#69506=CARTESIAN_POINT('Origin',(0.,133.2,13.3));
#69507=CARTESIAN_POINT('',(-7.31008487907097,133.2,10.5567976631721));
#69508=CARTESIAN_POINT('Origin',(-6.70494843988083,133.2,11.1214301896566));
#69509=CARTESIAN_POINT('',(-7.06568821984138,144.,10.7848359934202));
#69510=CARTESIAN_POINT('',(-7.06568821984138,138.6,10.7848359934202));
#69511=CARTESIAN_POINT('',(-7.31008487907097,144.,10.5567976631721));
#69512=CARTESIAN_POINT('Origin',(-7.06159463349151,144.,11.005548816766));
#69513=CARTESIAN_POINT('Origin',(0.,144.,13.3));
#69514=CARTESIAN_POINT('Origin',(-7.75872111940616,133.2,12.4255020918945));
#69515=CARTESIAN_POINT('',(-7.43743486603367,144.,12.3332722133368));
#69516=CARTESIAN_POINT('',(-7.43743486603367,133.2,12.3332722133368));
#69517=CARTESIAN_POINT('',(-7.43743486603367,138.6,12.3332722133368));
#69518=CARTESIAN_POINT('',(-6.96320280119572,144.,12.1971370214664));
#69519=CARTESIAN_POINT('',(-6.96320280119572,144.,12.1971370214664));
#69520=CARTESIAN_POINT('',(-6.96320280119572,133.2,12.1971370214664));
#69521=CARTESIAN_POINT('',(-6.96320280119572,133.2,12.1971370214664));
#69522=CARTESIAN_POINT('',(-6.96320280119572,133.2,12.1971370214664));
#69523=CARTESIAN_POINT('Origin',(-7.3335859289189,133.2,12.1384740970763));
#69524=CARTESIAN_POINT('',(-7.37215620887551,133.2,11.9211189928285));
#69525=CARTESIAN_POINT('Origin',(0.,133.2,13.3));
#69526=CARTESIAN_POINT('',(-7.64921699387799,133.2,11.7341202534779));
#69527=CARTESIAN_POINT('Origin',(-6.96320280119572,133.2,12.1971370214664));
#69528=CARTESIAN_POINT('',(-7.37215620887551,144.,11.9211189928285));
#69529=CARTESIAN_POINT('',(-7.37215620887551,138.6,11.9211189928285));
#69530=CARTESIAN_POINT('',(-7.64921699387799,144.,11.7341202534779));
#69531=CARTESIAN_POINT('Origin',(-7.3335859289189,144.,12.1384740970763));
#69532=CARTESIAN_POINT('Origin',(0.,144.,13.3));
#69533=CARTESIAN_POINT('Origin',(-7.8,133.2,13.65));
#69534=CARTESIAN_POINT('',(-7.4970972452634,144.,13.5086453811229));
#69535=CARTESIAN_POINT('',(-7.4970972452634,133.2,13.5086453811229));
#69536=CARTESIAN_POINT('',(-7.4970972452634,138.6,13.5086453811229));
#69537=CARTESIAN_POINT('',(-7.05,144.,13.3));
#69538=CARTESIAN_POINT('',(-7.05,144.,13.3));
#69539=CARTESIAN_POINT('',(-7.05,133.2,13.3));
#69540=CARTESIAN_POINT('',(-7.05,133.2,13.3));
#69541=CARTESIAN_POINT('',(-7.05,133.2,13.3));
#69542=CARTESIAN_POINT('Origin',(-7.425,133.2,13.3));
#69543=CARTESIAN_POINT('',(-7.5,133.2,13.3));
#69544=CARTESIAN_POINT('Origin',(0.,133.2,13.3));
#69545=CARTESIAN_POINT('',(-7.4970972452634,133.2,13.0913546188771));
#69546=CARTESIAN_POINT('',(-7.8,133.2,12.95));
#69547=CARTESIAN_POINT('Origin',(0.,133.2,13.3));
#69548=CARTESIAN_POINT('Origin',(-7.05,133.2,13.3));
#69549=CARTESIAN_POINT('',(-7.4970972452634,144.,13.0913546188771));
#69550=CARTESIAN_POINT('',(-7.4970972452634,138.6,13.0913546188771));
#69551=CARTESIAN_POINT('',(-7.8,144.,12.95));
#69552=CARTESIAN_POINT('Origin',(-7.425,144.,13.3));
#69553=CARTESIAN_POINT('',(-7.5,144.,13.3));
#69554=CARTESIAN_POINT('Origin',(0.,144.,13.3));
#69555=CARTESIAN_POINT('Origin',(0.,144.,13.3));
#69556=CARTESIAN_POINT('Origin',(-7.64921699387799,133.2,14.8658797465221));
#69557=CARTESIAN_POINT('',(-7.37215620887551,144.,14.6788810071715));
#69558=CARTESIAN_POINT('',(-7.37215620887551,133.2,14.6788810071715));
#69559=CARTESIAN_POINT('',(-7.37215620887551,138.6,14.6788810071715));
#69560=CARTESIAN_POINT('',(-6.96320280119572,144.,14.4028629785336));
#69561=CARTESIAN_POINT('',(-6.96320280119572,144.,14.4028629785336));
#69562=CARTESIAN_POINT('',(-6.96320280119572,133.2,14.4028629785336));
#69563=CARTESIAN_POINT('',(-6.96320280119572,133.2,14.4028629785336));
#69564=CARTESIAN_POINT('',(-6.96320280119572,133.2,14.4028629785336));
#69565=CARTESIAN_POINT('Origin',(-7.3335859289189,133.2,14.4615259029237));
#69566=CARTESIAN_POINT('',(-7.43743486603367,133.2,14.2667277866632));
#69567=CARTESIAN_POINT('Origin',(0.,133.2,13.3));
#69568=CARTESIAN_POINT('',(-7.75872111940616,133.2,14.1744979081055));
#69569=CARTESIAN_POINT('Origin',(-6.96320280119572,133.2,14.4028629785336));
#69570=CARTESIAN_POINT('',(-7.43743486603367,144.,14.2667277866632));
#69571=CARTESIAN_POINT('',(-7.43743486603367,138.6,14.2667277866632));
#69572=CARTESIAN_POINT('',(-7.75872111940616,144.,14.1744979081055));
#69573=CARTESIAN_POINT('Origin',(-7.3335859289189,144.,14.4615259029237));
#69574=CARTESIAN_POINT('Origin',(0.,144.,13.3));
#69575=CARTESIAN_POINT('Origin',(-7.31008487907097,133.2,16.0432023368279));
#69576=CARTESIAN_POINT('',(-7.06568821984138,144.,15.8151640065798));
#69577=CARTESIAN_POINT('',(-7.06568821984138,133.2,15.8151640065798));
#69578=CARTESIAN_POINT('',(-7.06568821984138,138.6,15.8151640065798));
#69579=CARTESIAN_POINT('',(-6.70494843988083,144.,15.4785698103434));
#69580=CARTESIAN_POINT('',(-6.70494843988083,144.,15.4785698103434));
#69581=CARTESIAN_POINT('',(-6.70494843988083,133.2,15.4785698103434));
#69582=CARTESIAN_POINT('',(-6.70494843988083,133.2,15.4785698103434));
#69583=CARTESIAN_POINT('',(-6.70494843988083,133.2,15.4785698103434));
#69584=CARTESIAN_POINT('Origin',(-7.06159463349151,133.2,15.594451183234));
#69585=CARTESIAN_POINT('',(-7.19463815697102,133.2,15.4182969079562));
#69586=CARTESIAN_POINT('Origin',(0.,133.2,13.3));
#69587=CARTESIAN_POINT('',(-7.52639677513343,133.2,15.3774627754213));
#69588=CARTESIAN_POINT('Origin',(-6.70494843988083,133.2,15.4785698103434));
#69589=CARTESIAN_POINT('',(-7.19463815697102,144.,15.4182969079562));
#69590=CARTESIAN_POINT('',(-7.19463815697102,138.6,15.4182969079562));
#69591=CARTESIAN_POINT('',(-7.52639677513343,144.,15.3774627754213));
#69592=CARTESIAN_POINT('Origin',(-7.06159463349151,144.,15.594451183234));
#69593=CARTESIAN_POINT('Origin',(0.,144.,13.3));
#69594=CARTESIAN_POINT('Origin',(-6.79095421376043,133.2,17.1529781814344));
#69595=CARTESIAN_POINT('',(-6.58523953715999,144.,16.8895153207954));
#69596=CARTESIAN_POINT('',(-6.58523953715999,133.2,16.8895153207954));
#69597=CARTESIAN_POINT('',(-6.58523953715999,138.6,16.8895153207954));
#69598=CARTESIAN_POINT('',(-6.28159599552799,144.,16.5006330231638));
#69599=CARTESIAN_POINT('',(-6.28159599552799,144.,16.5006330231638));
#69600=CARTESIAN_POINT('',(-6.28159599552799,133.2,16.5006330231638));
#69601=CARTESIAN_POINT('',(-6.28159599552799,133.2,16.5006330231638));
#69602=CARTESIAN_POINT('',(-6.28159599552799,133.2,16.5006330231638));
#69603=CARTESIAN_POINT('Origin',(-6.61572344209863,133.2,16.6708794605661));
#69604=CARTESIAN_POINT('',(-6.77468557884867,133.2,16.5177065291508));
#69605=CARTESIAN_POINT('Origin',(0.,133.2,13.3));
#69606=CARTESIAN_POINT('',(-7.10874756357811,133.2,16.5292736145025));
#69607=CARTESIAN_POINT('Origin',(-6.28159599552799,133.2,16.5006330231638));
#69608=CARTESIAN_POINT('',(-6.77468557884867,144.,16.5177065291508));
#69609=CARTESIAN_POINT('',(-6.77468557884867,138.6,16.5177065291508));
#69610=CARTESIAN_POINT('',(-7.10874756357811,144.,16.5292736145025));
#69611=CARTESIAN_POINT('Origin',(-6.61572344209863,144.,16.6708794605661));
#69612=CARTESIAN_POINT('Origin',(0.,144.,13.3));
#69613=CARTESIAN_POINT('Origin',(-6.10460771782222,133.2,18.1678809159125));
#69614=CARTESIAN_POINT('',(-5.9426404019167,144.,17.8754808548946));
#69615=CARTESIAN_POINT('',(-5.9426404019167,133.2,17.8754808548946));
#69616=CARTESIAN_POINT('',(-5.9426404019167,138.6,17.8754808548946));
#69617=CARTESIAN_POINT('',(-5.70356981034338,144.,17.4438860286619));
#69618=CARTESIAN_POINT('',(-5.70356981034338,144.,17.4438860286619));
#69619=CARTESIAN_POINT('',(-5.70356981034338,133.2,17.4438860286619));
#69620=CARTESIAN_POINT('',(-5.70356981034338,133.2,17.4438860286619));
#69621=CARTESIAN_POINT('',(-5.70356981034338,133.2,17.4438860286619));
#69622=CARTESIAN_POINT('Origin',(-6.00695118323398,133.2,17.6643054982716));
#69623=CARTESIAN_POINT('',(-6.18791775788269,133.2,17.5378855366421));
#69624=CARTESIAN_POINT('Origin',(0.,133.2,13.3));
#69625=CARTESIAN_POINT('',(-6.51605739442696,133.2,17.6015690198501));
#69626=CARTESIAN_POINT('Origin',(-5.70356981034338,133.2,17.4438860286619));
#69627=CARTESIAN_POINT('',(-6.18791775788269,144.,17.5378855366421));
#69628=CARTESIAN_POINT('',(-6.18791775788269,138.6,17.5378855366421));
#69629=CARTESIAN_POINT('',(-6.51605739442696,144.,17.6015690198501));
#69630=CARTESIAN_POINT('Origin',(-6.00695118323398,144.,17.6643054982716));
#69631=CARTESIAN_POINT('Origin',(0.,144.,13.3));
#69632=CARTESIAN_POINT('Origin',(-5.26794551983978,133.2,19.0629202666704));
#69633=CARTESIAN_POINT('',(-5.15371373748547,144.,18.748782865196));
#69634=CARTESIAN_POINT('',(-5.15371373748547,133.2,18.748782865196));
#69635=CARTESIAN_POINT('',(-5.15371373748547,138.6,18.748782865196));
#69636=CARTESIAN_POINT('',(-4.98510280736516,144.,18.2851028073652));
#69637=CARTESIAN_POINT('',(-4.98510280736516,144.,18.2851028073652));
#69638=CARTESIAN_POINT('',(-4.98510280736516,133.2,18.2851028073652));
#69639=CARTESIAN_POINT('',(-4.98510280736516,133.2,18.2851028073652));
#69640=CARTESIAN_POINT('',(-4.98510280736516,133.2,18.2851028073652));
#69641=CARTESIAN_POINT('Origin',(-5.25026785031011,133.2,18.5502678503101));
#69642=CARTESIAN_POINT('',(-5.44878286519601,133.2,18.4537137374855));
#69643=CARTESIAN_POINT('Origin',(0.,133.2,13.3));
#69644=CARTESIAN_POINT('',(-5.76292026667036,133.2,18.5679455198398));
#69645=CARTESIAN_POINT('Origin',(-4.98510280736516,133.2,18.2851028073652));
#69646=CARTESIAN_POINT('',(-5.44878286519601,144.,18.4537137374855));
#69647=CARTESIAN_POINT('',(-5.448782865196,138.6,18.4537137374855));
#69648=CARTESIAN_POINT('',(-5.76292026667036,144.,18.5679455198398));
#69649=CARTESIAN_POINT('Origin',(-5.25026785031011,144.,18.5502678503101));
#69650=CARTESIAN_POINT('Origin',(0.,144.,13.3));
#69651=CARTESIAN_POINT('Origin',(-4.30156901985006,133.2,19.816057394427));
#69652=CARTESIAN_POINT('',(-4.23788553664207,144.,19.4879177578827));
#69653=CARTESIAN_POINT('',(-4.23788553664207,133.2,19.4879177578827));
#69654=CARTESIAN_POINT('',(-4.23788553664207,138.6,19.4879177578827));
#69655=CARTESIAN_POINT('',(-4.14388602866194,144.,19.0035698103434));
#69656=CARTESIAN_POINT('',(-4.14388602866194,144.,19.0035698103434));
#69657=CARTESIAN_POINT('',(-4.14388602866194,133.2,19.0035698103434));
#69658=CARTESIAN_POINT('',(-4.14388602866194,133.2,19.0035698103434));
#69659=CARTESIAN_POINT('',(-4.14388602866194,133.2,19.0035698103434));
#69660=CARTESIAN_POINT('Origin',(-4.36430549827161,133.2,19.306951183234));
#69661=CARTESIAN_POINT('',(-4.57548085489463,133.2,19.2426404019167));
#69662=CARTESIAN_POINT('Origin',(0.,133.2,13.3));
#69663=CARTESIAN_POINT('',(-4.86788091591252,133.2,19.4046077178222));
#69664=CARTESIAN_POINT('Origin',(-4.14388602866194,133.2,19.0035698103434));
#69665=CARTESIAN_POINT('',(-4.57548085489463,144.,19.2426404019167));
#69666=CARTESIAN_POINT('',(-4.57548085489463,138.6,19.2426404019167));
#69667=CARTESIAN_POINT('',(-4.86788091591252,144.,19.4046077178222));
#69668=CARTESIAN_POINT('Origin',(-4.36430549827161,144.,19.306951183234));
#69669=CARTESIAN_POINT('Origin',(0.,144.,13.3));
#69670=CARTESIAN_POINT('Origin',(-3.22927361450253,133.2,20.4087475635781));
#69671=CARTESIAN_POINT('',(-3.21770652915082,144.,20.0746855788487));
#69672=CARTESIAN_POINT('',(-3.21770652915082,133.2,20.0746855788487));
#69673=CARTESIAN_POINT('',(-3.21770652915082,138.6,20.0746855788487));
#69674=CARTESIAN_POINT('',(-3.2006330231638,144.,19.581595995528));
#69675=CARTESIAN_POINT('',(-3.2006330231638,144.,19.581595995528));
#69676=CARTESIAN_POINT('',(-3.2006330231638,133.2,19.581595995528));
#69677=CARTESIAN_POINT('',(-3.2006330231638,133.2,19.581595995528));
#69678=CARTESIAN_POINT('',(-3.2006330231638,133.2,19.581595995528));
#69679=CARTESIAN_POINT('Origin',(-3.37087946056613,133.2,19.9157234420986));
#69680=CARTESIAN_POINT('',(-3.5895153207954,133.2,19.88523953716));
#69681=CARTESIAN_POINT('Origin',(0.,133.2,13.3));
#69682=CARTESIAN_POINT('',(-3.85297818143439,133.2,20.0909542137604));
#69683=CARTESIAN_POINT('Origin',(-3.2006330231638,133.2,19.581595995528));
#69684=CARTESIAN_POINT('',(-3.5895153207954,144.,19.88523953716));
#69685=CARTESIAN_POINT('',(-3.5895153207954,138.6,19.88523953716));
#69686=CARTESIAN_POINT('',(-3.85297818143439,144.,20.0909542137604));
#69687=CARTESIAN_POINT('Origin',(-3.37087946056613,144.,19.9157234420986));
#69688=CARTESIAN_POINT('Origin',(0.,144.,13.3));
#69689=CARTESIAN_POINT('Origin',(-2.07746277542129,133.2,20.8263967751334));
#69690=CARTESIAN_POINT('',(-2.11829690795615,144.,20.494638156971));
#69691=CARTESIAN_POINT('',(-2.11829690795615,133.2,20.494638156971));
#69692=CARTESIAN_POINT('',(-2.11829690795616,138.6,20.494638156971));
#69693=CARTESIAN_POINT('',(-2.17856981034338,144.,20.0049484398808));
#69694=CARTESIAN_POINT('',(-2.17856981034338,144.,20.0049484398808));
#69695=CARTESIAN_POINT('',(-2.17856981034338,133.2,20.0049484398808));
#69696=CARTESIAN_POINT('',(-2.17856981034338,133.2,20.0049484398808));
#69697=CARTESIAN_POINT('',(-2.17856981034338,133.2,20.0049484398808));
#69698=CARTESIAN_POINT('Origin',(-2.29445118323398,133.2,20.3615946334915));
#69699=CARTESIAN_POINT('',(-2.51516400657983,133.2,20.3656882198414));
#69700=CARTESIAN_POINT('Origin',(0.,133.2,13.3));
#69701=CARTESIAN_POINT('',(-2.74320233682789,133.2,20.610084879071));
#69702=CARTESIAN_POINT('Origin',(-2.17856981034338,133.2,20.0049484398808));
#69703=CARTESIAN_POINT('',(-2.51516400657983,144.,20.3656882198414));
#69704=CARTESIAN_POINT('',(-2.51516400657983,138.6,20.3656882198414));
#69705=CARTESIAN_POINT('',(-2.74320233682789,144.,20.610084879071));
#69706=CARTESIAN_POINT('Origin',(-2.29445118323398,144.,20.3615946334915));
#69707=CARTESIAN_POINT('Origin',(0.,144.,13.3));
#69708=CARTESIAN_POINT('Origin',(-0.874497908105503,133.2,21.0587211194062));
#69709=CARTESIAN_POINT('',(-0.966727786663231,144.,20.7374348660337));
#69710=CARTESIAN_POINT('',(-0.966727786663231,133.2,20.7374348660337));
#69711=CARTESIAN_POINT('',(-0.966727786663232,138.6,20.7374348660337));
#69712=CARTESIAN_POINT('',(-1.10286297853363,144.,20.2632028011957));
#69713=CARTESIAN_POINT('',(-1.10286297853363,144.,20.2632028011957));
#69714=CARTESIAN_POINT('',(-1.10286297853363,133.2,20.2632028011957));
#69715=CARTESIAN_POINT('',(-1.10286297853363,133.2,20.2632028011957));
#69716=CARTESIAN_POINT('',(-1.10286297853363,133.2,20.2632028011957));
#69717=CARTESIAN_POINT('Origin',(-1.16152590292371,133.2,20.6335859289189));
#69718=CARTESIAN_POINT('',(-1.37888100717151,133.2,20.6721562088755));
#69719=CARTESIAN_POINT('Origin',(0.,133.2,13.3));
#69720=CARTESIAN_POINT('',(-1.5658797465221,133.2,20.949216993878));
#69721=CARTESIAN_POINT('Origin',(-1.10286297853363,133.2,20.2632028011957));
#69722=CARTESIAN_POINT('',(-1.37888100717151,144.,20.6721562088755));
#69723=CARTESIAN_POINT('',(-1.37888100717151,138.6,20.6721562088755));
#69724=CARTESIAN_POINT('',(-1.5658797465221,144.,20.949216993878));
#69725=CARTESIAN_POINT('Origin',(-1.16152590292371,144.,20.6335859289189));
#69726=CARTESIAN_POINT('Origin',(0.,144.,13.3));
#69727=CARTESIAN_POINT('Origin',(0.349999999999999,133.2,21.1));
#69728=CARTESIAN_POINT('',(0.208645381122919,144.,20.7970972452634));
#69729=CARTESIAN_POINT('',(0.208645381122919,133.2,20.7970972452634));
#69730=CARTESIAN_POINT('',(0.208645381122919,138.6,20.7970972452634));
#69731=CARTESIAN_POINT('',(0.,144.,20.35));
#69732=CARTESIAN_POINT('',(0.,144.,20.35));
#69733=CARTESIAN_POINT('',(0.,133.2,20.35));
#69734=CARTESIAN_POINT('',(0.,133.2,20.35));
#69735=CARTESIAN_POINT('',(0.,133.2,20.35));
#69736=CARTESIAN_POINT('Origin',(0.,133.2,20.725));
#69737=CARTESIAN_POINT('',(-0.208645381122919,133.2,20.7970972452634));
#69738=CARTESIAN_POINT('Origin',(0.,133.2,13.3));
#69739=CARTESIAN_POINT('',(-0.349999999999999,133.2,21.1));
#69740=CARTESIAN_POINT('Origin',(0.,133.2,20.35));
#69741=CARTESIAN_POINT('',(-0.208645381122919,144.,20.7970972452634));
#69742=CARTESIAN_POINT('',(-0.208645381122919,138.6,20.7970972452634));
#69743=CARTESIAN_POINT('',(-0.349999999999999,144.,21.1));
#69744=CARTESIAN_POINT('Origin',(0.,144.,20.725));
#69745=CARTESIAN_POINT('Origin',(0.,144.,13.3));
#69746=CARTESIAN_POINT('Origin',(1.5658797465221,133.2,20.949216993878));
#69747=CARTESIAN_POINT('',(1.37888100717151,144.,20.6721562088755));
#69748=CARTESIAN_POINT('',(1.37888100717151,133.2,20.6721562088755));
#69749=CARTESIAN_POINT('',(1.37888100717151,138.6,20.6721562088755));
#69750=CARTESIAN_POINT('',(1.10286297853363,144.,20.2632028011957));
#69751=CARTESIAN_POINT('',(1.10286297853363,144.,20.2632028011957));
#69752=CARTESIAN_POINT('',(1.10286297853363,133.2,20.2632028011957));
#69753=CARTESIAN_POINT('',(1.10286297853363,133.2,20.2632028011957));
#69754=CARTESIAN_POINT('',(1.10286297853363,133.2,20.2632028011957));
#69755=CARTESIAN_POINT('Origin',(1.16152590292371,133.2,20.6335859289189));
#69756=CARTESIAN_POINT('',(0.966727786663231,133.2,20.7374348660337));
#69757=CARTESIAN_POINT('Origin',(0.,133.2,13.3));
#69758=CARTESIAN_POINT('',(0.874497908105503,133.2,21.0587211194062));
#69759=CARTESIAN_POINT('Origin',(1.10286297853363,133.2,20.2632028011957));
#69760=CARTESIAN_POINT('',(0.966727786663231,144.,20.7374348660337));
#69761=CARTESIAN_POINT('',(0.966727786663232,138.6,20.7374348660337));
#69762=CARTESIAN_POINT('',(0.874497908105503,144.,21.0587211194062));
#69763=CARTESIAN_POINT('Origin',(1.16152590292371,144.,20.6335859289189));
#69764=CARTESIAN_POINT('Origin',(0.,144.,13.3));
#69765=CARTESIAN_POINT('Origin',(2.74320233682789,133.2,20.610084879071));
#69766=CARTESIAN_POINT('',(2.51516400657983,144.,20.3656882198414));
#69767=CARTESIAN_POINT('',(2.51516400657983,133.2,20.3656882198414));
#69768=CARTESIAN_POINT('',(2.51516400657983,138.6,20.3656882198414));
#69769=CARTESIAN_POINT('',(2.17856981034338,144.,20.0049484398808));
#69770=CARTESIAN_POINT('',(2.17856981034338,144.,20.0049484398808));
#69771=CARTESIAN_POINT('',(2.17856981034338,133.2,20.0049484398808));
#69772=CARTESIAN_POINT('',(2.17856981034338,133.2,20.0049484398808));
#69773=CARTESIAN_POINT('',(2.17856981034338,133.2,20.0049484398808));
#69774=CARTESIAN_POINT('Origin',(2.29445118323399,133.2,20.3615946334915));
#69775=CARTESIAN_POINT('',(2.11829690795615,133.2,20.494638156971));
#69776=CARTESIAN_POINT('Origin',(0.,133.2,13.3));
#69777=CARTESIAN_POINT('',(2.07746277542129,133.2,20.8263967751334));
#69778=CARTESIAN_POINT('Origin',(2.17856981034338,133.2,20.0049484398808));
#69779=CARTESIAN_POINT('',(2.11829690795615,144.,20.494638156971));
#69780=CARTESIAN_POINT('',(2.11829690795616,138.6,20.494638156971));
#69781=CARTESIAN_POINT('',(2.07746277542129,144.,20.8263967751334));
#69782=CARTESIAN_POINT('Origin',(2.29445118323399,144.,20.3615946334915));
#69783=CARTESIAN_POINT('Origin',(0.,144.,13.3));
#69784=CARTESIAN_POINT('Origin',(3.85297818143439,133.2,20.0909542137604));
#69785=CARTESIAN_POINT('',(3.5895153207954,144.,19.88523953716));
#69786=CARTESIAN_POINT('',(3.5895153207954,133.2,19.88523953716));
#69787=CARTESIAN_POINT('',(3.5895153207954,138.6,19.88523953716));
#69788=CARTESIAN_POINT('',(3.20063302316381,144.,19.581595995528));
#69789=CARTESIAN_POINT('',(3.20063302316381,144.,19.581595995528));
#69790=CARTESIAN_POINT('',(3.20063302316381,133.2,19.581595995528));
#69791=CARTESIAN_POINT('',(3.20063302316381,133.2,19.581595995528));
#69792=CARTESIAN_POINT('',(3.20063302316381,133.2,19.581595995528));
#69793=CARTESIAN_POINT('Origin',(3.37087946056613,133.2,19.9157234420986));
#69794=CARTESIAN_POINT('',(3.21770652915082,133.2,20.0746855788487));
#69795=CARTESIAN_POINT('Origin',(0.,133.2,13.3));
#69796=CARTESIAN_POINT('',(3.22927361450254,133.2,20.4087475635781));
#69797=CARTESIAN_POINT('Origin',(3.20063302316381,133.2,19.581595995528));
#69798=CARTESIAN_POINT('',(3.21770652915082,144.,20.0746855788487));
#69799=CARTESIAN_POINT('',(3.21770652915082,138.6,20.0746855788487));
#69800=CARTESIAN_POINT('',(3.22927361450254,144.,20.4087475635781));
#69801=CARTESIAN_POINT('Origin',(3.37087946056613,144.,19.9157234420986));
#69802=CARTESIAN_POINT('Origin',(0.,144.,13.3));
#69803=CARTESIAN_POINT('Origin',(4.86788091591252,133.2,19.4046077178222));
#69804=CARTESIAN_POINT('',(4.57548085489463,144.,19.2426404019167));
#69805=CARTESIAN_POINT('',(4.57548085489463,133.2,19.2426404019167));
#69806=CARTESIAN_POINT('',(4.57548085489463,138.6,19.2426404019167));
#69807=CARTESIAN_POINT('',(4.14388602866194,144.,19.0035698103434));
#69808=CARTESIAN_POINT('',(4.14388602866194,144.,19.0035698103434));
#69809=CARTESIAN_POINT('',(4.14388602866194,133.2,19.0035698103434));
#69810=CARTESIAN_POINT('',(4.14388602866194,133.2,19.0035698103434));
#69811=CARTESIAN_POINT('',(4.14388602866194,133.2,19.0035698103434));
#69812=CARTESIAN_POINT('Origin',(4.36430549827161,133.2,19.306951183234));
#69813=CARTESIAN_POINT('',(4.23788553664207,133.2,19.4879177578827));
#69814=CARTESIAN_POINT('Origin',(0.,133.2,13.3));
#69815=CARTESIAN_POINT('',(4.30156901985006,133.2,19.816057394427));
#69816=CARTESIAN_POINT('Origin',(4.14388602866194,133.2,19.0035698103434));
#69817=CARTESIAN_POINT('',(4.23788553664207,144.,19.4879177578827));
#69818=CARTESIAN_POINT('',(4.23788553664207,138.6,19.4879177578827));
#69819=CARTESIAN_POINT('',(4.30156901985006,144.,19.816057394427));
#69820=CARTESIAN_POINT('Origin',(4.36430549827161,144.,19.306951183234));
#69821=CARTESIAN_POINT('Origin',(0.,144.,13.3));
#69822=CARTESIAN_POINT('Origin',(5.76292026667036,133.2,18.5679455198398));
#69823=CARTESIAN_POINT('',(5.44878286519601,144.,18.4537137374855));
#69824=CARTESIAN_POINT('',(5.44878286519601,133.2,18.4537137374855));
#69825=CARTESIAN_POINT('',(5.44878286519601,138.6,18.4537137374855));
#69826=CARTESIAN_POINT('',(4.98510280736516,144.,18.2851028073652));
#69827=CARTESIAN_POINT('',(4.98510280736516,144.,18.2851028073652));
#69828=CARTESIAN_POINT('',(4.98510280736516,133.2,18.2851028073652));
#69829=CARTESIAN_POINT('',(4.98510280736516,133.2,18.2851028073652));
#69830=CARTESIAN_POINT('',(4.98510280736516,133.2,18.2851028073652));
#69831=CARTESIAN_POINT('Origin',(5.25026785031011,133.2,18.5502678503101));
#69832=CARTESIAN_POINT('',(5.15371373748547,133.2,18.748782865196));
#69833=CARTESIAN_POINT('Origin',(0.,133.2,13.3));
#69834=CARTESIAN_POINT('',(5.26794551983978,133.2,19.0629202666704));
#69835=CARTESIAN_POINT('Origin',(4.98510280736516,133.2,18.2851028073652));
#69836=CARTESIAN_POINT('',(5.15371373748547,144.,18.748782865196));
#69837=CARTESIAN_POINT('',(5.15371373748547,138.6,18.748782865196));
#69838=CARTESIAN_POINT('',(5.26794551983978,144.,19.0629202666704));
#69839=CARTESIAN_POINT('Origin',(5.25026785031011,144.,18.5502678503101));
#69840=CARTESIAN_POINT('Origin',(0.,144.,13.3));
#69841=CARTESIAN_POINT('Origin',(6.51605739442696,133.2,17.6015690198501));
#69842=CARTESIAN_POINT('',(6.18791775788269,144.,17.5378855366421));
#69843=CARTESIAN_POINT('',(6.18791775788269,133.2,17.5378855366421));
#69844=CARTESIAN_POINT('',(6.18791775788269,138.6,17.5378855366421));
#69845=CARTESIAN_POINT('',(5.70356981034338,144.,17.4438860286619));
#69846=CARTESIAN_POINT('',(5.70356981034338,144.,17.4438860286619));
#69847=CARTESIAN_POINT('',(5.70356981034338,133.2,17.4438860286619));
#69848=CARTESIAN_POINT('',(5.70356981034338,133.2,17.4438860286619));
#69849=CARTESIAN_POINT('',(5.70356981034338,133.2,17.4438860286619));
#69850=CARTESIAN_POINT('Origin',(6.00695118323398,133.2,17.6643054982716));
#69851=CARTESIAN_POINT('',(5.9426404019167,133.2,17.8754808548946));
#69852=CARTESIAN_POINT('Origin',(0.,133.2,13.3));
#69853=CARTESIAN_POINT('',(6.10460771782223,133.2,18.1678809159125));
#69854=CARTESIAN_POINT('Origin',(5.70356981034338,133.2,17.4438860286619));
#69855=CARTESIAN_POINT('',(5.9426404019167,144.,17.8754808548946));
#69856=CARTESIAN_POINT('',(5.9426404019167,138.6,17.8754808548946));
#69857=CARTESIAN_POINT('',(6.10460771782223,144.,18.1678809159125));
#69858=CARTESIAN_POINT('Origin',(6.00695118323398,144.,17.6643054982716));
#69859=CARTESIAN_POINT('Origin',(0.,144.,13.3));
#69860=CARTESIAN_POINT('Origin',(7.10874756357811,133.2,16.5292736145025));
#69861=CARTESIAN_POINT('',(6.77468557884867,144.,16.5177065291508));
#69862=CARTESIAN_POINT('',(6.77468557884867,133.2,16.5177065291508));
#69863=CARTESIAN_POINT('',(6.77468557884867,138.6,16.5177065291508));
#69864=CARTESIAN_POINT('',(6.28159599552799,144.,16.5006330231638));
#69865=CARTESIAN_POINT('',(6.28159599552799,144.,16.5006330231638));
#69866=CARTESIAN_POINT('',(6.28159599552799,133.2,16.5006330231638));
#69867=CARTESIAN_POINT('',(6.28159599552799,133.2,16.5006330231638));
#69868=CARTESIAN_POINT('',(6.28159599552799,133.2,16.5006330231638));
#69869=CARTESIAN_POINT('Origin',(6.61572344209863,133.2,16.6708794605661));
#69870=CARTESIAN_POINT('',(6.58523953715999,133.2,16.8895153207954));
#69871=CARTESIAN_POINT('Origin',(0.,133.2,13.3));
#69872=CARTESIAN_POINT('',(6.79095421376043,133.2,17.1529781814344));
#69873=CARTESIAN_POINT('Origin',(6.28159599552799,133.2,16.5006330231638));
#69874=CARTESIAN_POINT('',(6.58523953715999,144.,16.8895153207954));
#69875=CARTESIAN_POINT('',(6.58523953715999,138.6,16.8895153207954));
#69876=CARTESIAN_POINT('',(6.79095421376043,144.,17.1529781814344));
#69877=CARTESIAN_POINT('Origin',(6.61572344209863,144.,16.6708794605661));
#69878=CARTESIAN_POINT('Origin',(0.,144.,13.3));
#69879=CARTESIAN_POINT('Origin',(7.52639677513343,133.2,15.3774627754213));
#69880=CARTESIAN_POINT('',(7.19463815697102,144.,15.4182969079562));
#69881=CARTESIAN_POINT('',(7.19463815697102,133.2,15.4182969079562));
#69882=CARTESIAN_POINT('',(7.19463815697102,138.6,15.4182969079562));
#69883=CARTESIAN_POINT('',(6.70494843988083,144.,15.4785698103434));
#69884=CARTESIAN_POINT('',(6.70494843988083,144.,15.4785698103434));
#69885=CARTESIAN_POINT('',(6.70494843988083,133.2,15.4785698103434));
#69886=CARTESIAN_POINT('',(6.70494843988083,133.2,15.4785698103434));
#69887=CARTESIAN_POINT('',(6.70494843988083,133.2,15.4785698103434));
#69888=CARTESIAN_POINT('Origin',(7.06159463349151,133.2,15.594451183234));
#69889=CARTESIAN_POINT('',(7.06568821984138,133.2,15.8151640065798));
#69890=CARTESIAN_POINT('Origin',(0.,133.2,13.3));
#69891=CARTESIAN_POINT('',(7.31008487907097,133.2,16.0432023368279));
#69892=CARTESIAN_POINT('Origin',(6.70494843988083,133.2,15.4785698103434));
#69893=CARTESIAN_POINT('',(7.06568821984138,144.,15.8151640065798));
#69894=CARTESIAN_POINT('',(7.06568821984138,138.6,15.8151640065798));
#69895=CARTESIAN_POINT('',(7.31008487907097,144.,16.0432023368279));
#69896=CARTESIAN_POINT('Origin',(7.06159463349151,144.,15.594451183234));
#69897=CARTESIAN_POINT('Origin',(0.,144.,13.3));
#69898=CARTESIAN_POINT('Origin',(7.75872111940616,133.2,14.1744979081055));
#69899=CARTESIAN_POINT('',(7.43743486603367,144.,14.2667277866632));
#69900=CARTESIAN_POINT('',(7.43743486603367,138.6,14.2667277866632));
#69901=CARTESIAN_POINT('',(6.96320280119572,144.,14.4028629785336));
#69902=CARTESIAN_POINT('',(6.96320280119572,144.,14.4028629785336));
#69903=CARTESIAN_POINT('',(6.96320280119572,133.2,14.4028629785336));
#69904=CARTESIAN_POINT('Origin',(7.3335859289189,133.2,14.4615259029237));
#69905=CARTESIAN_POINT('Origin',(0.,133.2,13.3));
#69906=CARTESIAN_POINT('Origin',(6.96320280119572,133.2,14.4028629785336));
#69907=CARTESIAN_POINT('',(7.37215620887551,144.,14.6788810071715));
#69908=CARTESIAN_POINT('',(7.64921699387799,144.,14.8658797465221));
#69909=CARTESIAN_POINT('',(7.37215620887551,138.6,14.6788810071715));
#69910=CARTESIAN_POINT('Origin',(7.3335859289189,144.,14.4615259029237));
#69911=CARTESIAN_POINT('Origin',(0.,144.,13.3));
#69912=CARTESIAN_POINT('Origin',(7.425,133.2,13.3));
#69913=CARTESIAN_POINT('Origin',(0.,133.2,13.3));
#69914=CARTESIAN_POINT('Origin',(7.425,144.,13.3));
#69915=CARTESIAN_POINT('Origin',(0.,144.,13.3));
#69916=CARTESIAN_POINT('Origin',(0.,144.95,13.3));
#69917=CARTESIAN_POINT('',(-2.01,144.7,13.3));
#69918=CARTESIAN_POINT('Origin',(0.,144.7,13.3));
#69919=CARTESIAN_POINT('',(-5.8,145.2,13.3));
#69920=CARTESIAN_POINT('',(-3.905,144.95,13.3));
#69921=CARTESIAN_POINT('Origin',(0.,145.2,13.3));
#69922=CARTESIAN_POINT('Origin',(6.9,145.2,13.3));
#69923=CARTESIAN_POINT('',(-6.9,145.2,13.3));
#69924=CARTESIAN_POINT('Origin',(0.,145.2,13.3));
#69925=CARTESIAN_POINT('Origin',(0.,144.9,13.3));
#69926=CARTESIAN_POINT('',(-7.5,144.6,13.3));
#69927=CARTESIAN_POINT('Origin',(0.,144.6,13.3));
#69928=CARTESIAN_POINT('',(-7.2,144.9,13.3));
#69929=CARTESIAN_POINT('Origin',(0.,138.6,13.3));
#69930=CARTESIAN_POINT('',(-7.5,132.6,13.3));
#69931=CARTESIAN_POINT('Origin',(0.,132.6,13.3));
#69932=CARTESIAN_POINT('',(-7.5,138.6,13.3));
#69933=CARTESIAN_POINT('',(-7.5,138.6,13.3));
#69934=CARTESIAN_POINT('Origin',(0.,132.4,13.3));
#69935=CARTESIAN_POINT('',(-7.1,132.2,13.3));
#69936=CARTESIAN_POINT('',(-7.3,132.4,13.3));
#69937=CARTESIAN_POINT('Origin',(0.,132.2,13.3));
#69938=CARTESIAN_POINT('Origin',(2.8,132.2,13.3));
#69939=CARTESIAN_POINT('',(-2.8,132.2,13.3));
#69940=CARTESIAN_POINT('Origin',(0.,132.2,13.3));
#69941=CARTESIAN_POINT('Origin',(0.,131.125,13.3));
#69942=CARTESIAN_POINT('',(-2.8,130.05,13.3));
#69943=CARTESIAN_POINT('Origin',(0.,130.05,13.3));
#69944=CARTESIAN_POINT('',(-2.8,131.125,13.3));
#69945=CARTESIAN_POINT('Origin',(2.01,130.05,13.3));
#69946=CARTESIAN_POINT('',(-2.01,130.05,13.3));
#69947=CARTESIAN_POINT('Origin',(0.,130.05,13.3));
#69948=CARTESIAN_POINT('Origin',(0.,137.625,13.3));
#69949=CARTESIAN_POINT('',(-2.01,137.625,13.3));
#69950=CARTESIAN_POINT('',(0.,0.,0.));
#69951=CARTESIAN_POINT('Ctrl Pts',(18.3,110.643929117918,2.64843108169734));
#69952=CARTESIAN_POINT('Ctrl Pts',(18.1272,110.643929117918,2.64843108169734));
#69953=CARTESIAN_POINT('Ctrl Pts',(18.3,110.643929117918,2.78376536481082));
#69954=CARTESIAN_POINT('Ctrl Pts',(18.1272,110.643929117918,2.78376536481082));
#69955=CARTESIAN_POINT('Ctrl Pts',(18.3,110.529331588745,2.86452936045825));
#69956=CARTESIAN_POINT('Ctrl Pts',(18.1272,110.529331588745,2.86452936045825));
#69957=CARTESIAN_POINT('',(18.3,110.643929117918,2.64843108169734));
#69958=CARTESIAN_POINT('',(18.3,110.529331588745,2.86452936045825));
#69959=CARTESIAN_POINT('Ctrl Pts',(18.3,110.643929117918,2.64843108169734));
#69960=CARTESIAN_POINT('Ctrl Pts',(18.3,110.643929117918,2.78376536481082));
#69961=CARTESIAN_POINT('Ctrl Pts',(18.3,110.529331588745,2.86452936045825));
#69962=CARTESIAN_POINT('',(18.18,110.643929117918,2.64843108169734));
#69963=CARTESIAN_POINT('',(18.3,110.643929117918,2.64843108169734));
#69964=CARTESIAN_POINT('',(18.18,110.529331588745,2.86452936045825));
#69965=CARTESIAN_POINT('Ctrl Pts',(18.18,110.643929117918,2.64843108169734));
#69966=CARTESIAN_POINT('Ctrl Pts',(18.18,110.643929117918,2.78376536481082));
#69967=CARTESIAN_POINT('Ctrl Pts',(18.18,110.529331588745,2.86452936045825));
#69968=CARTESIAN_POINT('',(18.3,110.529331588745,2.86452936045825));
#69969=CARTESIAN_POINT('Ctrl Pts',(18.3,110.514051938057,2.41869034282863));
#69970=CARTESIAN_POINT('Ctrl Pts',(18.1272,110.514051938057,2.41869034282863));
#69971=CARTESIAN_POINT('Ctrl Pts',(18.3,110.643929117918,2.51091407649219));
#69972=CARTESIAN_POINT('Ctrl Pts',(18.1272,110.643929117918,2.51091407649219));
#69973=CARTESIAN_POINT('Ctrl Pts',(18.3,110.643929117918,2.64843108169734));
#69974=CARTESIAN_POINT('Ctrl Pts',(18.1272,110.643929117918,2.64843108169734));
#69975=CARTESIAN_POINT('',(18.3,110.514051938057,2.41869034282863));
#69976=CARTESIAN_POINT('Ctrl Pts',(18.3,110.514051938057,2.41869034282863));
#69977=CARTESIAN_POINT('Ctrl Pts',(18.3,110.643929117918,2.51091407649219));
#69978=CARTESIAN_POINT('Ctrl Pts',(18.3,110.643929117918,2.64843108169734));
#69979=CARTESIAN_POINT('',(18.18,110.514051938057,2.41869034282863));
#69980=CARTESIAN_POINT('',(18.3,110.514051938057,2.41869034282863));
#69981=CARTESIAN_POINT('Ctrl Pts',(18.18,110.514051938057,2.41869034282863));
#69982=CARTESIAN_POINT('Ctrl Pts',(18.18,110.643929117918,2.51091407649219));
#69983=CARTESIAN_POINT('Ctrl Pts',(18.18,110.643929117918,2.64843108169734));
#69984=CARTESIAN_POINT('Ctrl Pts',(18.3,109.989085966349,2.32646660916507));
#69985=CARTESIAN_POINT('Ctrl Pts',(18.1272,109.989085966349,2.32646660916507));
#69986=CARTESIAN_POINT('Ctrl Pts',(18.3,110.384174609184,2.32646660916507));
#69987=CARTESIAN_POINT('Ctrl Pts',(18.1272,110.384174609184,2.32646660916507));
#69988=CARTESIAN_POINT('Ctrl Pts',(18.3,110.514051938057,2.41869034282863));
#69989=CARTESIAN_POINT('Ctrl Pts',(18.1272,110.514051938057,2.41869034282863));
#69990=CARTESIAN_POINT('',(18.3,109.989085966349,2.32646660916507));
#69991=CARTESIAN_POINT('Ctrl Pts',(18.3,109.989085966349,2.32646660916507));
#69992=CARTESIAN_POINT('Ctrl Pts',(18.3,110.384174609184,2.32646660916507));
#69993=CARTESIAN_POINT('Ctrl Pts',(18.3,110.514051938057,2.41869034282863));
#69994=CARTESIAN_POINT('',(18.18,109.989085966349,2.32646660916507));
#69995=CARTESIAN_POINT('',(18.3,109.989085966349,2.32646660916507));
#69996=CARTESIAN_POINT('Ctrl Pts',(18.18,109.989085966349,2.32646660916507));
#69997=CARTESIAN_POINT('Ctrl Pts',(18.18,110.384174609184,2.32646660916507));
#69998=CARTESIAN_POINT('Ctrl Pts',(18.18,110.514051938057,2.41869034282863));
#69999=CARTESIAN_POINT('Ctrl Pts',(18.3,109.465211504698,2.41869034282863));
#70000=CARTESIAN_POINT('Ctrl Pts',(18.1272,109.465211504698,2.41869034282863));
#70001=CARTESIAN_POINT('Ctrl Pts',(18.3,109.596180194616,2.32646660916507));
#70002=CARTESIAN_POINT('Ctrl Pts',(18.1272,109.596180194616,2.32646660916507));
#70003=CARTESIAN_POINT('Ctrl Pts',(18.3,109.989085966349,2.32646660916507));
#70004=CARTESIAN_POINT('Ctrl Pts',(18.1272,109.989085966349,2.32646660916507));
#70005=CARTESIAN_POINT('',(18.3,109.465211504698,2.41869034282863));
#70006=CARTESIAN_POINT('Ctrl Pts',(18.3,109.465211504698,2.41869034282863));
#70007=CARTESIAN_POINT('Ctrl Pts',(18.3,109.596180194616,2.32646660916507));
#70008=CARTESIAN_POINT('Ctrl Pts',(18.3,109.989085966349,2.32646660916507));
#70009=CARTESIAN_POINT('',(18.18,109.465211504698,2.41869034282863));
#70010=CARTESIAN_POINT('',(18.3,109.465211504698,2.41869034282863));
#70011=CARTESIAN_POINT('Ctrl Pts',(18.18,109.465211504698,2.41869034282863));
#70012=CARTESIAN_POINT('Ctrl Pts',(18.18,109.596180194616,2.32646660916507));
#70013=CARTESIAN_POINT('Ctrl Pts',(18.18,109.989085966349,2.32646660916507));
#70014=CARTESIAN_POINT('Ctrl Pts',(18.3,109.334242814779,2.64624821059406));
#70015=CARTESIAN_POINT('Ctrl Pts',(18.1272,109.334242814779,2.64624821059406));
#70016=CARTESIAN_POINT('Ctrl Pts',(18.3,109.334242814779,2.51091407649219));
#70017=CARTESIAN_POINT('Ctrl Pts',(18.1272,109.334242814779,2.51091407649219));
#70018=CARTESIAN_POINT('Ctrl Pts',(18.3,109.465211504698,2.41869034282863));
#70019=CARTESIAN_POINT('Ctrl Pts',(18.1272,109.465211504698,2.41869034282863));
#70020=CARTESIAN_POINT('',(18.3,109.334242814779,2.64624821059406));
#70021=CARTESIAN_POINT('Ctrl Pts',(18.3,109.334242814779,2.64624821059406));
#70022=CARTESIAN_POINT('Ctrl Pts',(18.3,109.334242814779,2.51091407649219));
#70023=CARTESIAN_POINT('Ctrl Pts',(18.3,109.465211504698,2.41869034282863));
#70024=CARTESIAN_POINT('',(18.18,109.334242814779,2.64624821059406));
#70025=CARTESIAN_POINT('',(18.3,109.334242814779,2.64624821059406));
#70026=CARTESIAN_POINT('Ctrl Pts',(18.18,109.334242814779,2.64624821059406));
#70027=CARTESIAN_POINT('Ctrl Pts',(18.18,109.334242814779,2.51091407649219));
#70028=CARTESIAN_POINT('Ctrl Pts',(18.18,109.465211504698,2.41869034282863));
#70029=CARTESIAN_POINT('Ctrl Pts',(18.3,109.464665824175,2.8738062273711));
#70030=CARTESIAN_POINT('Ctrl Pts',(18.1272,109.464665824175,2.8738062273711));
#70031=CARTESIAN_POINT('Ctrl Pts',(18.3,109.334242814779,2.78158249370754));
#70032=CARTESIAN_POINT('Ctrl Pts',(18.1272,109.334242814779,2.78158249370754));
#70033=CARTESIAN_POINT('Ctrl Pts',(18.3,109.334242814779,2.64624821059406));
#70034=CARTESIAN_POINT('Ctrl Pts',(18.1272,109.334242814779,2.64624821059406));
#70035=CARTESIAN_POINT('',(18.3,109.464665824175,2.8738062273711));
#70036=CARTESIAN_POINT('Ctrl Pts',(18.3,109.464665824175,2.8738062273711));
#70037=CARTESIAN_POINT('Ctrl Pts',(18.3,109.334242814779,2.78158249370754));
#70038=CARTESIAN_POINT('Ctrl Pts',(18.3,109.334242814779,2.64624821059406));
#70039=CARTESIAN_POINT('',(18.18,109.464665824175,2.8738062273711));
#70040=CARTESIAN_POINT('',(18.3,109.464665824175,2.8738062273711));
#70041=CARTESIAN_POINT('Ctrl Pts',(18.18,109.464665824175,2.8738062273711));
#70042=CARTESIAN_POINT('Ctrl Pts',(18.18,109.334242814779,2.78158249370754));
#70043=CARTESIAN_POINT('Ctrl Pts',(18.18,109.334242814779,2.64624821059406));
#70044=CARTESIAN_POINT('Ctrl Pts',(18.3,109.989085966349,2.96602996103466));
#70045=CARTESIAN_POINT('Ctrl Pts',(18.1272,109.989085966349,2.96602996103466));
#70046=CARTESIAN_POINT('Ctrl Pts',(18.3,109.59508883357,2.96602996103466));
#70047=CARTESIAN_POINT('Ctrl Pts',(18.1272,109.59508883357,2.96602996103466));
#70048=CARTESIAN_POINT('Ctrl Pts',(18.3,109.464665824175,2.8738062273711));
#70049=CARTESIAN_POINT('Ctrl Pts',(18.1272,109.464665824175,2.8738062273711));
#70050=CARTESIAN_POINT('',(18.3,109.989085966349,2.96602996103466));
#70051=CARTESIAN_POINT('Ctrl Pts',(18.3,109.989085966349,2.96602996103466));
#70052=CARTESIAN_POINT('Ctrl Pts',(18.3,109.59508883357,2.96602996103466));
#70053=CARTESIAN_POINT('Ctrl Pts',(18.3,109.464665824175,2.8738062273711));
#70054=CARTESIAN_POINT('',(18.18,109.989085966349,2.96602996103466));
#70055=CARTESIAN_POINT('',(18.3,109.989085966349,2.96602996103466));
#70056=CARTESIAN_POINT('Ctrl Pts',(18.18,109.989085966349,2.96602996103466));
#70057=CARTESIAN_POINT('Ctrl Pts',(18.18,109.59508883357,2.96602996103466));
#70058=CARTESIAN_POINT('Ctrl Pts',(18.18,109.464665824175,2.8738062273711));
#70059=CARTESIAN_POINT('Ctrl Pts',(18.3,110.529331588745,2.86452936045825));
#70060=CARTESIAN_POINT('Ctrl Pts',(18.1272,110.529331588745,2.86452936045825));
#70061=CARTESIAN_POINT('Ctrl Pts',(18.3,110.383083099127,2.96602996103466));
#70062=CARTESIAN_POINT('Ctrl Pts',(18.1272,110.383083099127,2.96602996103466));
#70063=CARTESIAN_POINT('Ctrl Pts',(18.3,109.989085966349,2.96602996103466));
#70064=CARTESIAN_POINT('Ctrl Pts',(18.1272,109.989085966349,2.96602996103466));
#70065=CARTESIAN_POINT('Ctrl Pts',(18.3,110.529331588745,2.86452936045825));
#70066=CARTESIAN_POINT('Ctrl Pts',(18.3,110.383083099127,2.96602996103466));
#70067=CARTESIAN_POINT('Ctrl Pts',(18.3,109.989085966349,2.96602996103466));
#70068=CARTESIAN_POINT('Ctrl Pts',(18.18,110.529331588745,2.86452936045825));
#70069=CARTESIAN_POINT('Ctrl Pts',(18.18,110.383083099127,2.96602996103466));
#70070=CARTESIAN_POINT('Ctrl Pts',(18.18,109.989085966349,2.96602996103466));
#70071=CARTESIAN_POINT('Ctrl Pts',(18.3,109.172714823484,2.64624821059406));
#70072=CARTESIAN_POINT('Ctrl Pts',(18.1272,109.172714823484,2.64624821059406));
#70073=CARTESIAN_POINT('Ctrl Pts',(18.3,109.172714823484,2.87762614004314));
#70074=CARTESIAN_POINT('Ctrl Pts',(18.1272,109.172714823484,2.87762614004314));
#70075=CARTESIAN_POINT('Ctrl Pts',(18.3,109.338608556986,3.00968619100749));
#70076=CARTESIAN_POINT('Ctrl Pts',(18.1272,109.338608556986,3.00968619100749));
#70077=CARTESIAN_POINT('',(18.3,109.172714823484,2.64624821059406));
#70078=CARTESIAN_POINT('',(18.3,109.338608556986,3.00968619100749));
#70079=CARTESIAN_POINT('Ctrl Pts',(18.3,109.172714823484,2.64624821059406));
#70080=CARTESIAN_POINT('Ctrl Pts',(18.3,109.172714823484,2.87762614004314));
#70081=CARTESIAN_POINT('Ctrl Pts',(18.3,109.338608556986,3.00968619100749));
#70082=CARTESIAN_POINT('',(18.18,109.172714823484,2.64624821059406));
#70083=CARTESIAN_POINT('',(18.3,109.172714823484,2.64624821059406));
#70084=CARTESIAN_POINT('',(18.18,109.338608556986,3.00968619100749));
#70085=CARTESIAN_POINT('Ctrl Pts',(18.18,109.172714823484,2.64624821059406));
#70086=CARTESIAN_POINT('Ctrl Pts',(18.18,109.172714823484,2.87762614004314));
#70087=CARTESIAN_POINT('Ctrl Pts',(18.18,109.338608556986,3.00968619100749));
#70088=CARTESIAN_POINT('',(18.3,109.338608556986,3.00968619100749));
#70089=CARTESIAN_POINT('Ctrl Pts',(18.3,109.267121428251,2.35538886897266));
#70090=CARTESIAN_POINT('Ctrl Pts',(18.1272,109.267121428251,2.35538886897266));
#70091=CARTESIAN_POINT('Ctrl Pts',(18.3,109.172714823484,2.47053207866847));
#70092=CARTESIAN_POINT('Ctrl Pts',(18.1272,109.172714823484,2.47053207866847));
#70093=CARTESIAN_POINT('Ctrl Pts',(18.3,109.172714823484,2.64624821059406));
#70094=CARTESIAN_POINT('Ctrl Pts',(18.1272,109.172714823484,2.64624821059406));
#70095=CARTESIAN_POINT('',(18.3,109.267121428251,2.35538886897266));
#70096=CARTESIAN_POINT('Ctrl Pts',(18.3,109.267121428251,2.35538886897266));
#70097=CARTESIAN_POINT('Ctrl Pts',(18.3,109.172714823484,2.47053207866847));
#70098=CARTESIAN_POINT('Ctrl Pts',(18.3,109.172714823484,2.64624821059406));
#70099=CARTESIAN_POINT('',(18.18,109.267121428251,2.35538886897266));
#70100=CARTESIAN_POINT('',(18.3,109.267121428251,2.35538886897266));
#70101=CARTESIAN_POINT('Ctrl Pts',(18.18,109.267121428251,2.35538886897266));
#70102=CARTESIAN_POINT('Ctrl Pts',(18.18,109.172714823484,2.47053207866847));
#70103=CARTESIAN_POINT('Ctrl Pts',(18.18,109.172714823484,2.64624821059406));
#70104=CARTESIAN_POINT('Ctrl Pts',(18.3,109.534515613317,2.18240113966167));
#70105=CARTESIAN_POINT('Ctrl Pts',(18.1272,109.534515613317,2.18240113966167));
#70106=CARTESIAN_POINT('Ctrl Pts',(18.3,109.361528033018,2.24024551026523));
#70107=CARTESIAN_POINT('Ctrl Pts',(18.1272,109.361528033018,2.24024551026523));
#70108=CARTESIAN_POINT('Ctrl Pts',(18.3,109.267121428251,2.35538886897266));
#70109=CARTESIAN_POINT('Ctrl Pts',(18.1272,109.267121428251,2.35538886897266));
#70110=CARTESIAN_POINT('',(18.3,109.534515613317,2.18240113966167));
#70111=CARTESIAN_POINT('Ctrl Pts',(18.3,109.534515613317,2.18240113966167));
#70112=CARTESIAN_POINT('Ctrl Pts',(18.3,109.361528033018,2.24024551026523));
#70113=CARTESIAN_POINT('Ctrl Pts',(18.3,109.267121428251,2.35538886897266));
#70114=CARTESIAN_POINT('',(18.18,109.534515613317,2.18240113966167));
#70115=CARTESIAN_POINT('',(18.3,109.534515613317,2.18240113966167));
#70116=CARTESIAN_POINT('Ctrl Pts',(18.18,109.534515613317,2.18240113966167));
#70117=CARTESIAN_POINT('Ctrl Pts',(18.18,109.361528033018,2.24024551026523));
#70118=CARTESIAN_POINT('Ctrl Pts',(18.18,109.267121428251,2.35538886897266));
#70119=CARTESIAN_POINT('Ctrl Pts',(18.3,109.989085966349,2.12455647103488));
#70120=CARTESIAN_POINT('Ctrl Pts',(18.1272,109.989085966349,2.12455647103488));
#70121=CARTESIAN_POINT('Ctrl Pts',(18.3,109.70750349164,2.12455647103488));
#70122=CARTESIAN_POINT('Ctrl Pts',(18.1272,109.70750349164,2.12455647103488));
#70123=CARTESIAN_POINT('Ctrl Pts',(18.3,109.534515613317,2.18240113966167));
#70124=CARTESIAN_POINT('Ctrl Pts',(18.1272,109.534515613317,2.18240113966167));
#70125=CARTESIAN_POINT('',(18.3,109.989085966349,2.12455647103488));
#70126=CARTESIAN_POINT('Ctrl Pts',(18.3,109.989085966349,2.12455647103488));
#70127=CARTESIAN_POINT('Ctrl Pts',(18.3,109.70750349164,2.12455647103488));
#70128=CARTESIAN_POINT('Ctrl Pts',(18.3,109.534515613317,2.18240113966167));
#70129=CARTESIAN_POINT('',(18.18,109.989085966349,2.12455647103488));
#70130=CARTESIAN_POINT('',(18.3,109.989085966349,2.12455647103488));
#70131=CARTESIAN_POINT('Ctrl Pts',(18.18,109.989085966349,2.12455647103488));
#70132=CARTESIAN_POINT('Ctrl Pts',(18.18,109.70750349164,2.12455647103488));
#70133=CARTESIAN_POINT('Ctrl Pts',(18.18,109.534515613317,2.18240113966167));
#70134=CARTESIAN_POINT('Ctrl Pts',(18.3,110.367257767916,2.16057302467525));
#70135=CARTESIAN_POINT('Ctrl Pts',(18.1272,110.367257767916,2.16057302467525));
#70136=CARTESIAN_POINT('Ctrl Pts',(18.3,110.227012211084,2.12455647103488));
#70137=CARTESIAN_POINT('Ctrl Pts',(18.1272,110.227012211084,2.12455647103488));
#70138=CARTESIAN_POINT('Ctrl Pts',(18.3,109.989085966349,2.12455647103488));
#70139=CARTESIAN_POINT('Ctrl Pts',(18.1272,109.989085966349,2.12455647103488));
#70140=CARTESIAN_POINT('',(18.3,110.367257767916,2.16057302467525));
#70141=CARTESIAN_POINT('Ctrl Pts',(18.3,110.367257767916,2.16057302467525));
#70142=CARTESIAN_POINT('Ctrl Pts',(18.3,110.227012211084,2.12455647103488));
#70143=CARTESIAN_POINT('Ctrl Pts',(18.3,109.989085966349,2.12455647103488));
#70144=CARTESIAN_POINT('',(18.18,110.367257767916,2.16057302467525));
#70145=CARTESIAN_POINT('',(18.3,110.367257767916,2.16057302467525));
#70146=CARTESIAN_POINT('Ctrl Pts',(18.18,110.367257767916,2.16057302467525));
#70147=CARTESIAN_POINT('Ctrl Pts',(18.18,110.227012211084,2.12455647103488));
#70148=CARTESIAN_POINT('Ctrl Pts',(18.18,109.989085966349,2.12455647103488));
#70149=CARTESIAN_POINT('Ctrl Pts',(18.3,110.605184161663,2.25989090315998));
#70150=CARTESIAN_POINT('Ctrl Pts',(18.1272,110.605184161663,2.25989090315998));
#70151=CARTESIAN_POINT('Ctrl Pts',(18.3,110.507503473759,2.19658928029239));
#70152=CARTESIAN_POINT('Ctrl Pts',(18.1272,110.507503473759,2.19658928029239));
#70153=CARTESIAN_POINT('Ctrl Pts',(18.3,110.367257767916,2.16057302467525));
#70154=CARTESIAN_POINT('Ctrl Pts',(18.1272,110.367257767916,2.16057302467525));
#70155=CARTESIAN_POINT('',(18.3,110.605184161663,2.25989090315998));
#70156=CARTESIAN_POINT('Ctrl Pts',(18.3,110.605184161663,2.25989090315998));
#70157=CARTESIAN_POINT('Ctrl Pts',(18.3,110.507503473759,2.19658928029239));
#70158=CARTESIAN_POINT('Ctrl Pts',(18.3,110.367257767916,2.16057302467525));
#70159=CARTESIAN_POINT('',(18.18,110.605184161663,2.25989090315998));
#70160=CARTESIAN_POINT('',(18.3,110.605184161663,2.25989090315998));
#70161=CARTESIAN_POINT('Ctrl Pts',(18.18,110.605184161663,2.25989090315998));
#70162=CARTESIAN_POINT('Ctrl Pts',(18.18,110.507503473759,2.19658928029239));
#70163=CARTESIAN_POINT('Ctrl Pts',(18.18,110.367257767916,2.16057302467525));
#70164=CARTESIAN_POINT('Ctrl Pts',(18.3,110.754706734419,2.420327533409));
#70165=CARTESIAN_POINT('Ctrl Pts',(18.1272,110.754706734419,2.420327533409));
#70166=CARTESIAN_POINT('Ctrl Pts',(18.3,110.702864998579,2.32319237701595));
#70167=CARTESIAN_POINT('Ctrl Pts',(18.1272,110.702864998579,2.32319237701595));
#70168=CARTESIAN_POINT('Ctrl Pts',(18.3,110.605184161663,2.25989090315998));
#70169=CARTESIAN_POINT('Ctrl Pts',(18.1272,110.605184161663,2.25989090315998));
#70170=CARTESIAN_POINT('',(18.3,110.754706734419,2.420327533409));
#70171=CARTESIAN_POINT('Ctrl Pts',(18.3,110.754706734419,2.420327533409));
#70172=CARTESIAN_POINT('Ctrl Pts',(18.3,110.702864998579,2.32319237701595));
#70173=CARTESIAN_POINT('Ctrl Pts',(18.3,110.605184161663,2.25989090315998));
#70174=CARTESIAN_POINT('',(18.18,110.754706734419,2.420327533409));
#70175=CARTESIAN_POINT('',(18.3,110.754706734419,2.420327533409));
#70176=CARTESIAN_POINT('Ctrl Pts',(18.18,110.754706734419,2.420327533409));
#70177=CARTESIAN_POINT('Ctrl Pts',(18.18,110.702864998579,2.32319237701595));
#70178=CARTESIAN_POINT('Ctrl Pts',(18.18,110.605184161663,2.25989090315998));
#70179=CARTESIAN_POINT('Ctrl Pts',(18.3,110.806548470259,2.64624821059406));
#70180=CARTESIAN_POINT('Ctrl Pts',(18.1272,110.806548470259,2.64624821059406));
#70181=CARTESIAN_POINT('Ctrl Pts',(18.3,110.806548470259,2.51746254079044));
#70182=CARTESIAN_POINT('Ctrl Pts',(18.1272,110.806548470259,2.51746254079044));
#70183=CARTESIAN_POINT('Ctrl Pts',(18.3,110.754706734419,2.420327533409));
#70184=CARTESIAN_POINT('Ctrl Pts',(18.1272,110.754706734419,2.420327533409));
#70185=CARTESIAN_POINT('',(18.3,110.806548470259,2.64624821059406));
#70186=CARTESIAN_POINT('Ctrl Pts',(18.3,110.806548470259,2.64624821059406));
#70187=CARTESIAN_POINT('Ctrl Pts',(18.3,110.806548470259,2.51746254079044));
#70188=CARTESIAN_POINT('Ctrl Pts',(18.3,110.754706734419,2.420327533409));
#70189=CARTESIAN_POINT('',(18.18,110.806548470259,2.64624821059406));
#70190=CARTESIAN_POINT('',(18.3,110.806548470259,2.64624821059406));
#70191=CARTESIAN_POINT('Ctrl Pts',(18.18,110.806548470259,2.64624821059406));
#70192=CARTESIAN_POINT('Ctrl Pts',(18.18,110.806548470259,2.51746254079044));
#70193=CARTESIAN_POINT('Ctrl Pts',(18.18,110.754706734419,2.420327533409));
#70194=CARTESIAN_POINT('Ctrl Pts',(18.3,110.712687695026,2.93601634018123));
#70195=CARTESIAN_POINT('Ctrl Pts',(18.1272,110.712687695026,2.93601634018123));
#70196=CARTESIAN_POINT('Ctrl Pts',(18.3,110.806548470259,2.82087313048542));
#70197=CARTESIAN_POINT('Ctrl Pts',(18.1272,110.806548470259,2.82087313048542));
#70198=CARTESIAN_POINT('Ctrl Pts',(18.3,110.806548470259,2.64624821059406));
#70199=CARTESIAN_POINT('Ctrl Pts',(18.1272,110.806548470259,2.64624821059406));
#70200=CARTESIAN_POINT('',(18.3,110.712687695026,2.93601634018123));
#70201=CARTESIAN_POINT('Ctrl Pts',(18.3,110.712687695026,2.93601634018123));
#70202=CARTESIAN_POINT('Ctrl Pts',(18.3,110.806548470259,2.82087313048542));
#70203=CARTESIAN_POINT('Ctrl Pts',(18.3,110.806548470259,2.64624821059406));
#70204=CARTESIAN_POINT('',(18.18,110.712687695026,2.93601634018123));
#70205=CARTESIAN_POINT('',(18.3,110.712687695026,2.93601634018123));
#70206=CARTESIAN_POINT('Ctrl Pts',(18.18,110.712687695026,2.93601634018123));
#70207=CARTESIAN_POINT('Ctrl Pts',(18.18,110.806548470259,2.82087313048542));
#70208=CARTESIAN_POINT('Ctrl Pts',(18.18,110.806548470259,2.64624821059406));
#70209=CARTESIAN_POINT('Ctrl Pts',(18.3,110.445839041471,3.10954975001514));
#70210=CARTESIAN_POINT('Ctrl Pts',(18.1272,110.445839041471,3.10954975001514));
#70211=CARTESIAN_POINT('Ctrl Pts',(18.3,110.618826770782,3.05115954987705));
#70212=CARTESIAN_POINT('Ctrl Pts',(18.1272,110.618826770782,3.05115954987705));
#70213=CARTESIAN_POINT('Ctrl Pts',(18.3,110.712687695026,2.93601634018123));
#70214=CARTESIAN_POINT('Ctrl Pts',(18.1272,110.712687695026,2.93601634018123));
#70215=CARTESIAN_POINT('',(18.3,110.445839041471,3.10954975001514));
#70216=CARTESIAN_POINT('Ctrl Pts',(18.3,110.445839041471,3.10954975001514));
#70217=CARTESIAN_POINT('Ctrl Pts',(18.3,110.618826770782,3.05115954987705));
#70218=CARTESIAN_POINT('Ctrl Pts',(18.3,110.712687695026,2.93601634018123));
#70219=CARTESIAN_POINT('',(18.18,110.445839041471,3.10954975001514));
#70220=CARTESIAN_POINT('',(18.3,110.445839041471,3.10954975001514));
#70221=CARTESIAN_POINT('Ctrl Pts',(18.18,110.445839041471,3.10954975001514));
#70222=CARTESIAN_POINT('Ctrl Pts',(18.18,110.618826770782,3.05115954987705));
#70223=CARTESIAN_POINT('Ctrl Pts',(18.18,110.712687695026,2.93601634018123));
#70224=CARTESIAN_POINT('Ctrl Pts',(18.3,109.989085966349,3.16793995015323));
#70225=CARTESIAN_POINT('Ctrl Pts',(18.1272,109.989085966349,3.16793995015323));
#70226=CARTESIAN_POINT('Ctrl Pts',(18.3,110.27285131216,3.16793995015323));
#70227=CARTESIAN_POINT('Ctrl Pts',(18.1272,110.27285131216,3.16793995015323));
#70228=CARTESIAN_POINT('Ctrl Pts',(18.3,110.445839041471,3.10954975001514));
#70229=CARTESIAN_POINT('Ctrl Pts',(18.1272,110.445839041471,3.10954975001514));
#70230=CARTESIAN_POINT('',(18.3,109.989085966349,3.16793995015323));
#70231=CARTESIAN_POINT('Ctrl Pts',(18.3,109.989085966349,3.16793995015323));
#70232=CARTESIAN_POINT('Ctrl Pts',(18.3,110.27285131216,3.16793995015323));
#70233=CARTESIAN_POINT('Ctrl Pts',(18.3,110.445839041471,3.10954975001514));
#70234=CARTESIAN_POINT('',(18.18,109.989085966349,3.16793995015323));
#70235=CARTESIAN_POINT('',(18.3,109.989085966349,3.16793995015323));
#70236=CARTESIAN_POINT('Ctrl Pts',(18.18,109.989085966349,3.16793995015323));
#70237=CARTESIAN_POINT('Ctrl Pts',(18.18,110.27285131216,3.16793995015323));
#70238=CARTESIAN_POINT('Ctrl Pts',(18.18,110.445839041471,3.10954975001514));
#70239=CARTESIAN_POINT('Ctrl Pts',(18.3,109.338608556986,3.00968619100749));
#70240=CARTESIAN_POINT('Ctrl Pts',(18.1272,109.338608556986,3.00968619100749));
#70241=CARTESIAN_POINT('Ctrl Pts',(18.3,109.538335675001,3.16793995015323));
#70242=CARTESIAN_POINT('Ctrl Pts',(18.1272,109.538335675001,3.16793995015323));
#70243=CARTESIAN_POINT('Ctrl Pts',(18.3,109.989085966349,3.16793995015323));
#70244=CARTESIAN_POINT('Ctrl Pts',(18.1272,109.989085966349,3.16793995015323));
#70245=CARTESIAN_POINT('Ctrl Pts',(18.3,109.338608556986,3.00968619100749));
#70246=CARTESIAN_POINT('Ctrl Pts',(18.3,109.538335675001,3.16793995015323));
#70247=CARTESIAN_POINT('Ctrl Pts',(18.3,109.989085966349,3.16793995015323));
#70248=CARTESIAN_POINT('Ctrl Pts',(18.18,109.338608556986,3.00968619100749));
#70249=CARTESIAN_POINT('Ctrl Pts',(18.18,109.538335675001,3.16793995015323));
#70250=CARTESIAN_POINT('Ctrl Pts',(18.18,109.989085966349,3.16793995015323));
#70251=CARTESIAN_POINT('Origin',(18.18,109.989631646872,3.29999987538904));
#70252=CARTESIAN_POINT('Origin',(18.3,110.484583848715,3.78130966834724));
#70253=CARTESIAN_POINT('',(18.3,110.484583848715,3.78130966834724));
#70254=CARTESIAN_POINT('',(18.3,109.76316499114,4.28226457946002));
#70255=CARTESIAN_POINT('',(18.3,96.4250103615061,13.5443097793353));
#70256=CARTESIAN_POINT('',(18.18,110.484583848715,3.78130966834724));
#70257=CARTESIAN_POINT('',(18.3,110.484583848715,3.78130966834724));
#70258=CARTESIAN_POINT('',(18.18,109.76316499114,4.28226457946002));
#70259=CARTESIAN_POINT('',(18.18,110.484583848715,3.78130966834724));
#70260=CARTESIAN_POINT('',(18.3,109.76316499114,4.28226457946002));
#70261=CARTESIAN_POINT('Origin',(18.3,109.76316499114,3.78130966834724));
#70262=CARTESIAN_POINT('',(18.3,109.76316499114,3.78130966834724));
#70263=CARTESIAN_POINT('',(18.3,89.8815824955702,3.78130966834724));
#70264=CARTESIAN_POINT('',(18.18,109.76316499114,3.78130966834724));
#70265=CARTESIAN_POINT('',(18.3,109.76316499114,3.78130966834724));
#70266=CARTESIAN_POINT('',(18.18,109.76316499114,3.78130966834724));
#70267=CARTESIAN_POINT('Origin',(18.3,109.76316499114,4.28226457946002));
#70268=CARTESIAN_POINT('',(18.3,109.76316499114,4.89113228973001));
#70269=CARTESIAN_POINT('',(18.18,109.76316499114,4.28226457946002));
#70270=CARTESIAN_POINT('Origin',(18.3,109.58308326602,3.58485670797527));
#70271=CARTESIAN_POINT('',(18.3,109.58308326602,3.58485670797527));
#70272=CARTESIAN_POINT('',(18.3,109.200000041723,3.58485670797527));
#70273=CARTESIAN_POINT('',(18.3,89.7915416330099,3.58485670797527));
#70274=CARTESIAN_POINT('',(18.18,109.58308326602,3.58485670797527));
#70275=CARTESIAN_POINT('',(18.3,109.58308326602,3.58485670797527));
#70276=CARTESIAN_POINT('',(18.18,109.200000041723,3.58485670797527));
#70277=CARTESIAN_POINT('',(18.18,109.58308326602,3.58485670797527));
#70278=CARTESIAN_POINT('',(18.3,109.200000041723,3.58485670797527));
#70279=CARTESIAN_POINT('Origin',(18.3,109.58308326602,3.36875842921436));
#70280=CARTESIAN_POINT('',(18.3,109.58308326602,3.36875842921436));
#70281=CARTESIAN_POINT('',(18.3,109.58308326602,4.43437921460718));
#70282=CARTESIAN_POINT('',(18.18,109.58308326602,3.36875842921436));
#70283=CARTESIAN_POINT('',(18.3,109.58308326602,3.36875842921436));
#70284=CARTESIAN_POINT('',(18.18,109.58308326602,3.36875842921436));
#70285=CARTESIAN_POINT('Origin',(18.3,109.76316499114,3.36875842921436));
#70286=CARTESIAN_POINT('',(18.3,109.76316499114,3.36875842921436));
#70287=CARTESIAN_POINT('',(18.3,89.8815824955702,3.36875842921436));
#70288=CARTESIAN_POINT('',(18.18,109.76316499114,3.36875842921436));
#70289=CARTESIAN_POINT('',(18.3,109.76316499114,3.36875842921436));
#70290=CARTESIAN_POINT('',(18.18,109.76316499114,3.36875842921436));
#70291=CARTESIAN_POINT('Origin',(18.3,109.76316499114,3.58485670797527));
#70292=CARTESIAN_POINT('',(18.3,109.76316499114,3.58485670797527));
#70293=CARTESIAN_POINT('',(18.3,109.76316499114,4.54242835398763));
#70294=CARTESIAN_POINT('',(18.18,109.76316499114,3.58485670797527));
#70295=CARTESIAN_POINT('',(18.3,109.76316499114,3.58485670797527));
#70296=CARTESIAN_POINT('',(18.18,109.76316499114,3.58485670797527));
#70297=CARTESIAN_POINT('Origin',(18.3,110.80000000596,3.58485670797527));
#70298=CARTESIAN_POINT('',(18.3,110.80000000596,3.58485670797527));
#70299=CARTESIAN_POINT('',(18.3,90.4000000029802,3.58485670797527));
#70300=CARTESIAN_POINT('',(18.18,110.80000000596,3.58485670797527));
#70301=CARTESIAN_POINT('',(18.3,110.80000000596,3.58485670797527));
#70302=CARTESIAN_POINT('',(18.18,110.80000000596,3.58485670797527));
#70303=CARTESIAN_POINT('Origin',(18.3,110.80000000596,3.74529326371849));
#70304=CARTESIAN_POINT('',(18.3,110.80000000596,3.74529326371849));
#70305=CARTESIAN_POINT('',(18.3,110.80000000596,4.62264663185924));
#70306=CARTESIAN_POINT('',(18.18,110.80000000596,3.74529326371849));
#70307=CARTESIAN_POINT('',(18.3,110.80000000596,3.74529326371849));
#70308=CARTESIAN_POINT('',(18.18,110.80000000596,3.74529326371849));
#70309=CARTESIAN_POINT('Origin',(18.3,109.76316499114,4.47544327974319));
#70310=CARTESIAN_POINT('',(18.3,109.76316499114,4.47544327974319));
#70311=CARTESIAN_POINT('',(18.3,96.2313997020141,14.0046533290512));
#70312=CARTESIAN_POINT('',(18.18,109.76316499114,4.47544327974319));
#70313=CARTESIAN_POINT('',(18.3,109.76316499114,4.47544327974319));
#70314=CARTESIAN_POINT('',(18.18,109.76316499114,4.47544327974319));
#70315=CARTESIAN_POINT('Origin',(18.3,109.58308326602,4.47544327974319));
#70316=CARTESIAN_POINT('',(18.3,109.58308326602,4.47544327974319));
#70317=CARTESIAN_POINT('',(18.3,89.7915416330099,4.47544327974319));
#70318=CARTESIAN_POINT('',(18.18,109.58308326602,4.47544327974319));
#70319=CARTESIAN_POINT('',(18.3,109.58308326602,4.47544327974319));
#70320=CARTESIAN_POINT('',(18.18,109.58308326602,4.47544327974319));
#70321=CARTESIAN_POINT('Origin',(18.3,109.58308326602,3.78130966834724));
#70322=CARTESIAN_POINT('',(18.3,109.58308326602,3.78130966834724));
#70323=CARTESIAN_POINT('',(18.3,109.58308326602,4.64065483417362));
#70324=CARTESIAN_POINT('',(18.18,109.58308326602,3.78130966834724));
#70325=CARTESIAN_POINT('',(18.3,109.58308326602,3.78130966834724));
#70326=CARTESIAN_POINT('',(18.18,109.58308326602,3.78130966834724));
#70327=CARTESIAN_POINT('Origin',(18.3,109.200000041723,3.78130966834724));
#70328=CARTESIAN_POINT('',(18.3,109.200000041723,3.78130966834724));
#70329=CARTESIAN_POINT('',(18.3,89.6000000208616,3.78130966834724));
#70330=CARTESIAN_POINT('',(18.18,109.200000041723,3.78130966834724));
#70331=CARTESIAN_POINT('',(18.3,109.200000041723,3.78130966834724));
#70332=CARTESIAN_POINT('',(18.18,109.200000041723,3.78130966834724));
#70333=CARTESIAN_POINT('Origin',(18.3,109.200000041723,3.58485670797527));
#70334=CARTESIAN_POINT('',(18.3,109.200000041723,4.54242835398763));
#70335=CARTESIAN_POINT('',(18.18,109.200000041723,3.58485670797527));
#70336=CARTESIAN_POINT('Origin',(18.18,109.989631646872,3.29999987538904));
#70337=CARTESIAN_POINT('Origin',(18.3,70.,5.5));
#70338=CARTESIAN_POINT('Origin',(18.3,70.,5.5));
#70339=CARTESIAN_POINT('Ctrl Pts',(18.3,100.643929117918,2.68117321692407));
#70340=CARTESIAN_POINT('Ctrl Pts',(18.1272,100.643929117918,2.68117321692407));
#70341=CARTESIAN_POINT('Ctrl Pts',(18.3,100.643929117918,2.81650750003755));
#70342=CARTESIAN_POINT('Ctrl Pts',(18.1272,100.643929117918,2.81650750003755));
#70343=CARTESIAN_POINT('Ctrl Pts',(18.3,100.529331588745,2.89727149568498));
#70344=CARTESIAN_POINT('Ctrl Pts',(18.1272,100.529331588745,2.89727149568498));
#70345=CARTESIAN_POINT('',(18.3,100.643929117918,2.68117321692407));
#70346=CARTESIAN_POINT('',(18.3,100.529331588745,2.89727149568498));
#70347=CARTESIAN_POINT('Ctrl Pts',(18.3,100.643929117918,2.68117321692407));
#70348=CARTESIAN_POINT('Ctrl Pts',(18.3,100.643929117918,2.81650750003755));
#70349=CARTESIAN_POINT('Ctrl Pts',(18.3,100.529331588745,2.89727149568498));
#70350=CARTESIAN_POINT('',(18.18,100.643929117918,2.68117321692407));
#70351=CARTESIAN_POINT('',(18.3,100.643929117918,2.68117321692407));
#70352=CARTESIAN_POINT('',(18.18,100.529331588745,2.89727149568498));
#70353=CARTESIAN_POINT('Ctrl Pts',(18.18,100.643929117918,2.68117321692407));
#70354=CARTESIAN_POINT('Ctrl Pts',(18.18,100.643929117918,2.81650750003755));
#70355=CARTESIAN_POINT('Ctrl Pts',(18.18,100.529331588745,2.89727149568498));
#70356=CARTESIAN_POINT('',(18.3,100.529331588745,2.89727149568498));
#70357=CARTESIAN_POINT('Ctrl Pts',(18.3,100.514051938057,2.45143247805536));
#70358=CARTESIAN_POINT('Ctrl Pts',(18.1272,100.514051938057,2.45143247805536));
#70359=CARTESIAN_POINT('Ctrl Pts',(18.3,100.643929117918,2.54365621171892));
#70360=CARTESIAN_POINT('Ctrl Pts',(18.1272,100.643929117918,2.54365621171892));
#70361=CARTESIAN_POINT('Ctrl Pts',(18.3,100.643929117918,2.68117321692407));
#70362=CARTESIAN_POINT('Ctrl Pts',(18.1272,100.643929117918,2.68117321692407));
#70363=CARTESIAN_POINT('',(18.3,100.514051938057,2.45143247805536));
#70364=CARTESIAN_POINT('Ctrl Pts',(18.3,100.514051938057,2.45143247805536));
#70365=CARTESIAN_POINT('Ctrl Pts',(18.3,100.643929117918,2.54365621171892));
#70366=CARTESIAN_POINT('Ctrl Pts',(18.3,100.643929117918,2.68117321692407));
#70367=CARTESIAN_POINT('',(18.18,100.514051938057,2.45143247805536));
#70368=CARTESIAN_POINT('',(18.3,100.514051938057,2.45143247805536));
#70369=CARTESIAN_POINT('Ctrl Pts',(18.18,100.514051938057,2.45143247805536));
#70370=CARTESIAN_POINT('Ctrl Pts',(18.18,100.643929117918,2.54365621171892));
#70371=CARTESIAN_POINT('Ctrl Pts',(18.18,100.643929117918,2.68117321692407));
#70372=CARTESIAN_POINT('Ctrl Pts',(18.3,99.9890859663486,2.3592087443918));
#70373=CARTESIAN_POINT('Ctrl Pts',(18.1272,99.9890859663486,2.3592087443918));
#70374=CARTESIAN_POINT('Ctrl Pts',(18.3,100.384174609184,2.3592087443918));
#70375=CARTESIAN_POINT('Ctrl Pts',(18.1272,100.384174609184,2.3592087443918));
#70376=CARTESIAN_POINT('Ctrl Pts',(18.3,100.514051938057,2.45143247805536));
#70377=CARTESIAN_POINT('Ctrl Pts',(18.1272,100.514051938057,2.45143247805536));
#70378=CARTESIAN_POINT('',(18.3,99.9890859663486,2.3592087443918));
#70379=CARTESIAN_POINT('Ctrl Pts',(18.3,99.9890859663486,2.3592087443918));
#70380=CARTESIAN_POINT('Ctrl Pts',(18.3,100.384174609184,2.3592087443918));
#70381=CARTESIAN_POINT('Ctrl Pts',(18.3,100.514051938057,2.45143247805536));
#70382=CARTESIAN_POINT('',(18.18,99.9890859663486,2.3592087443918));
#70383=CARTESIAN_POINT('',(18.3,99.9890859663486,2.3592087443918));
#70384=CARTESIAN_POINT('Ctrl Pts',(18.18,99.9890859663486,2.3592087443918));
#70385=CARTESIAN_POINT('Ctrl Pts',(18.18,100.384174609184,2.3592087443918));
#70386=CARTESIAN_POINT('Ctrl Pts',(18.18,100.514051938057,2.45143247805536));
#70387=CARTESIAN_POINT('Ctrl Pts',(18.3,99.4652115046978,2.45143247805536));
#70388=CARTESIAN_POINT('Ctrl Pts',(18.1272,99.4652115046978,2.45143247805536));
#70389=CARTESIAN_POINT('Ctrl Pts',(18.3,99.5961801946163,2.3592087443918));
#70390=CARTESIAN_POINT('Ctrl Pts',(18.1272,99.5961801946163,2.3592087443918));
#70391=CARTESIAN_POINT('Ctrl Pts',(18.3,99.9890859663486,2.3592087443918));
#70392=CARTESIAN_POINT('Ctrl Pts',(18.1272,99.9890859663486,2.3592087443918));
#70393=CARTESIAN_POINT('',(18.3,99.4652115046978,2.45143247805536));
#70394=CARTESIAN_POINT('Ctrl Pts',(18.3,99.4652115046978,2.45143247805536));
#70395=CARTESIAN_POINT('Ctrl Pts',(18.3,99.5961801946163,2.3592087443918));
#70396=CARTESIAN_POINT('Ctrl Pts',(18.3,99.9890859663486,2.3592087443918));
#70397=CARTESIAN_POINT('',(18.18,99.4652115046978,2.45143247805536));
#70398=CARTESIAN_POINT('',(18.3,99.4652115046978,2.45143247805536));
#70399=CARTESIAN_POINT('Ctrl Pts',(18.18,99.4652115046978,2.45143247805536));
#70400=CARTESIAN_POINT('Ctrl Pts',(18.18,99.5961801946163,2.3592087443918));
#70401=CARTESIAN_POINT('Ctrl Pts',(18.18,99.9890859663486,2.3592087443918));
#70402=CARTESIAN_POINT('Ctrl Pts',(18.3,99.3342428147793,2.67899034582078));
#70403=CARTESIAN_POINT('Ctrl Pts',(18.1272,99.3342428147793,2.67899034582078));
#70404=CARTESIAN_POINT('Ctrl Pts',(18.3,99.3342428147793,2.54365621171892));
#70405=CARTESIAN_POINT('Ctrl Pts',(18.1272,99.3342428147793,2.54365621171892));
#70406=CARTESIAN_POINT('Ctrl Pts',(18.3,99.4652115046978,2.45143247805536));
#70407=CARTESIAN_POINT('Ctrl Pts',(18.1272,99.4652115046978,2.45143247805536));
#70408=CARTESIAN_POINT('',(18.3,99.3342428147793,2.67899034582078));
#70409=CARTESIAN_POINT('Ctrl Pts',(18.3,99.3342428147793,2.67899034582078));
#70410=CARTESIAN_POINT('Ctrl Pts',(18.3,99.3342428147793,2.54365621171892));
#70411=CARTESIAN_POINT('Ctrl Pts',(18.3,99.4652115046978,2.45143247805536));
#70412=CARTESIAN_POINT('',(18.18,99.3342428147793,2.67899034582078));
#70413=CARTESIAN_POINT('',(18.3,99.3342428147793,2.67899034582078));
#70414=CARTESIAN_POINT('Ctrl Pts',(18.18,99.3342428147793,2.67899034582078));
#70415=CARTESIAN_POINT('Ctrl Pts',(18.18,99.3342428147793,2.54365621171892));
#70416=CARTESIAN_POINT('Ctrl Pts',(18.18,99.4652115046978,2.45143247805536));
#70417=CARTESIAN_POINT('Ctrl Pts',(18.3,99.4646658241749,2.90654836259782));
#70418=CARTESIAN_POINT('Ctrl Pts',(18.1272,99.4646658241749,2.90654836259782));
#70419=CARTESIAN_POINT('Ctrl Pts',(18.3,99.3342428147793,2.81432462893426));
#70420=CARTESIAN_POINT('Ctrl Pts',(18.1272,99.3342428147793,2.81432462893426));
#70421=CARTESIAN_POINT('Ctrl Pts',(18.3,99.3342428147793,2.67899034582078));
#70422=CARTESIAN_POINT('Ctrl Pts',(18.1272,99.3342428147793,2.67899034582078));
#70423=CARTESIAN_POINT('',(18.3,99.4646658241749,2.90654836259782));
#70424=CARTESIAN_POINT('Ctrl Pts',(18.3,99.4646658241749,2.90654836259782));
#70425=CARTESIAN_POINT('Ctrl Pts',(18.3,99.3342428147793,2.81432462893426));
#70426=CARTESIAN_POINT('Ctrl Pts',(18.3,99.3342428147793,2.67899034582078));
#70427=CARTESIAN_POINT('',(18.18,99.4646658241749,2.90654836259782));
#70428=CARTESIAN_POINT('',(18.3,99.4646658241749,2.90654836259782));
#70429=CARTESIAN_POINT('Ctrl Pts',(18.18,99.4646658241749,2.90654836259782));
#70430=CARTESIAN_POINT('Ctrl Pts',(18.18,99.3342428147793,2.81432462893426));
#70431=CARTESIAN_POINT('Ctrl Pts',(18.18,99.3342428147793,2.67899034582078));
#70432=CARTESIAN_POINT('Ctrl Pts',(18.3,99.9890859663486,2.99877209626138));
#70433=CARTESIAN_POINT('Ctrl Pts',(18.1272,99.9890859663486,2.99877209626138));
#70434=CARTESIAN_POINT('Ctrl Pts',(18.3,99.5950888335705,2.99877209626138));
#70435=CARTESIAN_POINT('Ctrl Pts',(18.1272,99.5950888335705,2.99877209626138));
#70436=CARTESIAN_POINT('Ctrl Pts',(18.3,99.4646658241749,2.90654836259782));
#70437=CARTESIAN_POINT('Ctrl Pts',(18.1272,99.4646658241749,2.90654836259782));
#70438=CARTESIAN_POINT('',(18.3,99.9890859663486,2.99877209626138));
#70439=CARTESIAN_POINT('Ctrl Pts',(18.3,99.9890859663486,2.99877209626138));
#70440=CARTESIAN_POINT('Ctrl Pts',(18.3,99.5950888335705,2.99877209626138));
#70441=CARTESIAN_POINT('Ctrl Pts',(18.3,99.4646658241749,2.90654836259782));
#70442=CARTESIAN_POINT('',(18.18,99.9890859663486,2.99877209626138));
#70443=CARTESIAN_POINT('',(18.3,99.9890859663486,2.99877209626138));
#70444=CARTESIAN_POINT('Ctrl Pts',(18.18,99.9890859663486,2.99877209626138));
#70445=CARTESIAN_POINT('Ctrl Pts',(18.18,99.5950888335705,2.99877209626138));
#70446=CARTESIAN_POINT('Ctrl Pts',(18.18,99.4646658241749,2.90654836259782));
#70447=CARTESIAN_POINT('Ctrl Pts',(18.3,100.529331588745,2.89727149568498));
#70448=CARTESIAN_POINT('Ctrl Pts',(18.1272,100.529331588745,2.89727149568498));
#70449=CARTESIAN_POINT('Ctrl Pts',(18.3,100.383083099127,2.99877209626138));
#70450=CARTESIAN_POINT('Ctrl Pts',(18.1272,100.383083099127,2.99877209626138));
#70451=CARTESIAN_POINT('Ctrl Pts',(18.3,99.9890859663486,2.99877209626138));
#70452=CARTESIAN_POINT('Ctrl Pts',(18.1272,99.9890859663486,2.99877209626138));
#70453=CARTESIAN_POINT('Ctrl Pts',(18.3,100.529331588745,2.89727149568498));
#70454=CARTESIAN_POINT('Ctrl Pts',(18.3,100.383083099127,2.99877209626138));
#70455=CARTESIAN_POINT('Ctrl Pts',(18.3,99.9890859663486,2.99877209626138));
#70456=CARTESIAN_POINT('Ctrl Pts',(18.18,100.529331588745,2.89727149568498));
#70457=CARTESIAN_POINT('Ctrl Pts',(18.18,100.383083099127,2.99877209626138));
#70458=CARTESIAN_POINT('Ctrl Pts',(18.18,99.9890859663486,2.99877209626138));
#70459=CARTESIAN_POINT('Ctrl Pts',(18.3,99.1727148234844,2.67899034582078));
#70460=CARTESIAN_POINT('Ctrl Pts',(18.1272,99.1727148234844,2.67899034582078));
#70461=CARTESIAN_POINT('Ctrl Pts',(18.3,99.1727148234844,2.91036827526987));
#70462=CARTESIAN_POINT('Ctrl Pts',(18.1272,99.1727148234844,2.91036827526987));
#70463=CARTESIAN_POINT('Ctrl Pts',(18.3,99.3386085569858,3.04242832623422));
#70464=CARTESIAN_POINT('Ctrl Pts',(18.1272,99.3386085569858,3.04242832623422));
#70465=CARTESIAN_POINT('',(18.3,99.1727148234844,2.67899034582078));
#70466=CARTESIAN_POINT('',(18.3,99.3386085569858,3.04242832623422));
#70467=CARTESIAN_POINT('Ctrl Pts',(18.3,99.1727148234844,2.67899034582078));
#70468=CARTESIAN_POINT('Ctrl Pts',(18.3,99.1727148234844,2.91036827526987));
#70469=CARTESIAN_POINT('Ctrl Pts',(18.3,99.3386085569858,3.04242832623422));
#70470=CARTESIAN_POINT('',(18.18,99.1727148234844,2.67899034582078));
#70471=CARTESIAN_POINT('',(18.3,99.1727148234844,2.67899034582078));
#70472=CARTESIAN_POINT('',(18.18,99.3386085569858,3.04242832623422));
#70473=CARTESIAN_POINT('Ctrl Pts',(18.18,99.1727148234844,2.67899034582078));
#70474=CARTESIAN_POINT('Ctrl Pts',(18.18,99.1727148234844,2.91036827526987));
#70475=CARTESIAN_POINT('Ctrl Pts',(18.18,99.3386085569858,3.04242832623422));
#70476=CARTESIAN_POINT('',(18.3,99.3386085569858,3.04242832623422));
#70477=CARTESIAN_POINT('Ctrl Pts',(18.3,99.2671214282513,2.38813100419939));
#70478=CARTESIAN_POINT('Ctrl Pts',(18.1272,99.2671214282513,2.38813100419939));
#70479=CARTESIAN_POINT('Ctrl Pts',(18.3,99.1727148234844,2.5032742138952));
#70480=CARTESIAN_POINT('Ctrl Pts',(18.1272,99.1727148234844,2.5032742138952));
#70481=CARTESIAN_POINT('Ctrl Pts',(18.3,99.1727148234844,2.67899034582078));
#70482=CARTESIAN_POINT('Ctrl Pts',(18.1272,99.1727148234844,2.67899034582078));
#70483=CARTESIAN_POINT('',(18.3,99.2671214282513,2.38813100419939));
#70484=CARTESIAN_POINT('Ctrl Pts',(18.3,99.2671214282513,2.38813100419939));
#70485=CARTESIAN_POINT('Ctrl Pts',(18.3,99.1727148234844,2.5032742138952));
#70486=CARTESIAN_POINT('Ctrl Pts',(18.3,99.1727148234844,2.67899034582078));
#70487=CARTESIAN_POINT('',(18.18,99.2671214282513,2.38813100419939));
#70488=CARTESIAN_POINT('',(18.3,99.2671214282513,2.38813100419939));
#70489=CARTESIAN_POINT('Ctrl Pts',(18.18,99.2671214282513,2.38813100419939));
#70490=CARTESIAN_POINT('Ctrl Pts',(18.18,99.1727148234844,2.5032742138952));
#70491=CARTESIAN_POINT('Ctrl Pts',(18.18,99.1727148234844,2.67899034582078));
#70492=CARTESIAN_POINT('Ctrl Pts',(18.3,99.5345156133175,2.2151432748884));
#70493=CARTESIAN_POINT('Ctrl Pts',(18.1272,99.5345156133175,2.2151432748884));
#70494=CARTESIAN_POINT('Ctrl Pts',(18.3,99.3615280330181,2.27298764549196));
#70495=CARTESIAN_POINT('Ctrl Pts',(18.1272,99.3615280330181,2.27298764549196));
#70496=CARTESIAN_POINT('Ctrl Pts',(18.3,99.2671214282513,2.38813100419939));
#70497=CARTESIAN_POINT('Ctrl Pts',(18.1272,99.2671214282513,2.38813100419939));
#70498=CARTESIAN_POINT('',(18.3,99.5345156133175,2.2151432748884));
#70499=CARTESIAN_POINT('Ctrl Pts',(18.3,99.5345156133175,2.2151432748884));
#70500=CARTESIAN_POINT('Ctrl Pts',(18.3,99.3615280330181,2.27298764549196));
#70501=CARTESIAN_POINT('Ctrl Pts',(18.3,99.2671214282513,2.38813100419939));
#70502=CARTESIAN_POINT('',(18.18,99.5345156133175,2.2151432748884));
#70503=CARTESIAN_POINT('',(18.3,99.5345156133175,2.2151432748884));
#70504=CARTESIAN_POINT('Ctrl Pts',(18.18,99.5345156133175,2.2151432748884));
#70505=CARTESIAN_POINT('Ctrl Pts',(18.18,99.3615280330181,2.27298764549196));
#70506=CARTESIAN_POINT('Ctrl Pts',(18.18,99.2671214282513,2.38813100419939));
#70507=CARTESIAN_POINT('Ctrl Pts',(18.3,99.9890859663486,2.15729875527322));
#70508=CARTESIAN_POINT('Ctrl Pts',(18.1272,99.9890859663486,2.15729875527322));
#70509=CARTESIAN_POINT('Ctrl Pts',(18.3,99.7075034916401,2.15729875527322));
#70510=CARTESIAN_POINT('Ctrl Pts',(18.1272,99.7075034916401,2.15729875527322));
#70511=CARTESIAN_POINT('Ctrl Pts',(18.3,99.5345156133175,2.2151432748884));
#70512=CARTESIAN_POINT('Ctrl Pts',(18.1272,99.5345156133175,2.2151432748884));
#70513=CARTESIAN_POINT('',(18.3,99.9890859663486,2.15729875527322));
#70514=CARTESIAN_POINT('Ctrl Pts',(18.3,99.9890859663486,2.15729875527322));
#70515=CARTESIAN_POINT('Ctrl Pts',(18.3,99.7075034916401,2.15729875527322));
#70516=CARTESIAN_POINT('Ctrl Pts',(18.3,99.5345156133175,2.2151432748884));
#70517=CARTESIAN_POINT('',(18.18,99.9890859663486,2.15729875527322));
#70518=CARTESIAN_POINT('',(18.3,99.9890859663486,2.15729875527322));
#70519=CARTESIAN_POINT('Ctrl Pts',(18.18,99.9890859663486,2.15729875527322));
#70520=CARTESIAN_POINT('Ctrl Pts',(18.18,99.7075034916401,2.15729875527322));
#70521=CARTESIAN_POINT('Ctrl Pts',(18.18,99.5345156133175,2.2151432748884));
#70522=CARTESIAN_POINT('Ctrl Pts',(18.3,100.367257767916,2.19331515990198));
#70523=CARTESIAN_POINT('Ctrl Pts',(18.1272,100.367257767916,2.19331515990198));
#70524=CARTESIAN_POINT('Ctrl Pts',(18.3,100.227012211084,2.15729875527322));
#70525=CARTESIAN_POINT('Ctrl Pts',(18.1272,100.227012211084,2.15729875527322));
#70526=CARTESIAN_POINT('Ctrl Pts',(18.3,99.9890859663486,2.15729875527322));
#70527=CARTESIAN_POINT('Ctrl Pts',(18.1272,99.9890859663486,2.15729875527322));
#70528=CARTESIAN_POINT('',(18.3,100.367257767916,2.19331515990198));
#70529=CARTESIAN_POINT('Ctrl Pts',(18.3,100.367257767916,2.19331515990198));
#70530=CARTESIAN_POINT('Ctrl Pts',(18.3,100.227012211084,2.15729875527322));
#70531=CARTESIAN_POINT('Ctrl Pts',(18.3,99.9890859663486,2.15729875527322));
#70532=CARTESIAN_POINT('',(18.18,100.367257767916,2.19331515990198));
#70533=CARTESIAN_POINT('',(18.3,100.367257767916,2.19331515990198));
#70534=CARTESIAN_POINT('Ctrl Pts',(18.18,100.367257767916,2.19331515990198));
#70535=CARTESIAN_POINT('Ctrl Pts',(18.18,100.227012211084,2.15729875527322));
#70536=CARTESIAN_POINT('Ctrl Pts',(18.18,99.9890859663486,2.15729875527322));
#70537=CARTESIAN_POINT('Ctrl Pts',(18.3,100.605184161663,2.2926330383867));
#70538=CARTESIAN_POINT('Ctrl Pts',(18.1272,100.605184161663,2.2926330383867));
#70539=CARTESIAN_POINT('Ctrl Pts',(18.3,100.507503473759,2.22933141551912));
#70540=CARTESIAN_POINT('Ctrl Pts',(18.1272,100.507503473759,2.22933141551912));
#70541=CARTESIAN_POINT('Ctrl Pts',(18.3,100.367257767916,2.19331515990198));
#70542=CARTESIAN_POINT('Ctrl Pts',(18.1272,100.367257767916,2.19331515990198));
#70543=CARTESIAN_POINT('',(18.3,100.605184161663,2.2926330383867));
#70544=CARTESIAN_POINT('Ctrl Pts',(18.3,100.605184161663,2.2926330383867));
#70545=CARTESIAN_POINT('Ctrl Pts',(18.3,100.507503473759,2.22933141551912));
#70546=CARTESIAN_POINT('Ctrl Pts',(18.3,100.367257767916,2.19331515990198));
#70547=CARTESIAN_POINT('',(18.18,100.605184161663,2.2926330383867));
#70548=CARTESIAN_POINT('',(18.3,100.605184161663,2.2926330383867));
#70549=CARTESIAN_POINT('Ctrl Pts',(18.18,100.605184161663,2.2926330383867));
#70550=CARTESIAN_POINT('Ctrl Pts',(18.18,100.507503473759,2.22933141551912));
#70551=CARTESIAN_POINT('Ctrl Pts',(18.18,100.367257767916,2.19331515990198));
#70552=CARTESIAN_POINT('Ctrl Pts',(18.3,100.754706734419,2.45306966863573));
#70553=CARTESIAN_POINT('Ctrl Pts',(18.1272,100.754706734419,2.45306966863573));
#70554=CARTESIAN_POINT('Ctrl Pts',(18.3,100.702864998579,2.35593451224267));
#70555=CARTESIAN_POINT('Ctrl Pts',(18.1272,100.702864998579,2.35593451224267));
#70556=CARTESIAN_POINT('Ctrl Pts',(18.3,100.605184161663,2.2926330383867));
#70557=CARTESIAN_POINT('Ctrl Pts',(18.1272,100.605184161663,2.2926330383867));
#70558=CARTESIAN_POINT('',(18.3,100.754706734419,2.45306966863573));
#70559=CARTESIAN_POINT('Ctrl Pts',(18.3,100.754706734419,2.45306966863573));
#70560=CARTESIAN_POINT('Ctrl Pts',(18.3,100.702864998579,2.35593451224267));
#70561=CARTESIAN_POINT('Ctrl Pts',(18.3,100.605184161663,2.2926330383867));
#70562=CARTESIAN_POINT('',(18.18,100.754706734419,2.45306966863573));
#70563=CARTESIAN_POINT('',(18.3,100.754706734419,2.45306966863573));
#70564=CARTESIAN_POINT('Ctrl Pts',(18.18,100.754706734419,2.45306966863573));
#70565=CARTESIAN_POINT('Ctrl Pts',(18.18,100.702864998579,2.35593451224267));
#70566=CARTESIAN_POINT('Ctrl Pts',(18.18,100.605184161663,2.2926330383867));
#70567=CARTESIAN_POINT('Ctrl Pts',(18.3,100.806548470259,2.67899034582078));
#70568=CARTESIAN_POINT('Ctrl Pts',(18.1272,100.806548470259,2.67899034582078));
#70569=CARTESIAN_POINT('Ctrl Pts',(18.3,100.806548470259,2.55020467601716));
#70570=CARTESIAN_POINT('Ctrl Pts',(18.1272,100.806548470259,2.55020467601716));
#70571=CARTESIAN_POINT('Ctrl Pts',(18.3,100.754706734419,2.45306966863573));
#70572=CARTESIAN_POINT('Ctrl Pts',(18.1272,100.754706734419,2.45306966863573));
#70573=CARTESIAN_POINT('',(18.3,100.806548470259,2.67899034582078));
#70574=CARTESIAN_POINT('Ctrl Pts',(18.3,100.806548470259,2.67899034582078));
#70575=CARTESIAN_POINT('Ctrl Pts',(18.3,100.806548470259,2.55020467601716));
#70576=CARTESIAN_POINT('Ctrl Pts',(18.3,100.754706734419,2.45306966863573));
#70577=CARTESIAN_POINT('',(18.18,100.806548470259,2.67899034582078));
#70578=CARTESIAN_POINT('',(18.3,100.806548470259,2.67899034582078));
#70579=CARTESIAN_POINT('Ctrl Pts',(18.18,100.806548470259,2.67899034582078));
#70580=CARTESIAN_POINT('Ctrl Pts',(18.18,100.806548470259,2.55020467601716));
#70581=CARTESIAN_POINT('Ctrl Pts',(18.18,100.754706734419,2.45306966863573));
#70582=CARTESIAN_POINT('Ctrl Pts',(18.3,100.712687695026,2.96875847540796));
#70583=CARTESIAN_POINT('Ctrl Pts',(18.1272,100.712687695026,2.96875847540796));
#70584=CARTESIAN_POINT('Ctrl Pts',(18.3,100.806548470259,2.85361526571214));
#70585=CARTESIAN_POINT('Ctrl Pts',(18.1272,100.806548470259,2.85361526571214));
#70586=CARTESIAN_POINT('Ctrl Pts',(18.3,100.806548470259,2.67899034582078));
#70587=CARTESIAN_POINT('Ctrl Pts',(18.1272,100.806548470259,2.67899034582078));
#70588=CARTESIAN_POINT('',(18.3,100.712687695026,2.96875847540796));
#70589=CARTESIAN_POINT('Ctrl Pts',(18.3,100.712687695026,2.96875847540796));
#70590=CARTESIAN_POINT('Ctrl Pts',(18.3,100.806548470259,2.85361526571214));
#70591=CARTESIAN_POINT('Ctrl Pts',(18.3,100.806548470259,2.67899034582078));
#70592=CARTESIAN_POINT('',(18.18,100.712687695026,2.96875847540796));
#70593=CARTESIAN_POINT('',(18.3,100.712687695026,2.96875847540796));
#70594=CARTESIAN_POINT('Ctrl Pts',(18.18,100.712687695026,2.96875847540796));
#70595=CARTESIAN_POINT('Ctrl Pts',(18.18,100.806548470259,2.85361526571214));
#70596=CARTESIAN_POINT('Ctrl Pts',(18.18,100.806548470259,2.67899034582078));
#70597=CARTESIAN_POINT('Ctrl Pts',(18.3,100.445839041471,3.14229188524187));
#70598=CARTESIAN_POINT('Ctrl Pts',(18.1272,100.445839041471,3.14229188524187));
#70599=CARTESIAN_POINT('Ctrl Pts',(18.3,100.618826770782,3.08390168510377));
#70600=CARTESIAN_POINT('Ctrl Pts',(18.1272,100.618826770782,3.08390168510377));
#70601=CARTESIAN_POINT('Ctrl Pts',(18.3,100.712687695026,2.96875847540796));
#70602=CARTESIAN_POINT('Ctrl Pts',(18.1272,100.712687695026,2.96875847540796));
#70603=CARTESIAN_POINT('',(18.3,100.445839041471,3.14229188524187));
#70604=CARTESIAN_POINT('Ctrl Pts',(18.3,100.445839041471,3.14229188524187));
#70605=CARTESIAN_POINT('Ctrl Pts',(18.3,100.618826770782,3.08390168510377));
#70606=CARTESIAN_POINT('Ctrl Pts',(18.3,100.712687695026,2.96875847540796));
#70607=CARTESIAN_POINT('',(18.18,100.445839041471,3.14229188524187));
#70608=CARTESIAN_POINT('',(18.3,100.445839041471,3.14229188524187));
#70609=CARTESIAN_POINT('Ctrl Pts',(18.18,100.445839041471,3.14229188524187));
#70610=CARTESIAN_POINT('Ctrl Pts',(18.18,100.618826770782,3.08390168510377));
#70611=CARTESIAN_POINT('Ctrl Pts',(18.18,100.712687695026,2.96875847540796));
#70612=CARTESIAN_POINT('Ctrl Pts',(18.3,99.9890859663486,3.20068208537996));
#70613=CARTESIAN_POINT('Ctrl Pts',(18.1272,99.9890859663486,3.20068208537996));
#70614=CARTESIAN_POINT('Ctrl Pts',(18.3,100.27285131216,3.20068208537996));
#70615=CARTESIAN_POINT('Ctrl Pts',(18.1272,100.27285131216,3.20068208537996));
#70616=CARTESIAN_POINT('Ctrl Pts',(18.3,100.445839041471,3.14229188524187));
#70617=CARTESIAN_POINT('Ctrl Pts',(18.1272,100.445839041471,3.14229188524187));
#70618=CARTESIAN_POINT('',(18.3,99.9890859663486,3.20068208537996));
#70619=CARTESIAN_POINT('Ctrl Pts',(18.3,99.9890859663486,3.20068208537996));
#70620=CARTESIAN_POINT('Ctrl Pts',(18.3,100.27285131216,3.20068208537996));
#70621=CARTESIAN_POINT('Ctrl Pts',(18.3,100.445839041471,3.14229188524187));
#70622=CARTESIAN_POINT('',(18.18,99.9890859663486,3.20068208537996));
#70623=CARTESIAN_POINT('',(18.3,99.9890859663486,3.20068208537996));
#70624=CARTESIAN_POINT('Ctrl Pts',(18.18,99.9890859663486,3.20068208537996));
#70625=CARTESIAN_POINT('Ctrl Pts',(18.18,100.27285131216,3.20068208537996));
#70626=CARTESIAN_POINT('Ctrl Pts',(18.18,100.445839041471,3.14229188524187));
#70627=CARTESIAN_POINT('Ctrl Pts',(18.3,99.3386085569858,3.04242832623422));
#70628=CARTESIAN_POINT('Ctrl Pts',(18.1272,99.3386085569858,3.04242832623422));
#70629=CARTESIAN_POINT('Ctrl Pts',(18.3,99.5383356750011,3.20068208537996));
#70630=CARTESIAN_POINT('Ctrl Pts',(18.1272,99.5383356750011,3.20068208537996));
#70631=CARTESIAN_POINT('Ctrl Pts',(18.3,99.9890859663486,3.20068208537996));
#70632=CARTESIAN_POINT('Ctrl Pts',(18.1272,99.9890859663486,3.20068208537996));
#70633=CARTESIAN_POINT('Ctrl Pts',(18.3,99.3386085569858,3.04242832623422));
#70634=CARTESIAN_POINT('Ctrl Pts',(18.3,99.5383356750011,3.20068208537996));
#70635=CARTESIAN_POINT('Ctrl Pts',(18.3,99.9890859663486,3.20068208537996));
#70636=CARTESIAN_POINT('Ctrl Pts',(18.18,99.3386085569858,3.04242832623422));
#70637=CARTESIAN_POINT('Ctrl Pts',(18.18,99.5383356750011,3.20068208537996));
#70638=CARTESIAN_POINT('Ctrl Pts',(18.18,99.9890859663486,3.20068208537996));
#70639=CARTESIAN_POINT('Origin',(18.18,99.9890859663486,3.29999992661178));
#70640=CARTESIAN_POINT('Ctrl Pts',(18.3,99.1716234624386,3.93410628698766));
#70641=CARTESIAN_POINT('Ctrl Pts',(18.1272,99.1716234624386,3.93410628698766));
#70642=CARTESIAN_POINT('Ctrl Pts',(18.3,99.1716234624386,4.14474749974906));
#70643=CARTESIAN_POINT('Ctrl Pts',(18.1272,99.1716234624386,4.14474749974906));
#70644=CARTESIAN_POINT('Ctrl Pts',(18.3,99.2971350491047,4.28390165828168));
#70645=CARTESIAN_POINT('Ctrl Pts',(18.1272,99.2971350491047,4.28390165828168));
#70646=CARTESIAN_POINT('',(18.3,99.1716234624386,3.93410628698766));
#70647=CARTESIAN_POINT('',(18.3,99.2971350491047,4.28390165828168));
#70648=CARTESIAN_POINT('Ctrl Pts',(18.3,99.1716234624386,3.93410628698766));
#70649=CARTESIAN_POINT('Ctrl Pts',(18.3,99.1716234624386,4.14474749974906));
#70650=CARTESIAN_POINT('Ctrl Pts',(18.3,99.2971350491047,4.28390165828168));
#70651=CARTESIAN_POINT('',(18.18,99.1716234624386,3.93410628698766));
#70652=CARTESIAN_POINT('',(18.3,99.1716234624386,3.93410628698766));
#70653=CARTESIAN_POINT('',(18.18,99.2971350491047,4.28390165828168));
#70654=CARTESIAN_POINT('Ctrl Pts',(18.18,99.1716234624386,3.93410628698766));
#70655=CARTESIAN_POINT('Ctrl Pts',(18.18,99.1716234624386,4.14474749974906));
#70656=CARTESIAN_POINT('Ctrl Pts',(18.18,99.2971350491047,4.28390165828168));
#70657=CARTESIAN_POINT('',(18.3,99.2971350491047,4.28390165828168));
#70658=CARTESIAN_POINT('Ctrl Pts',(18.3,99.3173261225223,3.54774890504777));
#70659=CARTESIAN_POINT('Ctrl Pts',(18.1272,99.3173261225223,3.54774890504777));
#70660=CARTESIAN_POINT('Ctrl Pts',(18.3,99.1716234624386,3.70054563544691));
#70661=CARTESIAN_POINT('Ctrl Pts',(18.1272,99.1716234624386,3.70054563544691));
#70662=CARTESIAN_POINT('Ctrl Pts',(18.3,99.1716234624386,3.93410628698766));
#70663=CARTESIAN_POINT('Ctrl Pts',(18.1272,99.1716234624386,3.93410628698766));
#70664=CARTESIAN_POINT('',(18.3,99.3173261225223,3.54774890504777));
#70665=CARTESIAN_POINT('Ctrl Pts',(18.3,99.3173261225223,3.54774890504777));
#70666=CARTESIAN_POINT('Ctrl Pts',(18.3,99.1716234624386,3.70054563544691));
#70667=CARTESIAN_POINT('Ctrl Pts',(18.3,99.1716234624386,3.93410628698766));
#70668=CARTESIAN_POINT('',(18.18,99.3173261225223,3.54774890504777));
#70669=CARTESIAN_POINT('',(18.3,99.3173261225223,3.54774890504777));
#70670=CARTESIAN_POINT('Ctrl Pts',(18.18,99.3173261225223,3.54774890504777));
#70671=CARTESIAN_POINT('Ctrl Pts',(18.18,99.1716234624386,3.70054563544691));
#70672=CARTESIAN_POINT('Ctrl Pts',(18.18,99.1716234624386,3.93410628698766));
#70673=CARTESIAN_POINT('Ctrl Pts',(18.3,99.6725784480572,3.39495224915445));
#70674=CARTESIAN_POINT('Ctrl Pts',(18.1272,99.6725784480572,3.39495224915445));
#70675=CARTESIAN_POINT('Ctrl Pts',(18.3,99.4630287826061,3.39495224915445));
#70676=CARTESIAN_POINT('Ctrl Pts',(18.1272,99.4630287826061,3.39495224915445));
#70677=CARTESIAN_POINT('Ctrl Pts',(18.3,99.3173261225223,3.54774890504777));
#70678=CARTESIAN_POINT('Ctrl Pts',(18.1272,99.3173261225223,3.54774890504777));
#70679=CARTESIAN_POINT('',(18.3,99.6725784480572,3.39495224915445));
#70680=CARTESIAN_POINT('Ctrl Pts',(18.3,99.6725784480572,3.39495224915445));
#70681=CARTESIAN_POINT('Ctrl Pts',(18.3,99.4630287826061,3.39495224915445));
#70682=CARTESIAN_POINT('Ctrl Pts',(18.3,99.3173261225223,3.54774890504777));
#70683=CARTESIAN_POINT('',(18.18,99.6725784480572,3.39495224915445));
#70684=CARTESIAN_POINT('',(18.3,99.6725784480572,3.39495224915445));
#70685=CARTESIAN_POINT('Ctrl Pts',(18.18,99.6725784480572,3.39495224915445));
#70686=CARTESIAN_POINT('Ctrl Pts',(18.18,99.4630287826061,3.39495224915445));
#70687=CARTESIAN_POINT('Ctrl Pts',(18.18,99.3173261225223,3.54774890504777));
#70688=CARTESIAN_POINT('Ctrl Pts',(18.3,99.9306957662105,3.47353329919279));
#70689=CARTESIAN_POINT('Ctrl Pts',(18.1272,99.9306957662105,3.47353329919279));
#70690=CARTESIAN_POINT('Ctrl Pts',(18.3,99.8275579750538,3.39495224915445));
#70691=CARTESIAN_POINT('Ctrl Pts',(18.1272,99.8275579750538,3.39495224915445));
#70692=CARTESIAN_POINT('Ctrl Pts',(18.3,99.6725784480572,3.39495224915445));
#70693=CARTESIAN_POINT('Ctrl Pts',(18.1272,99.6725784480572,3.39495224915445));
#70694=CARTESIAN_POINT('',(18.3,99.9306957662105,3.47353329919279));
#70695=CARTESIAN_POINT('Ctrl Pts',(18.3,99.9306957662105,3.47353329919279));
#70696=CARTESIAN_POINT('Ctrl Pts',(18.3,99.8275579750538,3.39495224915445));
#70697=CARTESIAN_POINT('Ctrl Pts',(18.3,99.6725784480572,3.39495224915445));
#70698=CARTESIAN_POINT('',(18.18,99.9306957662105,3.47353329919279));
#70699=CARTESIAN_POINT('',(18.3,99.9306957662105,3.47353329919279));
#70700=CARTESIAN_POINT('Ctrl Pts',(18.18,99.9306957662105,3.47353329919279));
#70701=CARTESIAN_POINT('Ctrl Pts',(18.18,99.8275579750538,3.39495224915445));
#70702=CARTESIAN_POINT('Ctrl Pts',(18.18,99.6725784480572,3.39495224915445));
#70703=CARTESIAN_POINT('Ctrl Pts',(18.3,100.066575729847,3.69399717114866));
#70704=CARTESIAN_POINT('Ctrl Pts',(18.1272,100.066575729847,3.69399717114866));
#70705=CARTESIAN_POINT('Ctrl Pts',(18.3,100.033833557367,3.55211449824274));
#70706=CARTESIAN_POINT('Ctrl Pts',(18.1272,100.033833557367,3.55211449824274));
#70707=CARTESIAN_POINT('Ctrl Pts',(18.3,99.9306957662105,3.47353329919279));
#70708=CARTESIAN_POINT('Ctrl Pts',(18.1272,99.9306957662105,3.47353329919279));
#70709=CARTESIAN_POINT('',(18.3,100.066575729847,3.69399717114866));
#70710=CARTESIAN_POINT('Ctrl Pts',(18.3,100.066575729847,3.69399717114866));
#70711=CARTESIAN_POINT('Ctrl Pts',(18.3,100.033833557367,3.55211449824274));
#70712=CARTESIAN_POINT('Ctrl Pts',(18.3,99.9306957662105,3.47353329919279));
#70713=CARTESIAN_POINT('',(18.18,100.066575729847,3.69399717114866));
#70714=CARTESIAN_POINT('',(18.3,100.066575729847,3.69399717114866));
#70715=CARTESIAN_POINT('Ctrl Pts',(18.18,100.066575729847,3.69399717114866));
#70716=CARTESIAN_POINT('Ctrl Pts',(18.18,100.033833557367,3.55211449824274));
#70717=CARTESIAN_POINT('Ctrl Pts',(18.18,99.9306957662105,3.47353329919279));
#70718=CARTESIAN_POINT('Ctrl Pts',(18.3,100.20191001296,3.52919502221048));
#70719=CARTESIAN_POINT('Ctrl Pts',(18.1272,100.20191001296,3.52919502221048));
#70720=CARTESIAN_POINT('Ctrl Pts',(18.3,100.116780275106,3.58485667072237));
#70721=CARTESIAN_POINT('Ctrl Pts',(18.1272,100.116780275106,3.58485667072237));
#70722=CARTESIAN_POINT('Ctrl Pts',(18.3,100.066575729847,3.69399717114866));
#70723=CARTESIAN_POINT('Ctrl Pts',(18.1272,100.066575729847,3.69399717114866));
#70724=CARTESIAN_POINT('',(18.3,100.20191001296,3.52919502221048));
#70725=CARTESIAN_POINT('Ctrl Pts',(18.3,100.20191001296,3.52919502221048));
#70726=CARTESIAN_POINT('Ctrl Pts',(18.3,100.116780275106,3.58485667072237));
#70727=CARTESIAN_POINT('Ctrl Pts',(18.3,100.066575729847,3.69399717114866));
#70728=CARTESIAN_POINT('',(18.18,100.20191001296,3.52919502221048));
#70729=CARTESIAN_POINT('',(18.3,100.20191001296,3.52919502221048));
#70730=CARTESIAN_POINT('Ctrl Pts',(18.18,100.20191001296,3.52919502221048));
#70731=CARTESIAN_POINT('Ctrl Pts',(18.18,100.116780275106,3.58485667072237));
#70732=CARTESIAN_POINT('Ctrl Pts',(18.18,100.066575729847,3.69399717114866));
#70733=CARTESIAN_POINT('Ctrl Pts',(18.3,100.390723073483,3.47353329919279));
#70734=CARTESIAN_POINT('Ctrl Pts',(18.1272,100.390723073483,3.47353329919279));
#70735=CARTESIAN_POINT('Ctrl Pts',(18.3,100.287039601803,3.47353329919279));
#70736=CARTESIAN_POINT('Ctrl Pts',(18.1272,100.287039601803,3.47353329919279));
#70737=CARTESIAN_POINT('Ctrl Pts',(18.3,100.20191001296,3.52919502221048));
#70738=CARTESIAN_POINT('Ctrl Pts',(18.1272,100.20191001296,3.52919502221048));
#70739=CARTESIAN_POINT('',(18.3,100.390723073483,3.47353329919279));
#70740=CARTESIAN_POINT('Ctrl Pts',(18.3,100.390723073483,3.47353329919279));
#70741=CARTESIAN_POINT('Ctrl Pts',(18.3,100.287039601803,3.47353329919279));
#70742=CARTESIAN_POINT('Ctrl Pts',(18.3,100.20191001296,3.52919502221048));
#70743=CARTESIAN_POINT('',(18.18,100.390723073483,3.47353329919279));
#70744=CARTESIAN_POINT('',(18.3,100.390723073483,3.47353329919279));
#70745=CARTESIAN_POINT('Ctrl Pts',(18.18,100.390723073483,3.47353329919279));
#70746=CARTESIAN_POINT('Ctrl Pts',(18.18,100.287039601803,3.47353329919279));
#70747=CARTESIAN_POINT('Ctrl Pts',(18.18,100.20191001296,3.52919502221048));
#70748=CARTESIAN_POINT('Ctrl Pts',(18.3,100.596998506784,3.53192349933088));
#70749=CARTESIAN_POINT('Ctrl Pts',(18.1272,100.596998506784,3.53192349933088));
#70750=CARTESIAN_POINT('Ctrl Pts',(18.3,100.499863499403,3.47353329919279));
#70751=CARTESIAN_POINT('Ctrl Pts',(18.1272,100.499863499403,3.47353329919279));
#70752=CARTESIAN_POINT('Ctrl Pts',(18.3,100.390723073483,3.47353329919279));
#70753=CARTESIAN_POINT('Ctrl Pts',(18.1272,100.390723073483,3.47353329919279));
#70754=CARTESIAN_POINT('',(18.3,100.596998506784,3.53192349933088));
#70755=CARTESIAN_POINT('Ctrl Pts',(18.3,100.596998506784,3.53192349933088));
#70756=CARTESIAN_POINT('Ctrl Pts',(18.3,100.499863499403,3.47353329919279));
#70757=CARTESIAN_POINT('Ctrl Pts',(18.3,100.390723073483,3.47353329919279));
#70758=CARTESIAN_POINT('',(18.18,100.596998506784,3.53192349933088));
#70759=CARTESIAN_POINT('',(18.3,100.596998506784,3.53192349933088));
#70760=CARTESIAN_POINT('Ctrl Pts',(18.18,100.596998506784,3.53192349933088));
#70761=CARTESIAN_POINT('Ctrl Pts',(18.18,100.499863499403,3.47353329919279));
#70762=CARTESIAN_POINT('Ctrl Pts',(18.18,100.390723073483,3.47353329919279));
#70763=CARTESIAN_POINT('Ctrl Pts',(18.3,100.750340992212,3.70054563544691));
#70764=CARTESIAN_POINT('Ctrl Pts',(18.1272,100.750340992212,3.70054563544691));
#70765=CARTESIAN_POINT('Ctrl Pts',(18.3,100.694133663177,3.59031369946897));
#70766=CARTESIAN_POINT('Ctrl Pts',(18.1272,100.694133663177,3.59031369946897));
#70767=CARTESIAN_POINT('Ctrl Pts',(18.3,100.596998506784,3.53192349933088));
#70768=CARTESIAN_POINT('Ctrl Pts',(18.1272,100.596998506784,3.53192349933088));
#70769=CARTESIAN_POINT('',(18.3,100.750340992212,3.70054563544691));
#70770=CARTESIAN_POINT('Ctrl Pts',(18.3,100.750340992212,3.70054563544691));
#70771=CARTESIAN_POINT('Ctrl Pts',(18.3,100.694133663177,3.59031369946897));
#70772=CARTESIAN_POINT('Ctrl Pts',(18.3,100.596998506784,3.53192349933088));
#70773=CARTESIAN_POINT('',(18.18,100.750340992212,3.70054563544691));
#70774=CARTESIAN_POINT('',(18.3,100.750340992212,3.70054563544691));
#70775=CARTESIAN_POINT('Ctrl Pts',(18.18,100.750340992212,3.70054563544691));
#70776=CARTESIAN_POINT('Ctrl Pts',(18.18,100.694133663177,3.59031369946897));
#70777=CARTESIAN_POINT('Ctrl Pts',(18.18,100.596998506784,3.53192349933088));
#70778=CARTESIAN_POINT('Ctrl Pts',(18.3,100.806548321247,3.94174618683755));
#70779=CARTESIAN_POINT('Ctrl Pts',(18.1272,100.806548321247,3.94174618683755));
#70780=CARTESIAN_POINT('Ctrl Pts',(18.3,100.806548321247,3.81077749691904));
#70781=CARTESIAN_POINT('Ctrl Pts',(18.1272,100.806548321247,3.81077749691904));
#70782=CARTESIAN_POINT('Ctrl Pts',(18.3,100.750340992212,3.70054563544691));
#70783=CARTESIAN_POINT('Ctrl Pts',(18.1272,100.750340992212,3.70054563544691));
#70784=CARTESIAN_POINT('',(18.3,100.806548321247,3.94174618683755));
#70785=CARTESIAN_POINT('Ctrl Pts',(18.3,100.806548321247,3.94174618683755));
#70786=CARTESIAN_POINT('Ctrl Pts',(18.3,100.806548321247,3.81077749691904));
#70787=CARTESIAN_POINT('Ctrl Pts',(18.3,100.750340992212,3.70054563544691));
#70788=CARTESIAN_POINT('',(18.18,100.806548321247,3.94174618683755));
#70789=CARTESIAN_POINT('',(18.3,100.806548321247,3.94174618683755));
#70790=CARTESIAN_POINT('Ctrl Pts',(18.18,100.806548321247,3.94174618683755));
#70791=CARTESIAN_POINT('Ctrl Pts',(18.18,100.806548321247,3.81077749691904));
#70792=CARTESIAN_POINT('Ctrl Pts',(18.18,100.750340992212,3.70054563544691));
#70793=CARTESIAN_POINT('Ctrl Pts',(18.3,100.69795357585,4.25934502892196));
#70794=CARTESIAN_POINT('Ctrl Pts',(18.1272,100.69795357585,4.25934502892196));
#70795=CARTESIAN_POINT('Ctrl Pts',(18.3,100.806548321247,4.13165064565837));
#70796=CARTESIAN_POINT('Ctrl Pts',(18.1272,100.806548321247,4.13165064565837));
#70797=CARTESIAN_POINT('Ctrl Pts',(18.3,100.806548321247,3.94174618683755));
#70798=CARTESIAN_POINT('Ctrl Pts',(18.1272,100.806548321247,3.94174618683755));
#70799=CARTESIAN_POINT('',(18.3,100.69795357585,4.25934502892196));
#70800=CARTESIAN_POINT('Ctrl Pts',(18.3,100.69795357585,4.25934502892196));
#70801=CARTESIAN_POINT('Ctrl Pts',(18.3,100.806548321247,4.13165064565837));
#70802=CARTESIAN_POINT('Ctrl Pts',(18.3,100.806548321247,3.94174618683755));
#70803=CARTESIAN_POINT('',(18.18,100.69795357585,4.25934502892196));
#70804=CARTESIAN_POINT('',(18.3,100.69795357585,4.25934502892196));
#70805=CARTESIAN_POINT('Ctrl Pts',(18.18,100.69795357585,4.25934502892196));
#70806=CARTESIAN_POINT('Ctrl Pts',(18.18,100.806548321247,4.13165064565837));
#70807=CARTESIAN_POINT('Ctrl Pts',(18.18,100.806548321247,3.94174618683755));
#70808=CARTESIAN_POINT('Ctrl Pts',(18.3,100.39181458354,4.4230558168143));
#70809=CARTESIAN_POINT('Ctrl Pts',(18.1272,100.39181458354,4.4230558168143));
#70810=CARTESIAN_POINT('Ctrl Pts',(18.3,100.58935868144,4.38703944943845));
#70811=CARTESIAN_POINT('Ctrl Pts',(18.1272,100.58935868144,4.38703944943845));
#70812=CARTESIAN_POINT('Ctrl Pts',(18.3,100.69795357585,4.25934502892196));
#70813=CARTESIAN_POINT('Ctrl Pts',(18.1272,100.69795357585,4.25934502892196));
#70814=CARTESIAN_POINT('',(18.3,100.39181458354,4.4230558168143));
#70815=CARTESIAN_POINT('Ctrl Pts',(18.3,100.39181458354,4.4230558168143));
#70816=CARTESIAN_POINT('Ctrl Pts',(18.3,100.58935868144,4.38703944943845));
#70817=CARTESIAN_POINT('Ctrl Pts',(18.3,100.69795357585,4.25934502892196));
#70818=CARTESIAN_POINT('',(18.18,100.39181458354,4.4230558168143));
#70819=CARTESIAN_POINT('',(18.3,100.39181458354,4.4230558168143));
#70820=CARTESIAN_POINT('Ctrl Pts',(18.18,100.39181458354,4.4230558168143));
#70821=CARTESIAN_POINT('Ctrl Pts',(18.18,100.58935868144,4.38703944943845));
#70822=CARTESIAN_POINT('Ctrl Pts',(18.18,100.69795357585,4.25934502892196));
#70823=CARTESIAN_POINT('Origin',(18.3,100.356889539957,4.22660289369523));
#70824=CARTESIAN_POINT('',(18.3,100.356889539957,4.22660289369523));
#70825=CARTESIAN_POINT('',(18.3,100.001593808947,2.22806895448985));
#70826=CARTESIAN_POINT('',(18.18,100.356889539957,4.22660289369523));
#70827=CARTESIAN_POINT('',(18.3,100.356889539957,4.22660289369523));
#70828=CARTESIAN_POINT('',(18.18,100.356889539957,4.22660289369523));
#70829=CARTESIAN_POINT('Ctrl Pts',(18.3,100.572987669706,4.12837641350925));
#70830=CARTESIAN_POINT('Ctrl Pts',(18.1272,100.572987669706,4.12837641350925));
#70831=CARTESIAN_POINT('Ctrl Pts',(18.3,100.500954860449,4.20477477870882));
#70832=CARTESIAN_POINT('Ctrl Pts',(18.1272,100.500954860449,4.20477477870882));
#70833=CARTESIAN_POINT('Ctrl Pts',(18.3,100.356889539957,4.22660289369523));
#70834=CARTESIAN_POINT('Ctrl Pts',(18.1272,100.356889539957,4.22660289369523));
#70835=CARTESIAN_POINT('',(18.3,100.572987669706,4.12837641350925));
#70836=CARTESIAN_POINT('Ctrl Pts',(18.3,100.572987669706,4.12837641350925));
#70837=CARTESIAN_POINT('Ctrl Pts',(18.3,100.500954860449,4.20477477870882));
#70838=CARTESIAN_POINT('Ctrl Pts',(18.3,100.356889539957,4.22660289369523));
#70839=CARTESIAN_POINT('',(18.18,100.572987669706,4.12837641350925));
#70840=CARTESIAN_POINT('',(18.3,100.572987669706,4.12837641350925));
#70841=CARTESIAN_POINT('Ctrl Pts',(18.18,100.572987669706,4.12837641350925));
#70842=CARTESIAN_POINT('Ctrl Pts',(18.18,100.500954860449,4.20477477870882));
#70843=CARTESIAN_POINT('Ctrl Pts',(18.18,100.356889539957,4.22660289369523));
#70844=CARTESIAN_POINT('Ctrl Pts',(18.3,100.645020329952,3.93738051913679));
#70845=CARTESIAN_POINT('Ctrl Pts',(18.1272,100.645020329952,3.93738051913679));
#70846=CARTESIAN_POINT('Ctrl Pts',(18.3,100.645020329952,4.05197804830968));
#70847=CARTESIAN_POINT('Ctrl Pts',(18.1272,100.645020329952,4.05197804830968));
#70848=CARTESIAN_POINT('Ctrl Pts',(18.3,100.572987669706,4.12837641350925));
#70849=CARTESIAN_POINT('Ctrl Pts',(18.1272,100.572987669706,4.12837641350925));
#70850=CARTESIAN_POINT('',(18.3,100.645020329952,3.93738051913679));
#70851=CARTESIAN_POINT('Ctrl Pts',(18.3,100.645020329952,3.93738051913679));
#70852=CARTESIAN_POINT('Ctrl Pts',(18.3,100.645020329952,4.05197804830968));
#70853=CARTESIAN_POINT('Ctrl Pts',(18.3,100.572987669706,4.12837641350925));
#70854=CARTESIAN_POINT('',(18.18,100.645020329952,3.93738051913679));
#70855=CARTESIAN_POINT('',(18.3,100.645020329952,3.93738051913679));
#70856=CARTESIAN_POINT('Ctrl Pts',(18.18,100.645020329952,3.93738051913679));
#70857=CARTESIAN_POINT('Ctrl Pts',(18.18,100.645020329952,4.05197804830968));
#70858=CARTESIAN_POINT('Ctrl Pts',(18.18,100.572987669706,4.12837641350925));
#70859=CARTESIAN_POINT('Ctrl Pts',(18.3,100.574079030752,3.74856745861471));
#70860=CARTESIAN_POINT('Ctrl Pts',(18.1272,100.574079030752,3.74856745861471));
#70861=CARTESIAN_POINT('Ctrl Pts',(18.3,100.645020329952,3.82169162891805));
#70862=CARTESIAN_POINT('Ctrl Pts',(18.1272,100.645020329952,3.82169162891805));
#70863=CARTESIAN_POINT('Ctrl Pts',(18.3,100.645020329952,3.93738051913679));
#70864=CARTESIAN_POINT('Ctrl Pts',(18.1272,100.645020329952,3.93738051913679));
#70865=CARTESIAN_POINT('',(18.3,100.574079030752,3.74856745861471));
#70866=CARTESIAN_POINT('Ctrl Pts',(18.3,100.574079030752,3.74856745861471));
#70867=CARTESIAN_POINT('Ctrl Pts',(18.3,100.645020329952,3.82169162891805));
#70868=CARTESIAN_POINT('Ctrl Pts',(18.3,100.645020329952,3.93738051913679));
#70869=CARTESIAN_POINT('',(18.18,100.574079030752,3.74856745861471));
#70870=CARTESIAN_POINT('',(18.3,100.574079030752,3.74856745861471));
#70871=CARTESIAN_POINT('Ctrl Pts',(18.18,100.574079030752,3.74856745861471));
#70872=CARTESIAN_POINT('Ctrl Pts',(18.18,100.645020329952,3.82169162891805));
#70873=CARTESIAN_POINT('Ctrl Pts',(18.18,100.645020329952,3.93738051913679));
#70874=CARTESIAN_POINT('Ctrl Pts',(18.3,100.395088666677,3.67544328831136));
#70875=CARTESIAN_POINT('Ctrl Pts',(18.1272,100.395088666677,3.67544328831136));
#70876=CARTESIAN_POINT('Ctrl Pts',(18.3,100.503137731552,3.67544328831136));
#70877=CARTESIAN_POINT('Ctrl Pts',(18.1272,100.503137731552,3.67544328831136));
#70878=CARTESIAN_POINT('Ctrl Pts',(18.3,100.574079030752,3.74856745861471));
#70879=CARTESIAN_POINT('Ctrl Pts',(18.1272,100.574079030752,3.74856745861471));
#70880=CARTESIAN_POINT('',(18.3,100.395088666677,3.67544328831136));
#70881=CARTESIAN_POINT('Ctrl Pts',(18.3,100.395088666677,3.67544328831136));
#70882=CARTESIAN_POINT('Ctrl Pts',(18.3,100.503137731552,3.67544328831136));
#70883=CARTESIAN_POINT('Ctrl Pts',(18.3,100.574079030752,3.74856745861471));
#70884=CARTESIAN_POINT('',(18.18,100.395088666677,3.67544328831136));
#70885=CARTESIAN_POINT('',(18.3,100.395088666677,3.67544328831136));
#70886=CARTESIAN_POINT('Ctrl Pts',(18.18,100.395088666677,3.67544328831136));
#70887=CARTESIAN_POINT('Ctrl Pts',(18.18,100.503137731552,3.67544328831136));
#70888=CARTESIAN_POINT('Ctrl Pts',(18.18,100.574079030752,3.74856745861471));
#70889=CARTESIAN_POINT('Ctrl Pts',(18.3,100.193178826571,3.77585252784193));
#70890=CARTESIAN_POINT('Ctrl Pts',(18.1272,100.193178826571,3.77585252784193));
#70891=CARTESIAN_POINT('Ctrl Pts',(18.3,100.258663022518,3.67544328831136));
#70892=CARTESIAN_POINT('Ctrl Pts',(18.1272,100.258663022518,3.67544328831136));
#70893=CARTESIAN_POINT('Ctrl Pts',(18.3,100.395088666677,3.67544328831136));
#70894=CARTESIAN_POINT('Ctrl Pts',(18.1272,100.395088666677,3.67544328831136));
#70895=CARTESIAN_POINT('',(18.3,100.193178826571,3.77585252784193));
#70896=CARTESIAN_POINT('Ctrl Pts',(18.3,100.193178826571,3.77585252784193));
#70897=CARTESIAN_POINT('Ctrl Pts',(18.3,100.258663022518,3.67544328831136));
#70898=CARTESIAN_POINT('Ctrl Pts',(18.3,100.395088666677,3.67544328831136));
#70899=CARTESIAN_POINT('',(18.18,100.193178826571,3.77585252784193));
#70900=CARTESIAN_POINT('',(18.3,100.193178826571,3.77585252784193));
#70901=CARTESIAN_POINT('Ctrl Pts',(18.18,100.193178826571,3.77585252784193));
#70902=CARTESIAN_POINT('Ctrl Pts',(18.18,100.258663022518,3.67544328831136));
#70903=CARTESIAN_POINT('Ctrl Pts',(18.18,100.395088666677,3.67544328831136));
#70904=CARTESIAN_POINT('Ctrl Pts',(18.3,100.127694481611,4.0017734285444));
#70905=CARTESIAN_POINT('Ctrl Pts',(18.1272,100.127694481611,4.0017734285444));
#70906=CARTESIAN_POINT('Ctrl Pts',(18.3,100.127694481611,3.87626184187829));
#70907=CARTESIAN_POINT('Ctrl Pts',(18.1272,100.127694481611,3.87626184187829));
#70908=CARTESIAN_POINT('Ctrl Pts',(18.3,100.193178826571,3.77585252784193));
#70909=CARTESIAN_POINT('Ctrl Pts',(18.1272,100.193178826571,3.77585252784193));
#70910=CARTESIAN_POINT('',(18.3,100.127694481611,4.0017734285444));
#70911=CARTESIAN_POINT('Ctrl Pts',(18.3,100.127694481611,4.0017734285444));
#70912=CARTESIAN_POINT('Ctrl Pts',(18.3,100.127694481611,3.87626184187829));
#70913=CARTESIAN_POINT('Ctrl Pts',(18.3,100.193178826571,3.77585252784193));
#70914=CARTESIAN_POINT('',(18.18,100.127694481611,4.0017734285444));
#70915=CARTESIAN_POINT('',(18.3,100.127694481611,4.0017734285444));
#70916=CARTESIAN_POINT('Ctrl Pts',(18.18,100.127694481611,4.0017734285444));
#70917=CARTESIAN_POINT('Ctrl Pts',(18.18,100.127694481611,3.87626184187829));
#70918=CARTESIAN_POINT('Ctrl Pts',(18.18,100.193178826571,3.77585252784193));
#70919=CARTESIAN_POINT('Ctrl Pts',(18.3,100.129877203703,4.03342416547239));
#70920=CARTESIAN_POINT('Ctrl Pts',(18.1272,100.129877203703,4.03342416547239));
#70921=CARTESIAN_POINT('Ctrl Pts',(18.3,100.127694481611,4.01377884708345));
#70922=CARTESIAN_POINT('Ctrl Pts',(18.1272,100.127694481611,4.01377884708345));
#70923=CARTESIAN_POINT('Ctrl Pts',(18.3,100.127694481611,4.0017734285444));
#70924=CARTESIAN_POINT('Ctrl Pts',(18.1272,100.127694481611,4.0017734285444));
#70925=CARTESIAN_POINT('',(18.3,100.129877203703,4.03342416547239));
#70926=CARTESIAN_POINT('Ctrl Pts',(18.3,100.129877203703,4.03342416547239));
#70927=CARTESIAN_POINT('Ctrl Pts',(18.3,100.127694481611,4.01377884708345));
#70928=CARTESIAN_POINT('Ctrl Pts',(18.3,100.127694481611,4.0017734285444));
#70929=CARTESIAN_POINT('',(18.18,100.129877203703,4.03342416547239));
#70930=CARTESIAN_POINT('',(18.3,100.129877203703,4.03342416547239));
#70931=CARTESIAN_POINT('Ctrl Pts',(18.18,100.129877203703,4.03342416547239));
#70932=CARTESIAN_POINT('Ctrl Pts',(18.18,100.127694481611,4.01377884708345));
#70933=CARTESIAN_POINT('Ctrl Pts',(18.18,100.127694481611,4.0017734285444));
#70934=CARTESIAN_POINT('Origin',(18.3,99.9574353039265,4.05525228045881));
#70935=CARTESIAN_POINT('',(18.3,99.9574353039265,4.05525228045881));
#70936=CARTESIAN_POINT('',(18.3,85.124940537059,5.93278553500053));
#70937=CARTESIAN_POINT('',(18.18,99.9574353039265,4.05525228045881));
#70938=CARTESIAN_POINT('',(18.3,99.9574353039265,4.05525228045881));
#70939=CARTESIAN_POINT('',(18.18,99.9574353039265,4.05525228045881));
#70940=CARTESIAN_POINT('Ctrl Pts',(18.3,99.9792634189129,3.91664383970201));
#70941=CARTESIAN_POINT('Ctrl Pts',(18.1272,99.9792634189129,3.91664383970201));
#70942=CARTESIAN_POINT('Ctrl Pts',(18.3,99.9792634189129,3.9723054882139));
#70943=CARTESIAN_POINT('Ctrl Pts',(18.1272,99.9792634189129,3.9723054882139));
#70944=CARTESIAN_POINT('Ctrl Pts',(18.3,99.9574353039265,4.05525228045881));
#70945=CARTESIAN_POINT('Ctrl Pts',(18.1272,99.9574353039265,4.05525228045881));
#70946=CARTESIAN_POINT('',(18.3,99.9792634189129,3.91664383970201));
#70947=CARTESIAN_POINT('Ctrl Pts',(18.3,99.9792634189129,3.91664383970201));
#70948=CARTESIAN_POINT('Ctrl Pts',(18.3,99.9792634189129,3.9723054882139));
#70949=CARTESIAN_POINT('Ctrl Pts',(18.3,99.9574353039265,4.05525228045881));
#70950=CARTESIAN_POINT('',(18.18,99.9792634189129,3.91664383970201));
#70951=CARTESIAN_POINT('',(18.3,99.9792634189129,3.91664383970201));
#70952=CARTESIAN_POINT('Ctrl Pts',(18.18,99.9792634189129,3.91664383970201));
#70953=CARTESIAN_POINT('Ctrl Pts',(18.18,99.9792634189129,3.9723054882139));
#70954=CARTESIAN_POINT('Ctrl Pts',(18.18,99.9574353039265,4.05525228045881));
#70955=CARTESIAN_POINT('Ctrl Pts',(18.3,99.8914052784443,3.69181437455118));
#70956=CARTESIAN_POINT('Ctrl Pts',(18.1272,99.8914052784443,3.69181437455118));
#70957=CARTESIAN_POINT('Ctrl Pts',(18.3,99.9792634189129,3.78021819554269));
#70958=CARTESIAN_POINT('Ctrl Pts',(18.1272,99.9792634189129,3.78021819554269));
#70959=CARTESIAN_POINT('Ctrl Pts',(18.3,99.9792634189129,3.91664383970201));
#70960=CARTESIAN_POINT('Ctrl Pts',(18.1272,99.9792634189129,3.91664383970201));
#70961=CARTESIAN_POINT('',(18.3,99.8914052784443,3.69181437455118));
#70962=CARTESIAN_POINT('Ctrl Pts',(18.3,99.8914052784443,3.69181437455118));
#70963=CARTESIAN_POINT('Ctrl Pts',(18.3,99.9792634189129,3.78021819554269));
#70964=CARTESIAN_POINT('Ctrl Pts',(18.3,99.9792634189129,3.91664383970201));
#70965=CARTESIAN_POINT('',(18.18,99.8914052784443,3.69181437455118));
#70966=CARTESIAN_POINT('',(18.3,99.8914052784443,3.69181437455118));
#70967=CARTESIAN_POINT('Ctrl Pts',(18.18,99.8914052784443,3.69181437455118));
#70968=CARTESIAN_POINT('Ctrl Pts',(18.18,99.9792634189129,3.78021819554269));
#70969=CARTESIAN_POINT('Ctrl Pts',(18.18,99.9792634189129,3.91664383970201));
#70970=CARTESIAN_POINT('Ctrl Pts',(18.3,99.6682130038738,3.60341055355966));
#70971=CARTESIAN_POINT('Ctrl Pts',(18.1272,99.6682130038738,3.60341055355966));
#70972=CARTESIAN_POINT('Ctrl Pts',(18.3,99.8035471379757,3.60341055355966));
#70973=CARTESIAN_POINT('Ctrl Pts',(18.1272,99.8035471379757,3.60341055355966));
#70974=CARTESIAN_POINT('Ctrl Pts',(18.3,99.8914052784443,3.69181437455118));
#70975=CARTESIAN_POINT('Ctrl Pts',(18.1272,99.8914052784443,3.69181437455118));
#70976=CARTESIAN_POINT('',(18.3,99.6682130038738,3.60341055355966));
#70977=CARTESIAN_POINT('Ctrl Pts',(18.3,99.6682130038738,3.60341055355966));
#70978=CARTESIAN_POINT('Ctrl Pts',(18.3,99.8035471379757,3.60341055355966));
#70979=CARTESIAN_POINT('Ctrl Pts',(18.3,99.8914052784443,3.69181437455118));
#70980=CARTESIAN_POINT('',(18.18,99.6682130038738,3.60341055355966));
#70981=CARTESIAN_POINT('',(18.3,99.6682130038738,3.60341055355966));
#70982=CARTESIAN_POINT('Ctrl Pts',(18.18,99.6682130038738,3.60341055355966));
#70983=CARTESIAN_POINT('Ctrl Pts',(18.18,99.8035471379757,3.60341055355966));
#70984=CARTESIAN_POINT('Ctrl Pts',(18.18,99.8914052784443,3.69181437455118));
#70985=CARTESIAN_POINT('Ctrl Pts',(18.3,99.4302864611149,3.69890851937234));
#70986=CARTESIAN_POINT('Ctrl Pts',(18.1272,99.4302864611149,3.69890851937234));
#70987=CARTESIAN_POINT('Ctrl Pts',(18.3,99.5263301074505,3.60341055355966));
#70988=CARTESIAN_POINT('Ctrl Pts',(18.1272,99.5263301074505,3.60341055355966));
#70989=CARTESIAN_POINT('Ctrl Pts',(18.3,99.6682130038738,3.60341055355966));
#70990=CARTESIAN_POINT('Ctrl Pts',(18.1272,99.6682130038738,3.60341055355966));
#70991=CARTESIAN_POINT('',(18.3,99.4302864611149,3.69890851937234));
#70992=CARTESIAN_POINT('Ctrl Pts',(18.3,99.4302864611149,3.69890851937234));
#70993=CARTESIAN_POINT('Ctrl Pts',(18.3,99.5263301074505,3.60341055355966));
#70994=CARTESIAN_POINT('Ctrl Pts',(18.3,99.6682130038738,3.60341055355966));
#70995=CARTESIAN_POINT('',(18.18,99.4302864611149,3.69890851937234));
#70996=CARTESIAN_POINT('',(18.3,99.4302864611149,3.69890851937234));
#70997=CARTESIAN_POINT('Ctrl Pts',(18.18,99.4302864611149,3.69890851937234));
#70998=CARTESIAN_POINT('Ctrl Pts',(18.18,99.5263301074505,3.60341055355966));
#70999=CARTESIAN_POINT('Ctrl Pts',(18.18,99.6682130038738,3.60341055355966));
#71000=CARTESIAN_POINT('Ctrl Pts',(18.3,99.3342428147793,3.93301485143602));
#71001=CARTESIAN_POINT('Ctrl Pts',(18.1272,99.3342428147793,3.93301485143602));
#71002=CARTESIAN_POINT('Ctrl Pts',(18.3,99.3342428147793,3.79440641067922));
#71003=CARTESIAN_POINT('Ctrl Pts',(18.1272,99.3342428147793,3.79440641067922));
#71004=CARTESIAN_POINT('Ctrl Pts',(18.3,99.4302864611149,3.69890851937234));
#71005=CARTESIAN_POINT('Ctrl Pts',(18.1272,99.4302864611149,3.69890851937234));
#71006=CARTESIAN_POINT('',(18.3,99.3342428147793,3.93301485143602));
#71007=CARTESIAN_POINT('Ctrl Pts',(18.3,99.3342428147793,3.93301485143602));
#71008=CARTESIAN_POINT('Ctrl Pts',(18.3,99.3342428147793,3.79440641067922));
#71009=CARTESIAN_POINT('Ctrl Pts',(18.3,99.4302864611149,3.69890851937234));
#71010=CARTESIAN_POINT('',(18.18,99.3342428147793,3.93301485143602));
#71011=CARTESIAN_POINT('',(18.3,99.3342428147793,3.93301485143602));
#71012=CARTESIAN_POINT('Ctrl Pts',(18.18,99.3342428147793,3.93301485143602));
#71013=CARTESIAN_POINT('Ctrl Pts',(18.18,99.3342428147793,3.79440641067922));
#71014=CARTESIAN_POINT('Ctrl Pts',(18.18,99.4302864611149,3.69890851937234));
#71015=CARTESIAN_POINT('Ctrl Pts',(18.3,99.4079126656055,4.13110492788255));
#71016=CARTESIAN_POINT('Ctrl Pts',(18.1272,99.4079126656055,4.13110492788255));
#71017=CARTESIAN_POINT('Ctrl Pts',(18.3,99.3342428147793,4.0497952517122));
#71018=CARTESIAN_POINT('Ctrl Pts',(18.1272,99.3342428147793,4.0497952517122));
#71019=CARTESIAN_POINT('Ctrl Pts',(18.3,99.3342428147793,3.93301485143602));
#71020=CARTESIAN_POINT('Ctrl Pts',(18.1272,99.3342428147793,3.93301485143602));
#71021=CARTESIAN_POINT('',(18.3,99.4079126656055,4.13110492788255));
#71022=CARTESIAN_POINT('Ctrl Pts',(18.3,99.4079126656055,4.13110492788255));
#71023=CARTESIAN_POINT('Ctrl Pts',(18.3,99.3342428147793,4.0497952517122));
#71024=CARTESIAN_POINT('Ctrl Pts',(18.3,99.3342428147793,3.93301485143602));
#71025=CARTESIAN_POINT('',(18.18,99.4079126656055,4.13110492788255));
#71026=CARTESIAN_POINT('',(18.3,99.4079126656055,4.13110492788255));
#71027=CARTESIAN_POINT('Ctrl Pts',(18.18,99.4079126656055,4.13110492788255));
#71028=CARTESIAN_POINT('Ctrl Pts',(18.18,99.3342428147793,4.0497952517122));
#71029=CARTESIAN_POINT('Ctrl Pts',(18.18,99.3342428147793,3.93301485143602));
#71030=CARTESIAN_POINT('Ctrl Pts',(18.3,99.6485676109791,4.24624817483127));
#71031=CARTESIAN_POINT('Ctrl Pts',(18.1272,99.6485676109791,4.24624817483127));
#71032=CARTESIAN_POINT('Ctrl Pts',(18.3,99.4815825164318,4.2124146413058));
#71033=CARTESIAN_POINT('Ctrl Pts',(18.1272,99.4815825164318,4.2124146413058));
#71034=CARTESIAN_POINT('Ctrl Pts',(18.3,99.4079126656055,4.13110492788255));
#71035=CARTESIAN_POINT('Ctrl Pts',(18.1272,99.4079126656055,4.13110492788255));
#71036=CARTESIAN_POINT('',(18.3,99.6485676109791,4.24624817483127));
#71037=CARTESIAN_POINT('Ctrl Pts',(18.3,99.6485676109791,4.24624817483127));
#71038=CARTESIAN_POINT('Ctrl Pts',(18.3,99.4815825164318,4.2124146413058));
#71039=CARTESIAN_POINT('Ctrl Pts',(18.3,99.4079126656055,4.13110492788255));
#71040=CARTESIAN_POINT('',(18.18,99.6485676109791,4.24624817483127));
#71041=CARTESIAN_POINT('',(18.3,99.6485676109791,4.24624817483127));
#71042=CARTESIAN_POINT('Ctrl Pts',(18.18,99.6485676109791,4.24624817483127));
#71043=CARTESIAN_POINT('Ctrl Pts',(18.18,99.4815825164318,4.2124146413058));
#71044=CARTESIAN_POINT('Ctrl Pts',(18.18,99.4079126656055,4.13110492788255));
#71045=CARTESIAN_POINT('Origin',(18.3,99.6223737537861,4.44270109795034));
#71046=CARTESIAN_POINT('',(18.3,99.6223737537861,4.44270109795034));
#71047=CARTESIAN_POINT('',(18.3,99.2944047342843,6.90245615040001));
#71048=CARTESIAN_POINT('',(18.18,99.6223737537861,4.44270109795034));
#71049=CARTESIAN_POINT('',(18.3,99.6223737537861,4.44270109795034));
#71050=CARTESIAN_POINT('',(18.18,99.6223737537861,4.44270109795034));
#71051=CARTESIAN_POINT('Ctrl Pts',(18.3,99.2971350491047,4.28390165828168));
#71052=CARTESIAN_POINT('Ctrl Pts',(18.1272,99.2971350491047,4.28390165828168));
#71053=CARTESIAN_POINT('Ctrl Pts',(18.3,99.4226466357708,4.4230558168143));
#71054=CARTESIAN_POINT('Ctrl Pts',(18.1272,99.4226466357708,4.4230558168143));
#71055=CARTESIAN_POINT('Ctrl Pts',(18.3,99.6223737537861,4.44270109795034));
#71056=CARTESIAN_POINT('Ctrl Pts',(18.1272,99.6223737537861,4.44270109795034));
#71057=CARTESIAN_POINT('Ctrl Pts',(18.3,99.2971350491047,4.28390165828168));
#71058=CARTESIAN_POINT('Ctrl Pts',(18.3,99.4226466357708,4.4230558168143));
#71059=CARTESIAN_POINT('Ctrl Pts',(18.3,99.6223737537861,4.44270109795034));
#71060=CARTESIAN_POINT('Ctrl Pts',(18.18,99.2971350491047,4.28390165828168));
#71061=CARTESIAN_POINT('Ctrl Pts',(18.18,99.4226466357708,4.4230558168143));
#71062=CARTESIAN_POINT('Ctrl Pts',(18.18,99.6223737537861,4.44270109795034));
#71063=CARTESIAN_POINT('Origin',(18.18,99.9890859663486,3.29999992661178));
#71064=CARTESIAN_POINT('Origin',(18.3,70.,5.5));
#71065=CARTESIAN_POINT('Ctrl Pts',(18.3,90.643929117918,2.66698497384787));
#71066=CARTESIAN_POINT('Ctrl Pts',(18.1272,90.643929117918,2.66698497384787));
#71067=CARTESIAN_POINT('Ctrl Pts',(18.3,90.643929117918,2.80231925696135));
#71068=CARTESIAN_POINT('Ctrl Pts',(18.1272,90.643929117918,2.80231925696135));
#71069=CARTESIAN_POINT('Ctrl Pts',(18.3,90.5293315887451,2.88308325260878));
#71070=CARTESIAN_POINT('Ctrl Pts',(18.1272,90.5293315887451,2.88308325260878));
#71071=CARTESIAN_POINT('',(18.3,90.643929117918,2.66698497384787));
#71072=CARTESIAN_POINT('',(18.3,90.5293315887451,2.88308325260878));
#71073=CARTESIAN_POINT('Ctrl Pts',(18.3,90.643929117918,2.66698497384787));
#71074=CARTESIAN_POINT('Ctrl Pts',(18.3,90.643929117918,2.80231925696135));
#71075=CARTESIAN_POINT('Ctrl Pts',(18.3,90.5293315887451,2.88308325260878));
#71076=CARTESIAN_POINT('',(18.18,90.643929117918,2.66698497384787));
#71077=CARTESIAN_POINT('',(18.3,90.643929117918,2.66698497384787));
#71078=CARTESIAN_POINT('',(18.18,90.5293315887451,2.88308325260878));
#71079=CARTESIAN_POINT('Ctrl Pts',(18.18,90.643929117918,2.66698497384787));
#71080=CARTESIAN_POINT('Ctrl Pts',(18.18,90.643929117918,2.80231925696135));
#71081=CARTESIAN_POINT('Ctrl Pts',(18.18,90.5293315887451,2.88308325260878));
#71082=CARTESIAN_POINT('',(18.3,90.5293315887451,2.88308325260878));
#71083=CARTESIAN_POINT('Ctrl Pts',(18.3,90.5140519380569,2.43724423497915));
#71084=CARTESIAN_POINT('Ctrl Pts',(18.1272,90.5140519380569,2.43724423497915));
#71085=CARTESIAN_POINT('Ctrl Pts',(18.3,90.643929117918,2.52946796864271));
#71086=CARTESIAN_POINT('Ctrl Pts',(18.1272,90.643929117918,2.52946796864271));
#71087=CARTESIAN_POINT('Ctrl Pts',(18.3,90.643929117918,2.66698497384787));
#71088=CARTESIAN_POINT('Ctrl Pts',(18.1272,90.643929117918,2.66698497384787));
#71089=CARTESIAN_POINT('',(18.3,90.5140519380569,2.43724423497915));
#71090=CARTESIAN_POINT('Ctrl Pts',(18.3,90.5140519380569,2.43724423497915));
#71091=CARTESIAN_POINT('Ctrl Pts',(18.3,90.643929117918,2.52946796864271));
#71092=CARTESIAN_POINT('Ctrl Pts',(18.3,90.643929117918,2.66698497384787));
#71093=CARTESIAN_POINT('',(18.18,90.5140519380569,2.43724423497915));
#71094=CARTESIAN_POINT('',(18.3,90.5140519380569,2.43724423497915));
#71095=CARTESIAN_POINT('Ctrl Pts',(18.18,90.5140519380569,2.43724423497915));
#71096=CARTESIAN_POINT('Ctrl Pts',(18.18,90.643929117918,2.52946796864271));
#71097=CARTESIAN_POINT('Ctrl Pts',(18.18,90.643929117918,2.66698497384787));
#71098=CARTESIAN_POINT('Ctrl Pts',(18.3,89.9890859663486,2.34502050131559));
#71099=CARTESIAN_POINT('Ctrl Pts',(18.1272,89.9890859663486,2.34502050131559));
#71100=CARTESIAN_POINT('Ctrl Pts',(18.3,90.3841746091843,2.34502050131559));
#71101=CARTESIAN_POINT('Ctrl Pts',(18.1272,90.3841746091843,2.34502050131559));
#71102=CARTESIAN_POINT('Ctrl Pts',(18.3,90.5140519380569,2.43724423497915));
#71103=CARTESIAN_POINT('Ctrl Pts',(18.1272,90.5140519380569,2.43724423497915));
#71104=CARTESIAN_POINT('',(18.3,89.9890859663486,2.34502050131559));
#71105=CARTESIAN_POINT('Ctrl Pts',(18.3,89.9890859663486,2.34502050131559));
#71106=CARTESIAN_POINT('Ctrl Pts',(18.3,90.3841746091843,2.34502050131559));
#71107=CARTESIAN_POINT('Ctrl Pts',(18.3,90.5140519380569,2.43724423497915));
#71108=CARTESIAN_POINT('',(18.18,89.9890859663486,2.34502050131559));
#71109=CARTESIAN_POINT('',(18.3,89.9890859663486,2.34502050131559));
#71110=CARTESIAN_POINT('Ctrl Pts',(18.18,89.9890859663486,2.34502050131559));
#71111=CARTESIAN_POINT('Ctrl Pts',(18.18,90.3841746091843,2.34502050131559));
#71112=CARTESIAN_POINT('Ctrl Pts',(18.18,90.5140519380569,2.43724423497915));
#71113=CARTESIAN_POINT('Ctrl Pts',(18.3,89.4652115046978,2.43724423497915));
#71114=CARTESIAN_POINT('Ctrl Pts',(18.1272,89.4652115046978,2.43724423497915));
#71115=CARTESIAN_POINT('Ctrl Pts',(18.3,89.5961801946163,2.34502050131559));
#71116=CARTESIAN_POINT('Ctrl Pts',(18.1272,89.5961801946163,2.34502050131559));
#71117=CARTESIAN_POINT('Ctrl Pts',(18.3,89.9890859663486,2.34502050131559));
#71118=CARTESIAN_POINT('Ctrl Pts',(18.1272,89.9890859663486,2.34502050131559));
#71119=CARTESIAN_POINT('',(18.3,89.4652115046978,2.43724423497915));
#71120=CARTESIAN_POINT('Ctrl Pts',(18.3,89.4652115046978,2.43724423497915));
#71121=CARTESIAN_POINT('Ctrl Pts',(18.3,89.5961801946163,2.34502050131559));
#71122=CARTESIAN_POINT('Ctrl Pts',(18.3,89.9890859663486,2.34502050131559));
#71123=CARTESIAN_POINT('',(18.18,89.4652115046978,2.43724423497915));
#71124=CARTESIAN_POINT('',(18.3,89.4652115046978,2.43724423497915));
#71125=CARTESIAN_POINT('Ctrl Pts',(18.18,89.4652115046978,2.43724423497915));
#71126=CARTESIAN_POINT('Ctrl Pts',(18.18,89.5961801946163,2.34502050131559));
#71127=CARTESIAN_POINT('Ctrl Pts',(18.18,89.9890859663486,2.34502050131559));
#71128=CARTESIAN_POINT('Ctrl Pts',(18.3,89.3342428147793,2.66480210274458));
#71129=CARTESIAN_POINT('Ctrl Pts',(18.1272,89.3342428147793,2.66480210274458));
#71130=CARTESIAN_POINT('Ctrl Pts',(18.3,89.3342428147793,2.52946796864271));
#71131=CARTESIAN_POINT('Ctrl Pts',(18.1272,89.3342428147793,2.52946796864271));
#71132=CARTESIAN_POINT('Ctrl Pts',(18.3,89.4652115046978,2.43724423497915));
#71133=CARTESIAN_POINT('Ctrl Pts',(18.1272,89.4652115046978,2.43724423497915));
#71134=CARTESIAN_POINT('',(18.3,89.3342428147793,2.66480210274458));
#71135=CARTESIAN_POINT('Ctrl Pts',(18.3,89.3342428147793,2.66480210274458));
#71136=CARTESIAN_POINT('Ctrl Pts',(18.3,89.3342428147793,2.52946796864271));
#71137=CARTESIAN_POINT('Ctrl Pts',(18.3,89.4652115046978,2.43724423497915));
#71138=CARTESIAN_POINT('',(18.18,89.3342428147793,2.66480210274458));
#71139=CARTESIAN_POINT('',(18.3,89.3342428147793,2.66480210274458));
#71140=CARTESIAN_POINT('Ctrl Pts',(18.18,89.3342428147793,2.66480210274458));
#71141=CARTESIAN_POINT('Ctrl Pts',(18.18,89.3342428147793,2.52946796864271));
#71142=CARTESIAN_POINT('Ctrl Pts',(18.18,89.4652115046978,2.43724423497915));
#71143=CARTESIAN_POINT('Ctrl Pts',(18.3,89.4646658241749,2.89236011952162));
#71144=CARTESIAN_POINT('Ctrl Pts',(18.1272,89.4646658241749,2.89236011952162));
#71145=CARTESIAN_POINT('Ctrl Pts',(18.3,89.3342428147793,2.80013638585806));
#71146=CARTESIAN_POINT('Ctrl Pts',(18.1272,89.3342428147793,2.80013638585806));
#71147=CARTESIAN_POINT('Ctrl Pts',(18.3,89.3342428147793,2.66480210274458));
#71148=CARTESIAN_POINT('Ctrl Pts',(18.1272,89.3342428147793,2.66480210274458));
#71149=CARTESIAN_POINT('',(18.3,89.4646658241749,2.89236011952162));
#71150=CARTESIAN_POINT('Ctrl Pts',(18.3,89.4646658241749,2.89236011952162));
#71151=CARTESIAN_POINT('Ctrl Pts',(18.3,89.3342428147793,2.80013638585806));
#71152=CARTESIAN_POINT('Ctrl Pts',(18.3,89.3342428147793,2.66480210274458));
#71153=CARTESIAN_POINT('',(18.18,89.4646658241749,2.89236011952162));
#71154=CARTESIAN_POINT('',(18.3,89.4646658241749,2.89236011952162));
#71155=CARTESIAN_POINT('Ctrl Pts',(18.18,89.4646658241749,2.89236011952162));
#71156=CARTESIAN_POINT('Ctrl Pts',(18.18,89.3342428147793,2.80013638585806));
#71157=CARTESIAN_POINT('Ctrl Pts',(18.18,89.3342428147793,2.66480210274458));
#71158=CARTESIAN_POINT('Ctrl Pts',(18.3,89.9890859663486,2.98458385318518));
#71159=CARTESIAN_POINT('Ctrl Pts',(18.1272,89.9890859663486,2.98458385318518));
#71160=CARTESIAN_POINT('Ctrl Pts',(18.3,89.5950888335705,2.98458385318518));
#71161=CARTESIAN_POINT('Ctrl Pts',(18.1272,89.5950888335705,2.98458385318518));
#71162=CARTESIAN_POINT('Ctrl Pts',(18.3,89.4646658241749,2.89236011952162));
#71163=CARTESIAN_POINT('Ctrl Pts',(18.1272,89.4646658241749,2.89236011952162));
#71164=CARTESIAN_POINT('',(18.3,89.9890859663486,2.98458385318518));
#71165=CARTESIAN_POINT('Ctrl Pts',(18.3,89.9890859663486,2.98458385318518));
#71166=CARTESIAN_POINT('Ctrl Pts',(18.3,89.5950888335705,2.98458385318518));
#71167=CARTESIAN_POINT('Ctrl Pts',(18.3,89.4646658241749,2.89236011952162));
#71168=CARTESIAN_POINT('',(18.18,89.9890859663486,2.98458385318518));
#71169=CARTESIAN_POINT('',(18.3,89.9890859663486,2.98458385318518));
#71170=CARTESIAN_POINT('Ctrl Pts',(18.18,89.9890859663486,2.98458385318518));
#71171=CARTESIAN_POINT('Ctrl Pts',(18.18,89.5950888335705,2.98458385318518));
#71172=CARTESIAN_POINT('Ctrl Pts',(18.18,89.4646658241749,2.89236011952162));
#71173=CARTESIAN_POINT('Ctrl Pts',(18.3,90.5293315887451,2.88308325260878));
#71174=CARTESIAN_POINT('Ctrl Pts',(18.1272,90.5293315887451,2.88308325260878));
#71175=CARTESIAN_POINT('Ctrl Pts',(18.3,90.3830830991268,2.98458385318518));
#71176=CARTESIAN_POINT('Ctrl Pts',(18.1272,90.3830830991268,2.98458385318518));
#71177=CARTESIAN_POINT('Ctrl Pts',(18.3,89.9890859663486,2.98458385318518));
#71178=CARTESIAN_POINT('Ctrl Pts',(18.1272,89.9890859663486,2.98458385318518));
#71179=CARTESIAN_POINT('Ctrl Pts',(18.3,90.5293315887451,2.88308325260878));
#71180=CARTESIAN_POINT('Ctrl Pts',(18.3,90.3830830991268,2.98458385318518));
#71181=CARTESIAN_POINT('Ctrl Pts',(18.3,89.9890859663486,2.98458385318518));
#71182=CARTESIAN_POINT('Ctrl Pts',(18.18,90.5293315887451,2.88308325260878));
#71183=CARTESIAN_POINT('Ctrl Pts',(18.18,90.3830830991268,2.98458385318518));
#71184=CARTESIAN_POINT('Ctrl Pts',(18.18,89.9890859663486,2.98458385318518));
#71185=CARTESIAN_POINT('Ctrl Pts',(18.3,89.1727148234844,2.66480210274458));
#71186=CARTESIAN_POINT('Ctrl Pts',(18.1272,89.1727148234844,2.66480210274458));
#71187=CARTESIAN_POINT('Ctrl Pts',(18.3,89.1727148234844,2.89618003219366));
#71188=CARTESIAN_POINT('Ctrl Pts',(18.1272,89.1727148234844,2.89618003219366));
#71189=CARTESIAN_POINT('Ctrl Pts',(18.3,89.3386085569858,3.02824008315802));
#71190=CARTESIAN_POINT('Ctrl Pts',(18.1272,89.3386085569858,3.02824008315802));
#71191=CARTESIAN_POINT('',(18.3,89.1727148234844,2.66480210274458));
#71192=CARTESIAN_POINT('',(18.3,89.3386085569858,3.02824008315802));
#71193=CARTESIAN_POINT('Ctrl Pts',(18.3,89.1727148234844,2.66480210274458));
#71194=CARTESIAN_POINT('Ctrl Pts',(18.3,89.1727148234844,2.89618003219366));
#71195=CARTESIAN_POINT('Ctrl Pts',(18.3,89.3386085569858,3.02824008315802));
#71196=CARTESIAN_POINT('',(18.18,89.1727148234844,2.66480210274458));
#71197=CARTESIAN_POINT('',(18.3,89.1727148234844,2.66480210274458));
#71198=CARTESIAN_POINT('',(18.18,89.3386085569858,3.02824008315802));
#71199=CARTESIAN_POINT('Ctrl Pts',(18.18,89.1727148234844,2.66480210274458));
#71200=CARTESIAN_POINT('Ctrl Pts',(18.18,89.1727148234844,2.89618003219366));
#71201=CARTESIAN_POINT('Ctrl Pts',(18.18,89.3386085569858,3.02824008315802));
#71202=CARTESIAN_POINT('',(18.3,89.3386085569858,3.02824008315802));
#71203=CARTESIAN_POINT('Ctrl Pts',(18.3,89.2671214282513,2.37394276112318));
#71204=CARTESIAN_POINT('Ctrl Pts',(18.1272,89.2671214282513,2.37394276112318));
#71205=CARTESIAN_POINT('Ctrl Pts',(18.3,89.1727148234844,2.489085970819));
#71206=CARTESIAN_POINT('Ctrl Pts',(18.1272,89.1727148234844,2.489085970819));
#71207=CARTESIAN_POINT('Ctrl Pts',(18.3,89.1727148234844,2.66480210274458));
#71208=CARTESIAN_POINT('Ctrl Pts',(18.1272,89.1727148234844,2.66480210274458));
#71209=CARTESIAN_POINT('',(18.3,89.2671214282513,2.37394276112318));
#71210=CARTESIAN_POINT('Ctrl Pts',(18.3,89.2671214282513,2.37394276112318));
#71211=CARTESIAN_POINT('Ctrl Pts',(18.3,89.1727148234844,2.489085970819));
#71212=CARTESIAN_POINT('Ctrl Pts',(18.3,89.1727148234844,2.66480210274458));
#71213=CARTESIAN_POINT('',(18.18,89.2671214282513,2.37394276112318));
#71214=CARTESIAN_POINT('',(18.3,89.2671214282513,2.37394276112318));
#71215=CARTESIAN_POINT('Ctrl Pts',(18.18,89.2671214282513,2.37394276112318));
#71216=CARTESIAN_POINT('Ctrl Pts',(18.18,89.1727148234844,2.489085970819));
#71217=CARTESIAN_POINT('Ctrl Pts',(18.18,89.1727148234844,2.66480210274458));
#71218=CARTESIAN_POINT('Ctrl Pts',(18.3,89.5345156133175,2.20095503181219));
#71219=CARTESIAN_POINT('Ctrl Pts',(18.1272,89.5345156133175,2.20095503181219));
#71220=CARTESIAN_POINT('Ctrl Pts',(18.3,89.3615280330181,2.25879940241575));
#71221=CARTESIAN_POINT('Ctrl Pts',(18.1272,89.3615280330181,2.25879940241575));
#71222=CARTESIAN_POINT('Ctrl Pts',(18.3,89.2671214282513,2.37394276112318));
#71223=CARTESIAN_POINT('Ctrl Pts',(18.1272,89.2671214282513,2.37394276112318));
#71224=CARTESIAN_POINT('',(18.3,89.5345156133175,2.20095503181219));
#71225=CARTESIAN_POINT('Ctrl Pts',(18.3,89.5345156133175,2.20095503181219));
#71226=CARTESIAN_POINT('Ctrl Pts',(18.3,89.3615280330181,2.25879940241575));
#71227=CARTESIAN_POINT('Ctrl Pts',(18.3,89.2671214282513,2.37394276112318));
#71228=CARTESIAN_POINT('',(18.18,89.5345156133175,2.20095503181219));
#71229=CARTESIAN_POINT('',(18.3,89.5345156133175,2.20095503181219));
#71230=CARTESIAN_POINT('Ctrl Pts',(18.18,89.5345156133175,2.20095503181219));
#71231=CARTESIAN_POINT('Ctrl Pts',(18.18,89.3615280330181,2.25879940241575));
#71232=CARTESIAN_POINT('Ctrl Pts',(18.18,89.2671214282513,2.37394276112318));
#71233=CARTESIAN_POINT('Ctrl Pts',(18.3,89.9890859663486,2.14311051219702));
#71234=CARTESIAN_POINT('Ctrl Pts',(18.1272,89.9890859663486,2.14311051219702));
#71235=CARTESIAN_POINT('Ctrl Pts',(18.3,89.7075034916401,2.14311051219702));
#71236=CARTESIAN_POINT('Ctrl Pts',(18.1272,89.7075034916401,2.14311051219702));
#71237=CARTESIAN_POINT('Ctrl Pts',(18.3,89.5345156133175,2.20095503181219));
#71238=CARTESIAN_POINT('Ctrl Pts',(18.1272,89.5345156133175,2.20095503181219));
#71239=CARTESIAN_POINT('',(18.3,89.9890859663486,2.14311051219702));
#71240=CARTESIAN_POINT('Ctrl Pts',(18.3,89.9890859663486,2.14311051219702));
#71241=CARTESIAN_POINT('Ctrl Pts',(18.3,89.7075034916401,2.14311051219702));
#71242=CARTESIAN_POINT('Ctrl Pts',(18.3,89.5345156133175,2.20095503181219));
#71243=CARTESIAN_POINT('',(18.18,89.9890859663486,2.14311051219702));
#71244=CARTESIAN_POINT('',(18.3,89.9890859663486,2.14311051219702));
#71245=CARTESIAN_POINT('Ctrl Pts',(18.18,89.9890859663486,2.14311051219702));
#71246=CARTESIAN_POINT('Ctrl Pts',(18.18,89.7075034916401,2.14311051219702));
#71247=CARTESIAN_POINT('Ctrl Pts',(18.18,89.5345156133175,2.20095503181219));
#71248=CARTESIAN_POINT('Ctrl Pts',(18.3,90.3672577679157,2.17912691682577));
#71249=CARTESIAN_POINT('Ctrl Pts',(18.1272,90.3672577679157,2.17912691682577));
#71250=CARTESIAN_POINT('Ctrl Pts',(18.3,90.2270122110844,2.14311051219702));
#71251=CARTESIAN_POINT('Ctrl Pts',(18.1272,90.2270122110844,2.14311051219702));
#71252=CARTESIAN_POINT('Ctrl Pts',(18.3,89.9890859663486,2.14311051219702));
#71253=CARTESIAN_POINT('Ctrl Pts',(18.1272,89.9890859663486,2.14311051219702));
#71254=CARTESIAN_POINT('',(18.3,90.3672577679157,2.17912691682577));
#71255=CARTESIAN_POINT('Ctrl Pts',(18.3,90.3672577679157,2.17912691682577));
#71256=CARTESIAN_POINT('Ctrl Pts',(18.3,90.2270122110844,2.14311051219702));
#71257=CARTESIAN_POINT('Ctrl Pts',(18.3,89.9890859663486,2.14311051219702));
#71258=CARTESIAN_POINT('',(18.18,90.3672577679157,2.17912691682577));
#71259=CARTESIAN_POINT('',(18.3,90.3672577679157,2.17912691682577));
#71260=CARTESIAN_POINT('Ctrl Pts',(18.18,90.3672577679157,2.17912691682577));
#71261=CARTESIAN_POINT('Ctrl Pts',(18.18,90.2270122110844,2.14311051219702));
#71262=CARTESIAN_POINT('Ctrl Pts',(18.18,89.9890859663486,2.14311051219702));
#71263=CARTESIAN_POINT('Ctrl Pts',(18.3,90.605184161663,2.2784447953105));
#71264=CARTESIAN_POINT('Ctrl Pts',(18.1272,90.605184161663,2.2784447953105));
#71265=CARTESIAN_POINT('Ctrl Pts',(18.3,90.5075034737587,2.21514317244291));
#71266=CARTESIAN_POINT('Ctrl Pts',(18.1272,90.5075034737587,2.21514317244291));
#71267=CARTESIAN_POINT('Ctrl Pts',(18.3,90.3672577679157,2.17912691682577));
#71268=CARTESIAN_POINT('Ctrl Pts',(18.1272,90.3672577679157,2.17912691682577));
#71269=CARTESIAN_POINT('',(18.3,90.605184161663,2.2784447953105));
#71270=CARTESIAN_POINT('Ctrl Pts',(18.3,90.605184161663,2.2784447953105));
#71271=CARTESIAN_POINT('Ctrl Pts',(18.3,90.5075034737587,2.21514317244291));
#71272=CARTESIAN_POINT('Ctrl Pts',(18.3,90.3672577679157,2.17912691682577));
#71273=CARTESIAN_POINT('',(18.18,90.605184161663,2.2784447953105));
#71274=CARTESIAN_POINT('',(18.3,90.605184161663,2.2784447953105));
#71275=CARTESIAN_POINT('Ctrl Pts',(18.18,90.605184161663,2.2784447953105));
#71276=CARTESIAN_POINT('Ctrl Pts',(18.18,90.5075034737587,2.21514317244291));
#71277=CARTESIAN_POINT('Ctrl Pts',(18.18,90.3672577679157,2.17912691682577));
#71278=CARTESIAN_POINT('Ctrl Pts',(18.3,90.7547067344189,2.43888142555952));
#71279=CARTESIAN_POINT('Ctrl Pts',(18.1272,90.7547067344189,2.43888142555952));
#71280=CARTESIAN_POINT('Ctrl Pts',(18.3,90.702864998579,2.34174626916647));
#71281=CARTESIAN_POINT('Ctrl Pts',(18.1272,90.702864998579,2.34174626916647));
#71282=CARTESIAN_POINT('Ctrl Pts',(18.3,90.605184161663,2.2784447953105));
#71283=CARTESIAN_POINT('Ctrl Pts',(18.1272,90.605184161663,2.2784447953105));
#71284=CARTESIAN_POINT('',(18.3,90.7547067344189,2.43888142555952));
#71285=CARTESIAN_POINT('Ctrl Pts',(18.3,90.7547067344189,2.43888142555952));
#71286=CARTESIAN_POINT('Ctrl Pts',(18.3,90.702864998579,2.34174626916647));
#71287=CARTESIAN_POINT('Ctrl Pts',(18.3,90.605184161663,2.2784447953105));
#71288=CARTESIAN_POINT('',(18.18,90.7547067344189,2.43888142555952));
#71289=CARTESIAN_POINT('',(18.3,90.7547067344189,2.43888142555952));
#71290=CARTESIAN_POINT('Ctrl Pts',(18.18,90.7547067344189,2.43888142555952));
#71291=CARTESIAN_POINT('Ctrl Pts',(18.18,90.702864998579,2.34174626916647));
#71292=CARTESIAN_POINT('Ctrl Pts',(18.18,90.605184161663,2.2784447953105));
#71293=CARTESIAN_POINT('Ctrl Pts',(18.3,90.8065484702587,2.66480210274458));
#71294=CARTESIAN_POINT('Ctrl Pts',(18.1272,90.8065484702587,2.66480210274458));
#71295=CARTESIAN_POINT('Ctrl Pts',(18.3,90.8065484702587,2.53601643294096));
#71296=CARTESIAN_POINT('Ctrl Pts',(18.1272,90.8065484702587,2.53601643294096));
#71297=CARTESIAN_POINT('Ctrl Pts',(18.3,90.7547067344189,2.43888142555952));
#71298=CARTESIAN_POINT('Ctrl Pts',(18.1272,90.7547067344189,2.43888142555952));
#71299=CARTESIAN_POINT('',(18.3,90.8065484702587,2.66480210274458));
#71300=CARTESIAN_POINT('Ctrl Pts',(18.3,90.8065484702587,2.66480210274458));
#71301=CARTESIAN_POINT('Ctrl Pts',(18.3,90.8065484702587,2.53601643294096));
#71302=CARTESIAN_POINT('Ctrl Pts',(18.3,90.7547067344189,2.43888142555952));
#71303=CARTESIAN_POINT('',(18.18,90.8065484702587,2.66480210274458));
#71304=CARTESIAN_POINT('',(18.3,90.8065484702587,2.66480210274458));
#71305=CARTESIAN_POINT('Ctrl Pts',(18.18,90.8065484702587,2.66480210274458));
#71306=CARTESIAN_POINT('Ctrl Pts',(18.18,90.8065484702587,2.53601643294096));
#71307=CARTESIAN_POINT('Ctrl Pts',(18.18,90.7547067344189,2.43888142555952));
#71308=CARTESIAN_POINT('Ctrl Pts',(18.3,90.7126876950264,2.95457023233175));
#71309=CARTESIAN_POINT('Ctrl Pts',(18.1272,90.7126876950264,2.95457023233175));
#71310=CARTESIAN_POINT('Ctrl Pts',(18.3,90.8065484702587,2.83942702263594));
#71311=CARTESIAN_POINT('Ctrl Pts',(18.1272,90.8065484702587,2.83942702263594));
#71312=CARTESIAN_POINT('Ctrl Pts',(18.3,90.8065484702587,2.66480210274458));
#71313=CARTESIAN_POINT('Ctrl Pts',(18.1272,90.8065484702587,2.66480210274458));
#71314=CARTESIAN_POINT('',(18.3,90.7126876950264,2.95457023233175));
#71315=CARTESIAN_POINT('Ctrl Pts',(18.3,90.7126876950264,2.95457023233175));
#71316=CARTESIAN_POINT('Ctrl Pts',(18.3,90.8065484702587,2.83942702263594));
#71317=CARTESIAN_POINT('Ctrl Pts',(18.3,90.8065484702587,2.66480210274458));
#71318=CARTESIAN_POINT('',(18.18,90.7126876950264,2.95457023233175));
#71319=CARTESIAN_POINT('',(18.3,90.7126876950264,2.95457023233175));
#71320=CARTESIAN_POINT('Ctrl Pts',(18.18,90.7126876950264,2.95457023233175));
#71321=CARTESIAN_POINT('Ctrl Pts',(18.18,90.8065484702587,2.83942702263594));
#71322=CARTESIAN_POINT('Ctrl Pts',(18.18,90.8065484702587,2.66480210274458));
#71323=CARTESIAN_POINT('Ctrl Pts',(18.3,90.4458390414715,3.12810364216566));
#71324=CARTESIAN_POINT('Ctrl Pts',(18.1272,90.4458390414715,3.12810364216566));
#71325=CARTESIAN_POINT('Ctrl Pts',(18.3,90.6188267707825,3.06971344202757));
#71326=CARTESIAN_POINT('Ctrl Pts',(18.1272,90.6188267707825,3.06971344202757));
#71327=CARTESIAN_POINT('Ctrl Pts',(18.3,90.7126876950264,2.95457023233175));
#71328=CARTESIAN_POINT('Ctrl Pts',(18.1272,90.7126876950264,2.95457023233175));
#71329=CARTESIAN_POINT('',(18.3,90.4458390414715,3.12810364216566));
#71330=CARTESIAN_POINT('Ctrl Pts',(18.3,90.4458390414715,3.12810364216566));
#71331=CARTESIAN_POINT('Ctrl Pts',(18.3,90.6188267707825,3.06971344202757));
#71332=CARTESIAN_POINT('Ctrl Pts',(18.3,90.7126876950264,2.95457023233175));
#71333=CARTESIAN_POINT('',(18.18,90.4458390414715,3.12810364216566));
#71334=CARTESIAN_POINT('',(18.3,90.4458390414715,3.12810364216566));
#71335=CARTESIAN_POINT('Ctrl Pts',(18.18,90.4458390414715,3.12810364216566));
#71336=CARTESIAN_POINT('Ctrl Pts',(18.18,90.6188267707825,3.06971344202757));
#71337=CARTESIAN_POINT('Ctrl Pts',(18.18,90.7126876950264,2.95457023233175));
#71338=CARTESIAN_POINT('Ctrl Pts',(18.3,89.9890859663486,3.18649384230375));
#71339=CARTESIAN_POINT('Ctrl Pts',(18.1272,89.9890859663486,3.18649384230375));
#71340=CARTESIAN_POINT('Ctrl Pts',(18.3,90.2728513121605,3.18649384230375));
#71341=CARTESIAN_POINT('Ctrl Pts',(18.1272,90.2728513121605,3.18649384230375));
#71342=CARTESIAN_POINT('Ctrl Pts',(18.3,90.4458390414715,3.12810364216566));
#71343=CARTESIAN_POINT('Ctrl Pts',(18.1272,90.4458390414715,3.12810364216566));
#71344=CARTESIAN_POINT('',(18.3,89.9890859663486,3.18649384230375));
#71345=CARTESIAN_POINT('Ctrl Pts',(18.3,89.9890859663486,3.18649384230375));
#71346=CARTESIAN_POINT('Ctrl Pts',(18.3,90.2728513121605,3.18649384230375));
#71347=CARTESIAN_POINT('Ctrl Pts',(18.3,90.4458390414715,3.12810364216566));
#71348=CARTESIAN_POINT('',(18.18,89.9890859663486,3.18649384230375));
#71349=CARTESIAN_POINT('',(18.3,89.9890859663486,3.18649384230375));
#71350=CARTESIAN_POINT('Ctrl Pts',(18.18,89.9890859663486,3.18649384230375));
#71351=CARTESIAN_POINT('Ctrl Pts',(18.18,90.2728513121605,3.18649384230375));
#71352=CARTESIAN_POINT('Ctrl Pts',(18.18,90.4458390414715,3.12810364216566));
#71353=CARTESIAN_POINT('Ctrl Pts',(18.3,89.3386085569858,3.02824008315802));
#71354=CARTESIAN_POINT('Ctrl Pts',(18.1272,89.3386085569858,3.02824008315802));
#71355=CARTESIAN_POINT('Ctrl Pts',(18.3,89.5383356750011,3.18649384230375));
#71356=CARTESIAN_POINT('Ctrl Pts',(18.1272,89.5383356750011,3.18649384230375));
#71357=CARTESIAN_POINT('Ctrl Pts',(18.3,89.9890859663486,3.18649384230375));
#71358=CARTESIAN_POINT('Ctrl Pts',(18.1272,89.9890859663486,3.18649384230375));
#71359=CARTESIAN_POINT('Ctrl Pts',(18.3,89.3386085569858,3.02824008315802));
#71360=CARTESIAN_POINT('Ctrl Pts',(18.3,89.5383356750011,3.18649384230375));
#71361=CARTESIAN_POINT('Ctrl Pts',(18.3,89.9890859663486,3.18649384230375));
#71362=CARTESIAN_POINT('Ctrl Pts',(18.18,89.3386085569858,3.02824008315802));
#71363=CARTESIAN_POINT('Ctrl Pts',(18.18,89.5383356750011,3.18649384230375));
#71364=CARTESIAN_POINT('Ctrl Pts',(18.18,89.9890859663486,3.18649384230375));
#71365=CARTESIAN_POINT('Origin',(18.18,89.9896316468716,3.29999995455146));
#71366=CARTESIAN_POINT('Ctrl Pts',(18.3,89.4952251255512,4.09890851974487));
#71367=CARTESIAN_POINT('Ctrl Pts',(18.1272,89.4952251255512,4.09890851974487));
#71368=CARTESIAN_POINT('Ctrl Pts',(18.3,89.4422920286655,4.14911313951015));
#71369=CARTESIAN_POINT('Ctrl Pts',(18.1272,89.4422920286655,4.14911313951015));
#71370=CARTESIAN_POINT('Ctrl Pts',(18.3,89.3888132512569,4.18185527473688));
#71371=CARTESIAN_POINT('Ctrl Pts',(18.1272,89.3888132512569,4.18185527473688));
#71372=CARTESIAN_POINT('',(18.3,89.4952251255512,4.09890851974487));
#71373=CARTESIAN_POINT('',(18.3,89.3888132512569,4.18185527473688));
#71374=CARTESIAN_POINT('Ctrl Pts',(18.3,89.4952251255512,4.09890851974487));
#71375=CARTESIAN_POINT('Ctrl Pts',(18.3,89.4422920286655,4.14911313951015));
#71376=CARTESIAN_POINT('Ctrl Pts',(18.3,89.3888132512569,4.18185527473688));
#71377=CARTESIAN_POINT('',(18.18,89.4952251255512,4.09890851974487));
#71378=CARTESIAN_POINT('',(18.3,89.4952251255512,4.09890851974487));
#71379=CARTESIAN_POINT('',(18.18,89.3888132512569,4.18185527473688));
#71380=CARTESIAN_POINT('Ctrl Pts',(18.18,89.4952251255512,4.09890851974487));
#71381=CARTESIAN_POINT('Ctrl Pts',(18.18,89.4422920286655,4.14911313951015));
#71382=CARTESIAN_POINT('Ctrl Pts',(18.18,89.3888132512569,4.18185527473688));
#71383=CARTESIAN_POINT('',(18.3,89.3888132512569,4.18185527473688));
#71384=CARTESIAN_POINT('Ctrl Pts',(18.3,89.6965892851353,3.87189629524946));
#71385=CARTESIAN_POINT('Ctrl Pts',(18.1272,89.6965892851353,3.87189629524946));
#71386=CARTESIAN_POINT('Ctrl Pts',(18.3,89.5481582224369,4.04870386272669));
#71387=CARTESIAN_POINT('Ctrl Pts',(18.1272,89.5481582224369,4.04870386272669));
#71388=CARTESIAN_POINT('Ctrl Pts',(18.3,89.4952251255512,4.09890851974487));
#71389=CARTESIAN_POINT('Ctrl Pts',(18.1272,89.4952251255512,4.09890851974487));
#71390=CARTESIAN_POINT('',(18.3,89.6965892851353,3.87189629524946));
#71391=CARTESIAN_POINT('Ctrl Pts',(18.3,89.6965892851353,3.87189629524946));
#71392=CARTESIAN_POINT('Ctrl Pts',(18.3,89.5481582224369,4.04870386272669));
#71393=CARTESIAN_POINT('Ctrl Pts',(18.3,89.4952251255512,4.09890851974487));
#71394=CARTESIAN_POINT('',(18.18,89.6965892851353,3.87189629524946));
#71395=CARTESIAN_POINT('',(18.3,89.6965892851353,3.87189629524946));
#71396=CARTESIAN_POINT('Ctrl Pts',(18.18,89.6965892851353,3.87189629524946));
#71397=CARTESIAN_POINT('Ctrl Pts',(18.18,89.5481582224369,4.04870386272669));
#71398=CARTESIAN_POINT('Ctrl Pts',(18.18,89.4952251255512,4.09890851974487));
#71399=CARTESIAN_POINT('Ctrl Pts',(18.3,89.978172057867,3.5690313860774));
#71400=CARTESIAN_POINT('Ctrl Pts',(18.1272,89.978172057867,3.5690313860774));
#71401=CARTESIAN_POINT('Ctrl Pts',(18.3,89.8755799472332,3.66016360968351));
#71402=CARTESIAN_POINT('Ctrl Pts',(18.1272,89.8755799472332,3.66016360968351));
#71403=CARTESIAN_POINT('Ctrl Pts',(18.3,89.6965892851353,3.87189629524946));
#71404=CARTESIAN_POINT('Ctrl Pts',(18.1272,89.6965892851353,3.87189629524946));
#71405=CARTESIAN_POINT('',(18.3,89.978172057867,3.5690313860774));
#71406=CARTESIAN_POINT('Ctrl Pts',(18.3,89.978172057867,3.5690313860774));
#71407=CARTESIAN_POINT('Ctrl Pts',(18.3,89.8755799472332,3.66016360968351));
#71408=CARTESIAN_POINT('Ctrl Pts',(18.3,89.6965892851353,3.87189629524946));
#71409=CARTESIAN_POINT('',(18.18,89.978172057867,3.5690313860774));
#71410=CARTESIAN_POINT('',(18.3,89.978172057867,3.5690313860774));
#71411=CARTESIAN_POINT('Ctrl Pts',(18.18,89.978172057867,3.5690313860774));
#71412=CARTESIAN_POINT('Ctrl Pts',(18.18,89.8755799472332,3.66016360968351));
#71413=CARTESIAN_POINT('Ctrl Pts',(18.18,89.6965892851353,3.87189629524946));
#71414=CARTESIAN_POINT('Ctrl Pts',(18.3,90.1735334336758,3.4386083766818));
#71415=CARTESIAN_POINT('Ctrl Pts',(18.1272,90.1735334336758,3.4386083766818));
#71416=CARTESIAN_POINT('Ctrl Pts',(18.3,90.0807640194893,3.47789901345968));
#71417=CARTESIAN_POINT('Ctrl Pts',(18.1272,90.0807640194893,3.47789901345968));
#71418=CARTESIAN_POINT('Ctrl Pts',(18.3,89.978172057867,3.5690313860774));
#71419=CARTESIAN_POINT('Ctrl Pts',(18.1272,89.978172057867,3.5690313860774));
#71420=CARTESIAN_POINT('',(18.3,90.1735334336758,3.4386083766818));
#71421=CARTESIAN_POINT('Ctrl Pts',(18.3,90.1735334336758,3.4386083766818));
#71422=CARTESIAN_POINT('Ctrl Pts',(18.3,90.0807640194893,3.47789901345968));
#71423=CARTESIAN_POINT('Ctrl Pts',(18.3,89.978172057867,3.5690313860774));
#71424=CARTESIAN_POINT('',(18.18,90.1735334336758,3.4386083766818));
#71425=CARTESIAN_POINT('',(18.3,90.1735334336758,3.4386083766818));
#71426=CARTESIAN_POINT('Ctrl Pts',(18.18,90.1735334336758,3.4386083766818));
#71427=CARTESIAN_POINT('Ctrl Pts',(18.18,90.0807640194893,3.47789901345968));
#71428=CARTESIAN_POINT('Ctrl Pts',(18.18,89.978172057867,3.5690313860774));
#71429=CARTESIAN_POINT('Ctrl Pts',(18.3,90.3623466432094,3.39931788891554));
#71430=CARTESIAN_POINT('Ctrl Pts',(18.1272,90.3623466432094,3.39931788891554));
#71431=CARTESIAN_POINT('Ctrl Pts',(18.3,90.2663029968738,3.39931788891554));
#71432=CARTESIAN_POINT('Ctrl Pts',(18.1272,90.2663029968738,3.39931788891554));
#71433=CARTESIAN_POINT('Ctrl Pts',(18.3,90.1735334336758,3.4386083766818));
#71434=CARTESIAN_POINT('Ctrl Pts',(18.1272,90.1735334336758,3.4386083766818));
#71435=CARTESIAN_POINT('',(18.3,90.3623466432094,3.39931788891554));
#71436=CARTESIAN_POINT('Ctrl Pts',(18.3,90.3623466432094,3.39931788891554));
#71437=CARTESIAN_POINT('Ctrl Pts',(18.3,90.2663029968738,3.39931788891554));
#71438=CARTESIAN_POINT('Ctrl Pts',(18.3,90.1735334336758,3.4386083766818));
#71439=CARTESIAN_POINT('',(18.18,90.3623466432094,3.39931788891554));
#71440=CARTESIAN_POINT('',(18.3,90.3623466432094,3.39931788891554));
#71441=CARTESIAN_POINT('Ctrl Pts',(18.18,90.3623466432094,3.39931788891554));
#71442=CARTESIAN_POINT('Ctrl Pts',(18.18,90.2663029968738,3.39931788891554));
#71443=CARTESIAN_POINT('Ctrl Pts',(18.18,90.1735334336758,3.4386083766818));
#71444=CARTESIAN_POINT('Ctrl Pts',(18.3,90.6788541615009,3.53356066197157));
#71445=CARTESIAN_POINT('Ctrl Pts',(18.1272,90.6788541615009,3.53356066197157));
#71446=CARTESIAN_POINT('Ctrl Pts',(18.3,90.5511597037315,3.39931788891554));
#71447=CARTESIAN_POINT('Ctrl Pts',(18.1272,90.5511597037315,3.39931788891554));
#71448=CARTESIAN_POINT('Ctrl Pts',(18.3,90.3623466432094,3.39931788891554));
#71449=CARTESIAN_POINT('Ctrl Pts',(18.1272,90.3623466432094,3.39931788891554));
#71450=CARTESIAN_POINT('',(18.3,90.6788541615009,3.53356066197157));
#71451=CARTESIAN_POINT('Ctrl Pts',(18.3,90.6788541615009,3.53356066197157));
#71452=CARTESIAN_POINT('Ctrl Pts',(18.3,90.5511597037315,3.39931788891554));
#71453=CARTESIAN_POINT('Ctrl Pts',(18.3,90.3623466432094,3.39931788891554));
#71454=CARTESIAN_POINT('',(18.18,90.6788541615009,3.53356066197157));
#71455=CARTESIAN_POINT('',(18.3,90.6788541615009,3.53356066197157));
#71456=CARTESIAN_POINT('Ctrl Pts',(18.18,90.6788541615009,3.53356066197157));
#71457=CARTESIAN_POINT('Ctrl Pts',(18.18,90.5511597037315,3.39931788891554));
#71458=CARTESIAN_POINT('Ctrl Pts',(18.18,90.3623466432094,3.39931788891554));
#71459=CARTESIAN_POINT('Ctrl Pts',(18.3,90.8065484702587,3.89809000343084));
#71460=CARTESIAN_POINT('Ctrl Pts',(18.1272,90.8065484702587,3.89809000343084));
#71461=CARTESIAN_POINT('Ctrl Pts',(18.3,90.8065484702587,3.6678034350276));
#71462=CARTESIAN_POINT('Ctrl Pts',(18.1272,90.8065484702587,3.6678034350276));
#71463=CARTESIAN_POINT('Ctrl Pts',(18.3,90.6788541615009,3.53356066197157));
#71464=CARTESIAN_POINT('Ctrl Pts',(18.1272,90.6788541615009,3.53356066197157));
#71465=CARTESIAN_POINT('',(18.3,90.8065484702587,3.89809000343084));
#71466=CARTESIAN_POINT('Ctrl Pts',(18.3,90.8065484702587,3.89809000343084));
#71467=CARTESIAN_POINT('Ctrl Pts',(18.3,90.8065484702587,3.6678034350276));
#71468=CARTESIAN_POINT('Ctrl Pts',(18.3,90.6788541615009,3.53356066197157));
#71469=CARTESIAN_POINT('',(18.18,90.8065484702587,3.89809000343084));
#71470=CARTESIAN_POINT('',(18.3,90.8065484702587,3.89809000343084));
#71471=CARTESIAN_POINT('Ctrl Pts',(18.18,90.8065484702587,3.89809000343084));
#71472=CARTESIAN_POINT('Ctrl Pts',(18.18,90.8065484702587,3.6678034350276));
#71473=CARTESIAN_POINT('Ctrl Pts',(18.18,90.6788541615009,3.53356066197157));
#71474=CARTESIAN_POINT('Ctrl Pts',(18.3,90.6881310284138,4.26152787208557));
#71475=CARTESIAN_POINT('Ctrl Pts',(18.1272,90.6881310284138,4.26152787208557));
#71476=CARTESIAN_POINT('Ctrl Pts',(18.3,90.8065484702587,4.12619362622499));
#71477=CARTESIAN_POINT('Ctrl Pts',(18.1272,90.8065484702587,4.12619362622499));
#71478=CARTESIAN_POINT('Ctrl Pts',(18.3,90.8065484702587,3.89809000343084));
#71479=CARTESIAN_POINT('Ctrl Pts',(18.1272,90.8065484702587,3.89809000343084));
#71480=CARTESIAN_POINT('',(18.3,90.6881310284138,4.26152787208557));
#71481=CARTESIAN_POINT('Ctrl Pts',(18.3,90.6881310284138,4.26152787208557));
#71482=CARTESIAN_POINT('Ctrl Pts',(18.3,90.8065484702587,4.12619362622499));
#71483=CARTESIAN_POINT('Ctrl Pts',(18.3,90.8065484702587,3.89809000343084));
#71484=CARTESIAN_POINT('',(18.18,90.6881310284138,4.26152787208557));
#71485=CARTESIAN_POINT('',(18.3,90.6881310284138,4.26152787208557));
#71486=CARTESIAN_POINT('Ctrl Pts',(18.18,90.6881310284138,4.26152787208557));
#71487=CARTESIAN_POINT('Ctrl Pts',(18.18,90.8065484702587,4.12619362622499));
#71488=CARTESIAN_POINT('Ctrl Pts',(18.18,90.8065484702587,3.89809000343084));
#71489=CARTESIAN_POINT('Ctrl Pts',(18.3,90.3437926113605,4.41759881600738));
#71490=CARTESIAN_POINT('Ctrl Pts',(18.1272,90.3437926113605,4.41759881600738));
#71491=CARTESIAN_POINT('Ctrl Pts',(18.3,90.5697135865688,4.39686211794615));
#71492=CARTESIAN_POINT('Ctrl Pts',(18.1272,90.5697135865688,4.39686211794615));
#71493=CARTESIAN_POINT('Ctrl Pts',(18.3,90.6881310284138,4.26152787208557));
#71494=CARTESIAN_POINT('Ctrl Pts',(18.1272,90.6881310284138,4.26152787208557));
#71495=CARTESIAN_POINT('',(18.3,90.3437926113605,4.41759881600738));
#71496=CARTESIAN_POINT('Ctrl Pts',(18.3,90.3437926113605,4.41759881600738));
#71497=CARTESIAN_POINT('Ctrl Pts',(18.3,90.5697135865688,4.39686211794615));
#71498=CARTESIAN_POINT('Ctrl Pts',(18.3,90.6881310284138,4.26152787208557));
#71499=CARTESIAN_POINT('',(18.18,90.3437926113605,4.41759881600738));
#71500=CARTESIAN_POINT('',(18.3,90.3437926113605,4.41759881600738));
#71501=CARTESIAN_POINT('Ctrl Pts',(18.18,90.3437926113605,4.41759881600738));
#71502=CARTESIAN_POINT('Ctrl Pts',(18.18,90.5697135865688,4.39686211794615));
#71503=CARTESIAN_POINT('Ctrl Pts',(18.18,90.6881310284138,4.26152787208557));
#71504=CARTESIAN_POINT('Origin',(18.3,90.3230560064316,4.21568888276815));
#71505=CARTESIAN_POINT('',(18.3,90.3230560064316,4.21568888276815));
#71506=CARTESIAN_POINT('',(18.3,90.2822558942559,3.8184228908779));
#71507=CARTESIAN_POINT('',(18.18,90.3230560064316,4.21568888276815));
#71508=CARTESIAN_POINT('',(18.3,90.3230560064316,4.21568888276815));
#71509=CARTESIAN_POINT('',(18.18,90.3230560064316,4.21568888276815));
#71510=CARTESIAN_POINT('Ctrl Pts',(18.3,90.5587995290756,4.12946785837412));
#71511=CARTESIAN_POINT('Ctrl Pts',(18.1272,90.5587995290756,4.12946785837412));
#71512=CARTESIAN_POINT('Ctrl Pts',(18.3,90.4736699402332,4.21459744721651));
#71513=CARTESIAN_POINT('Ctrl Pts',(18.1272,90.4736699402332,4.21459744721651));
#71514=CARTESIAN_POINT('Ctrl Pts',(18.3,90.3230560064316,4.21568888276815));
#71515=CARTESIAN_POINT('Ctrl Pts',(18.1272,90.3230560064316,4.21568888276815));
#71516=CARTESIAN_POINT('',(18.3,90.5587995290756,4.12946785837412));
#71517=CARTESIAN_POINT('Ctrl Pts',(18.3,90.5587995290756,4.12946785837412));
#71518=CARTESIAN_POINT('Ctrl Pts',(18.3,90.4736699402332,4.21459744721651));
#71519=CARTESIAN_POINT('Ctrl Pts',(18.3,90.3230560064316,4.21568888276815));
#71520=CARTESIAN_POINT('',(18.18,90.5587995290756,4.12946785837412));
#71521=CARTESIAN_POINT('',(18.3,90.5587995290756,4.12946785837412));
#71522=CARTESIAN_POINT('Ctrl Pts',(18.18,90.5587995290756,4.12946785837412));
#71523=CARTESIAN_POINT('Ctrl Pts',(18.18,90.4736699402332,4.21459744721651));
#71524=CARTESIAN_POINT('Ctrl Pts',(18.18,90.3230560064316,4.21568888276815));
#71525=CARTESIAN_POINT('Ctrl Pts',(18.3,90.643929117918,3.9024555966258));
#71526=CARTESIAN_POINT('Ctrl Pts',(18.1272,90.643929117918,3.9024555966258));
#71527=CARTESIAN_POINT('Ctrl Pts',(18.3,90.643929117918,4.04433826953173));
#71528=CARTESIAN_POINT('Ctrl Pts',(18.1272,90.643929117918,4.04433826953173));
#71529=CARTESIAN_POINT('Ctrl Pts',(18.3,90.5587995290756,4.12946785837412));
#71530=CARTESIAN_POINT('Ctrl Pts',(18.1272,90.5587995290756,4.12946785837412));
#71531=CARTESIAN_POINT('',(18.3,90.643929117918,3.9024555966258));
#71532=CARTESIAN_POINT('Ctrl Pts',(18.3,90.643929117918,3.9024555966258));
#71533=CARTESIAN_POINT('Ctrl Pts',(18.3,90.643929117918,4.04433826953173));
#71534=CARTESIAN_POINT('Ctrl Pts',(18.3,90.5587995290756,4.12946785837412));
#71535=CARTESIAN_POINT('',(18.18,90.643929117918,3.9024555966258));
#71536=CARTESIAN_POINT('',(18.3,90.643929117918,3.9024555966258));
#71537=CARTESIAN_POINT('Ctrl Pts',(18.18,90.643929117918,3.9024555966258));
#71538=CARTESIAN_POINT('Ctrl Pts',(18.18,90.643929117918,4.04433826953173));
#71539=CARTESIAN_POINT('Ctrl Pts',(18.18,90.5587995290756,4.12946785837412));
#71540=CARTESIAN_POINT('Ctrl Pts',(18.3,90.5637108027935,3.68472027629614));
#71541=CARTESIAN_POINT('Ctrl Pts',(18.1272,90.5637108027935,3.68472027629614));
#71542=CARTESIAN_POINT('Ctrl Pts',(18.3,90.643929117918,3.76821282356977));
#71543=CARTESIAN_POINT('Ctrl Pts',(18.1272,90.643929117918,3.76821282356977));
#71544=CARTESIAN_POINT('Ctrl Pts',(18.3,90.643929117918,3.9024555966258));
#71545=CARTESIAN_POINT('Ctrl Pts',(18.1272,90.643929117918,3.9024555966258));
#71546=CARTESIAN_POINT('',(18.3,90.5637108027935,3.68472027629614));
#71547=CARTESIAN_POINT('Ctrl Pts',(18.3,90.5637108027935,3.68472027629614));
#71548=CARTESIAN_POINT('Ctrl Pts',(18.3,90.643929117918,3.76821282356977));
#71549=CARTESIAN_POINT('Ctrl Pts',(18.3,90.643929117918,3.9024555966258));
#71550=CARTESIAN_POINT('',(18.18,90.5637108027935,3.68472027629614));
#71551=CARTESIAN_POINT('',(18.3,90.5637108027935,3.68472027629614));
#71552=CARTESIAN_POINT('Ctrl Pts',(18.18,90.5637108027935,3.68472027629614));
#71553=CARTESIAN_POINT('Ctrl Pts',(18.18,90.643929117918,3.76821282356977));
#71554=CARTESIAN_POINT('Ctrl Pts',(18.18,90.643929117918,3.9024555966258));
#71555=CARTESIAN_POINT('Ctrl Pts',(18.3,90.3667122364044,3.6012277290225));
#71556=CARTESIAN_POINT('Ctrl Pts',(18.1272,90.3667122364044,3.6012277290225));
#71557=CARTESIAN_POINT('Ctrl Pts',(18.3,90.4834926366806,3.6012277290225));
#71558=CARTESIAN_POINT('Ctrl Pts',(18.1272,90.4834926366806,3.6012277290225));
#71559=CARTESIAN_POINT('Ctrl Pts',(18.3,90.5637108027935,3.68472027629614));
#71560=CARTESIAN_POINT('Ctrl Pts',(18.1272,90.5637108027935,3.68472027629614));
#71561=CARTESIAN_POINT('',(18.3,90.3667122364044,3.6012277290225));
#71562=CARTESIAN_POINT('Ctrl Pts',(18.3,90.3667122364044,3.6012277290225));
#71563=CARTESIAN_POINT('Ctrl Pts',(18.3,90.4834926366806,3.6012277290225));
#71564=CARTESIAN_POINT('Ctrl Pts',(18.3,90.5637108027935,3.68472027629614));
#71565=CARTESIAN_POINT('',(18.18,90.3667122364044,3.6012277290225));
#71566=CARTESIAN_POINT('',(18.3,90.3667122364044,3.6012277290225));
#71567=CARTESIAN_POINT('Ctrl Pts',(18.18,90.3667122364044,3.6012277290225));
#71568=CARTESIAN_POINT('Ctrl Pts',(18.18,90.4834926366806,3.6012277290225));
#71569=CARTESIAN_POINT('Ctrl Pts',(18.18,90.5637108027935,3.68472027629614));
#71570=CARTESIAN_POINT('Ctrl Pts',(18.3,90.1304228842258,3.69290578216314));
#71571=CARTESIAN_POINT('Ctrl Pts',(18.1272,90.1304228842258,3.69290578216314));
#71572=CARTESIAN_POINT('Ctrl Pts',(18.3,90.255388790369,3.6012277290225));
#71573=CARTESIAN_POINT('Ctrl Pts',(18.1272,90.255388790369,3.6012277290225));
#71574=CARTESIAN_POINT('Ctrl Pts',(18.3,90.3667122364044,3.6012277290225));
#71575=CARTESIAN_POINT('Ctrl Pts',(18.1272,90.3667122364044,3.6012277290225));
#71576=CARTESIAN_POINT('',(18.3,90.1304228842258,3.69290578216314));
#71577=CARTESIAN_POINT('Ctrl Pts',(18.3,90.1304228842258,3.69290578216314));
#71578=CARTESIAN_POINT('Ctrl Pts',(18.3,90.255388790369,3.6012277290225));
#71579=CARTESIAN_POINT('Ctrl Pts',(18.3,90.3667122364044,3.6012277290225));
#71580=CARTESIAN_POINT('',(18.18,90.1304228842258,3.69290578216314));
#71581=CARTESIAN_POINT('',(18.3,90.1304228842258,3.69290578216314));
#71582=CARTESIAN_POINT('Ctrl Pts',(18.18,90.1304228842258,3.69290578216314));
#71583=CARTESIAN_POINT('Ctrl Pts',(18.18,90.255388790369,3.6012277290225));
#71584=CARTESIAN_POINT('Ctrl Pts',(18.18,90.3667122364044,3.6012277290225));
#71585=CARTESIAN_POINT('Ctrl Pts',(18.3,89.791541570425,4.04542966783047));
#71586=CARTESIAN_POINT('Ctrl Pts',(18.1272,89.791541570425,4.04542966783047));
#71587=CARTESIAN_POINT('Ctrl Pts',(18.3,90.0054569780826,3.78458383530378));
#71588=CARTESIAN_POINT('Ctrl Pts',(18.1272,90.0054569780826,3.78458383530378));
#71589=CARTESIAN_POINT('Ctrl Pts',(18.3,90.1304228842258,3.69290578216314));
#71590=CARTESIAN_POINT('Ctrl Pts',(18.1272,90.1304228842258,3.69290578216314));
#71591=CARTESIAN_POINT('',(18.3,89.791541570425,4.04542966783047));
#71592=CARTESIAN_POINT('Ctrl Pts',(18.3,89.791541570425,4.04542966783047));
#71593=CARTESIAN_POINT('Ctrl Pts',(18.3,90.0054569780826,3.78458383530378));
#71594=CARTESIAN_POINT('Ctrl Pts',(18.3,90.1304228842258,3.69290578216314));
#71595=CARTESIAN_POINT('',(18.18,89.791541570425,4.04542966783047));
#71596=CARTESIAN_POINT('',(18.3,89.791541570425,4.04542966783047));
#71597=CARTESIAN_POINT('Ctrl Pts',(18.18,89.791541570425,4.04542966783047));
#71598=CARTESIAN_POINT('Ctrl Pts',(18.18,90.0054569780826,3.78458383530378));
#71599=CARTESIAN_POINT('Ctrl Pts',(18.18,90.1304228842258,3.69290578216314));
#71600=CARTESIAN_POINT('Ctrl Pts',(18.3,89.5492495834827,4.30245558768511));
#71601=CARTESIAN_POINT('Ctrl Pts',(18.1272,89.5492495834827,4.30245558768511));
#71602=CARTESIAN_POINT('Ctrl Pts',(18.3,89.6540247142315,4.21350604891777));
#71603=CARTESIAN_POINT('Ctrl Pts',(18.1272,89.6540247142315,4.21350604891777));
#71604=CARTESIAN_POINT('Ctrl Pts',(18.3,89.791541570425,4.04542966783047));
#71605=CARTESIAN_POINT('Ctrl Pts',(18.1272,89.791541570425,4.04542966783047));
#71606=CARTESIAN_POINT('',(18.3,89.5492495834827,4.30245558768511));
#71607=CARTESIAN_POINT('Ctrl Pts',(18.3,89.5492495834827,4.30245558768511));
#71608=CARTESIAN_POINT('Ctrl Pts',(18.3,89.6540247142315,4.21350604891777));
#71609=CARTESIAN_POINT('Ctrl Pts',(18.3,89.791541570425,4.04542966783047));
#71610=CARTESIAN_POINT('',(18.18,89.5492495834827,4.30245558768511));
#71611=CARTESIAN_POINT('',(18.3,89.5492495834827,4.30245558768511));
#71612=CARTESIAN_POINT('Ctrl Pts',(18.18,89.5492495834827,4.30245558768511));
#71613=CARTESIAN_POINT('Ctrl Pts',(18.18,89.6540247142315,4.21350604891777));
#71614=CARTESIAN_POINT('Ctrl Pts',(18.18,89.791541570425,4.04542966783047));
#71615=CARTESIAN_POINT('Ctrl Pts',(18.3,89.3364258348942,4.43178708702326));
#71616=CARTESIAN_POINT('Ctrl Pts',(18.1272,89.3364258348942,4.43178708702326));
#71617=CARTESIAN_POINT('Ctrl Pts',(18.3,89.4444747507572,4.39140508919954));
#71618=CARTESIAN_POINT('Ctrl Pts',(18.1272,89.4444747507572,4.39140508919954));
#71619=CARTESIAN_POINT('Ctrl Pts',(18.3,89.5492495834827,4.30245558768511));
#71620=CARTESIAN_POINT('Ctrl Pts',(18.1272,89.5492495834827,4.30245558768511));
#71621=CARTESIAN_POINT('',(18.3,89.3364258348942,4.43178708702326));
#71622=CARTESIAN_POINT('Ctrl Pts',(18.3,89.3364258348942,4.43178708702326));
#71623=CARTESIAN_POINT('Ctrl Pts',(18.3,89.4444747507572,4.39140508919954));
#71624=CARTESIAN_POINT('Ctrl Pts',(18.3,89.5492495834827,4.30245558768511));
#71625=CARTESIAN_POINT('',(18.18,89.3364258348942,4.43178708702326));
#71626=CARTESIAN_POINT('',(18.3,89.3364258348942,4.43178708702326));
#71627=CARTESIAN_POINT('Ctrl Pts',(18.18,89.3364258348942,4.43178708702326));
#71628=CARTESIAN_POINT('Ctrl Pts',(18.18,89.4444747507572,4.39140508919954));
#71629=CARTESIAN_POINT('Ctrl Pts',(18.18,89.5492495834827,4.30245558768511));
#71630=CARTESIAN_POINT('Ctrl Pts',(18.3,89.2000000417232,4.45470658168197));
#71631=CARTESIAN_POINT('Ctrl Pts',(18.1272,89.2000000417232,4.45470658168197));
#71632=CARTESIAN_POINT('Ctrl Pts',(18.3,89.2709414899349,4.4568893969059));
#71633=CARTESIAN_POINT('Ctrl Pts',(18.1272,89.2709414899349,4.4568893969059));
#71634=CARTESIAN_POINT('Ctrl Pts',(18.3,89.3364258348942,4.43178708702326));
#71635=CARTESIAN_POINT('Ctrl Pts',(18.1272,89.3364258348942,4.43178708702326));
#71636=CARTESIAN_POINT('',(18.3,89.2000000417232,4.45470658168197));
#71637=CARTESIAN_POINT('Ctrl Pts',(18.3,89.2000000417232,4.45470658168197));
#71638=CARTESIAN_POINT('Ctrl Pts',(18.3,89.2709414899349,4.4568893969059));
#71639=CARTESIAN_POINT('Ctrl Pts',(18.3,89.3364258348942,4.43178708702326));
#71640=CARTESIAN_POINT('',(18.18,89.2000000417232,4.45470658168197));
#71641=CARTESIAN_POINT('',(18.3,89.2000000417232,4.45470658168197));
#71642=CARTESIAN_POINT('Ctrl Pts',(18.18,89.2000000417232,4.45470658168197));
#71643=CARTESIAN_POINT('Ctrl Pts',(18.18,89.2709414899349,4.4568893969059));
#71644=CARTESIAN_POINT('Ctrl Pts',(18.18,89.3364258348942,4.43178708702326));
#71645=CARTESIAN_POINT('Origin',(18.3,89.2000000417232,3.39713501781225));
#71646=CARTESIAN_POINT('',(18.3,89.2000000417232,3.39713501781225));
#71647=CARTESIAN_POINT('',(18.3,89.2000000417232,4.44856750890613));
#71648=CARTESIAN_POINT('',(18.18,89.2000000417232,3.39713501781225));
#71649=CARTESIAN_POINT('',(18.3,89.2000000417232,3.39713501781225));
#71650=CARTESIAN_POINT('',(18.18,89.2000000417232,3.39713501781225));
#71651=CARTESIAN_POINT('Origin',(18.3,89.3888132512569,3.39713501781225));
#71652=CARTESIAN_POINT('',(18.3,89.3888132512569,3.39713501781225));
#71653=CARTESIAN_POINT('',(18.3,79.6944066256285,3.39713501781225));
#71654=CARTESIAN_POINT('',(18.18,89.3888132512569,3.39713501781225));
#71655=CARTESIAN_POINT('',(18.3,89.3888132512569,3.39713501781225));
#71656=CARTESIAN_POINT('',(18.18,89.3888132512569,3.39713501781225));
#71657=CARTESIAN_POINT('Origin',(18.3,89.3888132512569,4.18185527473688));
#71658=CARTESIAN_POINT('',(18.3,89.3888132512569,4.84092763736844));
#71659=CARTESIAN_POINT('',(18.18,89.3888132512569,4.18185527473688));
#71660=CARTESIAN_POINT('Origin',(18.18,89.9896316468716,3.29999995455146));
#71661=CARTESIAN_POINT('Origin',(18.3,70.,5.5));
#71662=CARTESIAN_POINT('Ctrl Pts',(18.3,80.643929117918,2.7559345126152));
#71663=CARTESIAN_POINT('Ctrl Pts',(18.1272,80.643929117918,2.7559345126152));
#71664=CARTESIAN_POINT('Ctrl Pts',(18.3,80.643929117918,2.89126879572868));
#71665=CARTESIAN_POINT('Ctrl Pts',(18.1272,80.643929117918,2.89126879572868));
#71666=CARTESIAN_POINT('Ctrl Pts',(18.3,80.5293315887451,2.97203279137611));
#71667=CARTESIAN_POINT('Ctrl Pts',(18.1272,80.5293315887451,2.97203279137611));
#71668=CARTESIAN_POINT('',(18.3,80.643929117918,2.7559345126152));
#71669=CARTESIAN_POINT('',(18.3,80.5293315887451,2.97203279137611));
#71670=CARTESIAN_POINT('Ctrl Pts',(18.3,80.643929117918,2.7559345126152));
#71671=CARTESIAN_POINT('Ctrl Pts',(18.3,80.643929117918,2.89126879572868));
#71672=CARTESIAN_POINT('Ctrl Pts',(18.3,80.5293315887451,2.97203279137611));
#71673=CARTESIAN_POINT('',(18.18,80.643929117918,2.7559345126152));
#71674=CARTESIAN_POINT('',(18.3,80.643929117918,2.7559345126152));
#71675=CARTESIAN_POINT('',(18.18,80.5293315887451,2.97203279137611));
#71676=CARTESIAN_POINT('Ctrl Pts',(18.18,80.643929117918,2.7559345126152));
#71677=CARTESIAN_POINT('Ctrl Pts',(18.18,80.643929117918,2.89126879572868));
#71678=CARTESIAN_POINT('Ctrl Pts',(18.18,80.5293315887451,2.97203279137611));
#71679=CARTESIAN_POINT('',(18.3,80.5293315887451,2.97203279137611));
#71680=CARTESIAN_POINT('Ctrl Pts',(18.3,80.5140519380569,2.52619377374649));
#71681=CARTESIAN_POINT('Ctrl Pts',(18.1272,80.5140519380569,2.52619377374649));
#71682=CARTESIAN_POINT('Ctrl Pts',(18.3,80.643929117918,2.61841750741005));
#71683=CARTESIAN_POINT('Ctrl Pts',(18.1272,80.643929117918,2.61841750741005));
#71684=CARTESIAN_POINT('Ctrl Pts',(18.3,80.643929117918,2.7559345126152));
#71685=CARTESIAN_POINT('Ctrl Pts',(18.1272,80.643929117918,2.7559345126152));
#71686=CARTESIAN_POINT('',(18.3,80.5140519380569,2.52619377374649));
#71687=CARTESIAN_POINT('Ctrl Pts',(18.3,80.5140519380569,2.52619377374649));
#71688=CARTESIAN_POINT('Ctrl Pts',(18.3,80.643929117918,2.61841750741005));
#71689=CARTESIAN_POINT('Ctrl Pts',(18.3,80.643929117918,2.7559345126152));
#71690=CARTESIAN_POINT('',(18.18,80.5140519380569,2.52619377374649));
#71691=CARTESIAN_POINT('',(18.3,80.5140519380569,2.52619377374649));
#71692=CARTESIAN_POINT('Ctrl Pts',(18.18,80.5140519380569,2.52619377374649));
#71693=CARTESIAN_POINT('Ctrl Pts',(18.18,80.643929117918,2.61841750741005));
#71694=CARTESIAN_POINT('Ctrl Pts',(18.18,80.643929117918,2.7559345126152));
#71695=CARTESIAN_POINT('Ctrl Pts',(18.3,79.9890859663486,2.43397004008293));
#71696=CARTESIAN_POINT('Ctrl Pts',(18.1272,79.9890859663486,2.43397004008293));
#71697=CARTESIAN_POINT('Ctrl Pts',(18.3,80.3841746091843,2.43397004008293));
#71698=CARTESIAN_POINT('Ctrl Pts',(18.1272,80.3841746091843,2.43397004008293));
#71699=CARTESIAN_POINT('Ctrl Pts',(18.3,80.5140519380569,2.52619377374649));
#71700=CARTESIAN_POINT('Ctrl Pts',(18.1272,80.5140519380569,2.52619377374649));
#71701=CARTESIAN_POINT('',(18.3,79.9890859663486,2.43397004008293));
#71702=CARTESIAN_POINT('Ctrl Pts',(18.3,79.9890859663486,2.43397004008293));
#71703=CARTESIAN_POINT('Ctrl Pts',(18.3,80.3841746091843,2.43397004008293));
#71704=CARTESIAN_POINT('Ctrl Pts',(18.3,80.5140519380569,2.52619377374649));
#71705=CARTESIAN_POINT('',(18.18,79.9890859663486,2.43397004008293));
#71706=CARTESIAN_POINT('',(18.3,79.9890859663486,2.43397004008293));
#71707=CARTESIAN_POINT('Ctrl Pts',(18.18,79.9890859663486,2.43397004008293));
#71708=CARTESIAN_POINT('Ctrl Pts',(18.18,80.3841746091843,2.43397004008293));
#71709=CARTESIAN_POINT('Ctrl Pts',(18.18,80.5140519380569,2.52619377374649));
#71710=CARTESIAN_POINT('Ctrl Pts',(18.3,79.4652115046978,2.52619377374649));
#71711=CARTESIAN_POINT('Ctrl Pts',(18.1272,79.4652115046978,2.52619377374649));
#71712=CARTESIAN_POINT('Ctrl Pts',(18.3,79.5961801946163,2.43397004008293));
#71713=CARTESIAN_POINT('Ctrl Pts',(18.1272,79.5961801946163,2.43397004008293));
#71714=CARTESIAN_POINT('Ctrl Pts',(18.3,79.9890859663486,2.43397004008293));
#71715=CARTESIAN_POINT('Ctrl Pts',(18.1272,79.9890859663486,2.43397004008293));
#71716=CARTESIAN_POINT('',(18.3,79.4652115046978,2.52619377374649));
#71717=CARTESIAN_POINT('Ctrl Pts',(18.3,79.4652115046978,2.52619377374649));
#71718=CARTESIAN_POINT('Ctrl Pts',(18.3,79.5961801946163,2.43397004008293));
#71719=CARTESIAN_POINT('Ctrl Pts',(18.3,79.9890859663486,2.43397004008293));
#71720=CARTESIAN_POINT('',(18.18,79.4652115046978,2.52619377374649));
#71721=CARTESIAN_POINT('',(18.3,79.4652115046978,2.52619377374649));
#71722=CARTESIAN_POINT('Ctrl Pts',(18.18,79.4652115046978,2.52619377374649));
#71723=CARTESIAN_POINT('Ctrl Pts',(18.18,79.5961801946163,2.43397004008293));
#71724=CARTESIAN_POINT('Ctrl Pts',(18.18,79.9890859663486,2.43397004008293));
#71725=CARTESIAN_POINT('Ctrl Pts',(18.3,79.3342428147793,2.75375164151192));
#71726=CARTESIAN_POINT('Ctrl Pts',(18.1272,79.3342428147793,2.75375164151192));
#71727=CARTESIAN_POINT('Ctrl Pts',(18.3,79.3342428147793,2.61841750741005));
#71728=CARTESIAN_POINT('Ctrl Pts',(18.1272,79.3342428147793,2.61841750741005));
#71729=CARTESIAN_POINT('Ctrl Pts',(18.3,79.4652115046978,2.52619377374649));
#71730=CARTESIAN_POINT('Ctrl Pts',(18.1272,79.4652115046978,2.52619377374649));
#71731=CARTESIAN_POINT('',(18.3,79.3342428147793,2.75375164151192));
#71732=CARTESIAN_POINT('Ctrl Pts',(18.3,79.3342428147793,2.75375164151192));
#71733=CARTESIAN_POINT('Ctrl Pts',(18.3,79.3342428147793,2.61841750741005));
#71734=CARTESIAN_POINT('Ctrl Pts',(18.3,79.4652115046978,2.52619377374649));
#71735=CARTESIAN_POINT('',(18.18,79.3342428147793,2.75375164151192));
#71736=CARTESIAN_POINT('',(18.3,79.3342428147793,2.75375164151192));
#71737=CARTESIAN_POINT('Ctrl Pts',(18.18,79.3342428147793,2.75375164151192));
#71738=CARTESIAN_POINT('Ctrl Pts',(18.18,79.3342428147793,2.61841750741005));
#71739=CARTESIAN_POINT('Ctrl Pts',(18.18,79.4652115046978,2.52619377374649));
#71740=CARTESIAN_POINT('Ctrl Pts',(18.3,79.4646658241749,2.98130965828896));
#71741=CARTESIAN_POINT('Ctrl Pts',(18.1272,79.4646658241749,2.98130965828896));
#71742=CARTESIAN_POINT('Ctrl Pts',(18.3,79.3342428147793,2.8890859246254));
#71743=CARTESIAN_POINT('Ctrl Pts',(18.1272,79.3342428147793,2.8890859246254));
#71744=CARTESIAN_POINT('Ctrl Pts',(18.3,79.3342428147793,2.75375164151192));
#71745=CARTESIAN_POINT('Ctrl Pts',(18.1272,79.3342428147793,2.75375164151192));
#71746=CARTESIAN_POINT('',(18.3,79.4646658241749,2.98130965828896));
#71747=CARTESIAN_POINT('Ctrl Pts',(18.3,79.4646658241749,2.98130965828896));
#71748=CARTESIAN_POINT('Ctrl Pts',(18.3,79.3342428147793,2.8890859246254));
#71749=CARTESIAN_POINT('Ctrl Pts',(18.3,79.3342428147793,2.75375164151192));
#71750=CARTESIAN_POINT('',(18.18,79.4646658241749,2.98130965828896));
#71751=CARTESIAN_POINT('',(18.3,79.4646658241749,2.98130965828896));
#71752=CARTESIAN_POINT('Ctrl Pts',(18.18,79.4646658241749,2.98130965828896));
#71753=CARTESIAN_POINT('Ctrl Pts',(18.18,79.3342428147793,2.8890859246254));
#71754=CARTESIAN_POINT('Ctrl Pts',(18.18,79.3342428147793,2.75375164151192));
#71755=CARTESIAN_POINT('Ctrl Pts',(18.3,79.9890859663486,3.07353339195251));
#71756=CARTESIAN_POINT('Ctrl Pts',(18.1272,79.9890859663486,3.07353339195251));
#71757=CARTESIAN_POINT('Ctrl Pts',(18.3,79.5950888335705,3.07353339195251));
#71758=CARTESIAN_POINT('Ctrl Pts',(18.1272,79.5950888335705,3.07353339195251));
#71759=CARTESIAN_POINT('Ctrl Pts',(18.3,79.4646658241749,2.98130965828896));
#71760=CARTESIAN_POINT('Ctrl Pts',(18.1272,79.4646658241749,2.98130965828896));
#71761=CARTESIAN_POINT('',(18.3,79.9890859663486,3.07353339195251));
#71762=CARTESIAN_POINT('Ctrl Pts',(18.3,79.9890859663486,3.07353339195251));
#71763=CARTESIAN_POINT('Ctrl Pts',(18.3,79.5950888335705,3.07353339195251));
#71764=CARTESIAN_POINT('Ctrl Pts',(18.3,79.4646658241749,2.98130965828896));
#71765=CARTESIAN_POINT('',(18.18,79.9890859663486,3.07353339195251));
#71766=CARTESIAN_POINT('',(18.3,79.9890859663486,3.07353339195251));
#71767=CARTESIAN_POINT('Ctrl Pts',(18.18,79.9890859663486,3.07353339195251));
#71768=CARTESIAN_POINT('Ctrl Pts',(18.18,79.5950888335705,3.07353339195251));
#71769=CARTESIAN_POINT('Ctrl Pts',(18.18,79.4646658241749,2.98130965828896));
#71770=CARTESIAN_POINT('Ctrl Pts',(18.3,80.5293315887451,2.97203279137611));
#71771=CARTESIAN_POINT('Ctrl Pts',(18.1272,80.5293315887451,2.97203279137611));
#71772=CARTESIAN_POINT('Ctrl Pts',(18.3,80.3830830991268,3.07353339195251));
#71773=CARTESIAN_POINT('Ctrl Pts',(18.1272,80.3830830991268,3.07353339195251));
#71774=CARTESIAN_POINT('Ctrl Pts',(18.3,79.9890859663486,3.07353339195251));
#71775=CARTESIAN_POINT('Ctrl Pts',(18.1272,79.9890859663486,3.07353339195251));
#71776=CARTESIAN_POINT('Ctrl Pts',(18.3,80.5293315887451,2.97203279137611));
#71777=CARTESIAN_POINT('Ctrl Pts',(18.3,80.3830830991268,3.07353339195251));
#71778=CARTESIAN_POINT('Ctrl Pts',(18.3,79.9890859663486,3.07353339195251));
#71779=CARTESIAN_POINT('Ctrl Pts',(18.18,80.5293315887451,2.97203279137611));
#71780=CARTESIAN_POINT('Ctrl Pts',(18.18,80.3830830991268,3.07353339195251));
#71781=CARTESIAN_POINT('Ctrl Pts',(18.18,79.9890859663486,3.07353339195251));
#71782=CARTESIAN_POINT('Ctrl Pts',(18.3,79.1727148234844,2.75375164151192));
#71783=CARTESIAN_POINT('Ctrl Pts',(18.1272,79.1727148234844,2.75375164151192));
#71784=CARTESIAN_POINT('Ctrl Pts',(18.3,79.1727148234844,2.985129570961));
#71785=CARTESIAN_POINT('Ctrl Pts',(18.1272,79.1727148234844,2.985129570961));
#71786=CARTESIAN_POINT('Ctrl Pts',(18.3,79.3386085569858,3.11718962192535));
#71787=CARTESIAN_POINT('Ctrl Pts',(18.1272,79.3386085569858,3.11718962192535));
#71788=CARTESIAN_POINT('',(18.3,79.1727148234844,2.75375164151192));
#71789=CARTESIAN_POINT('',(18.3,79.3386085569858,3.11718962192535));
#71790=CARTESIAN_POINT('Ctrl Pts',(18.3,79.1727148234844,2.75375164151192));
#71791=CARTESIAN_POINT('Ctrl Pts',(18.3,79.1727148234844,2.985129570961));
#71792=CARTESIAN_POINT('Ctrl Pts',(18.3,79.3386085569858,3.11718962192535));
#71793=CARTESIAN_POINT('',(18.18,79.1727148234844,2.75375164151192));
#71794=CARTESIAN_POINT('',(18.3,79.1727148234844,2.75375164151192));
#71795=CARTESIAN_POINT('',(18.18,79.3386085569858,3.11718962192535));
#71796=CARTESIAN_POINT('Ctrl Pts',(18.18,79.1727148234844,2.75375164151192));
#71797=CARTESIAN_POINT('Ctrl Pts',(18.18,79.1727148234844,2.985129570961));
#71798=CARTESIAN_POINT('Ctrl Pts',(18.18,79.3386085569858,3.11718962192535));
#71799=CARTESIAN_POINT('',(18.3,79.3386085569858,3.11718962192535));
#71800=CARTESIAN_POINT('Ctrl Pts',(18.3,79.2671214282513,2.46289229989052));
#71801=CARTESIAN_POINT('Ctrl Pts',(18.1272,79.2671214282513,2.46289229989052));
#71802=CARTESIAN_POINT('Ctrl Pts',(18.3,79.1727148234844,2.57803550958633));
#71803=CARTESIAN_POINT('Ctrl Pts',(18.1272,79.1727148234844,2.57803550958633));
#71804=CARTESIAN_POINT('Ctrl Pts',(18.3,79.1727148234844,2.75375164151192));
#71805=CARTESIAN_POINT('Ctrl Pts',(18.1272,79.1727148234844,2.75375164151192));
#71806=CARTESIAN_POINT('',(18.3,79.2671214282513,2.46289229989052));
#71807=CARTESIAN_POINT('Ctrl Pts',(18.3,79.2671214282513,2.46289229989052));
#71808=CARTESIAN_POINT('Ctrl Pts',(18.3,79.1727148234844,2.57803550958633));
#71809=CARTESIAN_POINT('Ctrl Pts',(18.3,79.1727148234844,2.75375164151192));
#71810=CARTESIAN_POINT('',(18.18,79.2671214282513,2.46289229989052));
#71811=CARTESIAN_POINT('',(18.3,79.2671214282513,2.46289229989052));
#71812=CARTESIAN_POINT('Ctrl Pts',(18.18,79.2671214282513,2.46289229989052));
#71813=CARTESIAN_POINT('Ctrl Pts',(18.18,79.1727148234844,2.57803550958633));
#71814=CARTESIAN_POINT('Ctrl Pts',(18.18,79.1727148234844,2.75375164151192));
#71815=CARTESIAN_POINT('Ctrl Pts',(18.3,79.5345156133175,2.28990457057953));
#71816=CARTESIAN_POINT('Ctrl Pts',(18.1272,79.5345156133175,2.28990457057953));
#71817=CARTESIAN_POINT('Ctrl Pts',(18.3,79.3615280330181,2.34774894118309));
#71818=CARTESIAN_POINT('Ctrl Pts',(18.1272,79.3615280330181,2.34774894118309));
#71819=CARTESIAN_POINT('Ctrl Pts',(18.3,79.2671214282513,2.46289229989052));
#71820=CARTESIAN_POINT('Ctrl Pts',(18.1272,79.2671214282513,2.46289229989052));
#71821=CARTESIAN_POINT('',(18.3,79.5345156133175,2.28990457057953));
#71822=CARTESIAN_POINT('Ctrl Pts',(18.3,79.5345156133175,2.28990457057953));
#71823=CARTESIAN_POINT('Ctrl Pts',(18.3,79.3615280330181,2.34774894118309));
#71824=CARTESIAN_POINT('Ctrl Pts',(18.3,79.2671214282513,2.46289229989052));
#71825=CARTESIAN_POINT('',(18.18,79.5345156133175,2.28990457057953));
#71826=CARTESIAN_POINT('',(18.3,79.5345156133175,2.28990457057953));
#71827=CARTESIAN_POINT('Ctrl Pts',(18.18,79.5345156133175,2.28990457057953));
#71828=CARTESIAN_POINT('Ctrl Pts',(18.18,79.3615280330181,2.34774894118309));
#71829=CARTESIAN_POINT('Ctrl Pts',(18.18,79.2671214282513,2.46289229989052));
#71830=CARTESIAN_POINT('Ctrl Pts',(18.3,79.9890859663486,2.23206005096436));
#71831=CARTESIAN_POINT('Ctrl Pts',(18.1272,79.9890859663486,2.23206005096436));
#71832=CARTESIAN_POINT('Ctrl Pts',(18.3,79.7075034916401,2.23206005096436));
#71833=CARTESIAN_POINT('Ctrl Pts',(18.1272,79.7075034916401,2.23206005096436));
#71834=CARTESIAN_POINT('Ctrl Pts',(18.3,79.5345156133175,2.28990457057953));
#71835=CARTESIAN_POINT('Ctrl Pts',(18.1272,79.5345156133175,2.28990457057953));
#71836=CARTESIAN_POINT('',(18.3,79.9890859663486,2.23206005096436));
#71837=CARTESIAN_POINT('Ctrl Pts',(18.3,79.9890859663486,2.23206005096436));
#71838=CARTESIAN_POINT('Ctrl Pts',(18.3,79.7075034916401,2.23206005096436));
#71839=CARTESIAN_POINT('Ctrl Pts',(18.3,79.5345156133175,2.28990457057953));
#71840=CARTESIAN_POINT('',(18.18,79.9890859663486,2.23206005096436));
#71841=CARTESIAN_POINT('',(18.3,79.9890859663486,2.23206005096436));
#71842=CARTESIAN_POINT('Ctrl Pts',(18.18,79.9890859663486,2.23206005096436));
#71843=CARTESIAN_POINT('Ctrl Pts',(18.18,79.7075034916401,2.23206005096436));
#71844=CARTESIAN_POINT('Ctrl Pts',(18.18,79.5345156133175,2.28990457057953));
#71845=CARTESIAN_POINT('Ctrl Pts',(18.3,80.3672577679157,2.26807645559311));
#71846=CARTESIAN_POINT('Ctrl Pts',(18.1272,80.3672577679157,2.26807645559311));
#71847=CARTESIAN_POINT('Ctrl Pts',(18.3,80.2270122110844,2.23206005096436));
#71848=CARTESIAN_POINT('Ctrl Pts',(18.1272,80.2270122110844,2.23206005096436));
#71849=CARTESIAN_POINT('Ctrl Pts',(18.3,79.9890859663486,2.23206005096436));
#71850=CARTESIAN_POINT('Ctrl Pts',(18.1272,79.9890859663486,2.23206005096436));
#71851=CARTESIAN_POINT('',(18.3,80.3672577679157,2.26807645559311));
#71852=CARTESIAN_POINT('Ctrl Pts',(18.3,80.3672577679157,2.26807645559311));
#71853=CARTESIAN_POINT('Ctrl Pts',(18.3,80.2270122110844,2.23206005096436));
#71854=CARTESIAN_POINT('Ctrl Pts',(18.3,79.9890859663486,2.23206005096436));
#71855=CARTESIAN_POINT('',(18.18,80.3672577679157,2.26807645559311));
#71856=CARTESIAN_POINT('',(18.3,80.3672577679157,2.26807645559311));
#71857=CARTESIAN_POINT('Ctrl Pts',(18.18,80.3672577679157,2.26807645559311));
#71858=CARTESIAN_POINT('Ctrl Pts',(18.18,80.2270122110844,2.23206005096436));
#71859=CARTESIAN_POINT('Ctrl Pts',(18.18,79.9890859663486,2.23206005096436));
#71860=CARTESIAN_POINT('Ctrl Pts',(18.3,80.605184161663,2.36739433407783));
#71861=CARTESIAN_POINT('Ctrl Pts',(18.1272,80.605184161663,2.36739433407783));
#71862=CARTESIAN_POINT('Ctrl Pts',(18.3,80.5075034737587,2.30409256219864));
#71863=CARTESIAN_POINT('Ctrl Pts',(18.1272,80.5075034737587,2.30409256219864));
#71864=CARTESIAN_POINT('Ctrl Pts',(18.3,80.3672577679157,2.26807645559311));
#71865=CARTESIAN_POINT('Ctrl Pts',(18.1272,80.3672577679157,2.26807645559311));
#71866=CARTESIAN_POINT('',(18.3,80.605184161663,2.36739433407783));
#71867=CARTESIAN_POINT('Ctrl Pts',(18.3,80.605184161663,2.36739433407783));
#71868=CARTESIAN_POINT('Ctrl Pts',(18.3,80.5075034737587,2.30409256219864));
#71869=CARTESIAN_POINT('Ctrl Pts',(18.3,80.3672577679157,2.26807645559311));
#71870=CARTESIAN_POINT('',(18.18,80.605184161663,2.36739433407783));
#71871=CARTESIAN_POINT('',(18.3,80.605184161663,2.36739433407783));
#71872=CARTESIAN_POINT('Ctrl Pts',(18.18,80.605184161663,2.36739433407783));
#71873=CARTESIAN_POINT('Ctrl Pts',(18.18,80.5075034737587,2.30409256219864));
#71874=CARTESIAN_POINT('Ctrl Pts',(18.18,80.3672577679157,2.26807645559311));
#71875=CARTESIAN_POINT('Ctrl Pts',(18.3,80.7547067344189,2.52783096432686));
#71876=CARTESIAN_POINT('Ctrl Pts',(18.1272,80.7547067344189,2.52783096432686));
#71877=CARTESIAN_POINT('Ctrl Pts',(18.3,80.702864998579,2.43069580793381));
#71878=CARTESIAN_POINT('Ctrl Pts',(18.1272,80.702864998579,2.43069580793381));
#71879=CARTESIAN_POINT('Ctrl Pts',(18.3,80.605184161663,2.36739433407783));
#71880=CARTESIAN_POINT('Ctrl Pts',(18.1272,80.605184161663,2.36739433407783));
#71881=CARTESIAN_POINT('',(18.3,80.7547067344189,2.52783096432686));
#71882=CARTESIAN_POINT('Ctrl Pts',(18.3,80.7547067344189,2.52783096432686));
#71883=CARTESIAN_POINT('Ctrl Pts',(18.3,80.702864998579,2.43069580793381));
#71884=CARTESIAN_POINT('Ctrl Pts',(18.3,80.605184161663,2.36739433407783));
#71885=CARTESIAN_POINT('',(18.18,80.7547067344189,2.52783096432686));
#71886=CARTESIAN_POINT('',(18.3,80.7547067344189,2.52783096432686));
#71887=CARTESIAN_POINT('Ctrl Pts',(18.18,80.7547067344189,2.52783096432686));
#71888=CARTESIAN_POINT('Ctrl Pts',(18.18,80.702864998579,2.43069580793381));
#71889=CARTESIAN_POINT('Ctrl Pts',(18.18,80.605184161663,2.36739433407783));
#71890=CARTESIAN_POINT('Ctrl Pts',(18.3,80.8065484702587,2.75375164151192));
#71891=CARTESIAN_POINT('Ctrl Pts',(18.1272,80.8065484702587,2.75375164151192));
#71892=CARTESIAN_POINT('Ctrl Pts',(18.3,80.8065484702587,2.6249659717083));
#71893=CARTESIAN_POINT('Ctrl Pts',(18.1272,80.8065484702587,2.6249659717083));
#71894=CARTESIAN_POINT('Ctrl Pts',(18.3,80.7547067344189,2.52783096432686));
#71895=CARTESIAN_POINT('Ctrl Pts',(18.1272,80.7547067344189,2.52783096432686));
#71896=CARTESIAN_POINT('',(18.3,80.8065484702587,2.75375164151192));
#71897=CARTESIAN_POINT('Ctrl Pts',(18.3,80.8065484702587,2.75375164151192));
#71898=CARTESIAN_POINT('Ctrl Pts',(18.3,80.8065484702587,2.6249659717083));
#71899=CARTESIAN_POINT('Ctrl Pts',(18.3,80.7547067344189,2.52783096432686));
#71900=CARTESIAN_POINT('',(18.18,80.8065484702587,2.75375164151192));
#71901=CARTESIAN_POINT('',(18.3,80.8065484702587,2.75375164151192));
#71902=CARTESIAN_POINT('Ctrl Pts',(18.18,80.8065484702587,2.75375164151192));
#71903=CARTESIAN_POINT('Ctrl Pts',(18.18,80.8065484702587,2.6249659717083));
#71904=CARTESIAN_POINT('Ctrl Pts',(18.18,80.7547067344189,2.52783096432686));
#71905=CARTESIAN_POINT('Ctrl Pts',(18.3,80.7126876950264,3.04351977109909));
#71906=CARTESIAN_POINT('Ctrl Pts',(18.1272,80.7126876950264,3.04351977109909));
#71907=CARTESIAN_POINT('Ctrl Pts',(18.3,80.8065484702587,2.92837656140327));
#71908=CARTESIAN_POINT('Ctrl Pts',(18.1272,80.8065484702587,2.92837656140327));
#71909=CARTESIAN_POINT('Ctrl Pts',(18.3,80.8065484702587,2.75375164151192));
#71910=CARTESIAN_POINT('Ctrl Pts',(18.1272,80.8065484702587,2.75375164151192));
#71911=CARTESIAN_POINT('',(18.3,80.7126876950264,3.04351977109909));
#71912=CARTESIAN_POINT('Ctrl Pts',(18.3,80.7126876950264,3.04351977109909));
#71913=CARTESIAN_POINT('Ctrl Pts',(18.3,80.8065484702587,2.92837656140327));
#71914=CARTESIAN_POINT('Ctrl Pts',(18.3,80.8065484702587,2.75375164151192));
#71915=CARTESIAN_POINT('',(18.18,80.7126876950264,3.04351977109909));
#71916=CARTESIAN_POINT('',(18.3,80.7126876950264,3.04351977109909));
#71917=CARTESIAN_POINT('Ctrl Pts',(18.18,80.7126876950264,3.04351977109909));
#71918=CARTESIAN_POINT('Ctrl Pts',(18.18,80.8065484702587,2.92837656140327));
#71919=CARTESIAN_POINT('Ctrl Pts',(18.18,80.8065484702587,2.75375164151192));
#71920=CARTESIAN_POINT('Ctrl Pts',(18.3,80.4458390414715,3.217053180933));
#71921=CARTESIAN_POINT('Ctrl Pts',(18.1272,80.4458390414715,3.217053180933));
#71922=CARTESIAN_POINT('Ctrl Pts',(18.3,80.6188267707825,3.15866298079491));
#71923=CARTESIAN_POINT('Ctrl Pts',(18.1272,80.6188267707825,3.15866298079491));
#71924=CARTESIAN_POINT('Ctrl Pts',(18.3,80.7126876950264,3.04351977109909));
#71925=CARTESIAN_POINT('Ctrl Pts',(18.1272,80.7126876950264,3.04351977109909));
#71926=CARTESIAN_POINT('',(18.3,80.4458390414715,3.217053180933));
#71927=CARTESIAN_POINT('Ctrl Pts',(18.3,80.4458390414715,3.217053180933));
#71928=CARTESIAN_POINT('Ctrl Pts',(18.3,80.6188267707825,3.15866298079491));
#71929=CARTESIAN_POINT('Ctrl Pts',(18.3,80.7126876950264,3.04351977109909));
#71930=CARTESIAN_POINT('',(18.18,80.4458390414715,3.217053180933));
#71931=CARTESIAN_POINT('',(18.3,80.4458390414715,3.217053180933));
#71932=CARTESIAN_POINT('Ctrl Pts',(18.18,80.4458390414715,3.217053180933));
#71933=CARTESIAN_POINT('Ctrl Pts',(18.18,80.6188267707825,3.15866298079491));
#71934=CARTESIAN_POINT('Ctrl Pts',(18.18,80.7126876950264,3.04351977109909));
#71935=CARTESIAN_POINT('Ctrl Pts',(18.3,79.9890859663486,3.27544338107109));
#71936=CARTESIAN_POINT('Ctrl Pts',(18.1272,79.9890859663486,3.27544338107109));
#71937=CARTESIAN_POINT('Ctrl Pts',(18.3,80.2728513121605,3.27544338107109));
#71938=CARTESIAN_POINT('Ctrl Pts',(18.1272,80.2728513121605,3.27544338107109));
#71939=CARTESIAN_POINT('Ctrl Pts',(18.3,80.4458390414715,3.217053180933));
#71940=CARTESIAN_POINT('Ctrl Pts',(18.1272,80.4458390414715,3.217053180933));
#71941=CARTESIAN_POINT('',(18.3,79.9890859663486,3.27544338107109));
#71942=CARTESIAN_POINT('Ctrl Pts',(18.3,79.9890859663486,3.27544338107109));
#71943=CARTESIAN_POINT('Ctrl Pts',(18.3,80.2728513121605,3.27544338107109));
#71944=CARTESIAN_POINT('Ctrl Pts',(18.3,80.4458390414715,3.217053180933));
#71945=CARTESIAN_POINT('',(18.18,79.9890859663486,3.27544338107109));
#71946=CARTESIAN_POINT('',(18.3,79.9890859663486,3.27544338107109));
#71947=CARTESIAN_POINT('Ctrl Pts',(18.18,79.9890859663486,3.27544338107109));
#71948=CARTESIAN_POINT('Ctrl Pts',(18.18,80.2728513121605,3.27544338107109));
#71949=CARTESIAN_POINT('Ctrl Pts',(18.18,80.4458390414715,3.217053180933));
#71950=CARTESIAN_POINT('Ctrl Pts',(18.3,79.3386085569858,3.11718962192535));
#71951=CARTESIAN_POINT('Ctrl Pts',(18.1272,79.3386085569858,3.11718962192535));
#71952=CARTESIAN_POINT('Ctrl Pts',(18.3,79.5383356750011,3.27544338107109));
#71953=CARTESIAN_POINT('Ctrl Pts',(18.1272,79.5383356750011,3.27544338107109));
#71954=CARTESIAN_POINT('Ctrl Pts',(18.3,79.9890859663486,3.27544338107109));
#71955=CARTESIAN_POINT('Ctrl Pts',(18.1272,79.9890859663486,3.27544338107109));
#71956=CARTESIAN_POINT('Ctrl Pts',(18.3,79.3386085569858,3.11718962192535));
#71957=CARTESIAN_POINT('Ctrl Pts',(18.3,79.5383356750011,3.27544338107109));
#71958=CARTESIAN_POINT('Ctrl Pts',(18.3,79.9890859663486,3.27544338107109));
#71959=CARTESIAN_POINT('Ctrl Pts',(18.18,79.3386085569858,3.11718962192535));
#71960=CARTESIAN_POINT('Ctrl Pts',(18.18,79.5383356750011,3.27544338107109));
#71961=CARTESIAN_POINT('Ctrl Pts',(18.18,79.9890859663486,3.27544338107109));
#71962=CARTESIAN_POINT('Origin',(18.18,79.9896316468716,3.29999997317791));
#71963=CARTESIAN_POINT('Origin',(18.3,80.8065484702587,3.90518411099911));
#71964=CARTESIAN_POINT('',(18.3,80.8065484702587,3.90518411099911));
#71965=CARTESIAN_POINT('',(18.3,80.8065484702587,3.77858108878136));
#71966=CARTESIAN_POINT('',(18.3,80.8065484702587,4.70259205549955));
#71967=CARTESIAN_POINT('',(18.18,80.8065484702587,3.90518411099911));
#71968=CARTESIAN_POINT('',(18.3,80.8065484702587,3.90518411099911));
#71969=CARTESIAN_POINT('',(18.18,80.8065484702587,3.77858108878136));
#71970=CARTESIAN_POINT('',(18.18,80.8065484702587,3.90518411099911));
#71971=CARTESIAN_POINT('',(18.3,80.8065484702587,3.77858108878136));
#71972=CARTESIAN_POINT('Ctrl Pts',(18.3,80.5926330626011,4.07980895638466));
#71973=CARTESIAN_POINT('Ctrl Pts',(18.1272,80.5926330626011,4.07980895638466));
#71974=CARTESIAN_POINT('Ctrl Pts',(18.3,80.702864998579,3.95648016631603));
#71975=CARTESIAN_POINT('Ctrl Pts',(18.1272,80.702864998579,3.95648016631603));
#71976=CARTESIAN_POINT('Ctrl Pts',(18.3,80.8065484702587,3.90518411099911));
#71977=CARTESIAN_POINT('Ctrl Pts',(18.1272,80.8065484702587,3.90518411099911));
#71978=CARTESIAN_POINT('',(18.3,80.5926330626011,4.07980895638466));
#71979=CARTESIAN_POINT('Ctrl Pts',(18.3,80.5926330626011,4.07980895638466));
#71980=CARTESIAN_POINT('Ctrl Pts',(18.3,80.702864998579,3.95648016631603));
#71981=CARTESIAN_POINT('Ctrl Pts',(18.3,80.8065484702587,3.90518411099911));
#71982=CARTESIAN_POINT('',(18.18,80.5926330626011,4.07980895638466));
#71983=CARTESIAN_POINT('',(18.3,80.5926330626011,4.07980895638466));
#71984=CARTESIAN_POINT('Ctrl Pts',(18.18,80.5926330626011,4.07980895638466));
#71985=CARTESIAN_POINT('Ctrl Pts',(18.18,80.702864998579,3.95648016631603));
#71986=CARTESIAN_POINT('Ctrl Pts',(18.18,80.8065484702587,3.90518411099911));
#71987=CARTESIAN_POINT('Ctrl Pts',(18.3,80.4049113631248,4.36793989539146));
#71988=CARTESIAN_POINT('Ctrl Pts',(18.1272,80.4049113631248,4.36793989539146));
#71989=CARTESIAN_POINT('Ctrl Pts',(18.3,80.4824011266231,4.20313774645328));
#71990=CARTESIAN_POINT('Ctrl Pts',(18.1272,80.4824011266231,4.20313774645328));
#71991=CARTESIAN_POINT('Ctrl Pts',(18.3,80.5926330626011,4.07980895638466));
#71992=CARTESIAN_POINT('Ctrl Pts',(18.1272,80.5926330626011,4.07980895638466));
#71993=CARTESIAN_POINT('',(18.3,80.4049113631248,4.36793989539146));
#71994=CARTESIAN_POINT('Ctrl Pts',(18.3,80.4049113631248,4.36793989539146));
#71995=CARTESIAN_POINT('Ctrl Pts',(18.3,80.4824011266231,4.20313774645328));
#71996=CARTESIAN_POINT('Ctrl Pts',(18.3,80.5926330626011,4.07980895638466));
#71997=CARTESIAN_POINT('',(18.18,80.4049113631248,4.36793989539146));
#71998=CARTESIAN_POINT('',(18.3,80.4049113631248,4.36793989539146));
#71999=CARTESIAN_POINT('Ctrl Pts',(18.18,80.4049113631248,4.36793989539146));
#72000=CARTESIAN_POINT('Ctrl Pts',(18.18,80.4824011266231,4.20313774645328));
#72001=CARTESIAN_POINT('Ctrl Pts',(18.18,80.5926330626011,4.07980895638466));
#72002=CARTESIAN_POINT('Origin',(18.3,80.2150069415569,4.36793989539146));
#72003=CARTESIAN_POINT('',(18.3,80.2150069415569,4.36793989539146));
#72004=CARTESIAN_POINT('',(18.3,75.1075034707785,4.36793989539146));
#72005=CARTESIAN_POINT('',(18.18,80.2150069415569,4.36793989539146));
#72006=CARTESIAN_POINT('',(18.3,80.2150069415569,4.36793989539146));
#72007=CARTESIAN_POINT('',(18.18,80.2150069415569,4.36793989539146));
#72008=CARTESIAN_POINT('Ctrl Pts',(18.3,80.3165075421333,4.16111863255501));
#72009=CARTESIAN_POINT('Ctrl Pts',(18.1272,80.3165075421333,4.16111863255501));
#72010=CARTESIAN_POINT('Ctrl Pts',(18.3,80.2488404750824,4.27626184225082));
#72011=CARTESIAN_POINT('Ctrl Pts',(18.1272,80.2488404750824,4.27626184225082));
#72012=CARTESIAN_POINT('Ctrl Pts',(18.3,80.2150069415569,4.36793989539146));
#72013=CARTESIAN_POINT('Ctrl Pts',(18.1272,80.2150069415569,4.36793989539146));
#72014=CARTESIAN_POINT('',(18.3,80.3165075421333,4.16111863255501));
#72015=CARTESIAN_POINT('Ctrl Pts',(18.3,80.3165075421333,4.16111863255501));
#72016=CARTESIAN_POINT('Ctrl Pts',(18.3,80.2488404750824,4.27626184225082));
#72017=CARTESIAN_POINT('Ctrl Pts',(18.3,80.2150069415569,4.36793989539146));
#72018=CARTESIAN_POINT('',(18.18,80.3165075421333,4.16111863255501));
#72019=CARTESIAN_POINT('',(18.3,80.3165075421333,4.16111863255501));
#72020=CARTESIAN_POINT('Ctrl Pts',(18.18,80.3165075421333,4.16111863255501));
#72021=CARTESIAN_POINT('Ctrl Pts',(18.18,80.2488404750824,4.27626184225082));
#72022=CARTESIAN_POINT('Ctrl Pts',(18.18,80.2150069415569,4.36793989539146));
#72023=CARTESIAN_POINT('Ctrl Pts',(18.3,80.4518418252468,3.97503404915333));
#72024=CARTESIAN_POINT('Ctrl Pts',(18.1272,80.4518418252468,3.97503404915333));
#72025=CARTESIAN_POINT('Ctrl Pts',(18.3,80.3841747581959,4.04597542285919));
#72026=CARTESIAN_POINT('Ctrl Pts',(18.1272,80.3841747581959,4.04597542285919));
#72027=CARTESIAN_POINT('Ctrl Pts',(18.3,80.3165075421333,4.16111863255501));
#72028=CARTESIAN_POINT('Ctrl Pts',(18.1272,80.3165075421333,4.16111863255501));
#72029=CARTESIAN_POINT('',(18.3,80.4518418252468,3.97503404915333));
#72030=CARTESIAN_POINT('Ctrl Pts',(18.3,80.4518418252468,3.97503404915333));
#72031=CARTESIAN_POINT('Ctrl Pts',(18.3,80.3841747581959,4.04597542285919));
#72032=CARTESIAN_POINT('Ctrl Pts',(18.3,80.3165075421333,4.16111863255501));
#72033=CARTESIAN_POINT('',(18.18,80.4518418252468,3.97503404915333));
#72034=CARTESIAN_POINT('',(18.3,80.4518418252468,3.97503404915333));
#72035=CARTESIAN_POINT('Ctrl Pts',(18.18,80.4518418252468,3.97503404915333));
#72036=CARTESIAN_POINT('Ctrl Pts',(18.18,80.3841747581959,4.04597542285919));
#72037=CARTESIAN_POINT('Ctrl Pts',(18.18,80.3165075421333,4.16111863255501));
#72038=CARTESIAN_POINT('Origin',(18.3,79.2000000417232,3.97503404915333));
#72039=CARTESIAN_POINT('',(18.3,79.2000000417232,3.97503404915333));
#72040=CARTESIAN_POINT('',(18.3,74.6000000208616,3.97503404915333));
#72041=CARTESIAN_POINT('',(18.18,79.2000000417232,3.97503404915333));
#72042=CARTESIAN_POINT('',(18.3,79.2000000417232,3.97503404915333));
#72043=CARTESIAN_POINT('',(18.18,79.2000000417232,3.97503404915333));
#72044=CARTESIAN_POINT('Origin',(18.3,79.2000000417232,3.77858108878136));
#72045=CARTESIAN_POINT('',(18.3,79.2000000417232,3.77858108878136));
#72046=CARTESIAN_POINT('',(18.3,79.2000000417232,4.63929054439068));
#72047=CARTESIAN_POINT('',(18.18,79.2000000417232,3.77858108878136));
#72048=CARTESIAN_POINT('',(18.3,79.2000000417232,3.77858108878136));
#72049=CARTESIAN_POINT('',(18.18,79.2000000417232,3.77858108878136));
#72050=CARTESIAN_POINT('Origin',(18.3,80.8065484702587,3.77858108878136));
#72051=CARTESIAN_POINT('',(18.3,75.4032742351294,3.77858108878136));
#72052=CARTESIAN_POINT('',(18.18,80.8065484702587,3.77858108878136));
#72053=CARTESIAN_POINT('Origin',(18.18,79.9896316468716,3.29999997317791));
#72054=CARTESIAN_POINT('Origin',(18.3,70.,5.5));
#72055=CARTESIAN_POINT('Ctrl Pts',(18.3,70.6439290940762,3.30218293741345));
#72056=CARTESIAN_POINT('Ctrl Pts',(18.1272,70.6439290940762,3.30218293741345));
#72057=CARTESIAN_POINT('Ctrl Pts',(18.3,70.6439290940762,3.43751707151532));
#72058=CARTESIAN_POINT('Ctrl Pts',(18.1272,70.6439290940762,3.43751707151532));
#72059=CARTESIAN_POINT('Ctrl Pts',(18.3,70.5293315649033,3.51828106716275));
#72060=CARTESIAN_POINT('Ctrl Pts',(18.1272,70.5293315649033,3.51828106716275));
#72061=CARTESIAN_POINT('',(18.3,70.6439290940762,3.30218293741345));
#72062=CARTESIAN_POINT('',(18.3,70.5293315649033,3.51828106716275));
#72063=CARTESIAN_POINT('Ctrl Pts',(18.3,70.6439290940762,3.30218293741345));
#72064=CARTESIAN_POINT('Ctrl Pts',(18.3,70.6439290940762,3.43751707151532));
#72065=CARTESIAN_POINT('Ctrl Pts',(18.3,70.5293315649033,3.51828106716275));
#72066=CARTESIAN_POINT('',(18.18,70.6439290940762,3.30218293741345));
#72067=CARTESIAN_POINT('',(18.3,70.6439290940762,3.30218293741345));
#72068=CARTESIAN_POINT('',(18.18,70.5293315649033,3.51828106716275));
#72069=CARTESIAN_POINT('Ctrl Pts',(18.18,70.6439290940762,3.30218293741345));
#72070=CARTESIAN_POINT('Ctrl Pts',(18.18,70.6439290940762,3.43751707151532));
#72071=CARTESIAN_POINT('Ctrl Pts',(18.18,70.5293315649033,3.51828106716275));
#72072=CARTESIAN_POINT('',(18.3,70.5293315649033,3.51828106716275));
#72073=CARTESIAN_POINT('Ctrl Pts',(18.3,70.5140519142151,3.07244219854474));
#72074=CARTESIAN_POINT('Ctrl Pts',(18.1272,70.5140519142151,3.07244219854474));
#72075=CARTESIAN_POINT('Ctrl Pts',(18.3,70.6439290940762,3.16466578319669));
#72076=CARTESIAN_POINT('Ctrl Pts',(18.1272,70.6439290940762,3.16466578319669));
#72077=CARTESIAN_POINT('Ctrl Pts',(18.3,70.6439290940762,3.30218293741345));
#72078=CARTESIAN_POINT('Ctrl Pts',(18.1272,70.6439290940762,3.30218293741345));
#72079=CARTESIAN_POINT('',(18.3,70.5140519142151,3.07244219854474));
#72080=CARTESIAN_POINT('Ctrl Pts',(18.3,70.5140519142151,3.07244219854474));
#72081=CARTESIAN_POINT('Ctrl Pts',(18.3,70.6439290940762,3.16466578319669));
#72082=CARTESIAN_POINT('Ctrl Pts',(18.3,70.6439290940762,3.30218293741345));
#72083=CARTESIAN_POINT('',(18.18,70.5140519142151,3.07244219854474));
#72084=CARTESIAN_POINT('',(18.3,70.5140519142151,3.07244219854474));
#72085=CARTESIAN_POINT('Ctrl Pts',(18.18,70.5140519142151,3.07244219854474));
#72086=CARTESIAN_POINT('Ctrl Pts',(18.18,70.6439290940762,3.16466578319669));
#72087=CARTESIAN_POINT('Ctrl Pts',(18.18,70.6439290940762,3.30218293741345));
#72088=CARTESIAN_POINT('Ctrl Pts',(18.3,69.9890859425068,2.98021831586957));
#72089=CARTESIAN_POINT('Ctrl Pts',(18.1272,69.9890859425068,2.98021831586957));
#72090=CARTESIAN_POINT('Ctrl Pts',(18.3,70.3841745853424,2.98021831586957));
#72091=CARTESIAN_POINT('Ctrl Pts',(18.1272,70.3841745853424,2.98021831586957));
#72092=CARTESIAN_POINT('Ctrl Pts',(18.3,70.5140519142151,3.07244219854474));
#72093=CARTESIAN_POINT('Ctrl Pts',(18.1272,70.5140519142151,3.07244219854474));
#72094=CARTESIAN_POINT('',(18.3,69.9890859425068,2.98021831586957));
#72095=CARTESIAN_POINT('Ctrl Pts',(18.3,69.9890859425068,2.98021831586957));
#72096=CARTESIAN_POINT('Ctrl Pts',(18.3,70.3841745853424,2.98021831586957));
#72097=CARTESIAN_POINT('Ctrl Pts',(18.3,70.5140519142151,3.07244219854474));
#72098=CARTESIAN_POINT('',(18.18,69.9890859425068,2.98021831586957));
#72099=CARTESIAN_POINT('',(18.3,69.9890859425068,2.98021831586957));
#72100=CARTESIAN_POINT('Ctrl Pts',(18.18,69.9890859425068,2.98021831586957));
#72101=CARTESIAN_POINT('Ctrl Pts',(18.18,70.3841745853424,2.98021831586957));
#72102=CARTESIAN_POINT('Ctrl Pts',(18.18,70.5140519142151,3.07244219854474));
#72103=CARTESIAN_POINT('Ctrl Pts',(18.3,69.4652114808559,3.07244219854474));
#72104=CARTESIAN_POINT('Ctrl Pts',(18.1272,69.4652114808559,3.07244219854474));
#72105=CARTESIAN_POINT('Ctrl Pts',(18.3,69.5961800217628,2.98021831586957));
#72106=CARTESIAN_POINT('Ctrl Pts',(18.1272,69.5961800217628,2.98021831586957));
#72107=CARTESIAN_POINT('Ctrl Pts',(18.3,69.9890859425068,2.98021831586957));
#72108=CARTESIAN_POINT('Ctrl Pts',(18.1272,69.9890859425068,2.98021831586957));
#72109=CARTESIAN_POINT('',(18.3,69.4652114808559,3.07244219854474));
#72110=CARTESIAN_POINT('Ctrl Pts',(18.3,69.4652114808559,3.07244219854474));
#72111=CARTESIAN_POINT('Ctrl Pts',(18.3,69.5961800217628,2.98021831586957));
#72112=CARTESIAN_POINT('Ctrl Pts',(18.3,69.9890859425068,2.98021831586957));
#72113=CARTESIAN_POINT('',(18.18,69.4652114808559,3.07244219854474));
#72114=CARTESIAN_POINT('',(18.3,69.4652114808559,3.07244219854474));
#72115=CARTESIAN_POINT('Ctrl Pts',(18.18,69.4652114808559,3.07244219854474));
#72116=CARTESIAN_POINT('Ctrl Pts',(18.18,69.5961800217628,2.98021831586957));
#72117=CARTESIAN_POINT('Ctrl Pts',(18.18,69.9890859425068,2.98021831586957));
#72118=CARTESIAN_POINT('Ctrl Pts',(18.3,69.3342427909374,3.30000006631017));
#72119=CARTESIAN_POINT('Ctrl Pts',(18.1272,69.3342427909374,3.30000006631017));
#72120=CARTESIAN_POINT('Ctrl Pts',(18.3,69.3342427909374,3.16466578319669));
#72121=CARTESIAN_POINT('Ctrl Pts',(18.1272,69.3342427909374,3.16466578319669));
#72122=CARTESIAN_POINT('Ctrl Pts',(18.3,69.4652114808559,3.07244219854474));
#72123=CARTESIAN_POINT('Ctrl Pts',(18.1272,69.4652114808559,3.07244219854474));
#72124=CARTESIAN_POINT('',(18.3,69.3342427909374,3.30000006631017));
#72125=CARTESIAN_POINT('Ctrl Pts',(18.3,69.3342427909374,3.30000006631017));
#72126=CARTESIAN_POINT('Ctrl Pts',(18.3,69.3342427909374,3.16466578319669));
#72127=CARTESIAN_POINT('Ctrl Pts',(18.3,69.4652114808559,3.07244219854474));
#72128=CARTESIAN_POINT('',(18.18,69.3342427909374,3.30000006631017));
#72129=CARTESIAN_POINT('',(18.3,69.3342427909374,3.30000006631017));
#72130=CARTESIAN_POINT('Ctrl Pts',(18.18,69.3342427909374,3.30000006631017));
#72131=CARTESIAN_POINT('Ctrl Pts',(18.18,69.3342427909374,3.16466578319669));
#72132=CARTESIAN_POINT('Ctrl Pts',(18.18,69.4652114808559,3.07244219854474));
#72133=CARTESIAN_POINT('Ctrl Pts',(18.3,69.464665800333,3.5275580085814));
#72134=CARTESIAN_POINT('Ctrl Pts',(18.1272,69.464665800333,3.5275580085814));
#72135=CARTESIAN_POINT('Ctrl Pts',(18.3,69.3342427909374,3.43533434942365));
#72136=CARTESIAN_POINT('Ctrl Pts',(18.1272,69.3342427909374,3.43533434942365));
#72137=CARTESIAN_POINT('Ctrl Pts',(18.3,69.3342427909374,3.30000006631017));
#72138=CARTESIAN_POINT('Ctrl Pts',(18.1272,69.3342427909374,3.30000006631017));
#72139=CARTESIAN_POINT('',(18.3,69.464665800333,3.5275580085814));
#72140=CARTESIAN_POINT('Ctrl Pts',(18.3,69.464665800333,3.5275580085814));
#72141=CARTESIAN_POINT('Ctrl Pts',(18.3,69.3342427909374,3.43533434942365));
#72142=CARTESIAN_POINT('Ctrl Pts',(18.3,69.3342427909374,3.30000006631017));
#72143=CARTESIAN_POINT('',(18.18,69.464665800333,3.5275580085814));
#72144=CARTESIAN_POINT('',(18.3,69.464665800333,3.5275580085814));
#72145=CARTESIAN_POINT('Ctrl Pts',(18.18,69.464665800333,3.5275580085814));
#72146=CARTESIAN_POINT('Ctrl Pts',(18.18,69.3342427909374,3.43533434942365));
#72147=CARTESIAN_POINT('Ctrl Pts',(18.18,69.3342427909374,3.30000006631017));
#72148=CARTESIAN_POINT('Ctrl Pts',(18.3,69.9890859425068,3.61978174224496));
#72149=CARTESIAN_POINT('Ctrl Pts',(18.1272,69.9890859425068,3.61978174224496));
#72150=CARTESIAN_POINT('Ctrl Pts',(18.3,69.595088660717,3.61978174224496));
#72151=CARTESIAN_POINT('Ctrl Pts',(18.1272,69.595088660717,3.61978174224496));
#72152=CARTESIAN_POINT('Ctrl Pts',(18.3,69.464665800333,3.5275580085814));
#72153=CARTESIAN_POINT('Ctrl Pts',(18.1272,69.464665800333,3.5275580085814));
#72154=CARTESIAN_POINT('',(18.3,69.9890859425068,3.61978174224496));
#72155=CARTESIAN_POINT('Ctrl Pts',(18.3,69.9890859425068,3.61978174224496));
#72156=CARTESIAN_POINT('Ctrl Pts',(18.3,69.595088660717,3.61978174224496));
#72157=CARTESIAN_POINT('Ctrl Pts',(18.3,69.464665800333,3.5275580085814));
#72158=CARTESIAN_POINT('',(18.18,69.9890859425068,3.61978174224496));
#72159=CARTESIAN_POINT('',(18.3,69.9890859425068,3.61978174224496));
#72160=CARTESIAN_POINT('Ctrl Pts',(18.18,69.9890859425068,3.61978174224496));
#72161=CARTESIAN_POINT('Ctrl Pts',(18.18,69.595088660717,3.61978174224496));
#72162=CARTESIAN_POINT('Ctrl Pts',(18.18,69.464665800333,3.5275580085814));
#72163=CARTESIAN_POINT('Ctrl Pts',(18.3,70.5293315649033,3.51828106716275));
#72164=CARTESIAN_POINT('Ctrl Pts',(18.1272,70.5293315649033,3.51828106716275));
#72165=CARTESIAN_POINT('Ctrl Pts',(18.3,70.383083075285,3.61978174224496));
#72166=CARTESIAN_POINT('Ctrl Pts',(18.1272,70.383083075285,3.61978174224496));
#72167=CARTESIAN_POINT('Ctrl Pts',(18.3,69.9890859425068,3.61978174224496));
#72168=CARTESIAN_POINT('Ctrl Pts',(18.1272,69.9890859425068,3.61978174224496));
#72169=CARTESIAN_POINT('Ctrl Pts',(18.3,70.5293315649033,3.51828106716275));
#72170=CARTESIAN_POINT('Ctrl Pts',(18.3,70.383083075285,3.61978174224496));
#72171=CARTESIAN_POINT('Ctrl Pts',(18.3,69.9890859425068,3.61978174224496));
#72172=CARTESIAN_POINT('Ctrl Pts',(18.18,70.5293315649033,3.51828106716275));
#72173=CARTESIAN_POINT('Ctrl Pts',(18.18,70.383083075285,3.61978174224496));
#72174=CARTESIAN_POINT('Ctrl Pts',(18.18,69.9890859425068,3.61978174224496));
#72175=CARTESIAN_POINT('Ctrl Pts',(18.3,69.1727147996426,3.30000006631017));
#72176=CARTESIAN_POINT('Ctrl Pts',(18.1272,69.1727147996426,3.30000006631017));
#72177=CARTESIAN_POINT('Ctrl Pts',(18.3,69.1727147996426,3.53137792125344));
#72178=CARTESIAN_POINT('Ctrl Pts',(18.1272,69.1727147996426,3.53137792125344));
#72179=CARTESIAN_POINT('Ctrl Pts',(18.3,69.338608533144,3.6634379722178));
#72180=CARTESIAN_POINT('Ctrl Pts',(18.1272,69.338608533144,3.6634379722178));
#72181=CARTESIAN_POINT('',(18.3,69.1727147996426,3.30000006631017));
#72182=CARTESIAN_POINT('',(18.3,69.338608533144,3.6634379722178));
#72183=CARTESIAN_POINT('Ctrl Pts',(18.3,69.1727147996426,3.30000006631017));
#72184=CARTESIAN_POINT('Ctrl Pts',(18.3,69.1727147996426,3.53137792125344));
#72185=CARTESIAN_POINT('Ctrl Pts',(18.3,69.338608533144,3.6634379722178));
#72186=CARTESIAN_POINT('',(18.18,69.1727147996426,3.30000006631017));
#72187=CARTESIAN_POINT('',(18.3,69.1727147996426,3.30000006631017));
#72188=CARTESIAN_POINT('',(18.18,69.338608533144,3.6634379722178));
#72189=CARTESIAN_POINT('Ctrl Pts',(18.18,69.1727147996426,3.30000006631017));
#72190=CARTESIAN_POINT('Ctrl Pts',(18.18,69.1727147996426,3.53137792125344));
#72191=CARTESIAN_POINT('Ctrl Pts',(18.18,69.338608533144,3.6634379722178));
#72192=CARTESIAN_POINT('',(18.3,69.338608533144,3.6634379722178));
#72193=CARTESIAN_POINT('Ctrl Pts',(18.3,69.2671214044094,3.00914057567716));
#72194=CARTESIAN_POINT('Ctrl Pts',(18.1272,69.2671214044094,3.00914057567716));
#72195=CARTESIAN_POINT('Ctrl Pts',(18.3,69.1727147996426,3.12428393438458));
#72196=CARTESIAN_POINT('Ctrl Pts',(18.1272,69.1727147996426,3.12428393438458));
#72197=CARTESIAN_POINT('Ctrl Pts',(18.3,69.1727147996426,3.30000006631017));
#72198=CARTESIAN_POINT('Ctrl Pts',(18.1272,69.1727147996426,3.30000006631017));
#72199=CARTESIAN_POINT('',(18.3,69.2671214044094,3.00914057567716));
#72200=CARTESIAN_POINT('Ctrl Pts',(18.3,69.2671214044094,3.00914057567716));
#72201=CARTESIAN_POINT('Ctrl Pts',(18.3,69.1727147996426,3.12428393438458));
#72202=CARTESIAN_POINT('Ctrl Pts',(18.3,69.1727147996426,3.30000006631017));
#72203=CARTESIAN_POINT('',(18.18,69.2671214044094,3.00914057567716));
#72204=CARTESIAN_POINT('',(18.3,69.2671214044094,3.00914057567716));
#72205=CARTESIAN_POINT('Ctrl Pts',(18.18,69.2671214044094,3.00914057567716));
#72206=CARTESIAN_POINT('Ctrl Pts',(18.18,69.1727147996426,3.12428393438458));
#72207=CARTESIAN_POINT('Ctrl Pts',(18.18,69.1727147996426,3.30000006631017));
#72208=CARTESIAN_POINT('Ctrl Pts',(18.3,69.5345155894756,2.83615299537778));
#72209=CARTESIAN_POINT('Ctrl Pts',(18.1272,69.5345155894756,2.83615299537778));
#72210=CARTESIAN_POINT('Ctrl Pts',(18.3,69.3615280091763,2.89399736598134));
#72211=CARTESIAN_POINT('Ctrl Pts',(18.1272,69.3615280091763,2.89399736598134));
#72212=CARTESIAN_POINT('Ctrl Pts',(18.3,69.2671214044094,3.00914057567716));
#72213=CARTESIAN_POINT('Ctrl Pts',(18.1272,69.2671214044094,3.00914057567716));
#72214=CARTESIAN_POINT('',(18.3,69.5345155894756,2.83615299537778));
#72215=CARTESIAN_POINT('Ctrl Pts',(18.3,69.5345155894756,2.83615299537778));
#72216=CARTESIAN_POINT('Ctrl Pts',(18.3,69.3615280091763,2.89399736598134));
#72217=CARTESIAN_POINT('Ctrl Pts',(18.3,69.2671214044094,3.00914057567716));
#72218=CARTESIAN_POINT('',(18.18,69.5345155894756,2.83615299537778));
#72219=CARTESIAN_POINT('',(18.3,69.5345155894756,2.83615299537778));
#72220=CARTESIAN_POINT('Ctrl Pts',(18.18,69.5345155894756,2.83615299537778));
#72221=CARTESIAN_POINT('Ctrl Pts',(18.18,69.3615280091763,2.89399736598134));
#72222=CARTESIAN_POINT('Ctrl Pts',(18.18,69.2671214044094,3.00914057567716));
#72223=CARTESIAN_POINT('Ctrl Pts',(18.3,69.9890859425068,2.77830847576261));
#72224=CARTESIAN_POINT('Ctrl Pts',(18.1272,69.9890859425068,2.77830847576261));
#72225=CARTESIAN_POINT('Ctrl Pts',(18.3,69.7075034677982,2.77830847576261));
#72226=CARTESIAN_POINT('Ctrl Pts',(18.1272,69.7075034677982,2.77830847576261));
#72227=CARTESIAN_POINT('Ctrl Pts',(18.3,69.5345155894756,2.83615299537778));
#72228=CARTESIAN_POINT('Ctrl Pts',(18.1272,69.5345155894756,2.83615299537778));
#72229=CARTESIAN_POINT('',(18.3,69.9890859425068,2.77830847576261));
#72230=CARTESIAN_POINT('Ctrl Pts',(18.3,69.9890859425068,2.77830847576261));
#72231=CARTESIAN_POINT('Ctrl Pts',(18.3,69.7075034677982,2.77830847576261));
#72232=CARTESIAN_POINT('Ctrl Pts',(18.3,69.5345155894756,2.83615299537778));
#72233=CARTESIAN_POINT('',(18.18,69.9890859425068,2.77830847576261));
#72234=CARTESIAN_POINT('',(18.3,69.9890859425068,2.77830847576261));
#72235=CARTESIAN_POINT('Ctrl Pts',(18.18,69.9890859425068,2.77830847576261));
#72236=CARTESIAN_POINT('Ctrl Pts',(18.18,69.7075034677982,2.77830847576261));
#72237=CARTESIAN_POINT('Ctrl Pts',(18.18,69.5345155894756,2.83615299537778));
#72238=CARTESIAN_POINT('Ctrl Pts',(18.3,70.3672577440739,2.81432488039136));
#72239=CARTESIAN_POINT('Ctrl Pts',(18.1272,70.3672577440739,2.81432488039136));
#72240=CARTESIAN_POINT('Ctrl Pts',(18.3,70.2270121872425,2.77830847576261));
#72241=CARTESIAN_POINT('Ctrl Pts',(18.1272,70.2270121872425,2.77830847576261));
#72242=CARTESIAN_POINT('Ctrl Pts',(18.3,69.9890859425068,2.77830847576261));
#72243=CARTESIAN_POINT('Ctrl Pts',(18.1272,69.9890859425068,2.77830847576261));
#72244=CARTESIAN_POINT('',(18.3,70.3672577440739,2.81432488039136));
#72245=CARTESIAN_POINT('Ctrl Pts',(18.3,70.3672577440739,2.81432488039136));
#72246=CARTESIAN_POINT('Ctrl Pts',(18.3,70.2270121872425,2.77830847576261));
#72247=CARTESIAN_POINT('Ctrl Pts',(18.3,69.9890859425068,2.77830847576261));
#72248=CARTESIAN_POINT('',(18.18,70.3672577440739,2.81432488039136));
#72249=CARTESIAN_POINT('',(18.3,70.3672577440739,2.81432488039136));
#72250=CARTESIAN_POINT('Ctrl Pts',(18.18,70.3672577440739,2.81432488039136));
#72251=CARTESIAN_POINT('Ctrl Pts',(18.18,70.2270121872425,2.77830847576261));
#72252=CARTESIAN_POINT('Ctrl Pts',(18.18,69.9890859425068,2.77830847576261));
#72253=CARTESIAN_POINT('Ctrl Pts',(18.3,70.6051841378212,2.91364260986447));
#72254=CARTESIAN_POINT('Ctrl Pts',(18.1272,70.6051841378212,2.91364260986447));
#72255=CARTESIAN_POINT('Ctrl Pts',(18.3,70.5075034499168,2.8503411360085));
#72256=CARTESIAN_POINT('Ctrl Pts',(18.1272,70.5075034499168,2.8503411360085));
#72257=CARTESIAN_POINT('Ctrl Pts',(18.3,70.3672577440739,2.81432488039136));
#72258=CARTESIAN_POINT('Ctrl Pts',(18.1272,70.3672577440739,2.81432488039136));
#72259=CARTESIAN_POINT('',(18.3,70.6051841378212,2.91364260986447));
#72260=CARTESIAN_POINT('Ctrl Pts',(18.3,70.6051841378212,2.91364260986447));
#72261=CARTESIAN_POINT('Ctrl Pts',(18.3,70.5075034499168,2.8503411360085));
#72262=CARTESIAN_POINT('Ctrl Pts',(18.3,70.3672577440739,2.81432488039136));
#72263=CARTESIAN_POINT('',(18.18,70.6051841378212,2.91364260986447));
#72264=CARTESIAN_POINT('',(18.3,70.6051841378212,2.91364260986447));
#72265=CARTESIAN_POINT('Ctrl Pts',(18.18,70.6051841378212,2.91364260986447));
#72266=CARTESIAN_POINT('Ctrl Pts',(18.18,70.5075034499168,2.8503411360085));
#72267=CARTESIAN_POINT('Ctrl Pts',(18.18,70.3672577440739,2.81432488039136));
#72268=CARTESIAN_POINT('Ctrl Pts',(18.3,70.754706710577,3.0740792401135));
#72269=CARTESIAN_POINT('Ctrl Pts',(18.1272,70.754706710577,3.0740792401135));
#72270=CARTESIAN_POINT('Ctrl Pts',(18.3,70.7028649747372,2.97694423273206));
#72271=CARTESIAN_POINT('Ctrl Pts',(18.1272,70.7028649747372,2.97694423273206));
#72272=CARTESIAN_POINT('Ctrl Pts',(18.3,70.6051841378212,2.91364260986447));
#72273=CARTESIAN_POINT('Ctrl Pts',(18.1272,70.6051841378212,2.91364260986447));
#72274=CARTESIAN_POINT('',(18.3,70.754706710577,3.0740792401135));
#72275=CARTESIAN_POINT('Ctrl Pts',(18.3,70.754706710577,3.0740792401135));
#72276=CARTESIAN_POINT('Ctrl Pts',(18.3,70.7028649747372,2.97694423273206));
#72277=CARTESIAN_POINT('Ctrl Pts',(18.3,70.6051841378212,2.91364260986447));
#72278=CARTESIAN_POINT('',(18.18,70.754706710577,3.0740792401135));
#72279=CARTESIAN_POINT('',(18.3,70.754706710577,3.0740792401135));
#72280=CARTESIAN_POINT('Ctrl Pts',(18.18,70.754706710577,3.0740792401135));
#72281=CARTESIAN_POINT('Ctrl Pts',(18.18,70.7028649747372,2.97694423273206));
#72282=CARTESIAN_POINT('Ctrl Pts',(18.18,70.6051841378212,2.91364260986447));
#72283=CARTESIAN_POINT('Ctrl Pts',(18.3,70.8065484464169,3.30000006631017));
#72284=CARTESIAN_POINT('Ctrl Pts',(18.1272,70.8065484464169,3.30000006631017));
#72285=CARTESIAN_POINT('Ctrl Pts',(18.3,70.8065484464169,3.17121424749494));
#72286=CARTESIAN_POINT('Ctrl Pts',(18.1272,70.8065484464169,3.17121424749494));
#72287=CARTESIAN_POINT('Ctrl Pts',(18.3,70.754706710577,3.0740792401135));
#72288=CARTESIAN_POINT('Ctrl Pts',(18.1272,70.754706710577,3.0740792401135));
#72289=CARTESIAN_POINT('',(18.3,70.8065484464169,3.30000006631017));
#72290=CARTESIAN_POINT('Ctrl Pts',(18.3,70.8065484464169,3.30000006631017));
#72291=CARTESIAN_POINT('Ctrl Pts',(18.3,70.8065484464169,3.17121424749494));
#72292=CARTESIAN_POINT('Ctrl Pts',(18.3,70.754706710577,3.0740792401135));
#72293=CARTESIAN_POINT('',(18.18,70.8065484464169,3.30000006631017));
#72294=CARTESIAN_POINT('',(18.3,70.8065484464169,3.30000006631017));
#72295=CARTESIAN_POINT('Ctrl Pts',(18.18,70.8065484464169,3.30000006631017));
#72296=CARTESIAN_POINT('Ctrl Pts',(18.18,70.8065484464169,3.17121424749494));
#72297=CARTESIAN_POINT('Ctrl Pts',(18.18,70.754706710577,3.0740792401135));
#72298=CARTESIAN_POINT('Ctrl Pts',(18.3,70.7126876711845,3.58976812139153));
#72299=CARTESIAN_POINT('Ctrl Pts',(18.1272,70.7126876711845,3.58976812139153));
#72300=CARTESIAN_POINT('Ctrl Pts',(18.3,70.8065484464169,3.47462491169572));
#72301=CARTESIAN_POINT('Ctrl Pts',(18.1272,70.8065484464169,3.47462491169572));
#72302=CARTESIAN_POINT('Ctrl Pts',(18.3,70.8065484464169,3.30000006631017));
#72303=CARTESIAN_POINT('Ctrl Pts',(18.1272,70.8065484464169,3.30000006631017));
#72304=CARTESIAN_POINT('',(18.3,70.7126876711845,3.58976812139153));
#72305=CARTESIAN_POINT('Ctrl Pts',(18.3,70.7126876711845,3.58976812139153));
#72306=CARTESIAN_POINT('Ctrl Pts',(18.3,70.8065484464169,3.47462491169572));
#72307=CARTESIAN_POINT('Ctrl Pts',(18.3,70.8065484464169,3.30000006631017));
#72308=CARTESIAN_POINT('',(18.18,70.7126876711845,3.58976812139153));
#72309=CARTESIAN_POINT('',(18.3,70.7126876711845,3.58976812139153));
#72310=CARTESIAN_POINT('Ctrl Pts',(18.18,70.7126876711845,3.58976812139153));
#72311=CARTESIAN_POINT('Ctrl Pts',(18.18,70.8065484464169,3.47462491169572));
#72312=CARTESIAN_POINT('Ctrl Pts',(18.18,70.8065484464169,3.30000006631017));
#72313=CARTESIAN_POINT('Ctrl Pts',(18.3,70.4458389431238,3.76330153122544));
#72314=CARTESIAN_POINT('Ctrl Pts',(18.1272,70.4458389431238,3.76330153122544));
#72315=CARTESIAN_POINT('Ctrl Pts',(18.3,70.6188267469406,3.70491140559316));
#72316=CARTESIAN_POINT('Ctrl Pts',(18.1272,70.6188267469406,3.70491140559316));
#72317=CARTESIAN_POINT('Ctrl Pts',(18.3,70.7126876711845,3.58976812139153));
#72318=CARTESIAN_POINT('Ctrl Pts',(18.1272,70.7126876711845,3.58976812139153));
#72319=CARTESIAN_POINT('',(18.3,70.4458389431238,3.76330153122544));
#72320=CARTESIAN_POINT('Ctrl Pts',(18.3,70.4458389431238,3.76330153122544));
#72321=CARTESIAN_POINT('Ctrl Pts',(18.3,70.6188267469406,3.70491140559316));
#72322=CARTESIAN_POINT('Ctrl Pts',(18.3,70.7126876711845,3.58976812139153));
#72323=CARTESIAN_POINT('',(18.18,70.4458389431238,3.76330153122544));
#72324=CARTESIAN_POINT('',(18.3,70.4458389431238,3.76330153122544));
#72325=CARTESIAN_POINT('Ctrl Pts',(18.18,70.4458389431238,3.76330153122544));
#72326=CARTESIAN_POINT('Ctrl Pts',(18.18,70.6188267469406,3.70491140559316));
#72327=CARTESIAN_POINT('Ctrl Pts',(18.18,70.7126876711845,3.58976812139153));
#72328=CARTESIAN_POINT('Ctrl Pts',(18.3,69.9890859425068,3.82169173136353));
#72329=CARTESIAN_POINT('Ctrl Pts',(18.1272,69.9890859425068,3.82169173136353));
#72330=CARTESIAN_POINT('Ctrl Pts',(18.3,70.2728512883186,3.82169173136353));
#72331=CARTESIAN_POINT('Ctrl Pts',(18.1272,70.2728512883186,3.82169173136353));
#72332=CARTESIAN_POINT('Ctrl Pts',(18.3,70.4458389431238,3.76330153122544));
#72333=CARTESIAN_POINT('Ctrl Pts',(18.1272,70.4458389431238,3.76330153122544));
#72334=CARTESIAN_POINT('',(18.3,69.9890859425068,3.82169173136353));
#72335=CARTESIAN_POINT('Ctrl Pts',(18.3,69.9890859425068,3.82169173136353));
#72336=CARTESIAN_POINT('Ctrl Pts',(18.3,70.2728512883186,3.82169173136353));
#72337=CARTESIAN_POINT('Ctrl Pts',(18.3,70.4458389431238,3.76330153122544));
#72338=CARTESIAN_POINT('',(18.18,69.9890859425068,3.82169173136353));
#72339=CARTESIAN_POINT('',(18.3,69.9890859425068,3.82169173136353));
#72340=CARTESIAN_POINT('Ctrl Pts',(18.18,69.9890859425068,3.82169173136353));
#72341=CARTESIAN_POINT('Ctrl Pts',(18.18,70.2728512883186,3.82169173136353));
#72342=CARTESIAN_POINT('Ctrl Pts',(18.18,70.4458389431238,3.76330153122544));
#72343=CARTESIAN_POINT('Ctrl Pts',(18.3,69.338608533144,3.6634379722178));
#72344=CARTESIAN_POINT('Ctrl Pts',(18.1272,69.338608533144,3.6634379722178));
#72345=CARTESIAN_POINT('Ctrl Pts',(18.3,69.5383356511593,3.82169173136353));
#72346=CARTESIAN_POINT('Ctrl Pts',(18.1272,69.5383356511593,3.82169173136353));
#72347=CARTESIAN_POINT('Ctrl Pts',(18.3,69.9890859425068,3.82169173136353));
#72348=CARTESIAN_POINT('Ctrl Pts',(18.1272,69.9890859425068,3.82169173136353));
#72349=CARTESIAN_POINT('Ctrl Pts',(18.3,69.338608533144,3.6634379722178));
#72350=CARTESIAN_POINT('Ctrl Pts',(18.3,69.5383356511593,3.82169173136353));
#72351=CARTESIAN_POINT('Ctrl Pts',(18.3,69.9890859425068,3.82169173136353));
#72352=CARTESIAN_POINT('Ctrl Pts',(18.18,69.338608533144,3.6634379722178));
#72353=CARTESIAN_POINT('Ctrl Pts',(18.18,69.5383356511593,3.82169173136353));
#72354=CARTESIAN_POINT('Ctrl Pts',(18.18,69.9890859425068,3.82169173136353));
#72355=CARTESIAN_POINT('Origin',(18.18,69.9896316230297,3.30000010356307));
#72356=CARTESIAN_POINT('Origin',(18.3,70.,5.5));
#72357=CARTESIAN_POINT('Ctrl Pts',(18.3,60.643929117918,2.7559345126152));
#72358=CARTESIAN_POINT('Ctrl Pts',(18.1272,60.643929117918,2.7559345126152));
#72359=CARTESIAN_POINT('Ctrl Pts',(18.3,60.643929117918,2.89126879572868));
#72360=CARTESIAN_POINT('Ctrl Pts',(18.1272,60.643929117918,2.89126879572868));
#72361=CARTESIAN_POINT('Ctrl Pts',(18.3,60.5293315887451,2.97203279137611));
#72362=CARTESIAN_POINT('Ctrl Pts',(18.1272,60.5293315887451,2.97203279137611));
#72363=CARTESIAN_POINT('',(18.3,60.643929117918,2.7559345126152));
#72364=CARTESIAN_POINT('',(18.3,60.5293315887451,2.97203279137611));
#72365=CARTESIAN_POINT('Ctrl Pts',(18.3,60.643929117918,2.7559345126152));
#72366=CARTESIAN_POINT('Ctrl Pts',(18.3,60.643929117918,2.89126879572868));
#72367=CARTESIAN_POINT('Ctrl Pts',(18.3,60.5293315887451,2.97203279137611));
#72368=CARTESIAN_POINT('',(18.18,60.643929117918,2.7559345126152));
#72369=CARTESIAN_POINT('',(18.3,60.643929117918,2.7559345126152));
#72370=CARTESIAN_POINT('',(18.18,60.5293315887451,2.97203279137611));
#72371=CARTESIAN_POINT('Ctrl Pts',(18.18,60.643929117918,2.7559345126152));
#72372=CARTESIAN_POINT('Ctrl Pts',(18.18,60.643929117918,2.89126879572868));
#72373=CARTESIAN_POINT('Ctrl Pts',(18.18,60.5293315887451,2.97203279137611));
#72374=CARTESIAN_POINT('',(18.3,60.5293315887451,2.97203279137611));
#72375=CARTESIAN_POINT('Ctrl Pts',(18.3,60.5140519380569,2.52619377374649));
#72376=CARTESIAN_POINT('Ctrl Pts',(18.1272,60.5140519380569,2.52619377374649));
#72377=CARTESIAN_POINT('Ctrl Pts',(18.3,60.643929117918,2.61841750741005));
#72378=CARTESIAN_POINT('Ctrl Pts',(18.1272,60.643929117918,2.61841750741005));
#72379=CARTESIAN_POINT('Ctrl Pts',(18.3,60.643929117918,2.7559345126152));
#72380=CARTESIAN_POINT('Ctrl Pts',(18.1272,60.643929117918,2.7559345126152));
#72381=CARTESIAN_POINT('',(18.3,60.5140519380569,2.52619377374649));
#72382=CARTESIAN_POINT('Ctrl Pts',(18.3,60.5140519380569,2.52619377374649));
#72383=CARTESIAN_POINT('Ctrl Pts',(18.3,60.643929117918,2.61841750741005));
#72384=CARTESIAN_POINT('Ctrl Pts',(18.3,60.643929117918,2.7559345126152));
#72385=CARTESIAN_POINT('',(18.18,60.5140519380569,2.52619377374649));
#72386=CARTESIAN_POINT('',(18.3,60.5140519380569,2.52619377374649));
#72387=CARTESIAN_POINT('Ctrl Pts',(18.18,60.5140519380569,2.52619377374649));
#72388=CARTESIAN_POINT('Ctrl Pts',(18.18,60.643929117918,2.61841750741005));
#72389=CARTESIAN_POINT('Ctrl Pts',(18.18,60.643929117918,2.7559345126152));
#72390=CARTESIAN_POINT('Ctrl Pts',(18.3,59.9890859663486,2.43397004008293));
#72391=CARTESIAN_POINT('Ctrl Pts',(18.1272,59.9890859663486,2.43397004008293));
#72392=CARTESIAN_POINT('Ctrl Pts',(18.3,60.3841746091843,2.43397004008293));
#72393=CARTESIAN_POINT('Ctrl Pts',(18.1272,60.3841746091843,2.43397004008293));
#72394=CARTESIAN_POINT('Ctrl Pts',(18.3,60.5140519380569,2.52619377374649));
#72395=CARTESIAN_POINT('Ctrl Pts',(18.1272,60.5140519380569,2.52619377374649));
#72396=CARTESIAN_POINT('',(18.3,59.9890859663486,2.43397004008293));
#72397=CARTESIAN_POINT('Ctrl Pts',(18.3,59.9890859663486,2.43397004008293));
#72398=CARTESIAN_POINT('Ctrl Pts',(18.3,60.3841746091843,2.43397004008293));
#72399=CARTESIAN_POINT('Ctrl Pts',(18.3,60.5140519380569,2.52619377374649));
#72400=CARTESIAN_POINT('',(18.18,59.9890859663486,2.43397004008293));
#72401=CARTESIAN_POINT('',(18.3,59.9890859663486,2.43397004008293));
#72402=CARTESIAN_POINT('Ctrl Pts',(18.18,59.9890859663486,2.43397004008293));
#72403=CARTESIAN_POINT('Ctrl Pts',(18.18,60.3841746091843,2.43397004008293));
#72404=CARTESIAN_POINT('Ctrl Pts',(18.18,60.5140519380569,2.52619377374649));
#72405=CARTESIAN_POINT('Ctrl Pts',(18.3,59.4652115046978,2.52619377374649));
#72406=CARTESIAN_POINT('Ctrl Pts',(18.1272,59.4652115046978,2.52619377374649));
#72407=CARTESIAN_POINT('Ctrl Pts',(18.3,59.5961801946163,2.43397004008293));
#72408=CARTESIAN_POINT('Ctrl Pts',(18.1272,59.5961801946163,2.43397004008293));
#72409=CARTESIAN_POINT('Ctrl Pts',(18.3,59.9890859663486,2.43397004008293));
#72410=CARTESIAN_POINT('Ctrl Pts',(18.1272,59.9890859663486,2.43397004008293));
#72411=CARTESIAN_POINT('',(18.3,59.4652115046978,2.52619377374649));
#72412=CARTESIAN_POINT('Ctrl Pts',(18.3,59.4652115046978,2.52619377374649));
#72413=CARTESIAN_POINT('Ctrl Pts',(18.3,59.5961801946163,2.43397004008293));
#72414=CARTESIAN_POINT('Ctrl Pts',(18.3,59.9890859663486,2.43397004008293));
#72415=CARTESIAN_POINT('',(18.18,59.4652115046978,2.52619377374649));
#72416=CARTESIAN_POINT('',(18.3,59.4652115046978,2.52619377374649));
#72417=CARTESIAN_POINT('Ctrl Pts',(18.18,59.4652115046978,2.52619377374649));
#72418=CARTESIAN_POINT('Ctrl Pts',(18.18,59.5961801946163,2.43397004008293));
#72419=CARTESIAN_POINT('Ctrl Pts',(18.18,59.9890859663486,2.43397004008293));
#72420=CARTESIAN_POINT('Ctrl Pts',(18.3,59.3342428147793,2.75375164151192));
#72421=CARTESIAN_POINT('Ctrl Pts',(18.1272,59.3342428147793,2.75375164151192));
#72422=CARTESIAN_POINT('Ctrl Pts',(18.3,59.3342428147793,2.61841750741005));
#72423=CARTESIAN_POINT('Ctrl Pts',(18.1272,59.3342428147793,2.61841750741005));
#72424=CARTESIAN_POINT('Ctrl Pts',(18.3,59.4652115046978,2.52619377374649));
#72425=CARTESIAN_POINT('Ctrl Pts',(18.1272,59.4652115046978,2.52619377374649));
#72426=CARTESIAN_POINT('',(18.3,59.3342428147793,2.75375164151192));
#72427=CARTESIAN_POINT('Ctrl Pts',(18.3,59.3342428147793,2.75375164151192));
#72428=CARTESIAN_POINT('Ctrl Pts',(18.3,59.3342428147793,2.61841750741005));
#72429=CARTESIAN_POINT('Ctrl Pts',(18.3,59.4652115046978,2.52619377374649));
#72430=CARTESIAN_POINT('',(18.18,59.3342428147793,2.75375164151192));
#72431=CARTESIAN_POINT('',(18.3,59.3342428147793,2.75375164151192));
#72432=CARTESIAN_POINT('Ctrl Pts',(18.18,59.3342428147793,2.75375164151192));
#72433=CARTESIAN_POINT('Ctrl Pts',(18.18,59.3342428147793,2.61841750741005));
#72434=CARTESIAN_POINT('Ctrl Pts',(18.18,59.4652115046978,2.52619377374649));
#72435=CARTESIAN_POINT('Ctrl Pts',(18.3,59.4646658241749,2.98130965828896));
#72436=CARTESIAN_POINT('Ctrl Pts',(18.1272,59.4646658241749,2.98130965828896));
#72437=CARTESIAN_POINT('Ctrl Pts',(18.3,59.3342428147793,2.8890859246254));
#72438=CARTESIAN_POINT('Ctrl Pts',(18.1272,59.3342428147793,2.8890859246254));
#72439=CARTESIAN_POINT('Ctrl Pts',(18.3,59.3342428147793,2.75375164151192));
#72440=CARTESIAN_POINT('Ctrl Pts',(18.1272,59.3342428147793,2.75375164151192));
#72441=CARTESIAN_POINT('',(18.3,59.4646658241749,2.98130965828896));
#72442=CARTESIAN_POINT('Ctrl Pts',(18.3,59.4646658241749,2.98130965828896));
#72443=CARTESIAN_POINT('Ctrl Pts',(18.3,59.3342428147793,2.8890859246254));
#72444=CARTESIAN_POINT('Ctrl Pts',(18.3,59.3342428147793,2.75375164151192));
#72445=CARTESIAN_POINT('',(18.18,59.4646658241749,2.98130965828896));
#72446=CARTESIAN_POINT('',(18.3,59.4646658241749,2.98130965828896));
#72447=CARTESIAN_POINT('Ctrl Pts',(18.18,59.4646658241749,2.98130965828896));
#72448=CARTESIAN_POINT('Ctrl Pts',(18.18,59.3342428147793,2.8890859246254));
#72449=CARTESIAN_POINT('Ctrl Pts',(18.18,59.3342428147793,2.75375164151192));
#72450=CARTESIAN_POINT('Ctrl Pts',(18.3,59.9890859663486,3.07353339195251));
#72451=CARTESIAN_POINT('Ctrl Pts',(18.1272,59.9890859663486,3.07353339195251));
#72452=CARTESIAN_POINT('Ctrl Pts',(18.3,59.5950888335705,3.07353339195251));
#72453=CARTESIAN_POINT('Ctrl Pts',(18.1272,59.5950888335705,3.07353339195251));
#72454=CARTESIAN_POINT('Ctrl Pts',(18.3,59.4646658241749,2.98130965828896));
#72455=CARTESIAN_POINT('Ctrl Pts',(18.1272,59.4646658241749,2.98130965828896));
#72456=CARTESIAN_POINT('',(18.3,59.9890859663486,3.07353339195251));
#72457=CARTESIAN_POINT('Ctrl Pts',(18.3,59.9890859663486,3.07353339195251));
#72458=CARTESIAN_POINT('Ctrl Pts',(18.3,59.5950888335705,3.07353339195251));
#72459=CARTESIAN_POINT('Ctrl Pts',(18.3,59.4646658241749,2.98130965828896));
#72460=CARTESIAN_POINT('',(18.18,59.9890859663486,3.07353339195251));
#72461=CARTESIAN_POINT('',(18.3,59.9890859663486,3.07353339195251));
#72462=CARTESIAN_POINT('Ctrl Pts',(18.18,59.9890859663486,3.07353339195251));
#72463=CARTESIAN_POINT('Ctrl Pts',(18.18,59.5950888335705,3.07353339195251));
#72464=CARTESIAN_POINT('Ctrl Pts',(18.18,59.4646658241749,2.98130965828896));
#72465=CARTESIAN_POINT('Ctrl Pts',(18.3,60.5293315887451,2.97203279137611));
#72466=CARTESIAN_POINT('Ctrl Pts',(18.1272,60.5293315887451,2.97203279137611));
#72467=CARTESIAN_POINT('Ctrl Pts',(18.3,60.3830830991268,3.07353339195251));
#72468=CARTESIAN_POINT('Ctrl Pts',(18.1272,60.3830830991268,3.07353339195251));
#72469=CARTESIAN_POINT('Ctrl Pts',(18.3,59.9890859663486,3.07353339195251));
#72470=CARTESIAN_POINT('Ctrl Pts',(18.1272,59.9890859663486,3.07353339195251));
#72471=CARTESIAN_POINT('Ctrl Pts',(18.3,60.5293315887451,2.97203279137611));
#72472=CARTESIAN_POINT('Ctrl Pts',(18.3,60.3830830991268,3.07353339195251));
#72473=CARTESIAN_POINT('Ctrl Pts',(18.3,59.9890859663486,3.07353339195251));
#72474=CARTESIAN_POINT('Ctrl Pts',(18.18,60.5293315887451,2.97203279137611));
#72475=CARTESIAN_POINT('Ctrl Pts',(18.18,60.3830830991268,3.07353339195251));
#72476=CARTESIAN_POINT('Ctrl Pts',(18.18,59.9890859663486,3.07353339195251));
#72477=CARTESIAN_POINT('Ctrl Pts',(18.3,59.1727148234844,2.75375164151192));
#72478=CARTESIAN_POINT('Ctrl Pts',(18.1272,59.1727148234844,2.75375164151192));
#72479=CARTESIAN_POINT('Ctrl Pts',(18.3,59.1727148234844,2.985129570961));
#72480=CARTESIAN_POINT('Ctrl Pts',(18.1272,59.1727148234844,2.985129570961));
#72481=CARTESIAN_POINT('Ctrl Pts',(18.3,59.3386085569858,3.11718962192535));
#72482=CARTESIAN_POINT('Ctrl Pts',(18.1272,59.3386085569858,3.11718962192535));
#72483=CARTESIAN_POINT('',(18.3,59.1727148234844,2.75375164151192));
#72484=CARTESIAN_POINT('',(18.3,59.3386085569858,3.11718962192535));
#72485=CARTESIAN_POINT('Ctrl Pts',(18.3,59.1727148234844,2.75375164151192));
#72486=CARTESIAN_POINT('Ctrl Pts',(18.3,59.1727148234844,2.985129570961));
#72487=CARTESIAN_POINT('Ctrl Pts',(18.3,59.3386085569858,3.11718962192535));
#72488=CARTESIAN_POINT('',(18.18,59.1727148234844,2.75375164151192));
#72489=CARTESIAN_POINT('',(18.3,59.1727148234844,2.75375164151192));
#72490=CARTESIAN_POINT('',(18.18,59.3386085569858,3.11718962192535));
#72491=CARTESIAN_POINT('Ctrl Pts',(18.18,59.1727148234844,2.75375164151192));
#72492=CARTESIAN_POINT('Ctrl Pts',(18.18,59.1727148234844,2.985129570961));
#72493=CARTESIAN_POINT('Ctrl Pts',(18.18,59.3386085569858,3.11718962192535));
#72494=CARTESIAN_POINT('',(18.3,59.3386085569858,3.11718962192535));
#72495=CARTESIAN_POINT('Ctrl Pts',(18.3,59.2671214282513,2.46289229989052));
#72496=CARTESIAN_POINT('Ctrl Pts',(18.1272,59.2671214282513,2.46289229989052));
#72497=CARTESIAN_POINT('Ctrl Pts',(18.3,59.1727148234844,2.57803550958633));
#72498=CARTESIAN_POINT('Ctrl Pts',(18.1272,59.1727148234844,2.57803550958633));
#72499=CARTESIAN_POINT('Ctrl Pts',(18.3,59.1727148234844,2.75375164151192));
#72500=CARTESIAN_POINT('Ctrl Pts',(18.1272,59.1727148234844,2.75375164151192));
#72501=CARTESIAN_POINT('',(18.3,59.2671214282513,2.46289229989052));
#72502=CARTESIAN_POINT('Ctrl Pts',(18.3,59.2671214282513,2.46289229989052));
#72503=CARTESIAN_POINT('Ctrl Pts',(18.3,59.1727148234844,2.57803550958633));
#72504=CARTESIAN_POINT('Ctrl Pts',(18.3,59.1727148234844,2.75375164151192));
#72505=CARTESIAN_POINT('',(18.18,59.2671214282513,2.46289229989052));
#72506=CARTESIAN_POINT('',(18.3,59.2671214282513,2.46289229989052));
#72507=CARTESIAN_POINT('Ctrl Pts',(18.18,59.2671214282513,2.46289229989052));
#72508=CARTESIAN_POINT('Ctrl Pts',(18.18,59.1727148234844,2.57803550958633));
#72509=CARTESIAN_POINT('Ctrl Pts',(18.18,59.1727148234844,2.75375164151192));
#72510=CARTESIAN_POINT('Ctrl Pts',(18.3,59.5345156133175,2.28990457057953));
#72511=CARTESIAN_POINT('Ctrl Pts',(18.1272,59.5345156133175,2.28990457057953));
#72512=CARTESIAN_POINT('Ctrl Pts',(18.3,59.3615280330181,2.34774894118309));
#72513=CARTESIAN_POINT('Ctrl Pts',(18.1272,59.3615280330181,2.34774894118309));
#72514=CARTESIAN_POINT('Ctrl Pts',(18.3,59.2671214282513,2.46289229989052));
#72515=CARTESIAN_POINT('Ctrl Pts',(18.1272,59.2671214282513,2.46289229989052));
#72516=CARTESIAN_POINT('',(18.3,59.5345156133175,2.28990457057953));
#72517=CARTESIAN_POINT('Ctrl Pts',(18.3,59.5345156133175,2.28990457057953));
#72518=CARTESIAN_POINT('Ctrl Pts',(18.3,59.3615280330181,2.34774894118309));
#72519=CARTESIAN_POINT('Ctrl Pts',(18.3,59.2671214282513,2.46289229989052));
#72520=CARTESIAN_POINT('',(18.18,59.5345156133175,2.28990457057953));
#72521=CARTESIAN_POINT('',(18.3,59.5345156133175,2.28990457057953));
#72522=CARTESIAN_POINT('Ctrl Pts',(18.18,59.5345156133175,2.28990457057953));
#72523=CARTESIAN_POINT('Ctrl Pts',(18.18,59.3615280330181,2.34774894118309));
#72524=CARTESIAN_POINT('Ctrl Pts',(18.18,59.2671214282513,2.46289229989052));
#72525=CARTESIAN_POINT('Ctrl Pts',(18.3,59.9890859663486,2.23206005096436));
#72526=CARTESIAN_POINT('Ctrl Pts',(18.1272,59.9890859663486,2.23206005096436));
#72527=CARTESIAN_POINT('Ctrl Pts',(18.3,59.7075034916401,2.23206005096436));
#72528=CARTESIAN_POINT('Ctrl Pts',(18.1272,59.7075034916401,2.23206005096436));
#72529=CARTESIAN_POINT('Ctrl Pts',(18.3,59.5345156133175,2.28990457057953));
#72530=CARTESIAN_POINT('Ctrl Pts',(18.1272,59.5345156133175,2.28990457057953));
#72531=CARTESIAN_POINT('',(18.3,59.9890859663486,2.23206005096436));
#72532=CARTESIAN_POINT('Ctrl Pts',(18.3,59.9890859663486,2.23206005096436));
#72533=CARTESIAN_POINT('Ctrl Pts',(18.3,59.7075034916401,2.23206005096436));
#72534=CARTESIAN_POINT('Ctrl Pts',(18.3,59.5345156133175,2.28990457057953));
#72535=CARTESIAN_POINT('',(18.18,59.9890859663486,2.23206005096436));
#72536=CARTESIAN_POINT('',(18.3,59.9890859663486,2.23206005096436));
#72537=CARTESIAN_POINT('Ctrl Pts',(18.18,59.9890859663486,2.23206005096436));
#72538=CARTESIAN_POINT('Ctrl Pts',(18.18,59.7075034916401,2.23206005096436));
#72539=CARTESIAN_POINT('Ctrl Pts',(18.18,59.5345156133175,2.28990457057953));
#72540=CARTESIAN_POINT('Ctrl Pts',(18.3,60.3672577679157,2.26807645559311));
#72541=CARTESIAN_POINT('Ctrl Pts',(18.1272,60.3672577679157,2.26807645559311));
#72542=CARTESIAN_POINT('Ctrl Pts',(18.3,60.2270122110844,2.23206005096436));
#72543=CARTESIAN_POINT('Ctrl Pts',(18.1272,60.2270122110844,2.23206005096436));
#72544=CARTESIAN_POINT('Ctrl Pts',(18.3,59.9890859663486,2.23206005096436));
#72545=CARTESIAN_POINT('Ctrl Pts',(18.1272,59.9890859663486,2.23206005096436));
#72546=CARTESIAN_POINT('',(18.3,60.3672577679157,2.26807645559311));
#72547=CARTESIAN_POINT('Ctrl Pts',(18.3,60.3672577679157,2.26807645559311));
#72548=CARTESIAN_POINT('Ctrl Pts',(18.3,60.2270122110844,2.23206005096436));
#72549=CARTESIAN_POINT('Ctrl Pts',(18.3,59.9890859663486,2.23206005096436));
#72550=CARTESIAN_POINT('',(18.18,60.3672577679157,2.26807645559311));
#72551=CARTESIAN_POINT('',(18.3,60.3672577679157,2.26807645559311));
#72552=CARTESIAN_POINT('Ctrl Pts',(18.18,60.3672577679157,2.26807645559311));
#72553=CARTESIAN_POINT('Ctrl Pts',(18.18,60.2270122110844,2.23206005096436));
#72554=CARTESIAN_POINT('Ctrl Pts',(18.18,59.9890859663486,2.23206005096436));
#72555=CARTESIAN_POINT('Ctrl Pts',(18.3,60.605184161663,2.36739433407783));
#72556=CARTESIAN_POINT('Ctrl Pts',(18.1272,60.605184161663,2.36739433407783));
#72557=CARTESIAN_POINT('Ctrl Pts',(18.3,60.5075034737587,2.30409256219864));
#72558=CARTESIAN_POINT('Ctrl Pts',(18.1272,60.5075034737587,2.30409256219864));
#72559=CARTESIAN_POINT('Ctrl Pts',(18.3,60.3672577679157,2.26807645559311));
#72560=CARTESIAN_POINT('Ctrl Pts',(18.1272,60.3672577679157,2.26807645559311));
#72561=CARTESIAN_POINT('',(18.3,60.605184161663,2.36739433407783));
#72562=CARTESIAN_POINT('Ctrl Pts',(18.3,60.605184161663,2.36739433407783));
#72563=CARTESIAN_POINT('Ctrl Pts',(18.3,60.5075034737587,2.30409256219864));
#72564=CARTESIAN_POINT('Ctrl Pts',(18.3,60.3672577679157,2.26807645559311));
#72565=CARTESIAN_POINT('',(18.18,60.605184161663,2.36739433407783));
#72566=CARTESIAN_POINT('',(18.3,60.605184161663,2.36739433407783));
#72567=CARTESIAN_POINT('Ctrl Pts',(18.18,60.605184161663,2.36739433407783));
#72568=CARTESIAN_POINT('Ctrl Pts',(18.18,60.5075034737587,2.30409256219864));
#72569=CARTESIAN_POINT('Ctrl Pts',(18.18,60.3672577679157,2.26807645559311));
#72570=CARTESIAN_POINT('Ctrl Pts',(18.3,60.7547067344189,2.52783096432686));
#72571=CARTESIAN_POINT('Ctrl Pts',(18.1272,60.7547067344189,2.52783096432686));
#72572=CARTESIAN_POINT('Ctrl Pts',(18.3,60.702864998579,2.43069580793381));
#72573=CARTESIAN_POINT('Ctrl Pts',(18.1272,60.702864998579,2.43069580793381));
#72574=CARTESIAN_POINT('Ctrl Pts',(18.3,60.605184161663,2.36739433407783));
#72575=CARTESIAN_POINT('Ctrl Pts',(18.1272,60.605184161663,2.36739433407783));
#72576=CARTESIAN_POINT('',(18.3,60.7547067344189,2.52783096432686));
#72577=CARTESIAN_POINT('Ctrl Pts',(18.3,60.7547067344189,2.52783096432686));
#72578=CARTESIAN_POINT('Ctrl Pts',(18.3,60.702864998579,2.43069580793381));
#72579=CARTESIAN_POINT('Ctrl Pts',(18.3,60.605184161663,2.36739433407783));
#72580=CARTESIAN_POINT('',(18.18,60.7547067344189,2.52783096432686));
#72581=CARTESIAN_POINT('',(18.3,60.7547067344189,2.52783096432686));
#72582=CARTESIAN_POINT('Ctrl Pts',(18.18,60.7547067344189,2.52783096432686));
#72583=CARTESIAN_POINT('Ctrl Pts',(18.18,60.702864998579,2.43069580793381));
#72584=CARTESIAN_POINT('Ctrl Pts',(18.18,60.605184161663,2.36739433407783));
#72585=CARTESIAN_POINT('Ctrl Pts',(18.3,60.8065484702587,2.75375164151192));
#72586=CARTESIAN_POINT('Ctrl Pts',(18.1272,60.8065484702587,2.75375164151192));
#72587=CARTESIAN_POINT('Ctrl Pts',(18.3,60.8065484702587,2.6249659717083));
#72588=CARTESIAN_POINT('Ctrl Pts',(18.1272,60.8065484702587,2.6249659717083));
#72589=CARTESIAN_POINT('Ctrl Pts',(18.3,60.7547067344189,2.52783096432686));
#72590=CARTESIAN_POINT('Ctrl Pts',(18.1272,60.7547067344189,2.52783096432686));
#72591=CARTESIAN_POINT('',(18.3,60.8065484702587,2.75375164151192));
#72592=CARTESIAN_POINT('Ctrl Pts',(18.3,60.8065484702587,2.75375164151192));
#72593=CARTESIAN_POINT('Ctrl Pts',(18.3,60.8065484702587,2.6249659717083));
#72594=CARTESIAN_POINT('Ctrl Pts',(18.3,60.7547067344189,2.52783096432686));
#72595=CARTESIAN_POINT('',(18.18,60.8065484702587,2.75375164151192));
#72596=CARTESIAN_POINT('',(18.3,60.8065484702587,2.75375164151192));
#72597=CARTESIAN_POINT('Ctrl Pts',(18.18,60.8065484702587,2.75375164151192));
#72598=CARTESIAN_POINT('Ctrl Pts',(18.18,60.8065484702587,2.6249659717083));
#72599=CARTESIAN_POINT('Ctrl Pts',(18.18,60.7547067344189,2.52783096432686));
#72600=CARTESIAN_POINT('Ctrl Pts',(18.3,60.7126876950264,3.04351977109909));
#72601=CARTESIAN_POINT('Ctrl Pts',(18.1272,60.7126876950264,3.04351977109909));
#72602=CARTESIAN_POINT('Ctrl Pts',(18.3,60.8065484702587,2.92837656140327));
#72603=CARTESIAN_POINT('Ctrl Pts',(18.1272,60.8065484702587,2.92837656140327));
#72604=CARTESIAN_POINT('Ctrl Pts',(18.3,60.8065484702587,2.75375164151192));
#72605=CARTESIAN_POINT('Ctrl Pts',(18.1272,60.8065484702587,2.75375164151192));
#72606=CARTESIAN_POINT('',(18.3,60.7126876950264,3.04351977109909));
#72607=CARTESIAN_POINT('Ctrl Pts',(18.3,60.7126876950264,3.04351977109909));
#72608=CARTESIAN_POINT('Ctrl Pts',(18.3,60.8065484702587,2.92837656140327));
#72609=CARTESIAN_POINT('Ctrl Pts',(18.3,60.8065484702587,2.75375164151192));
#72610=CARTESIAN_POINT('',(18.18,60.7126876950264,3.04351977109909));
#72611=CARTESIAN_POINT('',(18.3,60.7126876950264,3.04351977109909));
#72612=CARTESIAN_POINT('Ctrl Pts',(18.18,60.7126876950264,3.04351977109909));
#72613=CARTESIAN_POINT('Ctrl Pts',(18.18,60.8065484702587,2.92837656140327));
#72614=CARTESIAN_POINT('Ctrl Pts',(18.18,60.8065484702587,2.75375164151192));
#72615=CARTESIAN_POINT('Ctrl Pts',(18.3,60.4458390414715,3.217053180933));
#72616=CARTESIAN_POINT('Ctrl Pts',(18.1272,60.4458390414715,3.217053180933));
#72617=CARTESIAN_POINT('Ctrl Pts',(18.3,60.6188267707825,3.15866298079491));
#72618=CARTESIAN_POINT('Ctrl Pts',(18.1272,60.6188267707825,3.15866298079491));
#72619=CARTESIAN_POINT('Ctrl Pts',(18.3,60.7126876950264,3.04351977109909));
#72620=CARTESIAN_POINT('Ctrl Pts',(18.1272,60.7126876950264,3.04351977109909));
#72621=CARTESIAN_POINT('',(18.3,60.4458390414715,3.217053180933));
#72622=CARTESIAN_POINT('Ctrl Pts',(18.3,60.4458390414715,3.217053180933));
#72623=CARTESIAN_POINT('Ctrl Pts',(18.3,60.6188267707825,3.15866298079491));
#72624=CARTESIAN_POINT('Ctrl Pts',(18.3,60.7126876950264,3.04351977109909));
#72625=CARTESIAN_POINT('',(18.18,60.4458390414715,3.217053180933));
#72626=CARTESIAN_POINT('',(18.3,60.4458390414715,3.217053180933));
#72627=CARTESIAN_POINT('Ctrl Pts',(18.18,60.4458390414715,3.217053180933));
#72628=CARTESIAN_POINT('Ctrl Pts',(18.18,60.6188267707825,3.15866298079491));
#72629=CARTESIAN_POINT('Ctrl Pts',(18.18,60.7126876950264,3.04351977109909));
#72630=CARTESIAN_POINT('Ctrl Pts',(18.3,59.9890859663486,3.27544338107109));
#72631=CARTESIAN_POINT('Ctrl Pts',(18.1272,59.9890859663486,3.27544338107109));
#72632=CARTESIAN_POINT('Ctrl Pts',(18.3,60.2728513121605,3.27544338107109));
#72633=CARTESIAN_POINT('Ctrl Pts',(18.1272,60.2728513121605,3.27544338107109));
#72634=CARTESIAN_POINT('Ctrl Pts',(18.3,60.4458390414715,3.217053180933));
#72635=CARTESIAN_POINT('Ctrl Pts',(18.1272,60.4458390414715,3.217053180933));
#72636=CARTESIAN_POINT('',(18.3,59.9890859663486,3.27544338107109));
#72637=CARTESIAN_POINT('Ctrl Pts',(18.3,59.9890859663486,3.27544338107109));
#72638=CARTESIAN_POINT('Ctrl Pts',(18.3,60.2728513121605,3.27544338107109));
#72639=CARTESIAN_POINT('Ctrl Pts',(18.3,60.4458390414715,3.217053180933));
#72640=CARTESIAN_POINT('',(18.18,59.9890859663486,3.27544338107109));
#72641=CARTESIAN_POINT('',(18.3,59.9890859663486,3.27544338107109));
#72642=CARTESIAN_POINT('Ctrl Pts',(18.18,59.9890859663486,3.27544338107109));
#72643=CARTESIAN_POINT('Ctrl Pts',(18.18,60.2728513121605,3.27544338107109));
#72644=CARTESIAN_POINT('Ctrl Pts',(18.18,60.4458390414715,3.217053180933));
#72645=CARTESIAN_POINT('Ctrl Pts',(18.3,59.3386085569858,3.11718962192535));
#72646=CARTESIAN_POINT('Ctrl Pts',(18.1272,59.3386085569858,3.11718962192535));
#72647=CARTESIAN_POINT('Ctrl Pts',(18.3,59.5383356750011,3.27544338107109));
#72648=CARTESIAN_POINT('Ctrl Pts',(18.1272,59.5383356750011,3.27544338107109));
#72649=CARTESIAN_POINT('Ctrl Pts',(18.3,59.9890859663486,3.27544338107109));
#72650=CARTESIAN_POINT('Ctrl Pts',(18.1272,59.9890859663486,3.27544338107109));
#72651=CARTESIAN_POINT('Ctrl Pts',(18.3,59.3386085569858,3.11718962192535));
#72652=CARTESIAN_POINT('Ctrl Pts',(18.3,59.5383356750011,3.27544338107109));
#72653=CARTESIAN_POINT('Ctrl Pts',(18.3,59.9890859663486,3.27544338107109));
#72654=CARTESIAN_POINT('Ctrl Pts',(18.18,59.3386085569858,3.11718962192535));
#72655=CARTESIAN_POINT('Ctrl Pts',(18.18,59.5383356750011,3.27544338107109));
#72656=CARTESIAN_POINT('Ctrl Pts',(18.18,59.9890859663486,3.27544338107109));
#72657=CARTESIAN_POINT('Origin',(18.18,59.9896316468716,3.29999997317791));
#72658=CARTESIAN_POINT('Origin',(18.3,60.8065484702587,3.90518411099911));
#72659=CARTESIAN_POINT('',(18.3,60.8065484702587,3.90518411099911));
#72660=CARTESIAN_POINT('',(18.3,60.8065484702587,3.77858108878136));
#72661=CARTESIAN_POINT('',(18.3,60.8065484702587,4.70259205549955));
#72662=CARTESIAN_POINT('',(18.18,60.8065484702587,3.90518411099911));
#72663=CARTESIAN_POINT('',(18.3,60.8065484702587,3.90518411099911));
#72664=CARTESIAN_POINT('',(18.18,60.8065484702587,3.77858108878136));
#72665=CARTESIAN_POINT('',(18.18,60.8065484702587,3.90518411099911));
#72666=CARTESIAN_POINT('',(18.3,60.8065484702587,3.77858108878136));
#72667=CARTESIAN_POINT('Ctrl Pts',(18.3,60.5926330626011,4.07980895638466));
#72668=CARTESIAN_POINT('Ctrl Pts',(18.1272,60.5926330626011,4.07980895638466));
#72669=CARTESIAN_POINT('Ctrl Pts',(18.3,60.702864998579,3.95648016631603));
#72670=CARTESIAN_POINT('Ctrl Pts',(18.1272,60.702864998579,3.95648016631603));
#72671=CARTESIAN_POINT('Ctrl Pts',(18.3,60.8065484702587,3.90518411099911));
#72672=CARTESIAN_POINT('Ctrl Pts',(18.1272,60.8065484702587,3.90518411099911));
#72673=CARTESIAN_POINT('',(18.3,60.5926330626011,4.07980895638466));
#72674=CARTESIAN_POINT('Ctrl Pts',(18.3,60.5926330626011,4.07980895638466));
#72675=CARTESIAN_POINT('Ctrl Pts',(18.3,60.702864998579,3.95648016631603));
#72676=CARTESIAN_POINT('Ctrl Pts',(18.3,60.8065484702587,3.90518411099911));
#72677=CARTESIAN_POINT('',(18.18,60.5926330626011,4.07980895638466));
#72678=CARTESIAN_POINT('',(18.3,60.5926330626011,4.07980895638466));
#72679=CARTESIAN_POINT('Ctrl Pts',(18.18,60.5926330626011,4.07980895638466));
#72680=CARTESIAN_POINT('Ctrl Pts',(18.18,60.702864998579,3.95648016631603));
#72681=CARTESIAN_POINT('Ctrl Pts',(18.18,60.8065484702587,3.90518411099911));
#72682=CARTESIAN_POINT('Ctrl Pts',(18.3,60.4049113631248,4.36793989539146));
#72683=CARTESIAN_POINT('Ctrl Pts',(18.1272,60.4049113631248,4.36793989539146));
#72684=CARTESIAN_POINT('Ctrl Pts',(18.3,60.4824011266231,4.20313774645328));
#72685=CARTESIAN_POINT('Ctrl Pts',(18.1272,60.4824011266231,4.20313774645328));
#72686=CARTESIAN_POINT('Ctrl Pts',(18.3,60.5926330626011,4.07980895638466));
#72687=CARTESIAN_POINT('Ctrl Pts',(18.1272,60.5926330626011,4.07980895638466));
#72688=CARTESIAN_POINT('',(18.3,60.4049113631248,4.36793989539146));
#72689=CARTESIAN_POINT('Ctrl Pts',(18.3,60.4049113631248,4.36793989539146));
#72690=CARTESIAN_POINT('Ctrl Pts',(18.3,60.4824011266231,4.20313774645328));
#72691=CARTESIAN_POINT('Ctrl Pts',(18.3,60.5926330626011,4.07980895638466));
#72692=CARTESIAN_POINT('',(18.18,60.4049113631248,4.36793989539146));
#72693=CARTESIAN_POINT('',(18.3,60.4049113631248,4.36793989539146));
#72694=CARTESIAN_POINT('Ctrl Pts',(18.18,60.4049113631248,4.36793989539146));
#72695=CARTESIAN_POINT('Ctrl Pts',(18.18,60.4824011266231,4.20313774645328));
#72696=CARTESIAN_POINT('Ctrl Pts',(18.18,60.5926330626011,4.07980895638466));
#72697=CARTESIAN_POINT('Origin',(18.3,60.2150069415569,4.36793989539146));
#72698=CARTESIAN_POINT('',(18.3,60.2150069415569,4.36793989539146));
#72699=CARTESIAN_POINT('',(18.3,65.1075034707785,4.36793989539146));
#72700=CARTESIAN_POINT('',(18.18,60.2150069415569,4.36793989539146));
#72701=CARTESIAN_POINT('',(18.3,60.2150069415569,4.36793989539146));
#72702=CARTESIAN_POINT('',(18.18,60.2150069415569,4.36793989539146));
#72703=CARTESIAN_POINT('Ctrl Pts',(18.3,60.3165075421333,4.16111863255501));
#72704=CARTESIAN_POINT('Ctrl Pts',(18.1272,60.3165075421333,4.16111863255501));
#72705=CARTESIAN_POINT('Ctrl Pts',(18.3,60.2488404750824,4.27626184225082));
#72706=CARTESIAN_POINT('Ctrl Pts',(18.1272,60.2488404750824,4.27626184225082));
#72707=CARTESIAN_POINT('Ctrl Pts',(18.3,60.2150069415569,4.36793989539146));
#72708=CARTESIAN_POINT('Ctrl Pts',(18.1272,60.2150069415569,4.36793989539146));
#72709=CARTESIAN_POINT('',(18.3,60.3165075421333,4.16111863255501));
#72710=CARTESIAN_POINT('Ctrl Pts',(18.3,60.3165075421333,4.16111863255501));
#72711=CARTESIAN_POINT('Ctrl Pts',(18.3,60.2488404750824,4.27626184225082));
#72712=CARTESIAN_POINT('Ctrl Pts',(18.3,60.2150069415569,4.36793989539146));
#72713=CARTESIAN_POINT('',(18.18,60.3165075421333,4.16111863255501));
#72714=CARTESIAN_POINT('',(18.3,60.3165075421333,4.16111863255501));
#72715=CARTESIAN_POINT('Ctrl Pts',(18.18,60.3165075421333,4.16111863255501));
#72716=CARTESIAN_POINT('Ctrl Pts',(18.18,60.2488404750824,4.27626184225082));
#72717=CARTESIAN_POINT('Ctrl Pts',(18.18,60.2150069415569,4.36793989539146));
#72718=CARTESIAN_POINT('Ctrl Pts',(18.3,60.4518418252468,3.97503404915333));
#72719=CARTESIAN_POINT('Ctrl Pts',(18.1272,60.4518418252468,3.97503404915333));
#72720=CARTESIAN_POINT('Ctrl Pts',(18.3,60.3841747581959,4.04597542285919));
#72721=CARTESIAN_POINT('Ctrl Pts',(18.1272,60.3841747581959,4.04597542285919));
#72722=CARTESIAN_POINT('Ctrl Pts',(18.3,60.3165075421333,4.16111863255501));
#72723=CARTESIAN_POINT('Ctrl Pts',(18.1272,60.3165075421333,4.16111863255501));
#72724=CARTESIAN_POINT('',(18.3,60.4518418252468,3.97503404915333));
#72725=CARTESIAN_POINT('Ctrl Pts',(18.3,60.4518418252468,3.97503404915333));
#72726=CARTESIAN_POINT('Ctrl Pts',(18.3,60.3841747581959,4.04597542285919));
#72727=CARTESIAN_POINT('Ctrl Pts',(18.3,60.3165075421333,4.16111863255501));
#72728=CARTESIAN_POINT('',(18.18,60.4518418252468,3.97503404915333));
#72729=CARTESIAN_POINT('',(18.3,60.4518418252468,3.97503404915333));
#72730=CARTESIAN_POINT('Ctrl Pts',(18.18,60.4518418252468,3.97503404915333));
#72731=CARTESIAN_POINT('Ctrl Pts',(18.18,60.3841747581959,4.04597542285919));
#72732=CARTESIAN_POINT('Ctrl Pts',(18.18,60.3165075421333,4.16111863255501));
#72733=CARTESIAN_POINT('Origin',(18.3,59.2000000417232,3.97503404915333));
#72734=CARTESIAN_POINT('',(18.3,59.2000000417232,3.97503404915333));
#72735=CARTESIAN_POINT('',(18.3,64.6000000208616,3.97503404915333));
#72736=CARTESIAN_POINT('',(18.18,59.2000000417232,3.97503404915333));
#72737=CARTESIAN_POINT('',(18.3,59.2000000417232,3.97503404915333));
#72738=CARTESIAN_POINT('',(18.18,59.2000000417232,3.97503404915333));
#72739=CARTESIAN_POINT('Origin',(18.3,59.2000000417232,3.77858108878136));
#72740=CARTESIAN_POINT('',(18.3,59.2000000417232,3.77858108878136));
#72741=CARTESIAN_POINT('',(18.3,59.2000000417232,4.63929054439068));
#72742=CARTESIAN_POINT('',(18.18,59.2000000417232,3.77858108878136));
#72743=CARTESIAN_POINT('',(18.3,59.2000000417232,3.77858108878136));
#72744=CARTESIAN_POINT('',(18.18,59.2000000417232,3.77858108878136));
#72745=CARTESIAN_POINT('Origin',(18.3,60.8065484702587,3.77858108878136));
#72746=CARTESIAN_POINT('',(18.3,65.4032742351294,3.77858108878136));
#72747=CARTESIAN_POINT('',(18.18,60.8065484702587,3.77858108878136));
#72748=CARTESIAN_POINT('Origin',(18.18,59.9896316468716,3.29999997317791));
#72749=CARTESIAN_POINT('Origin',(18.3,70.,5.5));
#72750=CARTESIAN_POINT('Ctrl Pts',(18.3,50.643929117918,2.66698497384787));
#72751=CARTESIAN_POINT('Ctrl Pts',(18.1272,50.643929117918,2.66698497384787));
#72752=CARTESIAN_POINT('Ctrl Pts',(18.3,50.643929117918,2.80231925696135));
#72753=CARTESIAN_POINT('Ctrl Pts',(18.1272,50.643929117918,2.80231925696135));
#72754=CARTESIAN_POINT('Ctrl Pts',(18.3,50.5293315887451,2.88308325260878));
#72755=CARTESIAN_POINT('Ctrl Pts',(18.1272,50.5293315887451,2.88308325260878));
#72756=CARTESIAN_POINT('',(18.3,50.643929117918,2.66698497384787));
#72757=CARTESIAN_POINT('',(18.3,50.5293315887451,2.88308325260878));
#72758=CARTESIAN_POINT('Ctrl Pts',(18.3,50.643929117918,2.66698497384787));
#72759=CARTESIAN_POINT('Ctrl Pts',(18.3,50.643929117918,2.80231925696135));
#72760=CARTESIAN_POINT('Ctrl Pts',(18.3,50.5293315887451,2.88308325260878));
#72761=CARTESIAN_POINT('',(18.18,50.643929117918,2.66698497384787));
#72762=CARTESIAN_POINT('',(18.3,50.643929117918,2.66698497384787));
#72763=CARTESIAN_POINT('',(18.18,50.5293315887451,2.88308325260878));
#72764=CARTESIAN_POINT('Ctrl Pts',(18.18,50.643929117918,2.66698497384787));
#72765=CARTESIAN_POINT('Ctrl Pts',(18.18,50.643929117918,2.80231925696135));
#72766=CARTESIAN_POINT('Ctrl Pts',(18.18,50.5293315887451,2.88308325260878));
#72767=CARTESIAN_POINT('',(18.3,50.5293315887451,2.88308325260878));
#72768=CARTESIAN_POINT('Ctrl Pts',(18.3,50.5140519380569,2.43724423497915));
#72769=CARTESIAN_POINT('Ctrl Pts',(18.1272,50.5140519380569,2.43724423497915));
#72770=CARTESIAN_POINT('Ctrl Pts',(18.3,50.643929117918,2.52946796864271));
#72771=CARTESIAN_POINT('Ctrl Pts',(18.1272,50.643929117918,2.52946796864271));
#72772=CARTESIAN_POINT('Ctrl Pts',(18.3,50.643929117918,2.66698497384787));
#72773=CARTESIAN_POINT('Ctrl Pts',(18.1272,50.643929117918,2.66698497384787));
#72774=CARTESIAN_POINT('',(18.3,50.5140519380569,2.43724423497915));
#72775=CARTESIAN_POINT('Ctrl Pts',(18.3,50.5140519380569,2.43724423497915));
#72776=CARTESIAN_POINT('Ctrl Pts',(18.3,50.643929117918,2.52946796864271));
#72777=CARTESIAN_POINT('Ctrl Pts',(18.3,50.643929117918,2.66698497384787));
#72778=CARTESIAN_POINT('',(18.18,50.5140519380569,2.43724423497915));
#72779=CARTESIAN_POINT('',(18.3,50.5140519380569,2.43724423497915));
#72780=CARTESIAN_POINT('Ctrl Pts',(18.18,50.5140519380569,2.43724423497915));
#72781=CARTESIAN_POINT('Ctrl Pts',(18.18,50.643929117918,2.52946796864271));
#72782=CARTESIAN_POINT('Ctrl Pts',(18.18,50.643929117918,2.66698497384787));
#72783=CARTESIAN_POINT('Ctrl Pts',(18.3,49.9890859663486,2.34502050131559));
#72784=CARTESIAN_POINT('Ctrl Pts',(18.1272,49.9890859663486,2.34502050131559));
#72785=CARTESIAN_POINT('Ctrl Pts',(18.3,50.3841746091843,2.34502050131559));
#72786=CARTESIAN_POINT('Ctrl Pts',(18.1272,50.3841746091843,2.34502050131559));
#72787=CARTESIAN_POINT('Ctrl Pts',(18.3,50.5140519380569,2.43724423497915));
#72788=CARTESIAN_POINT('Ctrl Pts',(18.1272,50.5140519380569,2.43724423497915));
#72789=CARTESIAN_POINT('',(18.3,49.9890859663486,2.34502050131559));
#72790=CARTESIAN_POINT('Ctrl Pts',(18.3,49.9890859663486,2.34502050131559));
#72791=CARTESIAN_POINT('Ctrl Pts',(18.3,50.3841746091843,2.34502050131559));
#72792=CARTESIAN_POINT('Ctrl Pts',(18.3,50.5140519380569,2.43724423497915));
#72793=CARTESIAN_POINT('',(18.18,49.9890859663486,2.34502050131559));
#72794=CARTESIAN_POINT('',(18.3,49.9890859663486,2.34502050131559));
#72795=CARTESIAN_POINT('Ctrl Pts',(18.18,49.9890859663486,2.34502050131559));
#72796=CARTESIAN_POINT('Ctrl Pts',(18.18,50.3841746091843,2.34502050131559));
#72797=CARTESIAN_POINT('Ctrl Pts',(18.18,50.5140519380569,2.43724423497915));
#72798=CARTESIAN_POINT('Ctrl Pts',(18.3,49.4652115046978,2.43724423497915));
#72799=CARTESIAN_POINT('Ctrl Pts',(18.1272,49.4652115046978,2.43724423497915));
#72800=CARTESIAN_POINT('Ctrl Pts',(18.3,49.5961801946163,2.34502050131559));
#72801=CARTESIAN_POINT('Ctrl Pts',(18.1272,49.5961801946163,2.34502050131559));
#72802=CARTESIAN_POINT('Ctrl Pts',(18.3,49.9890859663486,2.34502050131559));
#72803=CARTESIAN_POINT('Ctrl Pts',(18.1272,49.9890859663486,2.34502050131559));
#72804=CARTESIAN_POINT('',(18.3,49.4652115046978,2.43724423497915));
#72805=CARTESIAN_POINT('Ctrl Pts',(18.3,49.4652115046978,2.43724423497915));
#72806=CARTESIAN_POINT('Ctrl Pts',(18.3,49.5961801946163,2.34502050131559));
#72807=CARTESIAN_POINT('Ctrl Pts',(18.3,49.9890859663486,2.34502050131559));
#72808=CARTESIAN_POINT('',(18.18,49.4652115046978,2.43724423497915));
#72809=CARTESIAN_POINT('',(18.3,49.4652115046978,2.43724423497915));
#72810=CARTESIAN_POINT('Ctrl Pts',(18.18,49.4652115046978,2.43724423497915));
#72811=CARTESIAN_POINT('Ctrl Pts',(18.18,49.5961801946163,2.34502050131559));
#72812=CARTESIAN_POINT('Ctrl Pts',(18.18,49.9890859663486,2.34502050131559));
#72813=CARTESIAN_POINT('Ctrl Pts',(18.3,49.3342428147793,2.66480210274458));
#72814=CARTESIAN_POINT('Ctrl Pts',(18.1272,49.3342428147793,2.66480210274458));
#72815=CARTESIAN_POINT('Ctrl Pts',(18.3,49.3342428147793,2.52946796864271));
#72816=CARTESIAN_POINT('Ctrl Pts',(18.1272,49.3342428147793,2.52946796864271));
#72817=CARTESIAN_POINT('Ctrl Pts',(18.3,49.4652115046978,2.43724423497915));
#72818=CARTESIAN_POINT('Ctrl Pts',(18.1272,49.4652115046978,2.43724423497915));
#72819=CARTESIAN_POINT('',(18.3,49.3342428147793,2.66480210274458));
#72820=CARTESIAN_POINT('Ctrl Pts',(18.3,49.3342428147793,2.66480210274458));
#72821=CARTESIAN_POINT('Ctrl Pts',(18.3,49.3342428147793,2.52946796864271));
#72822=CARTESIAN_POINT('Ctrl Pts',(18.3,49.4652115046978,2.43724423497915));
#72823=CARTESIAN_POINT('',(18.18,49.3342428147793,2.66480210274458));
#72824=CARTESIAN_POINT('',(18.3,49.3342428147793,2.66480210274458));
#72825=CARTESIAN_POINT('Ctrl Pts',(18.18,49.3342428147793,2.66480210274458));
#72826=CARTESIAN_POINT('Ctrl Pts',(18.18,49.3342428147793,2.52946796864271));
#72827=CARTESIAN_POINT('Ctrl Pts',(18.18,49.4652115046978,2.43724423497915));
#72828=CARTESIAN_POINT('Ctrl Pts',(18.3,49.4646658241749,2.89236011952162));
#72829=CARTESIAN_POINT('Ctrl Pts',(18.1272,49.4646658241749,2.89236011952162));
#72830=CARTESIAN_POINT('Ctrl Pts',(18.3,49.3342428147793,2.80013638585806));
#72831=CARTESIAN_POINT('Ctrl Pts',(18.1272,49.3342428147793,2.80013638585806));
#72832=CARTESIAN_POINT('Ctrl Pts',(18.3,49.3342428147793,2.66480210274458));
#72833=CARTESIAN_POINT('Ctrl Pts',(18.1272,49.3342428147793,2.66480210274458));
#72834=CARTESIAN_POINT('',(18.3,49.4646658241749,2.89236011952162));
#72835=CARTESIAN_POINT('Ctrl Pts',(18.3,49.4646658241749,2.89236011952162));
#72836=CARTESIAN_POINT('Ctrl Pts',(18.3,49.3342428147793,2.80013638585806));
#72837=CARTESIAN_POINT('Ctrl Pts',(18.3,49.3342428147793,2.66480210274458));
#72838=CARTESIAN_POINT('',(18.18,49.4646658241749,2.89236011952162));
#72839=CARTESIAN_POINT('',(18.3,49.4646658241749,2.89236011952162));
#72840=CARTESIAN_POINT('Ctrl Pts',(18.18,49.4646658241749,2.89236011952162));
#72841=CARTESIAN_POINT('Ctrl Pts',(18.18,49.3342428147793,2.80013638585806));
#72842=CARTESIAN_POINT('Ctrl Pts',(18.18,49.3342428147793,2.66480210274458));
#72843=CARTESIAN_POINT('Ctrl Pts',(18.3,49.9890859663486,2.98458385318518));
#72844=CARTESIAN_POINT('Ctrl Pts',(18.1272,49.9890859663486,2.98458385318518));
#72845=CARTESIAN_POINT('Ctrl Pts',(18.3,49.5950888335705,2.98458385318518));
#72846=CARTESIAN_POINT('Ctrl Pts',(18.1272,49.5950888335705,2.98458385318518));
#72847=CARTESIAN_POINT('Ctrl Pts',(18.3,49.4646658241749,2.89236011952162));
#72848=CARTESIAN_POINT('Ctrl Pts',(18.1272,49.4646658241749,2.89236011952162));
#72849=CARTESIAN_POINT('',(18.3,49.9890859663486,2.98458385318518));
#72850=CARTESIAN_POINT('Ctrl Pts',(18.3,49.9890859663486,2.98458385318518));
#72851=CARTESIAN_POINT('Ctrl Pts',(18.3,49.5950888335705,2.98458385318518));
#72852=CARTESIAN_POINT('Ctrl Pts',(18.3,49.4646658241749,2.89236011952162));
#72853=CARTESIAN_POINT('',(18.18,49.9890859663486,2.98458385318518));
#72854=CARTESIAN_POINT('',(18.3,49.9890859663486,2.98458385318518));
#72855=CARTESIAN_POINT('Ctrl Pts',(18.18,49.9890859663486,2.98458385318518));
#72856=CARTESIAN_POINT('Ctrl Pts',(18.18,49.5950888335705,2.98458385318518));
#72857=CARTESIAN_POINT('Ctrl Pts',(18.18,49.4646658241749,2.89236011952162));
#72858=CARTESIAN_POINT('Ctrl Pts',(18.3,50.5293315887451,2.88308325260878));
#72859=CARTESIAN_POINT('Ctrl Pts',(18.1272,50.5293315887451,2.88308325260878));
#72860=CARTESIAN_POINT('Ctrl Pts',(18.3,50.3830830991268,2.98458385318518));
#72861=CARTESIAN_POINT('Ctrl Pts',(18.1272,50.3830830991268,2.98458385318518));
#72862=CARTESIAN_POINT('Ctrl Pts',(18.3,49.9890859663486,2.98458385318518));
#72863=CARTESIAN_POINT('Ctrl Pts',(18.1272,49.9890859663486,2.98458385318518));
#72864=CARTESIAN_POINT('Ctrl Pts',(18.3,50.5293315887451,2.88308325260878));
#72865=CARTESIAN_POINT('Ctrl Pts',(18.3,50.3830830991268,2.98458385318518));
#72866=CARTESIAN_POINT('Ctrl Pts',(18.3,49.9890859663486,2.98458385318518));
#72867=CARTESIAN_POINT('Ctrl Pts',(18.18,50.5293315887451,2.88308325260878));
#72868=CARTESIAN_POINT('Ctrl Pts',(18.18,50.3830830991268,2.98458385318518));
#72869=CARTESIAN_POINT('Ctrl Pts',(18.18,49.9890859663486,2.98458385318518));
#72870=CARTESIAN_POINT('Ctrl Pts',(18.3,49.1727148234844,2.66480210274458));
#72871=CARTESIAN_POINT('Ctrl Pts',(18.1272,49.1727148234844,2.66480210274458));
#72872=CARTESIAN_POINT('Ctrl Pts',(18.3,49.1727148234844,2.89618003219366));
#72873=CARTESIAN_POINT('Ctrl Pts',(18.1272,49.1727148234844,2.89618003219366));
#72874=CARTESIAN_POINT('Ctrl Pts',(18.3,49.3386085569858,3.02824008315802));
#72875=CARTESIAN_POINT('Ctrl Pts',(18.1272,49.3386085569858,3.02824008315802));
#72876=CARTESIAN_POINT('',(18.3,49.1727148234844,2.66480210274458));
#72877=CARTESIAN_POINT('',(18.3,49.3386085569858,3.02824008315802));
#72878=CARTESIAN_POINT('Ctrl Pts',(18.3,49.1727148234844,2.66480210274458));
#72879=CARTESIAN_POINT('Ctrl Pts',(18.3,49.1727148234844,2.89618003219366));
#72880=CARTESIAN_POINT('Ctrl Pts',(18.3,49.3386085569858,3.02824008315802));
#72881=CARTESIAN_POINT('',(18.18,49.1727148234844,2.66480210274458));
#72882=CARTESIAN_POINT('',(18.3,49.1727148234844,2.66480210274458));
#72883=CARTESIAN_POINT('',(18.18,49.3386085569858,3.02824008315802));
#72884=CARTESIAN_POINT('Ctrl Pts',(18.18,49.1727148234844,2.66480210274458));
#72885=CARTESIAN_POINT('Ctrl Pts',(18.18,49.1727148234844,2.89618003219366));
#72886=CARTESIAN_POINT('Ctrl Pts',(18.18,49.3386085569858,3.02824008315802));
#72887=CARTESIAN_POINT('',(18.3,49.3386085569858,3.02824008315802));
#72888=CARTESIAN_POINT('Ctrl Pts',(18.3,49.2671214282513,2.37394276112318));
#72889=CARTESIAN_POINT('Ctrl Pts',(18.1272,49.2671214282513,2.37394276112318));
#72890=CARTESIAN_POINT('Ctrl Pts',(18.3,49.1727148234844,2.489085970819));
#72891=CARTESIAN_POINT('Ctrl Pts',(18.1272,49.1727148234844,2.489085970819));
#72892=CARTESIAN_POINT('Ctrl Pts',(18.3,49.1727148234844,2.66480210274458));
#72893=CARTESIAN_POINT('Ctrl Pts',(18.1272,49.1727148234844,2.66480210274458));
#72894=CARTESIAN_POINT('',(18.3,49.2671214282513,2.37394276112318));
#72895=CARTESIAN_POINT('Ctrl Pts',(18.3,49.2671214282513,2.37394276112318));
#72896=CARTESIAN_POINT('Ctrl Pts',(18.3,49.1727148234844,2.489085970819));
#72897=CARTESIAN_POINT('Ctrl Pts',(18.3,49.1727148234844,2.66480210274458));
#72898=CARTESIAN_POINT('',(18.18,49.2671214282513,2.37394276112318));
#72899=CARTESIAN_POINT('',(18.3,49.2671214282513,2.37394276112318));
#72900=CARTESIAN_POINT('Ctrl Pts',(18.18,49.2671214282513,2.37394276112318));
#72901=CARTESIAN_POINT('Ctrl Pts',(18.18,49.1727148234844,2.489085970819));
#72902=CARTESIAN_POINT('Ctrl Pts',(18.18,49.1727148234844,2.66480210274458));
#72903=CARTESIAN_POINT('Ctrl Pts',(18.3,49.5345156133175,2.20095503181219));
#72904=CARTESIAN_POINT('Ctrl Pts',(18.1272,49.5345156133175,2.20095503181219));
#72905=CARTESIAN_POINT('Ctrl Pts',(18.3,49.3615280330181,2.25879940241575));
#72906=CARTESIAN_POINT('Ctrl Pts',(18.1272,49.3615280330181,2.25879940241575));
#72907=CARTESIAN_POINT('Ctrl Pts',(18.3,49.2671214282513,2.37394276112318));
#72908=CARTESIAN_POINT('Ctrl Pts',(18.1272,49.2671214282513,2.37394276112318));
#72909=CARTESIAN_POINT('',(18.3,49.5345156133175,2.20095503181219));
#72910=CARTESIAN_POINT('Ctrl Pts',(18.3,49.5345156133175,2.20095503181219));
#72911=CARTESIAN_POINT('Ctrl Pts',(18.3,49.3615280330181,2.25879940241575));
#72912=CARTESIAN_POINT('Ctrl Pts',(18.3,49.2671214282513,2.37394276112318));
#72913=CARTESIAN_POINT('',(18.18,49.5345156133175,2.20095503181219));
#72914=CARTESIAN_POINT('',(18.3,49.5345156133175,2.20095503181219));
#72915=CARTESIAN_POINT('Ctrl Pts',(18.18,49.5345156133175,2.20095503181219));
#72916=CARTESIAN_POINT('Ctrl Pts',(18.18,49.3615280330181,2.25879940241575));
#72917=CARTESIAN_POINT('Ctrl Pts',(18.18,49.2671214282513,2.37394276112318));
#72918=CARTESIAN_POINT('Ctrl Pts',(18.3,49.9890859663486,2.14311051219702));
#72919=CARTESIAN_POINT('Ctrl Pts',(18.1272,49.9890859663486,2.14311051219702));
#72920=CARTESIAN_POINT('Ctrl Pts',(18.3,49.7075034916401,2.14311051219702));
#72921=CARTESIAN_POINT('Ctrl Pts',(18.1272,49.7075034916401,2.14311051219702));
#72922=CARTESIAN_POINT('Ctrl Pts',(18.3,49.5345156133175,2.20095503181219));
#72923=CARTESIAN_POINT('Ctrl Pts',(18.1272,49.5345156133175,2.20095503181219));
#72924=CARTESIAN_POINT('',(18.3,49.9890859663486,2.14311051219702));
#72925=CARTESIAN_POINT('Ctrl Pts',(18.3,49.9890859663486,2.14311051219702));
#72926=CARTESIAN_POINT('Ctrl Pts',(18.3,49.7075034916401,2.14311051219702));
#72927=CARTESIAN_POINT('Ctrl Pts',(18.3,49.5345156133175,2.20095503181219));
#72928=CARTESIAN_POINT('',(18.18,49.9890859663486,2.14311051219702));
#72929=CARTESIAN_POINT('',(18.3,49.9890859663486,2.14311051219702));
#72930=CARTESIAN_POINT('Ctrl Pts',(18.18,49.9890859663486,2.14311051219702));
#72931=CARTESIAN_POINT('Ctrl Pts',(18.18,49.7075034916401,2.14311051219702));
#72932=CARTESIAN_POINT('Ctrl Pts',(18.18,49.5345156133175,2.20095503181219));
#72933=CARTESIAN_POINT('Ctrl Pts',(18.3,50.3672577679157,2.17912691682577));
#72934=CARTESIAN_POINT('Ctrl Pts',(18.1272,50.3672577679157,2.17912691682577));
#72935=CARTESIAN_POINT('Ctrl Pts',(18.3,50.2270122110844,2.14311051219702));
#72936=CARTESIAN_POINT('Ctrl Pts',(18.1272,50.2270122110844,2.14311051219702));
#72937=CARTESIAN_POINT('Ctrl Pts',(18.3,49.9890859663486,2.14311051219702));
#72938=CARTESIAN_POINT('Ctrl Pts',(18.1272,49.9890859663486,2.14311051219702));
#72939=CARTESIAN_POINT('',(18.3,50.3672577679157,2.17912691682577));
#72940=CARTESIAN_POINT('Ctrl Pts',(18.3,50.3672577679157,2.17912691682577));
#72941=CARTESIAN_POINT('Ctrl Pts',(18.3,50.2270122110844,2.14311051219702));
#72942=CARTESIAN_POINT('Ctrl Pts',(18.3,49.9890859663486,2.14311051219702));
#72943=CARTESIAN_POINT('',(18.18,50.3672577679157,2.17912691682577));
#72944=CARTESIAN_POINT('',(18.3,50.3672577679157,2.17912691682577));
#72945=CARTESIAN_POINT('Ctrl Pts',(18.18,50.3672577679157,2.17912691682577));
#72946=CARTESIAN_POINT('Ctrl Pts',(18.18,50.2270122110844,2.14311051219702));
#72947=CARTESIAN_POINT('Ctrl Pts',(18.18,49.9890859663486,2.14311051219702));
#72948=CARTESIAN_POINT('Ctrl Pts',(18.3,50.605184161663,2.2784447953105));
#72949=CARTESIAN_POINT('Ctrl Pts',(18.1272,50.605184161663,2.2784447953105));
#72950=CARTESIAN_POINT('Ctrl Pts',(18.3,50.5075034737587,2.21514317244291));
#72951=CARTESIAN_POINT('Ctrl Pts',(18.1272,50.5075034737587,2.21514317244291));
#72952=CARTESIAN_POINT('Ctrl Pts',(18.3,50.3672577679157,2.17912691682577));
#72953=CARTESIAN_POINT('Ctrl Pts',(18.1272,50.3672577679157,2.17912691682577));
#72954=CARTESIAN_POINT('',(18.3,50.605184161663,2.2784447953105));
#72955=CARTESIAN_POINT('Ctrl Pts',(18.3,50.605184161663,2.2784447953105));
#72956=CARTESIAN_POINT('Ctrl Pts',(18.3,50.5075034737587,2.21514317244291));
#72957=CARTESIAN_POINT('Ctrl Pts',(18.3,50.3672577679157,2.17912691682577));
#72958=CARTESIAN_POINT('',(18.18,50.605184161663,2.2784447953105));
#72959=CARTESIAN_POINT('',(18.3,50.605184161663,2.2784447953105));
#72960=CARTESIAN_POINT('Ctrl Pts',(18.18,50.605184161663,2.2784447953105));
#72961=CARTESIAN_POINT('Ctrl Pts',(18.18,50.5075034737587,2.21514317244291));
#72962=CARTESIAN_POINT('Ctrl Pts',(18.18,50.3672577679157,2.17912691682577));
#72963=CARTESIAN_POINT('Ctrl Pts',(18.3,50.7547067344189,2.43888142555952));
#72964=CARTESIAN_POINT('Ctrl Pts',(18.1272,50.7547067344189,2.43888142555952));
#72965=CARTESIAN_POINT('Ctrl Pts',(18.3,50.702864998579,2.34174626916647));
#72966=CARTESIAN_POINT('Ctrl Pts',(18.1272,50.702864998579,2.34174626916647));
#72967=CARTESIAN_POINT('Ctrl Pts',(18.3,50.605184161663,2.2784447953105));
#72968=CARTESIAN_POINT('Ctrl Pts',(18.1272,50.605184161663,2.2784447953105));
#72969=CARTESIAN_POINT('',(18.3,50.7547067344189,2.43888142555952));
#72970=CARTESIAN_POINT('Ctrl Pts',(18.3,50.7547067344189,2.43888142555952));
#72971=CARTESIAN_POINT('Ctrl Pts',(18.3,50.702864998579,2.34174626916647));
#72972=CARTESIAN_POINT('Ctrl Pts',(18.3,50.605184161663,2.2784447953105));
#72973=CARTESIAN_POINT('',(18.18,50.7547067344189,2.43888142555952));
#72974=CARTESIAN_POINT('',(18.3,50.7547067344189,2.43888142555952));
#72975=CARTESIAN_POINT('Ctrl Pts',(18.18,50.7547067344189,2.43888142555952));
#72976=CARTESIAN_POINT('Ctrl Pts',(18.18,50.702864998579,2.34174626916647));
#72977=CARTESIAN_POINT('Ctrl Pts',(18.18,50.605184161663,2.2784447953105));
#72978=CARTESIAN_POINT('Ctrl Pts',(18.3,50.8065484702587,2.66480210274458));
#72979=CARTESIAN_POINT('Ctrl Pts',(18.1272,50.8065484702587,2.66480210274458));
#72980=CARTESIAN_POINT('Ctrl Pts',(18.3,50.8065484702587,2.53601643294096));
#72981=CARTESIAN_POINT('Ctrl Pts',(18.1272,50.8065484702587,2.53601643294096));
#72982=CARTESIAN_POINT('Ctrl Pts',(18.3,50.7547067344189,2.43888142555952));
#72983=CARTESIAN_POINT('Ctrl Pts',(18.1272,50.7547067344189,2.43888142555952));
#72984=CARTESIAN_POINT('',(18.3,50.8065484702587,2.66480210274458));
#72985=CARTESIAN_POINT('Ctrl Pts',(18.3,50.8065484702587,2.66480210274458));
#72986=CARTESIAN_POINT('Ctrl Pts',(18.3,50.8065484702587,2.53601643294096));
#72987=CARTESIAN_POINT('Ctrl Pts',(18.3,50.7547067344189,2.43888142555952));
#72988=CARTESIAN_POINT('',(18.18,50.8065484702587,2.66480210274458));
#72989=CARTESIAN_POINT('',(18.3,50.8065484702587,2.66480210274458));
#72990=CARTESIAN_POINT('Ctrl Pts',(18.18,50.8065484702587,2.66480210274458));
#72991=CARTESIAN_POINT('Ctrl Pts',(18.18,50.8065484702587,2.53601643294096));
#72992=CARTESIAN_POINT('Ctrl Pts',(18.18,50.7547067344189,2.43888142555952));
#72993=CARTESIAN_POINT('Ctrl Pts',(18.3,50.7126876950264,2.95457023233175));
#72994=CARTESIAN_POINT('Ctrl Pts',(18.1272,50.7126876950264,2.95457023233175));
#72995=CARTESIAN_POINT('Ctrl Pts',(18.3,50.8065484702587,2.83942702263594));
#72996=CARTESIAN_POINT('Ctrl Pts',(18.1272,50.8065484702587,2.83942702263594));
#72997=CARTESIAN_POINT('Ctrl Pts',(18.3,50.8065484702587,2.66480210274458));
#72998=CARTESIAN_POINT('Ctrl Pts',(18.1272,50.8065484702587,2.66480210274458));
#72999=CARTESIAN_POINT('',(18.3,50.7126876950264,2.95457023233175));
#73000=CARTESIAN_POINT('Ctrl Pts',(18.3,50.7126876950264,2.95457023233175));
#73001=CARTESIAN_POINT('Ctrl Pts',(18.3,50.8065484702587,2.83942702263594));
#73002=CARTESIAN_POINT('Ctrl Pts',(18.3,50.8065484702587,2.66480210274458));
#73003=CARTESIAN_POINT('',(18.18,50.7126876950264,2.95457023233175));
#73004=CARTESIAN_POINT('',(18.3,50.7126876950264,2.95457023233175));
#73005=CARTESIAN_POINT('Ctrl Pts',(18.18,50.7126876950264,2.95457023233175));
#73006=CARTESIAN_POINT('Ctrl Pts',(18.18,50.8065484702587,2.83942702263594));
#73007=CARTESIAN_POINT('Ctrl Pts',(18.18,50.8065484702587,2.66480210274458));
#73008=CARTESIAN_POINT('Ctrl Pts',(18.3,50.4458390414715,3.12810364216566));
#73009=CARTESIAN_POINT('Ctrl Pts',(18.1272,50.4458390414715,3.12810364216566));
#73010=CARTESIAN_POINT('Ctrl Pts',(18.3,50.6188267707825,3.06971344202757));
#73011=CARTESIAN_POINT('Ctrl Pts',(18.1272,50.6188267707825,3.06971344202757));
#73012=CARTESIAN_POINT('Ctrl Pts',(18.3,50.7126876950264,2.95457023233175));
#73013=CARTESIAN_POINT('Ctrl Pts',(18.1272,50.7126876950264,2.95457023233175));
#73014=CARTESIAN_POINT('',(18.3,50.4458390414715,3.12810364216566));
#73015=CARTESIAN_POINT('Ctrl Pts',(18.3,50.4458390414715,3.12810364216566));
#73016=CARTESIAN_POINT('Ctrl Pts',(18.3,50.6188267707825,3.06971344202757));
#73017=CARTESIAN_POINT('Ctrl Pts',(18.3,50.7126876950264,2.95457023233175));
#73018=CARTESIAN_POINT('',(18.18,50.4458390414715,3.12810364216566));
#73019=CARTESIAN_POINT('',(18.3,50.4458390414715,3.12810364216566));
#73020=CARTESIAN_POINT('Ctrl Pts',(18.18,50.4458390414715,3.12810364216566));
#73021=CARTESIAN_POINT('Ctrl Pts',(18.18,50.6188267707825,3.06971344202757));
#73022=CARTESIAN_POINT('Ctrl Pts',(18.18,50.7126876950264,2.95457023233175));
#73023=CARTESIAN_POINT('Ctrl Pts',(18.3,49.9890859663486,3.18649384230375));
#73024=CARTESIAN_POINT('Ctrl Pts',(18.1272,49.9890859663486,3.18649384230375));
#73025=CARTESIAN_POINT('Ctrl Pts',(18.3,50.2728513121605,3.18649384230375));
#73026=CARTESIAN_POINT('Ctrl Pts',(18.1272,50.2728513121605,3.18649384230375));
#73027=CARTESIAN_POINT('Ctrl Pts',(18.3,50.4458390414715,3.12810364216566));
#73028=CARTESIAN_POINT('Ctrl Pts',(18.1272,50.4458390414715,3.12810364216566));
#73029=CARTESIAN_POINT('',(18.3,49.9890859663486,3.18649384230375));
#73030=CARTESIAN_POINT('Ctrl Pts',(18.3,49.9890859663486,3.18649384230375));
#73031=CARTESIAN_POINT('Ctrl Pts',(18.3,50.2728513121605,3.18649384230375));
#73032=CARTESIAN_POINT('Ctrl Pts',(18.3,50.4458390414715,3.12810364216566));
#73033=CARTESIAN_POINT('',(18.18,49.9890859663486,3.18649384230375));
#73034=CARTESIAN_POINT('',(18.3,49.9890859663486,3.18649384230375));
#73035=CARTESIAN_POINT('Ctrl Pts',(18.18,49.9890859663486,3.18649384230375));
#73036=CARTESIAN_POINT('Ctrl Pts',(18.18,50.2728513121605,3.18649384230375));
#73037=CARTESIAN_POINT('Ctrl Pts',(18.18,50.4458390414715,3.12810364216566));
#73038=CARTESIAN_POINT('Ctrl Pts',(18.3,49.3386085569858,3.02824008315802));
#73039=CARTESIAN_POINT('Ctrl Pts',(18.1272,49.3386085569858,3.02824008315802));
#73040=CARTESIAN_POINT('Ctrl Pts',(18.3,49.5383356750011,3.18649384230375));
#73041=CARTESIAN_POINT('Ctrl Pts',(18.1272,49.5383356750011,3.18649384230375));
#73042=CARTESIAN_POINT('Ctrl Pts',(18.3,49.9890859663486,3.18649384230375));
#73043=CARTESIAN_POINT('Ctrl Pts',(18.1272,49.9890859663486,3.18649384230375));
#73044=CARTESIAN_POINT('Ctrl Pts',(18.3,49.3386085569858,3.02824008315802));
#73045=CARTESIAN_POINT('Ctrl Pts',(18.3,49.5383356750011,3.18649384230375));
#73046=CARTESIAN_POINT('Ctrl Pts',(18.3,49.9890859663486,3.18649384230375));
#73047=CARTESIAN_POINT('Ctrl Pts',(18.18,49.3386085569858,3.02824008315802));
#73048=CARTESIAN_POINT('Ctrl Pts',(18.18,49.5383356750011,3.18649384230375));
#73049=CARTESIAN_POINT('Ctrl Pts',(18.18,49.9890859663486,3.18649384230375));
#73050=CARTESIAN_POINT('Origin',(18.18,49.9896316468716,3.29999995455146));
#73051=CARTESIAN_POINT('Ctrl Pts',(18.3,49.4952251255512,4.09890851974487));
#73052=CARTESIAN_POINT('Ctrl Pts',(18.1272,49.4952251255512,4.09890851974487));
#73053=CARTESIAN_POINT('Ctrl Pts',(18.3,49.4422920286655,4.14911313951015));
#73054=CARTESIAN_POINT('Ctrl Pts',(18.1272,49.4422920286655,4.14911313951015));
#73055=CARTESIAN_POINT('Ctrl Pts',(18.3,49.3888132512569,4.18185527473688));
#73056=CARTESIAN_POINT('Ctrl Pts',(18.1272,49.3888132512569,4.18185527473688));
#73057=CARTESIAN_POINT('',(18.3,49.4952251255512,4.09890851974487));
#73058=CARTESIAN_POINT('',(18.3,49.3888132512569,4.18185527473688));
#73059=CARTESIAN_POINT('Ctrl Pts',(18.3,49.4952251255512,4.09890851974487));
#73060=CARTESIAN_POINT('Ctrl Pts',(18.3,49.4422920286655,4.14911313951015));
#73061=CARTESIAN_POINT('Ctrl Pts',(18.3,49.3888132512569,4.18185527473688));
#73062=CARTESIAN_POINT('',(18.18,49.4952251255512,4.09890851974487));
#73063=CARTESIAN_POINT('',(18.3,49.4952251255512,4.09890851974487));
#73064=CARTESIAN_POINT('',(18.18,49.3888132512569,4.18185527473688));
#73065=CARTESIAN_POINT('Ctrl Pts',(18.18,49.4952251255512,4.09890851974487));
#73066=CARTESIAN_POINT('Ctrl Pts',(18.18,49.4422920286655,4.14911313951015));
#73067=CARTESIAN_POINT('Ctrl Pts',(18.18,49.3888132512569,4.18185527473688));
#73068=CARTESIAN_POINT('',(18.3,49.3888132512569,4.18185527473688));
#73069=CARTESIAN_POINT('Ctrl Pts',(18.3,49.6965892851353,3.87189629524946));
#73070=CARTESIAN_POINT('Ctrl Pts',(18.1272,49.6965892851353,3.87189629524946));
#73071=CARTESIAN_POINT('Ctrl Pts',(18.3,49.5481582224369,4.04870386272669));
#73072=CARTESIAN_POINT('Ctrl Pts',(18.1272,49.5481582224369,4.04870386272669));
#73073=CARTESIAN_POINT('Ctrl Pts',(18.3,49.4952251255512,4.09890851974487));
#73074=CARTESIAN_POINT('Ctrl Pts',(18.1272,49.4952251255512,4.09890851974487));
#73075=CARTESIAN_POINT('',(18.3,49.6965892851353,3.87189629524946));
#73076=CARTESIAN_POINT('Ctrl Pts',(18.3,49.6965892851353,3.87189629524946));
#73077=CARTESIAN_POINT('Ctrl Pts',(18.3,49.5481582224369,4.04870386272669));
#73078=CARTESIAN_POINT('Ctrl Pts',(18.3,49.4952251255512,4.09890851974487));
#73079=CARTESIAN_POINT('',(18.18,49.6965892851353,3.87189629524946));
#73080=CARTESIAN_POINT('',(18.3,49.6965892851353,3.87189629524946));
#73081=CARTESIAN_POINT('Ctrl Pts',(18.18,49.6965892851353,3.87189629524946));
#73082=CARTESIAN_POINT('Ctrl Pts',(18.18,49.5481582224369,4.04870386272669));
#73083=CARTESIAN_POINT('Ctrl Pts',(18.18,49.4952251255512,4.09890851974487));
#73084=CARTESIAN_POINT('Ctrl Pts',(18.3,49.978172057867,3.5690313860774));
#73085=CARTESIAN_POINT('Ctrl Pts',(18.1272,49.978172057867,3.5690313860774));
#73086=CARTESIAN_POINT('Ctrl Pts',(18.3,49.8755799472332,3.66016360968351));
#73087=CARTESIAN_POINT('Ctrl Pts',(18.1272,49.8755799472332,3.66016360968351));
#73088=CARTESIAN_POINT('Ctrl Pts',(18.3,49.6965892851353,3.87189629524946));
#73089=CARTESIAN_POINT('Ctrl Pts',(18.1272,49.6965892851353,3.87189629524946));
#73090=CARTESIAN_POINT('',(18.3,49.978172057867,3.5690313860774));
#73091=CARTESIAN_POINT('Ctrl Pts',(18.3,49.978172057867,3.5690313860774));
#73092=CARTESIAN_POINT('Ctrl Pts',(18.3,49.8755799472332,3.66016360968351));
#73093=CARTESIAN_POINT('Ctrl Pts',(18.3,49.6965892851353,3.87189629524946));
#73094=CARTESIAN_POINT('',(18.18,49.978172057867,3.5690313860774));
#73095=CARTESIAN_POINT('',(18.3,49.978172057867,3.5690313860774));
#73096=CARTESIAN_POINT('Ctrl Pts',(18.18,49.978172057867,3.5690313860774));
#73097=CARTESIAN_POINT('Ctrl Pts',(18.18,49.8755799472332,3.66016360968351));
#73098=CARTESIAN_POINT('Ctrl Pts',(18.18,49.6965892851353,3.87189629524946));
#73099=CARTESIAN_POINT('Ctrl Pts',(18.3,50.1735334336758,3.4386083766818));
#73100=CARTESIAN_POINT('Ctrl Pts',(18.1272,50.1735334336758,3.4386083766818));
#73101=CARTESIAN_POINT('Ctrl Pts',(18.3,50.0807640194893,3.47789901345968));
#73102=CARTESIAN_POINT('Ctrl Pts',(18.1272,50.0807640194893,3.47789901345968));
#73103=CARTESIAN_POINT('Ctrl Pts',(18.3,49.978172057867,3.5690313860774));
#73104=CARTESIAN_POINT('Ctrl Pts',(18.1272,49.978172057867,3.5690313860774));
#73105=CARTESIAN_POINT('',(18.3,50.1735334336758,3.4386083766818));
#73106=CARTESIAN_POINT('Ctrl Pts',(18.3,50.1735334336758,3.4386083766818));
#73107=CARTESIAN_POINT('Ctrl Pts',(18.3,50.0807640194893,3.47789901345968));
#73108=CARTESIAN_POINT('Ctrl Pts',(18.3,49.978172057867,3.5690313860774));
#73109=CARTESIAN_POINT('',(18.18,50.1735334336758,3.4386083766818));
#73110=CARTESIAN_POINT('',(18.3,50.1735334336758,3.4386083766818));
#73111=CARTESIAN_POINT('Ctrl Pts',(18.18,50.1735334336758,3.4386083766818));
#73112=CARTESIAN_POINT('Ctrl Pts',(18.18,50.0807640194893,3.47789901345968));
#73113=CARTESIAN_POINT('Ctrl Pts',(18.18,49.978172057867,3.5690313860774));
#73114=CARTESIAN_POINT('Ctrl Pts',(18.3,50.3623466432094,3.39931788891554));
#73115=CARTESIAN_POINT('Ctrl Pts',(18.1272,50.3623466432094,3.39931788891554));
#73116=CARTESIAN_POINT('Ctrl Pts',(18.3,50.2663029968738,3.39931788891554));
#73117=CARTESIAN_POINT('Ctrl Pts',(18.1272,50.2663029968738,3.39931788891554));
#73118=CARTESIAN_POINT('Ctrl Pts',(18.3,50.1735334336758,3.4386083766818));
#73119=CARTESIAN_POINT('Ctrl Pts',(18.1272,50.1735334336758,3.4386083766818));
#73120=CARTESIAN_POINT('',(18.3,50.3623466432094,3.39931788891554));
#73121=CARTESIAN_POINT('Ctrl Pts',(18.3,50.3623466432094,3.39931788891554));
#73122=CARTESIAN_POINT('Ctrl Pts',(18.3,50.2663029968738,3.39931788891554));
#73123=CARTESIAN_POINT('Ctrl Pts',(18.3,50.1735334336758,3.4386083766818));
#73124=CARTESIAN_POINT('',(18.18,50.3623466432094,3.39931788891554));
#73125=CARTESIAN_POINT('',(18.3,50.3623466432094,3.39931788891554));
#73126=CARTESIAN_POINT('Ctrl Pts',(18.18,50.3623466432094,3.39931788891554));
#73127=CARTESIAN_POINT('Ctrl Pts',(18.18,50.2663029968738,3.39931788891554));
#73128=CARTESIAN_POINT('Ctrl Pts',(18.18,50.1735334336758,3.4386083766818));
#73129=CARTESIAN_POINT('Ctrl Pts',(18.3,50.6788541615009,3.53356066197157));
#73130=CARTESIAN_POINT('Ctrl Pts',(18.1272,50.6788541615009,3.53356066197157));
#73131=CARTESIAN_POINT('Ctrl Pts',(18.3,50.5511597037315,3.39931788891554));
#73132=CARTESIAN_POINT('Ctrl Pts',(18.1272,50.5511597037315,3.39931788891554));
#73133=CARTESIAN_POINT('Ctrl Pts',(18.3,50.3623466432094,3.39931788891554));
#73134=CARTESIAN_POINT('Ctrl Pts',(18.1272,50.3623466432094,3.39931788891554));
#73135=CARTESIAN_POINT('',(18.3,50.6788541615009,3.53356066197157));
#73136=CARTESIAN_POINT('Ctrl Pts',(18.3,50.6788541615009,3.53356066197157));
#73137=CARTESIAN_POINT('Ctrl Pts',(18.3,50.5511597037315,3.39931788891554));
#73138=CARTESIAN_POINT('Ctrl Pts',(18.3,50.3623466432094,3.39931788891554));
#73139=CARTESIAN_POINT('',(18.18,50.6788541615009,3.53356066197157));
#73140=CARTESIAN_POINT('',(18.3,50.6788541615009,3.53356066197157));
#73141=CARTESIAN_POINT('Ctrl Pts',(18.18,50.6788541615009,3.53356066197157));
#73142=CARTESIAN_POINT('Ctrl Pts',(18.18,50.5511597037315,3.39931788891554));
#73143=CARTESIAN_POINT('Ctrl Pts',(18.18,50.3623466432094,3.39931788891554));
#73144=CARTESIAN_POINT('Ctrl Pts',(18.3,50.8065484702587,3.89809000343084));
#73145=CARTESIAN_POINT('Ctrl Pts',(18.1272,50.8065484702587,3.89809000343084));
#73146=CARTESIAN_POINT('Ctrl Pts',(18.3,50.8065484702587,3.6678034350276));
#73147=CARTESIAN_POINT('Ctrl Pts',(18.1272,50.8065484702587,3.6678034350276));
#73148=CARTESIAN_POINT('Ctrl Pts',(18.3,50.6788541615009,3.53356066197157));
#73149=CARTESIAN_POINT('Ctrl Pts',(18.1272,50.6788541615009,3.53356066197157));
#73150=CARTESIAN_POINT('',(18.3,50.8065484702587,3.89809000343084));
#73151=CARTESIAN_POINT('Ctrl Pts',(18.3,50.8065484702587,3.89809000343084));
#73152=CARTESIAN_POINT('Ctrl Pts',(18.3,50.8065484702587,3.6678034350276));
#73153=CARTESIAN_POINT('Ctrl Pts',(18.3,50.6788541615009,3.53356066197157));
#73154=CARTESIAN_POINT('',(18.18,50.8065484702587,3.89809000343084));
#73155=CARTESIAN_POINT('',(18.3,50.8065484702587,3.89809000343084));
#73156=CARTESIAN_POINT('Ctrl Pts',(18.18,50.8065484702587,3.89809000343084));
#73157=CARTESIAN_POINT('Ctrl Pts',(18.18,50.8065484702587,3.6678034350276));
#73158=CARTESIAN_POINT('Ctrl Pts',(18.18,50.6788541615009,3.53356066197157));
#73159=CARTESIAN_POINT('Ctrl Pts',(18.3,50.6881310284138,4.26152787208557));
#73160=CARTESIAN_POINT('Ctrl Pts',(18.1272,50.6881310284138,4.26152787208557));
#73161=CARTESIAN_POINT('Ctrl Pts',(18.3,50.8065484702587,4.12619362622499));
#73162=CARTESIAN_POINT('Ctrl Pts',(18.1272,50.8065484702587,4.12619362622499));
#73163=CARTESIAN_POINT('Ctrl Pts',(18.3,50.8065484702587,3.89809000343084));
#73164=CARTESIAN_POINT('Ctrl Pts',(18.1272,50.8065484702587,3.89809000343084));
#73165=CARTESIAN_POINT('',(18.3,50.6881310284138,4.26152787208557));
#73166=CARTESIAN_POINT('Ctrl Pts',(18.3,50.6881310284138,4.26152787208557));
#73167=CARTESIAN_POINT('Ctrl Pts',(18.3,50.8065484702587,4.12619362622499));
#73168=CARTESIAN_POINT('Ctrl Pts',(18.3,50.8065484702587,3.89809000343084));
#73169=CARTESIAN_POINT('',(18.18,50.6881310284138,4.26152787208557));
#73170=CARTESIAN_POINT('',(18.3,50.6881310284138,4.26152787208557));
#73171=CARTESIAN_POINT('Ctrl Pts',(18.18,50.6881310284138,4.26152787208557));
#73172=CARTESIAN_POINT('Ctrl Pts',(18.18,50.8065484702587,4.12619362622499));
#73173=CARTESIAN_POINT('Ctrl Pts',(18.18,50.8065484702587,3.89809000343084));
#73174=CARTESIAN_POINT('Ctrl Pts',(18.3,50.3437926113605,4.41759881600738));
#73175=CARTESIAN_POINT('Ctrl Pts',(18.1272,50.3437926113605,4.41759881600738));
#73176=CARTESIAN_POINT('Ctrl Pts',(18.3,50.5697135865688,4.39686211794615));
#73177=CARTESIAN_POINT('Ctrl Pts',(18.1272,50.5697135865688,4.39686211794615));
#73178=CARTESIAN_POINT('Ctrl Pts',(18.3,50.6881310284138,4.26152787208557));
#73179=CARTESIAN_POINT('Ctrl Pts',(18.1272,50.6881310284138,4.26152787208557));
#73180=CARTESIAN_POINT('',(18.3,50.3437926113605,4.41759881600738));
#73181=CARTESIAN_POINT('Ctrl Pts',(18.3,50.3437926113605,4.41759881600738));
#73182=CARTESIAN_POINT('Ctrl Pts',(18.3,50.5697135865688,4.39686211794615));
#73183=CARTESIAN_POINT('Ctrl Pts',(18.3,50.6881310284138,4.26152787208557));
#73184=CARTESIAN_POINT('',(18.18,50.3437926113605,4.41759881600738));
#73185=CARTESIAN_POINT('',(18.3,50.3437926113605,4.41759881600738));
#73186=CARTESIAN_POINT('Ctrl Pts',(18.18,50.3437926113605,4.41759881600738));
#73187=CARTESIAN_POINT('Ctrl Pts',(18.18,50.5697135865688,4.39686211794615));
#73188=CARTESIAN_POINT('Ctrl Pts',(18.18,50.6881310284138,4.26152787208557));
#73189=CARTESIAN_POINT('Origin',(18.3,50.3230560064316,4.21568888276815));
#73190=CARTESIAN_POINT('',(18.3,50.3230560064316,4.21568888276815));
#73191=CARTESIAN_POINT('',(18.3,50.4910090704177,5.85102851782062));
#73192=CARTESIAN_POINT('',(18.18,50.3230560064316,4.21568888276815));
#73193=CARTESIAN_POINT('',(18.3,50.3230560064316,4.21568888276815));
#73194=CARTESIAN_POINT('',(18.18,50.3230560064316,4.21568888276815));
#73195=CARTESIAN_POINT('Ctrl Pts',(18.3,50.5587995290756,4.12946785837412));
#73196=CARTESIAN_POINT('Ctrl Pts',(18.1272,50.5587995290756,4.12946785837412));
#73197=CARTESIAN_POINT('Ctrl Pts',(18.3,50.4736699402332,4.21459744721651));
#73198=CARTESIAN_POINT('Ctrl Pts',(18.1272,50.4736699402332,4.21459744721651));
#73199=CARTESIAN_POINT('Ctrl Pts',(18.3,50.3230560064316,4.21568888276815));
#73200=CARTESIAN_POINT('Ctrl Pts',(18.1272,50.3230560064316,4.21568888276815));
#73201=CARTESIAN_POINT('',(18.3,50.5587995290756,4.12946785837412));
#73202=CARTESIAN_POINT('Ctrl Pts',(18.3,50.5587995290756,4.12946785837412));
#73203=CARTESIAN_POINT('Ctrl Pts',(18.3,50.4736699402332,4.21459744721651));
#73204=CARTESIAN_POINT('Ctrl Pts',(18.3,50.3230560064316,4.21568888276815));
#73205=CARTESIAN_POINT('',(18.18,50.5587995290756,4.12946785837412));
#73206=CARTESIAN_POINT('',(18.3,50.5587995290756,4.12946785837412));
#73207=CARTESIAN_POINT('Ctrl Pts',(18.18,50.5587995290756,4.12946785837412));
#73208=CARTESIAN_POINT('Ctrl Pts',(18.18,50.4736699402332,4.21459744721651));
#73209=CARTESIAN_POINT('Ctrl Pts',(18.18,50.3230560064316,4.21568888276815));
#73210=CARTESIAN_POINT('Ctrl Pts',(18.3,50.643929117918,3.9024555966258));
#73211=CARTESIAN_POINT('Ctrl Pts',(18.1272,50.643929117918,3.9024555966258));
#73212=CARTESIAN_POINT('Ctrl Pts',(18.3,50.643929117918,4.04433826953173));
#73213=CARTESIAN_POINT('Ctrl Pts',(18.1272,50.643929117918,4.04433826953173));
#73214=CARTESIAN_POINT('Ctrl Pts',(18.3,50.5587995290756,4.12946785837412));
#73215=CARTESIAN_POINT('Ctrl Pts',(18.1272,50.5587995290756,4.12946785837412));
#73216=CARTESIAN_POINT('',(18.3,50.643929117918,3.9024555966258));
#73217=CARTESIAN_POINT('Ctrl Pts',(18.3,50.643929117918,3.9024555966258));
#73218=CARTESIAN_POINT('Ctrl Pts',(18.3,50.643929117918,4.04433826953173));
#73219=CARTESIAN_POINT('Ctrl Pts',(18.3,50.5587995290756,4.12946785837412));
#73220=CARTESIAN_POINT('',(18.18,50.643929117918,3.9024555966258));
#73221=CARTESIAN_POINT('',(18.3,50.643929117918,3.9024555966258));
#73222=CARTESIAN_POINT('Ctrl Pts',(18.18,50.643929117918,3.9024555966258));
#73223=CARTESIAN_POINT('Ctrl Pts',(18.18,50.643929117918,4.04433826953173));
#73224=CARTESIAN_POINT('Ctrl Pts',(18.18,50.5587995290756,4.12946785837412));
#73225=CARTESIAN_POINT('Ctrl Pts',(18.3,50.5637108027935,3.68472027629614));
#73226=CARTESIAN_POINT('Ctrl Pts',(18.1272,50.5637108027935,3.68472027629614));
#73227=CARTESIAN_POINT('Ctrl Pts',(18.3,50.643929117918,3.76821282356977));
#73228=CARTESIAN_POINT('Ctrl Pts',(18.1272,50.643929117918,3.76821282356977));
#73229=CARTESIAN_POINT('Ctrl Pts',(18.3,50.643929117918,3.9024555966258));
#73230=CARTESIAN_POINT('Ctrl Pts',(18.1272,50.643929117918,3.9024555966258));
#73231=CARTESIAN_POINT('',(18.3,50.5637108027935,3.68472027629614));
#73232=CARTESIAN_POINT('Ctrl Pts',(18.3,50.5637108027935,3.68472027629614));
#73233=CARTESIAN_POINT('Ctrl Pts',(18.3,50.643929117918,3.76821282356977));
#73234=CARTESIAN_POINT('Ctrl Pts',(18.3,50.643929117918,3.9024555966258));
#73235=CARTESIAN_POINT('',(18.18,50.5637108027935,3.68472027629614));
#73236=CARTESIAN_POINT('',(18.3,50.5637108027935,3.68472027629614));
#73237=CARTESIAN_POINT('Ctrl Pts',(18.18,50.5637108027935,3.68472027629614));
#73238=CARTESIAN_POINT('Ctrl Pts',(18.18,50.643929117918,3.76821282356977));
#73239=CARTESIAN_POINT('Ctrl Pts',(18.18,50.643929117918,3.9024555966258));
#73240=CARTESIAN_POINT('Ctrl Pts',(18.3,50.3667122364044,3.6012277290225));
#73241=CARTESIAN_POINT('Ctrl Pts',(18.1272,50.3667122364044,3.6012277290225));
#73242=CARTESIAN_POINT('Ctrl Pts',(18.3,50.4834926366806,3.6012277290225));
#73243=CARTESIAN_POINT('Ctrl Pts',(18.1272,50.4834926366806,3.6012277290225));
#73244=CARTESIAN_POINT('Ctrl Pts',(18.3,50.5637108027935,3.68472027629614));
#73245=CARTESIAN_POINT('Ctrl Pts',(18.1272,50.5637108027935,3.68472027629614));
#73246=CARTESIAN_POINT('',(18.3,50.3667122364044,3.6012277290225));
#73247=CARTESIAN_POINT('Ctrl Pts',(18.3,50.3667122364044,3.6012277290225));
#73248=CARTESIAN_POINT('Ctrl Pts',(18.3,50.4834926366806,3.6012277290225));
#73249=CARTESIAN_POINT('Ctrl Pts',(18.3,50.5637108027935,3.68472027629614));
#73250=CARTESIAN_POINT('',(18.18,50.3667122364044,3.6012277290225));
#73251=CARTESIAN_POINT('',(18.3,50.3667122364044,3.6012277290225));
#73252=CARTESIAN_POINT('Ctrl Pts',(18.18,50.3667122364044,3.6012277290225));
#73253=CARTESIAN_POINT('Ctrl Pts',(18.18,50.4834926366806,3.6012277290225));
#73254=CARTESIAN_POINT('Ctrl Pts',(18.18,50.5637108027935,3.68472027629614));
#73255=CARTESIAN_POINT('Ctrl Pts',(18.3,50.1304228842258,3.69290578216314));
#73256=CARTESIAN_POINT('Ctrl Pts',(18.1272,50.1304228842258,3.69290578216314));
#73257=CARTESIAN_POINT('Ctrl Pts',(18.3,50.255388790369,3.6012277290225));
#73258=CARTESIAN_POINT('Ctrl Pts',(18.1272,50.255388790369,3.6012277290225));
#73259=CARTESIAN_POINT('Ctrl Pts',(18.3,50.3667122364044,3.6012277290225));
#73260=CARTESIAN_POINT('Ctrl Pts',(18.1272,50.3667122364044,3.6012277290225));
#73261=CARTESIAN_POINT('',(18.3,50.1304228842258,3.69290578216314));
#73262=CARTESIAN_POINT('Ctrl Pts',(18.3,50.1304228842258,3.69290578216314));
#73263=CARTESIAN_POINT('Ctrl Pts',(18.3,50.255388790369,3.6012277290225));
#73264=CARTESIAN_POINT('Ctrl Pts',(18.3,50.3667122364044,3.6012277290225));
#73265=CARTESIAN_POINT('',(18.18,50.1304228842258,3.69290578216314));
#73266=CARTESIAN_POINT('',(18.3,50.1304228842258,3.69290578216314));
#73267=CARTESIAN_POINT('Ctrl Pts',(18.18,50.1304228842258,3.69290578216314));
#73268=CARTESIAN_POINT('Ctrl Pts',(18.18,50.255388790369,3.6012277290225));
#73269=CARTESIAN_POINT('Ctrl Pts',(18.18,50.3667122364044,3.6012277290225));
#73270=CARTESIAN_POINT('Ctrl Pts',(18.3,49.791541570425,4.04542966783047));
#73271=CARTESIAN_POINT('Ctrl Pts',(18.1272,49.791541570425,4.04542966783047));
#73272=CARTESIAN_POINT('Ctrl Pts',(18.3,50.0054569780826,3.78458383530378));
#73273=CARTESIAN_POINT('Ctrl Pts',(18.1272,50.0054569780826,3.78458383530378));
#73274=CARTESIAN_POINT('Ctrl Pts',(18.3,50.1304228842258,3.69290578216314));
#73275=CARTESIAN_POINT('Ctrl Pts',(18.1272,50.1304228842258,3.69290578216314));
#73276=CARTESIAN_POINT('',(18.3,49.791541570425,4.04542966783047));
#73277=CARTESIAN_POINT('Ctrl Pts',(18.3,49.791541570425,4.04542966783047));
#73278=CARTESIAN_POINT('Ctrl Pts',(18.3,50.0054569780826,3.78458383530378));
#73279=CARTESIAN_POINT('Ctrl Pts',(18.3,50.1304228842258,3.69290578216314));
#73280=CARTESIAN_POINT('',(18.18,49.791541570425,4.04542966783047));
#73281=CARTESIAN_POINT('',(18.3,49.791541570425,4.04542966783047));
#73282=CARTESIAN_POINT('Ctrl Pts',(18.18,49.791541570425,4.04542966783047));
#73283=CARTESIAN_POINT('Ctrl Pts',(18.18,50.0054569780826,3.78458383530378));
#73284=CARTESIAN_POINT('Ctrl Pts',(18.18,50.1304228842258,3.69290578216314));
#73285=CARTESIAN_POINT('Ctrl Pts',(18.3,49.5492495834827,4.30245558768511));
#73286=CARTESIAN_POINT('Ctrl Pts',(18.1272,49.5492495834827,4.30245558768511));
#73287=CARTESIAN_POINT('Ctrl Pts',(18.3,49.6540247142315,4.21350604891777));
#73288=CARTESIAN_POINT('Ctrl Pts',(18.1272,49.6540247142315,4.21350604891777));
#73289=CARTESIAN_POINT('Ctrl Pts',(18.3,49.791541570425,4.04542966783047));
#73290=CARTESIAN_POINT('Ctrl Pts',(18.1272,49.791541570425,4.04542966783047));
#73291=CARTESIAN_POINT('',(18.3,49.5492495834827,4.30245558768511));
#73292=CARTESIAN_POINT('Ctrl Pts',(18.3,49.5492495834827,4.30245558768511));
#73293=CARTESIAN_POINT('Ctrl Pts',(18.3,49.6540247142315,4.21350604891777));
#73294=CARTESIAN_POINT('Ctrl Pts',(18.3,49.791541570425,4.04542966783047));
#73295=CARTESIAN_POINT('',(18.18,49.5492495834827,4.30245558768511));
#73296=CARTESIAN_POINT('',(18.3,49.5492495834827,4.30245558768511));
#73297=CARTESIAN_POINT('Ctrl Pts',(18.18,49.5492495834827,4.30245558768511));
#73298=CARTESIAN_POINT('Ctrl Pts',(18.18,49.6540247142315,4.21350604891777));
#73299=CARTESIAN_POINT('Ctrl Pts',(18.18,49.791541570425,4.04542966783047));
#73300=CARTESIAN_POINT('Ctrl Pts',(18.3,49.3364258348942,4.43178708702326));
#73301=CARTESIAN_POINT('Ctrl Pts',(18.1272,49.3364258348942,4.43178708702326));
#73302=CARTESIAN_POINT('Ctrl Pts',(18.3,49.4444747507572,4.39140508919954));
#73303=CARTESIAN_POINT('Ctrl Pts',(18.1272,49.4444747507572,4.39140508919954));
#73304=CARTESIAN_POINT('Ctrl Pts',(18.3,49.5492495834827,4.30245558768511));
#73305=CARTESIAN_POINT('Ctrl Pts',(18.1272,49.5492495834827,4.30245558768511));
#73306=CARTESIAN_POINT('',(18.3,49.3364258348942,4.43178708702326));
#73307=CARTESIAN_POINT('Ctrl Pts',(18.3,49.3364258348942,4.43178708702326));
#73308=CARTESIAN_POINT('Ctrl Pts',(18.3,49.4444747507572,4.39140508919954));
#73309=CARTESIAN_POINT('Ctrl Pts',(18.3,49.5492495834827,4.30245558768511));
#73310=CARTESIAN_POINT('',(18.18,49.3364258348942,4.43178708702326));
#73311=CARTESIAN_POINT('',(18.3,49.3364258348942,4.43178708702326));
#73312=CARTESIAN_POINT('Ctrl Pts',(18.18,49.3364258348942,4.43178708702326));
#73313=CARTESIAN_POINT('Ctrl Pts',(18.18,49.4444747507572,4.39140508919954));
#73314=CARTESIAN_POINT('Ctrl Pts',(18.18,49.5492495834827,4.30245558768511));
#73315=CARTESIAN_POINT('Ctrl Pts',(18.3,49.2000000417232,4.45470658168197));
#73316=CARTESIAN_POINT('Ctrl Pts',(18.1272,49.2000000417232,4.45470658168197));
#73317=CARTESIAN_POINT('Ctrl Pts',(18.3,49.2709414899349,4.4568893969059));
#73318=CARTESIAN_POINT('Ctrl Pts',(18.1272,49.2709414899349,4.4568893969059));
#73319=CARTESIAN_POINT('Ctrl Pts',(18.3,49.3364258348942,4.43178708702326));
#73320=CARTESIAN_POINT('Ctrl Pts',(18.1272,49.3364258348942,4.43178708702326));
#73321=CARTESIAN_POINT('',(18.3,49.2000000417232,4.45470658168197));
#73322=CARTESIAN_POINT('Ctrl Pts',(18.3,49.2000000417232,4.45470658168197));
#73323=CARTESIAN_POINT('Ctrl Pts',(18.3,49.2709414899349,4.4568893969059));
#73324=CARTESIAN_POINT('Ctrl Pts',(18.3,49.3364258348942,4.43178708702326));
#73325=CARTESIAN_POINT('',(18.18,49.2000000417232,4.45470658168197));
#73326=CARTESIAN_POINT('',(18.3,49.2000000417232,4.45470658168197));
#73327=CARTESIAN_POINT('Ctrl Pts',(18.18,49.2000000417232,4.45470658168197));
#73328=CARTESIAN_POINT('Ctrl Pts',(18.18,49.2709414899349,4.4568893969059));
#73329=CARTESIAN_POINT('Ctrl Pts',(18.18,49.3364258348942,4.43178708702326));
#73330=CARTESIAN_POINT('Origin',(18.3,49.2000000417232,3.39713501781225));
#73331=CARTESIAN_POINT('',(18.3,49.2000000417232,3.39713501781225));
#73332=CARTESIAN_POINT('',(18.3,49.2000000417232,4.44856750890613));
#73333=CARTESIAN_POINT('',(18.18,49.2000000417232,3.39713501781225));
#73334=CARTESIAN_POINT('',(18.3,49.2000000417232,3.39713501781225));
#73335=CARTESIAN_POINT('',(18.18,49.2000000417232,3.39713501781225));
#73336=CARTESIAN_POINT('Origin',(18.3,49.3888132512569,3.39713501781225));
#73337=CARTESIAN_POINT('',(18.3,49.3888132512569,3.39713501781225));
#73338=CARTESIAN_POINT('',(18.3,59.6944066256285,3.39713501781225));
#73339=CARTESIAN_POINT('',(18.18,49.3888132512569,3.39713501781225));
#73340=CARTESIAN_POINT('',(18.3,49.3888132512569,3.39713501781225));
#73341=CARTESIAN_POINT('',(18.18,49.3888132512569,3.39713501781225));
#73342=CARTESIAN_POINT('Origin',(18.3,49.3888132512569,4.18185527473688));
#73343=CARTESIAN_POINT('',(18.3,49.3888132512569,4.84092763736844));
#73344=CARTESIAN_POINT('',(18.18,49.3888132512569,4.18185527473688));
#73345=CARTESIAN_POINT('Origin',(18.18,49.9896316468716,3.29999995455146));
#73346=CARTESIAN_POINT('Origin',(18.3,70.,5.5));
#73347=CARTESIAN_POINT('Ctrl Pts',(18.3,40.643929117918,2.68117321692407));
#73348=CARTESIAN_POINT('Ctrl Pts',(18.1272,40.643929117918,2.68117321692407));
#73349=CARTESIAN_POINT('Ctrl Pts',(18.3,40.643929117918,2.81650750003755));
#73350=CARTESIAN_POINT('Ctrl Pts',(18.1272,40.643929117918,2.81650750003755));
#73351=CARTESIAN_POINT('Ctrl Pts',(18.3,40.5293315887451,2.89727149568498));
#73352=CARTESIAN_POINT('Ctrl Pts',(18.1272,40.5293315887451,2.89727149568498));
#73353=CARTESIAN_POINT('',(18.3,40.643929117918,2.68117321692407));
#73354=CARTESIAN_POINT('',(18.3,40.5293315887451,2.89727149568498));
#73355=CARTESIAN_POINT('Ctrl Pts',(18.3,40.643929117918,2.68117321692407));
#73356=CARTESIAN_POINT('Ctrl Pts',(18.3,40.643929117918,2.81650750003755));
#73357=CARTESIAN_POINT('Ctrl Pts',(18.3,40.5293315887451,2.89727149568498));
#73358=CARTESIAN_POINT('',(18.18,40.643929117918,2.68117321692407));
#73359=CARTESIAN_POINT('',(18.3,40.643929117918,2.68117321692407));
#73360=CARTESIAN_POINT('',(18.18,40.5293315887451,2.89727149568498));
#73361=CARTESIAN_POINT('Ctrl Pts',(18.18,40.643929117918,2.68117321692407));
#73362=CARTESIAN_POINT('Ctrl Pts',(18.18,40.643929117918,2.81650750003755));
#73363=CARTESIAN_POINT('Ctrl Pts',(18.18,40.5293315887451,2.89727149568498));
#73364=CARTESIAN_POINT('',(18.3,40.5293315887451,2.89727149568498));
#73365=CARTESIAN_POINT('Ctrl Pts',(18.3,40.5140519380569,2.45143247805536));
#73366=CARTESIAN_POINT('Ctrl Pts',(18.1272,40.5140519380569,2.45143247805536));
#73367=CARTESIAN_POINT('Ctrl Pts',(18.3,40.643929117918,2.54365621171892));
#73368=CARTESIAN_POINT('Ctrl Pts',(18.1272,40.643929117918,2.54365621171892));
#73369=CARTESIAN_POINT('Ctrl Pts',(18.3,40.643929117918,2.68117321692407));
#73370=CARTESIAN_POINT('Ctrl Pts',(18.1272,40.643929117918,2.68117321692407));
#73371=CARTESIAN_POINT('',(18.3,40.5140519380569,2.45143247805536));
#73372=CARTESIAN_POINT('Ctrl Pts',(18.3,40.5140519380569,2.45143247805536));
#73373=CARTESIAN_POINT('Ctrl Pts',(18.3,40.643929117918,2.54365621171892));
#73374=CARTESIAN_POINT('Ctrl Pts',(18.3,40.643929117918,2.68117321692407));
#73375=CARTESIAN_POINT('',(18.18,40.5140519380569,2.45143247805536));
#73376=CARTESIAN_POINT('',(18.3,40.5140519380569,2.45143247805536));
#73377=CARTESIAN_POINT('Ctrl Pts',(18.18,40.5140519380569,2.45143247805536));
#73378=CARTESIAN_POINT('Ctrl Pts',(18.18,40.643929117918,2.54365621171892));
#73379=CARTESIAN_POINT('Ctrl Pts',(18.18,40.643929117918,2.68117321692407));
#73380=CARTESIAN_POINT('Ctrl Pts',(18.3,39.9890859663486,2.3592087443918));
#73381=CARTESIAN_POINT('Ctrl Pts',(18.1272,39.9890859663486,2.3592087443918));
#73382=CARTESIAN_POINT('Ctrl Pts',(18.3,40.3841746091843,2.3592087443918));
#73383=CARTESIAN_POINT('Ctrl Pts',(18.1272,40.3841746091843,2.3592087443918));
#73384=CARTESIAN_POINT('Ctrl Pts',(18.3,40.5140519380569,2.45143247805536));
#73385=CARTESIAN_POINT('Ctrl Pts',(18.1272,40.5140519380569,2.45143247805536));
#73386=CARTESIAN_POINT('',(18.3,39.9890859663486,2.3592087443918));
#73387=CARTESIAN_POINT('Ctrl Pts',(18.3,39.9890859663486,2.3592087443918));
#73388=CARTESIAN_POINT('Ctrl Pts',(18.3,40.3841746091843,2.3592087443918));
#73389=CARTESIAN_POINT('Ctrl Pts',(18.3,40.5140519380569,2.45143247805536));
#73390=CARTESIAN_POINT('',(18.18,39.9890859663486,2.3592087443918));
#73391=CARTESIAN_POINT('',(18.3,39.9890859663486,2.3592087443918));
#73392=CARTESIAN_POINT('Ctrl Pts',(18.18,39.9890859663486,2.3592087443918));
#73393=CARTESIAN_POINT('Ctrl Pts',(18.18,40.3841746091843,2.3592087443918));
#73394=CARTESIAN_POINT('Ctrl Pts',(18.18,40.5140519380569,2.45143247805536));
#73395=CARTESIAN_POINT('Ctrl Pts',(18.3,39.4652115046978,2.45143247805536));
#73396=CARTESIAN_POINT('Ctrl Pts',(18.1272,39.4652115046978,2.45143247805536));
#73397=CARTESIAN_POINT('Ctrl Pts',(18.3,39.5961801946163,2.3592087443918));
#73398=CARTESIAN_POINT('Ctrl Pts',(18.1272,39.5961801946163,2.3592087443918));
#73399=CARTESIAN_POINT('Ctrl Pts',(18.3,39.9890859663486,2.3592087443918));
#73400=CARTESIAN_POINT('Ctrl Pts',(18.1272,39.9890859663486,2.3592087443918));
#73401=CARTESIAN_POINT('',(18.3,39.4652115046978,2.45143247805536));
#73402=CARTESIAN_POINT('Ctrl Pts',(18.3,39.4652115046978,2.45143247805536));
#73403=CARTESIAN_POINT('Ctrl Pts',(18.3,39.5961801946163,2.3592087443918));
#73404=CARTESIAN_POINT('Ctrl Pts',(18.3,39.9890859663486,2.3592087443918));
#73405=CARTESIAN_POINT('',(18.18,39.4652115046978,2.45143247805536));
#73406=CARTESIAN_POINT('',(18.3,39.4652115046978,2.45143247805536));
#73407=CARTESIAN_POINT('Ctrl Pts',(18.18,39.4652115046978,2.45143247805536));
#73408=CARTESIAN_POINT('Ctrl Pts',(18.18,39.5961801946163,2.3592087443918));
#73409=CARTESIAN_POINT('Ctrl Pts',(18.18,39.9890859663486,2.3592087443918));
#73410=CARTESIAN_POINT('Ctrl Pts',(18.3,39.3342428147793,2.67899034582078));
#73411=CARTESIAN_POINT('Ctrl Pts',(18.1272,39.3342428147793,2.67899034582078));
#73412=CARTESIAN_POINT('Ctrl Pts',(18.3,39.3342428147793,2.54365621171892));
#73413=CARTESIAN_POINT('Ctrl Pts',(18.1272,39.3342428147793,2.54365621171892));
#73414=CARTESIAN_POINT('Ctrl Pts',(18.3,39.4652115046978,2.45143247805536));
#73415=CARTESIAN_POINT('Ctrl Pts',(18.1272,39.4652115046978,2.45143247805536));
#73416=CARTESIAN_POINT('',(18.3,39.3342428147793,2.67899034582078));
#73417=CARTESIAN_POINT('Ctrl Pts',(18.3,39.3342428147793,2.67899034582078));
#73418=CARTESIAN_POINT('Ctrl Pts',(18.3,39.3342428147793,2.54365621171892));
#73419=CARTESIAN_POINT('Ctrl Pts',(18.3,39.4652115046978,2.45143247805536));
#73420=CARTESIAN_POINT('',(18.18,39.3342428147793,2.67899034582078));
#73421=CARTESIAN_POINT('',(18.3,39.3342428147793,2.67899034582078));
#73422=CARTESIAN_POINT('Ctrl Pts',(18.18,39.3342428147793,2.67899034582078));
#73423=CARTESIAN_POINT('Ctrl Pts',(18.18,39.3342428147793,2.54365621171892));
#73424=CARTESIAN_POINT('Ctrl Pts',(18.18,39.4652115046978,2.45143247805536));
#73425=CARTESIAN_POINT('Ctrl Pts',(18.3,39.4646658241749,2.90654836259782));
#73426=CARTESIAN_POINT('Ctrl Pts',(18.1272,39.4646658241749,2.90654836259782));
#73427=CARTESIAN_POINT('Ctrl Pts',(18.3,39.3342428147793,2.81432462893426));
#73428=CARTESIAN_POINT('Ctrl Pts',(18.1272,39.3342428147793,2.81432462893426));
#73429=CARTESIAN_POINT('Ctrl Pts',(18.3,39.3342428147793,2.67899034582078));
#73430=CARTESIAN_POINT('Ctrl Pts',(18.1272,39.3342428147793,2.67899034582078));
#73431=CARTESIAN_POINT('',(18.3,39.4646658241749,2.90654836259782));
#73432=CARTESIAN_POINT('Ctrl Pts',(18.3,39.4646658241749,2.90654836259782));
#73433=CARTESIAN_POINT('Ctrl Pts',(18.3,39.3342428147793,2.81432462893426));
#73434=CARTESIAN_POINT('Ctrl Pts',(18.3,39.3342428147793,2.67899034582078));
#73435=CARTESIAN_POINT('',(18.18,39.4646658241749,2.90654836259782));
#73436=CARTESIAN_POINT('',(18.3,39.4646658241749,2.90654836259782));
#73437=CARTESIAN_POINT('Ctrl Pts',(18.18,39.4646658241749,2.90654836259782));
#73438=CARTESIAN_POINT('Ctrl Pts',(18.18,39.3342428147793,2.81432462893426));
#73439=CARTESIAN_POINT('Ctrl Pts',(18.18,39.3342428147793,2.67899034582078));
#73440=CARTESIAN_POINT('Ctrl Pts',(18.3,39.9890859663486,2.99877209626138));
#73441=CARTESIAN_POINT('Ctrl Pts',(18.1272,39.9890859663486,2.99877209626138));
#73442=CARTESIAN_POINT('Ctrl Pts',(18.3,39.5950888335705,2.99877209626138));
#73443=CARTESIAN_POINT('Ctrl Pts',(18.1272,39.5950888335705,2.99877209626138));
#73444=CARTESIAN_POINT('Ctrl Pts',(18.3,39.4646658241749,2.90654836259782));
#73445=CARTESIAN_POINT('Ctrl Pts',(18.1272,39.4646658241749,2.90654836259782));
#73446=CARTESIAN_POINT('',(18.3,39.9890859663486,2.99877209626138));
#73447=CARTESIAN_POINT('Ctrl Pts',(18.3,39.9890859663486,2.99877209626138));
#73448=CARTESIAN_POINT('Ctrl Pts',(18.3,39.5950888335705,2.99877209626138));
#73449=CARTESIAN_POINT('Ctrl Pts',(18.3,39.4646658241749,2.90654836259782));
#73450=CARTESIAN_POINT('',(18.18,39.9890859663486,2.99877209626138));
#73451=CARTESIAN_POINT('',(18.3,39.9890859663486,2.99877209626138));
#73452=CARTESIAN_POINT('Ctrl Pts',(18.18,39.9890859663486,2.99877209626138));
#73453=CARTESIAN_POINT('Ctrl Pts',(18.18,39.5950888335705,2.99877209626138));
#73454=CARTESIAN_POINT('Ctrl Pts',(18.18,39.4646658241749,2.90654836259782));
#73455=CARTESIAN_POINT('Ctrl Pts',(18.3,40.5293315887451,2.89727149568498));
#73456=CARTESIAN_POINT('Ctrl Pts',(18.1272,40.5293315887451,2.89727149568498));
#73457=CARTESIAN_POINT('Ctrl Pts',(18.3,40.3830830991268,2.99877209626138));
#73458=CARTESIAN_POINT('Ctrl Pts',(18.1272,40.3830830991268,2.99877209626138));
#73459=CARTESIAN_POINT('Ctrl Pts',(18.3,39.9890859663486,2.99877209626138));
#73460=CARTESIAN_POINT('Ctrl Pts',(18.1272,39.9890859663486,2.99877209626138));
#73461=CARTESIAN_POINT('Ctrl Pts',(18.3,40.5293315887451,2.89727149568498));
#73462=CARTESIAN_POINT('Ctrl Pts',(18.3,40.3830830991268,2.99877209626138));
#73463=CARTESIAN_POINT('Ctrl Pts',(18.3,39.9890859663486,2.99877209626138));
#73464=CARTESIAN_POINT('Ctrl Pts',(18.18,40.5293315887451,2.89727149568498));
#73465=CARTESIAN_POINT('Ctrl Pts',(18.18,40.3830830991268,2.99877209626138));
#73466=CARTESIAN_POINT('Ctrl Pts',(18.18,39.9890859663486,2.99877209626138));
#73467=CARTESIAN_POINT('Ctrl Pts',(18.3,39.1727148234844,2.67899034582078));
#73468=CARTESIAN_POINT('Ctrl Pts',(18.1272,39.1727148234844,2.67899034582078));
#73469=CARTESIAN_POINT('Ctrl Pts',(18.3,39.1727148234844,2.91036827526987));
#73470=CARTESIAN_POINT('Ctrl Pts',(18.1272,39.1727148234844,2.91036827526987));
#73471=CARTESIAN_POINT('Ctrl Pts',(18.3,39.3386085569858,3.04242832623422));
#73472=CARTESIAN_POINT('Ctrl Pts',(18.1272,39.3386085569858,3.04242832623422));
#73473=CARTESIAN_POINT('',(18.3,39.1727148234844,2.67899034582078));
#73474=CARTESIAN_POINT('',(18.3,39.3386085569858,3.04242832623422));
#73475=CARTESIAN_POINT('Ctrl Pts',(18.3,39.1727148234844,2.67899034582078));
#73476=CARTESIAN_POINT('Ctrl Pts',(18.3,39.1727148234844,2.91036827526987));
#73477=CARTESIAN_POINT('Ctrl Pts',(18.3,39.3386085569858,3.04242832623422));
#73478=CARTESIAN_POINT('',(18.18,39.1727148234844,2.67899034582078));
#73479=CARTESIAN_POINT('',(18.3,39.1727148234844,2.67899034582078));
#73480=CARTESIAN_POINT('',(18.18,39.3386085569858,3.04242832623422));
#73481=CARTESIAN_POINT('Ctrl Pts',(18.18,39.1727148234844,2.67899034582078));
#73482=CARTESIAN_POINT('Ctrl Pts',(18.18,39.1727148234844,2.91036827526987));
#73483=CARTESIAN_POINT('Ctrl Pts',(18.18,39.3386085569858,3.04242832623422));
#73484=CARTESIAN_POINT('',(18.3,39.3386085569858,3.04242832623422));
#73485=CARTESIAN_POINT('Ctrl Pts',(18.3,39.2671214282513,2.38813100419939));
#73486=CARTESIAN_POINT('Ctrl Pts',(18.1272,39.2671214282513,2.38813100419939));
#73487=CARTESIAN_POINT('Ctrl Pts',(18.3,39.1727148234844,2.5032742138952));
#73488=CARTESIAN_POINT('Ctrl Pts',(18.1272,39.1727148234844,2.5032742138952));
#73489=CARTESIAN_POINT('Ctrl Pts',(18.3,39.1727148234844,2.67899034582078));
#73490=CARTESIAN_POINT('Ctrl Pts',(18.1272,39.1727148234844,2.67899034582078));
#73491=CARTESIAN_POINT('',(18.3,39.2671214282513,2.38813100419939));
#73492=CARTESIAN_POINT('Ctrl Pts',(18.3,39.2671214282513,2.38813100419939));
#73493=CARTESIAN_POINT('Ctrl Pts',(18.3,39.1727148234844,2.5032742138952));
#73494=CARTESIAN_POINT('Ctrl Pts',(18.3,39.1727148234844,2.67899034582078));
#73495=CARTESIAN_POINT('',(18.18,39.2671214282513,2.38813100419939));
#73496=CARTESIAN_POINT('',(18.3,39.2671214282513,2.38813100419939));
#73497=CARTESIAN_POINT('Ctrl Pts',(18.18,39.2671214282513,2.38813100419939));
#73498=CARTESIAN_POINT('Ctrl Pts',(18.18,39.1727148234844,2.5032742138952));
#73499=CARTESIAN_POINT('Ctrl Pts',(18.18,39.1727148234844,2.67899034582078));
#73500=CARTESIAN_POINT('Ctrl Pts',(18.3,39.5345156133175,2.2151432748884));
#73501=CARTESIAN_POINT('Ctrl Pts',(18.1272,39.5345156133175,2.2151432748884));
#73502=CARTESIAN_POINT('Ctrl Pts',(18.3,39.3615280330181,2.27298764549196));
#73503=CARTESIAN_POINT('Ctrl Pts',(18.1272,39.3615280330181,2.27298764549196));
#73504=CARTESIAN_POINT('Ctrl Pts',(18.3,39.2671214282513,2.38813100419939));
#73505=CARTESIAN_POINT('Ctrl Pts',(18.1272,39.2671214282513,2.38813100419939));
#73506=CARTESIAN_POINT('',(18.3,39.5345156133175,2.2151432748884));
#73507=CARTESIAN_POINT('Ctrl Pts',(18.3,39.5345156133175,2.2151432748884));
#73508=CARTESIAN_POINT('Ctrl Pts',(18.3,39.3615280330181,2.27298764549196));
#73509=CARTESIAN_POINT('Ctrl Pts',(18.3,39.2671214282513,2.38813100419939));
#73510=CARTESIAN_POINT('',(18.18,39.5345156133175,2.2151432748884));
#73511=CARTESIAN_POINT('',(18.3,39.5345156133175,2.2151432748884));
#73512=CARTESIAN_POINT('Ctrl Pts',(18.18,39.5345156133175,2.2151432748884));
#73513=CARTESIAN_POINT('Ctrl Pts',(18.18,39.3615280330181,2.27298764549196));
#73514=CARTESIAN_POINT('Ctrl Pts',(18.18,39.2671214282513,2.38813100419939));
#73515=CARTESIAN_POINT('Ctrl Pts',(18.3,39.9890859663486,2.15729875527322));
#73516=CARTESIAN_POINT('Ctrl Pts',(18.1272,39.9890859663486,2.15729875527322));
#73517=CARTESIAN_POINT('Ctrl Pts',(18.3,39.7075034916401,2.15729875527322));
#73518=CARTESIAN_POINT('Ctrl Pts',(18.1272,39.7075034916401,2.15729875527322));
#73519=CARTESIAN_POINT('Ctrl Pts',(18.3,39.5345156133175,2.2151432748884));
#73520=CARTESIAN_POINT('Ctrl Pts',(18.1272,39.5345156133175,2.2151432748884));
#73521=CARTESIAN_POINT('',(18.3,39.9890859663486,2.15729875527322));
#73522=CARTESIAN_POINT('Ctrl Pts',(18.3,39.9890859663486,2.15729875527322));
#73523=CARTESIAN_POINT('Ctrl Pts',(18.3,39.7075034916401,2.15729875527322));
#73524=CARTESIAN_POINT('Ctrl Pts',(18.3,39.5345156133175,2.2151432748884));
#73525=CARTESIAN_POINT('',(18.18,39.9890859663486,2.15729875527322));
#73526=CARTESIAN_POINT('',(18.3,39.9890859663486,2.15729875527322));
#73527=CARTESIAN_POINT('Ctrl Pts',(18.18,39.9890859663486,2.15729875527322));
#73528=CARTESIAN_POINT('Ctrl Pts',(18.18,39.7075034916401,2.15729875527322));
#73529=CARTESIAN_POINT('Ctrl Pts',(18.18,39.5345156133175,2.2151432748884));
#73530=CARTESIAN_POINT('Ctrl Pts',(18.3,40.3672577679157,2.19331515990198));
#73531=CARTESIAN_POINT('Ctrl Pts',(18.1272,40.3672577679157,2.19331515990198));
#73532=CARTESIAN_POINT('Ctrl Pts',(18.3,40.2270122110844,2.15729875527322));
#73533=CARTESIAN_POINT('Ctrl Pts',(18.1272,40.2270122110844,2.15729875527322));
#73534=CARTESIAN_POINT('Ctrl Pts',(18.3,39.9890859663486,2.15729875527322));
#73535=CARTESIAN_POINT('Ctrl Pts',(18.1272,39.9890859663486,2.15729875527322));
#73536=CARTESIAN_POINT('',(18.3,40.3672577679157,2.19331515990198));
#73537=CARTESIAN_POINT('Ctrl Pts',(18.3,40.3672577679157,2.19331515990198));
#73538=CARTESIAN_POINT('Ctrl Pts',(18.3,40.2270122110844,2.15729875527322));
#73539=CARTESIAN_POINT('Ctrl Pts',(18.3,39.9890859663486,2.15729875527322));
#73540=CARTESIAN_POINT('',(18.18,40.3672577679157,2.19331515990198));
#73541=CARTESIAN_POINT('',(18.3,40.3672577679157,2.19331515990198));
#73542=CARTESIAN_POINT('Ctrl Pts',(18.18,40.3672577679157,2.19331515990198));
#73543=CARTESIAN_POINT('Ctrl Pts',(18.18,40.2270122110844,2.15729875527322));
#73544=CARTESIAN_POINT('Ctrl Pts',(18.18,39.9890859663486,2.15729875527322));
#73545=CARTESIAN_POINT('Ctrl Pts',(18.3,40.605184161663,2.2926330383867));
#73546=CARTESIAN_POINT('Ctrl Pts',(18.1272,40.605184161663,2.2926330383867));
#73547=CARTESIAN_POINT('Ctrl Pts',(18.3,40.5075034737587,2.22933141551912));
#73548=CARTESIAN_POINT('Ctrl Pts',(18.1272,40.5075034737587,2.22933141551912));
#73549=CARTESIAN_POINT('Ctrl Pts',(18.3,40.3672577679157,2.19331515990198));
#73550=CARTESIAN_POINT('Ctrl Pts',(18.1272,40.3672577679157,2.19331515990198));
#73551=CARTESIAN_POINT('',(18.3,40.605184161663,2.2926330383867));
#73552=CARTESIAN_POINT('Ctrl Pts',(18.3,40.605184161663,2.2926330383867));
#73553=CARTESIAN_POINT('Ctrl Pts',(18.3,40.5075034737587,2.22933141551912));
#73554=CARTESIAN_POINT('Ctrl Pts',(18.3,40.3672577679157,2.19331515990198));
#73555=CARTESIAN_POINT('',(18.18,40.605184161663,2.2926330383867));
#73556=CARTESIAN_POINT('',(18.3,40.605184161663,2.2926330383867));
#73557=CARTESIAN_POINT('Ctrl Pts',(18.18,40.605184161663,2.2926330383867));
#73558=CARTESIAN_POINT('Ctrl Pts',(18.18,40.5075034737587,2.22933141551912));
#73559=CARTESIAN_POINT('Ctrl Pts',(18.18,40.3672577679157,2.19331515990198));
#73560=CARTESIAN_POINT('Ctrl Pts',(18.3,40.7547067344189,2.45306966863573));
#73561=CARTESIAN_POINT('Ctrl Pts',(18.1272,40.7547067344189,2.45306966863573));
#73562=CARTESIAN_POINT('Ctrl Pts',(18.3,40.702864998579,2.35593451224267));
#73563=CARTESIAN_POINT('Ctrl Pts',(18.1272,40.702864998579,2.35593451224267));
#73564=CARTESIAN_POINT('Ctrl Pts',(18.3,40.605184161663,2.2926330383867));
#73565=CARTESIAN_POINT('Ctrl Pts',(18.1272,40.605184161663,2.2926330383867));
#73566=CARTESIAN_POINT('',(18.3,40.7547067344189,2.45306966863573));
#73567=CARTESIAN_POINT('Ctrl Pts',(18.3,40.7547067344189,2.45306966863573));
#73568=CARTESIAN_POINT('Ctrl Pts',(18.3,40.702864998579,2.35593451224267));
#73569=CARTESIAN_POINT('Ctrl Pts',(18.3,40.605184161663,2.2926330383867));
#73570=CARTESIAN_POINT('',(18.18,40.7547067344189,2.45306966863573));
#73571=CARTESIAN_POINT('',(18.3,40.7547067344189,2.45306966863573));
#73572=CARTESIAN_POINT('Ctrl Pts',(18.18,40.7547067344189,2.45306966863573));
#73573=CARTESIAN_POINT('Ctrl Pts',(18.18,40.702864998579,2.35593451224267));
#73574=CARTESIAN_POINT('Ctrl Pts',(18.18,40.605184161663,2.2926330383867));
#73575=CARTESIAN_POINT('Ctrl Pts',(18.3,40.8065484702587,2.67899034582078));
#73576=CARTESIAN_POINT('Ctrl Pts',(18.1272,40.8065484702587,2.67899034582078));
#73577=CARTESIAN_POINT('Ctrl Pts',(18.3,40.8065484702587,2.55020467601716));
#73578=CARTESIAN_POINT('Ctrl Pts',(18.1272,40.8065484702587,2.55020467601716));
#73579=CARTESIAN_POINT('Ctrl Pts',(18.3,40.7547067344189,2.45306966863573));
#73580=CARTESIAN_POINT('Ctrl Pts',(18.1272,40.7547067344189,2.45306966863573));
#73581=CARTESIAN_POINT('',(18.3,40.8065484702587,2.67899034582078));
#73582=CARTESIAN_POINT('Ctrl Pts',(18.3,40.8065484702587,2.67899034582078));
#73583=CARTESIAN_POINT('Ctrl Pts',(18.3,40.8065484702587,2.55020467601716));
#73584=CARTESIAN_POINT('Ctrl Pts',(18.3,40.7547067344189,2.45306966863573));
#73585=CARTESIAN_POINT('',(18.18,40.8065484702587,2.67899034582078));
#73586=CARTESIAN_POINT('',(18.3,40.8065484702587,2.67899034582078));
#73587=CARTESIAN_POINT('Ctrl Pts',(18.18,40.8065484702587,2.67899034582078));
#73588=CARTESIAN_POINT('Ctrl Pts',(18.18,40.8065484702587,2.55020467601716));
#73589=CARTESIAN_POINT('Ctrl Pts',(18.18,40.7547067344189,2.45306966863573));
#73590=CARTESIAN_POINT('Ctrl Pts',(18.3,40.7126876950264,2.96875847540796));
#73591=CARTESIAN_POINT('Ctrl Pts',(18.1272,40.7126876950264,2.96875847540796));
#73592=CARTESIAN_POINT('Ctrl Pts',(18.3,40.8065484702587,2.85361526571214));
#73593=CARTESIAN_POINT('Ctrl Pts',(18.1272,40.8065484702587,2.85361526571214));
#73594=CARTESIAN_POINT('Ctrl Pts',(18.3,40.8065484702587,2.67899034582078));
#73595=CARTESIAN_POINT('Ctrl Pts',(18.1272,40.8065484702587,2.67899034582078));
#73596=CARTESIAN_POINT('',(18.3,40.7126876950264,2.96875847540796));
#73597=CARTESIAN_POINT('Ctrl Pts',(18.3,40.7126876950264,2.96875847540796));
#73598=CARTESIAN_POINT('Ctrl Pts',(18.3,40.8065484702587,2.85361526571214));
#73599=CARTESIAN_POINT('Ctrl Pts',(18.3,40.8065484702587,2.67899034582078));
#73600=CARTESIAN_POINT('',(18.18,40.7126876950264,2.96875847540796));
#73601=CARTESIAN_POINT('',(18.3,40.7126876950264,2.96875847540796));
#73602=CARTESIAN_POINT('Ctrl Pts',(18.18,40.7126876950264,2.96875847540796));
#73603=CARTESIAN_POINT('Ctrl Pts',(18.18,40.8065484702587,2.85361526571214));
#73604=CARTESIAN_POINT('Ctrl Pts',(18.18,40.8065484702587,2.67899034582078));
#73605=CARTESIAN_POINT('Ctrl Pts',(18.3,40.4458390414715,3.14229188524187));
#73606=CARTESIAN_POINT('Ctrl Pts',(18.1272,40.4458390414715,3.14229188524187));
#73607=CARTESIAN_POINT('Ctrl Pts',(18.3,40.6188267707825,3.08390168510377));
#73608=CARTESIAN_POINT('Ctrl Pts',(18.1272,40.6188267707825,3.08390168510377));
#73609=CARTESIAN_POINT('Ctrl Pts',(18.3,40.7126876950264,2.96875847540796));
#73610=CARTESIAN_POINT('Ctrl Pts',(18.1272,40.7126876950264,2.96875847540796));
#73611=CARTESIAN_POINT('',(18.3,40.4458390414715,3.14229188524187));
#73612=CARTESIAN_POINT('Ctrl Pts',(18.3,40.4458390414715,3.14229188524187));
#73613=CARTESIAN_POINT('Ctrl Pts',(18.3,40.6188267707825,3.08390168510377));
#73614=CARTESIAN_POINT('Ctrl Pts',(18.3,40.7126876950264,2.96875847540796));
#73615=CARTESIAN_POINT('',(18.18,40.4458390414715,3.14229188524187));
#73616=CARTESIAN_POINT('',(18.3,40.4458390414715,3.14229188524187));
#73617=CARTESIAN_POINT('Ctrl Pts',(18.18,40.4458390414715,3.14229188524187));
#73618=CARTESIAN_POINT('Ctrl Pts',(18.18,40.6188267707825,3.08390168510377));
#73619=CARTESIAN_POINT('Ctrl Pts',(18.18,40.7126876950264,2.96875847540796));
#73620=CARTESIAN_POINT('Ctrl Pts',(18.3,39.9890859663486,3.20068208537996));
#73621=CARTESIAN_POINT('Ctrl Pts',(18.1272,39.9890859663486,3.20068208537996));
#73622=CARTESIAN_POINT('Ctrl Pts',(18.3,40.2728513121605,3.20068208537996));
#73623=CARTESIAN_POINT('Ctrl Pts',(18.1272,40.2728513121605,3.20068208537996));
#73624=CARTESIAN_POINT('Ctrl Pts',(18.3,40.4458390414715,3.14229188524187));
#73625=CARTESIAN_POINT('Ctrl Pts',(18.1272,40.4458390414715,3.14229188524187));
#73626=CARTESIAN_POINT('',(18.3,39.9890859663486,3.20068208537996));
#73627=CARTESIAN_POINT('Ctrl Pts',(18.3,39.9890859663486,3.20068208537996));
#73628=CARTESIAN_POINT('Ctrl Pts',(18.3,40.2728513121605,3.20068208537996));
#73629=CARTESIAN_POINT('Ctrl Pts',(18.3,40.4458390414715,3.14229188524187));
#73630=CARTESIAN_POINT('',(18.18,39.9890859663486,3.20068208537996));
#73631=CARTESIAN_POINT('',(18.3,39.9890859663486,3.20068208537996));
#73632=CARTESIAN_POINT('Ctrl Pts',(18.18,39.9890859663486,3.20068208537996));
#73633=CARTESIAN_POINT('Ctrl Pts',(18.18,40.2728513121605,3.20068208537996));
#73634=CARTESIAN_POINT('Ctrl Pts',(18.18,40.4458390414715,3.14229188524187));
#73635=CARTESIAN_POINT('Ctrl Pts',(18.3,39.3386085569858,3.04242832623422));
#73636=CARTESIAN_POINT('Ctrl Pts',(18.1272,39.3386085569858,3.04242832623422));
#73637=CARTESIAN_POINT('Ctrl Pts',(18.3,39.5383356750011,3.20068208537996));
#73638=CARTESIAN_POINT('Ctrl Pts',(18.1272,39.5383356750011,3.20068208537996));
#73639=CARTESIAN_POINT('Ctrl Pts',(18.3,39.9890859663486,3.20068208537996));
#73640=CARTESIAN_POINT('Ctrl Pts',(18.1272,39.9890859663486,3.20068208537996));
#73641=CARTESIAN_POINT('Ctrl Pts',(18.3,39.3386085569858,3.04242832623422));
#73642=CARTESIAN_POINT('Ctrl Pts',(18.3,39.5383356750011,3.20068208537996));
#73643=CARTESIAN_POINT('Ctrl Pts',(18.3,39.9890859663486,3.20068208537996));
#73644=CARTESIAN_POINT('Ctrl Pts',(18.18,39.3386085569858,3.04242832623422));
#73645=CARTESIAN_POINT('Ctrl Pts',(18.18,39.5383356750011,3.20068208537996));
#73646=CARTESIAN_POINT('Ctrl Pts',(18.18,39.9890859663486,3.20068208537996));
#73647=CARTESIAN_POINT('Origin',(18.18,39.9890859663486,3.29999992661178));
#73648=CARTESIAN_POINT('Ctrl Pts',(18.3,39.1716234624386,3.93410628698766));
#73649=CARTESIAN_POINT('Ctrl Pts',(18.1272,39.1716234624386,3.93410628698766));
#73650=CARTESIAN_POINT('Ctrl Pts',(18.3,39.1716234624386,4.14474749974906));
#73651=CARTESIAN_POINT('Ctrl Pts',(18.1272,39.1716234624386,4.14474749974906));
#73652=CARTESIAN_POINT('Ctrl Pts',(18.3,39.2971350491047,4.28390165828168));
#73653=CARTESIAN_POINT('Ctrl Pts',(18.1272,39.2971350491047,4.28390165828168));
#73654=CARTESIAN_POINT('',(18.3,39.1716234624386,3.93410628698766));
#73655=CARTESIAN_POINT('',(18.3,39.2971350491047,4.28390165828168));
#73656=CARTESIAN_POINT('Ctrl Pts',(18.3,39.1716234624386,3.93410628698766));
#73657=CARTESIAN_POINT('Ctrl Pts',(18.3,39.1716234624386,4.14474749974906));
#73658=CARTESIAN_POINT('Ctrl Pts',(18.3,39.2971350491047,4.28390165828168));
#73659=CARTESIAN_POINT('',(18.18,39.1716234624386,3.93410628698766));
#73660=CARTESIAN_POINT('',(18.3,39.1716234624386,3.93410628698766));
#73661=CARTESIAN_POINT('',(18.18,39.2971350491047,4.28390165828168));
#73662=CARTESIAN_POINT('Ctrl Pts',(18.18,39.1716234624386,3.93410628698766));
#73663=CARTESIAN_POINT('Ctrl Pts',(18.18,39.1716234624386,4.14474749974906));
#73664=CARTESIAN_POINT('Ctrl Pts',(18.18,39.2971350491047,4.28390165828168));
#73665=CARTESIAN_POINT('',(18.3,39.2971350491047,4.28390165828168));
#73666=CARTESIAN_POINT('Ctrl Pts',(18.3,39.3173261225223,3.54774890504777));
#73667=CARTESIAN_POINT('Ctrl Pts',(18.1272,39.3173261225223,3.54774890504777));
#73668=CARTESIAN_POINT('Ctrl Pts',(18.3,39.1716234624386,3.70054563544691));
#73669=CARTESIAN_POINT('Ctrl Pts',(18.1272,39.1716234624386,3.70054563544691));
#73670=CARTESIAN_POINT('Ctrl Pts',(18.3,39.1716234624386,3.93410628698766));
#73671=CARTESIAN_POINT('Ctrl Pts',(18.1272,39.1716234624386,3.93410628698766));
#73672=CARTESIAN_POINT('',(18.3,39.3173261225223,3.54774890504777));
#73673=CARTESIAN_POINT('Ctrl Pts',(18.3,39.3173261225223,3.54774890504777));
#73674=CARTESIAN_POINT('Ctrl Pts',(18.3,39.1716234624386,3.70054563544691));
#73675=CARTESIAN_POINT('Ctrl Pts',(18.3,39.1716234624386,3.93410628698766));
#73676=CARTESIAN_POINT('',(18.18,39.3173261225223,3.54774890504777));
#73677=CARTESIAN_POINT('',(18.3,39.3173261225223,3.54774890504777));
#73678=CARTESIAN_POINT('Ctrl Pts',(18.18,39.3173261225223,3.54774890504777));
#73679=CARTESIAN_POINT('Ctrl Pts',(18.18,39.1716234624386,3.70054563544691));
#73680=CARTESIAN_POINT('Ctrl Pts',(18.18,39.1716234624386,3.93410628698766));
#73681=CARTESIAN_POINT('Ctrl Pts',(18.3,39.6725784480572,3.39495224915445));
#73682=CARTESIAN_POINT('Ctrl Pts',(18.1272,39.6725784480572,3.39495224915445));
#73683=CARTESIAN_POINT('Ctrl Pts',(18.3,39.4630287826061,3.39495224915445));
#73684=CARTESIAN_POINT('Ctrl Pts',(18.1272,39.4630287826061,3.39495224915445));
#73685=CARTESIAN_POINT('Ctrl Pts',(18.3,39.3173261225223,3.54774890504777));
#73686=CARTESIAN_POINT('Ctrl Pts',(18.1272,39.3173261225223,3.54774890504777));
#73687=CARTESIAN_POINT('',(18.3,39.6725784480572,3.39495224915445));
#73688=CARTESIAN_POINT('Ctrl Pts',(18.3,39.6725784480572,3.39495224915445));
#73689=CARTESIAN_POINT('Ctrl Pts',(18.3,39.4630287826061,3.39495224915445));
#73690=CARTESIAN_POINT('Ctrl Pts',(18.3,39.3173261225223,3.54774890504777));
#73691=CARTESIAN_POINT('',(18.18,39.6725784480572,3.39495224915445));
#73692=CARTESIAN_POINT('',(18.3,39.6725784480572,3.39495224915445));
#73693=CARTESIAN_POINT('Ctrl Pts',(18.18,39.6725784480572,3.39495224915445));
#73694=CARTESIAN_POINT('Ctrl Pts',(18.18,39.4630287826061,3.39495224915445));
#73695=CARTESIAN_POINT('Ctrl Pts',(18.18,39.3173261225223,3.54774890504777));
#73696=CARTESIAN_POINT('Ctrl Pts',(18.3,39.9306957662105,3.47353329919279));
#73697=CARTESIAN_POINT('Ctrl Pts',(18.1272,39.9306957662105,3.47353329919279));
#73698=CARTESIAN_POINT('Ctrl Pts',(18.3,39.8275579750538,3.39495224915445));
#73699=CARTESIAN_POINT('Ctrl Pts',(18.1272,39.8275579750538,3.39495224915445));
#73700=CARTESIAN_POINT('Ctrl Pts',(18.3,39.6725784480572,3.39495224915445));
#73701=CARTESIAN_POINT('Ctrl Pts',(18.1272,39.6725784480572,3.39495224915445));
#73702=CARTESIAN_POINT('',(18.3,39.9306957662105,3.47353329919279));
#73703=CARTESIAN_POINT('Ctrl Pts',(18.3,39.9306957662105,3.47353329919279));
#73704=CARTESIAN_POINT('Ctrl Pts',(18.3,39.8275579750538,3.39495224915445));
#73705=CARTESIAN_POINT('Ctrl Pts',(18.3,39.6725784480572,3.39495224915445));
#73706=CARTESIAN_POINT('',(18.18,39.9306957662105,3.47353329919279));
#73707=CARTESIAN_POINT('',(18.3,39.9306957662105,3.47353329919279));
#73708=CARTESIAN_POINT('Ctrl Pts',(18.18,39.9306957662105,3.47353329919279));
#73709=CARTESIAN_POINT('Ctrl Pts',(18.18,39.8275579750538,3.39495224915445));
#73710=CARTESIAN_POINT('Ctrl Pts',(18.18,39.6725784480572,3.39495224915445));
#73711=CARTESIAN_POINT('Ctrl Pts',(18.3,40.0665757298469,3.69399717114866));
#73712=CARTESIAN_POINT('Ctrl Pts',(18.1272,40.0665757298469,3.69399717114866));
#73713=CARTESIAN_POINT('Ctrl Pts',(18.3,40.0338335573673,3.55211449824274));
#73714=CARTESIAN_POINT('Ctrl Pts',(18.1272,40.0338335573673,3.55211449824274));
#73715=CARTESIAN_POINT('Ctrl Pts',(18.3,39.9306957662105,3.47353329919279));
#73716=CARTESIAN_POINT('Ctrl Pts',(18.1272,39.9306957662105,3.47353329919279));
#73717=CARTESIAN_POINT('',(18.3,40.0665757298469,3.69399717114866));
#73718=CARTESIAN_POINT('Ctrl Pts',(18.3,40.0665757298469,3.69399717114866));
#73719=CARTESIAN_POINT('Ctrl Pts',(18.3,40.0338335573673,3.55211449824274));
#73720=CARTESIAN_POINT('Ctrl Pts',(18.3,39.9306957662105,3.47353329919279));
#73721=CARTESIAN_POINT('',(18.18,40.0665757298469,3.69399717114866));
#73722=CARTESIAN_POINT('',(18.3,40.0665757298469,3.69399717114866));
#73723=CARTESIAN_POINT('Ctrl Pts',(18.18,40.0665757298469,3.69399717114866));
#73724=CARTESIAN_POINT('Ctrl Pts',(18.18,40.0338335573673,3.55211449824274));
#73725=CARTESIAN_POINT('Ctrl Pts',(18.18,39.9306957662105,3.47353329919279));
#73726=CARTESIAN_POINT('Ctrl Pts',(18.3,40.2019100129604,3.52919502221048));
#73727=CARTESIAN_POINT('Ctrl Pts',(18.1272,40.2019100129604,3.52919502221048));
#73728=CARTESIAN_POINT('Ctrl Pts',(18.3,40.1167802751064,3.58485667072237));
#73729=CARTESIAN_POINT('Ctrl Pts',(18.1272,40.1167802751064,3.58485667072237));
#73730=CARTESIAN_POINT('Ctrl Pts',(18.3,40.0665757298469,3.69399717114866));
#73731=CARTESIAN_POINT('Ctrl Pts',(18.1272,40.0665757298469,3.69399717114866));
#73732=CARTESIAN_POINT('',(18.3,40.2019100129604,3.52919502221048));
#73733=CARTESIAN_POINT('Ctrl Pts',(18.3,40.2019100129604,3.52919502221048));
#73734=CARTESIAN_POINT('Ctrl Pts',(18.3,40.1167802751064,3.58485667072237));
#73735=CARTESIAN_POINT('Ctrl Pts',(18.3,40.0665757298469,3.69399717114866));
#73736=CARTESIAN_POINT('',(18.18,40.2019100129604,3.52919502221048));
#73737=CARTESIAN_POINT('',(18.3,40.2019100129604,3.52919502221048));
#73738=CARTESIAN_POINT('Ctrl Pts',(18.18,40.2019100129604,3.52919502221048));
#73739=CARTESIAN_POINT('Ctrl Pts',(18.18,40.1167802751064,3.58485667072237));
#73740=CARTESIAN_POINT('Ctrl Pts',(18.18,40.0665757298469,3.69399717114866));
#73741=CARTESIAN_POINT('Ctrl Pts',(18.3,40.3907230734825,3.47353329919279));
#73742=CARTESIAN_POINT('Ctrl Pts',(18.1272,40.3907230734825,3.47353329919279));
#73743=CARTESIAN_POINT('Ctrl Pts',(18.3,40.2870396018028,3.47353329919279));
#73744=CARTESIAN_POINT('Ctrl Pts',(18.1272,40.2870396018028,3.47353329919279));
#73745=CARTESIAN_POINT('Ctrl Pts',(18.3,40.2019100129604,3.52919502221048));
#73746=CARTESIAN_POINT('Ctrl Pts',(18.1272,40.2019100129604,3.52919502221048));
#73747=CARTESIAN_POINT('',(18.3,40.3907230734825,3.47353329919279));
#73748=CARTESIAN_POINT('Ctrl Pts',(18.3,40.3907230734825,3.47353329919279));
#73749=CARTESIAN_POINT('Ctrl Pts',(18.3,40.2870396018028,3.47353329919279));
#73750=CARTESIAN_POINT('Ctrl Pts',(18.3,40.2019100129604,3.52919502221048));
#73751=CARTESIAN_POINT('',(18.18,40.3907230734825,3.47353329919279));
#73752=CARTESIAN_POINT('',(18.3,40.3907230734825,3.47353329919279));
#73753=CARTESIAN_POINT('Ctrl Pts',(18.18,40.3907230734825,3.47353329919279));
#73754=CARTESIAN_POINT('Ctrl Pts',(18.18,40.2870396018028,3.47353329919279));
#73755=CARTESIAN_POINT('Ctrl Pts',(18.18,40.2019100129604,3.52919502221048));
#73756=CARTESIAN_POINT('Ctrl Pts',(18.3,40.5969985067844,3.53192349933088));
#73757=CARTESIAN_POINT('Ctrl Pts',(18.1272,40.5969985067844,3.53192349933088));
#73758=CARTESIAN_POINT('Ctrl Pts',(18.3,40.499863499403,3.47353329919279));
#73759=CARTESIAN_POINT('Ctrl Pts',(18.1272,40.499863499403,3.47353329919279));
#73760=CARTESIAN_POINT('Ctrl Pts',(18.3,40.3907230734825,3.47353329919279));
#73761=CARTESIAN_POINT('Ctrl Pts',(18.1272,40.3907230734825,3.47353329919279));
#73762=CARTESIAN_POINT('',(18.3,40.5969985067844,3.53192349933088));
#73763=CARTESIAN_POINT('Ctrl Pts',(18.3,40.5969985067844,3.53192349933088));
#73764=CARTESIAN_POINT('Ctrl Pts',(18.3,40.499863499403,3.47353329919279));
#73765=CARTESIAN_POINT('Ctrl Pts',(18.3,40.3907230734825,3.47353329919279));
#73766=CARTESIAN_POINT('',(18.18,40.5969985067844,3.53192349933088));
#73767=CARTESIAN_POINT('',(18.3,40.5969985067844,3.53192349933088));
#73768=CARTESIAN_POINT('Ctrl Pts',(18.18,40.5969985067844,3.53192349933088));
#73769=CARTESIAN_POINT('Ctrl Pts',(18.18,40.499863499403,3.47353329919279));
#73770=CARTESIAN_POINT('Ctrl Pts',(18.18,40.3907230734825,3.47353329919279));
#73771=CARTESIAN_POINT('Ctrl Pts',(18.3,40.7503409922123,3.70054563544691));
#73772=CARTESIAN_POINT('Ctrl Pts',(18.1272,40.7503409922123,3.70054563544691));
#73773=CARTESIAN_POINT('Ctrl Pts',(18.3,40.6941336631775,3.59031369946897));
#73774=CARTESIAN_POINT('Ctrl Pts',(18.1272,40.6941336631775,3.59031369946897));
#73775=CARTESIAN_POINT('Ctrl Pts',(18.3,40.5969985067844,3.53192349933088));
#73776=CARTESIAN_POINT('Ctrl Pts',(18.1272,40.5969985067844,3.53192349933088));
#73777=CARTESIAN_POINT('',(18.3,40.7503409922123,3.70054563544691));
#73778=CARTESIAN_POINT('Ctrl Pts',(18.3,40.7503409922123,3.70054563544691));
#73779=CARTESIAN_POINT('Ctrl Pts',(18.3,40.6941336631775,3.59031369946897));
#73780=CARTESIAN_POINT('Ctrl Pts',(18.3,40.5969985067844,3.53192349933088));
#73781=CARTESIAN_POINT('',(18.18,40.7503409922123,3.70054563544691));
#73782=CARTESIAN_POINT('',(18.3,40.7503409922123,3.70054563544691));
#73783=CARTESIAN_POINT('Ctrl Pts',(18.18,40.7503409922123,3.70054563544691));
#73784=CARTESIAN_POINT('Ctrl Pts',(18.18,40.6941336631775,3.59031369946897));
#73785=CARTESIAN_POINT('Ctrl Pts',(18.18,40.5969985067844,3.53192349933088));
#73786=CARTESIAN_POINT('Ctrl Pts',(18.3,40.8065483212471,3.94174618683755));
#73787=CARTESIAN_POINT('Ctrl Pts',(18.1272,40.8065483212471,3.94174618683755));
#73788=CARTESIAN_POINT('Ctrl Pts',(18.3,40.8065483212471,3.81077749691904));
#73789=CARTESIAN_POINT('Ctrl Pts',(18.1272,40.8065483212471,3.81077749691904));
#73790=CARTESIAN_POINT('Ctrl Pts',(18.3,40.7503409922123,3.70054563544691));
#73791=CARTESIAN_POINT('Ctrl Pts',(18.1272,40.7503409922123,3.70054563544691));
#73792=CARTESIAN_POINT('',(18.3,40.8065483212471,3.94174618683755));
#73793=CARTESIAN_POINT('Ctrl Pts',(18.3,40.8065483212471,3.94174618683755));
#73794=CARTESIAN_POINT('Ctrl Pts',(18.3,40.8065483212471,3.81077749691904));
#73795=CARTESIAN_POINT('Ctrl Pts',(18.3,40.7503409922123,3.70054563544691));
#73796=CARTESIAN_POINT('',(18.18,40.8065483212471,3.94174618683755));
#73797=CARTESIAN_POINT('',(18.3,40.8065483212471,3.94174618683755));
#73798=CARTESIAN_POINT('Ctrl Pts',(18.18,40.8065483212471,3.94174618683755));
#73799=CARTESIAN_POINT('Ctrl Pts',(18.18,40.8065483212471,3.81077749691904));
#73800=CARTESIAN_POINT('Ctrl Pts',(18.18,40.7503409922123,3.70054563544691));
#73801=CARTESIAN_POINT('Ctrl Pts',(18.3,40.6979535758495,4.25934502892196));
#73802=CARTESIAN_POINT('Ctrl Pts',(18.1272,40.6979535758495,4.25934502892196));
#73803=CARTESIAN_POINT('Ctrl Pts',(18.3,40.8065483212471,4.13165064565837));
#73804=CARTESIAN_POINT('Ctrl Pts',(18.1272,40.8065483212471,4.13165064565837));
#73805=CARTESIAN_POINT('Ctrl Pts',(18.3,40.8065483212471,3.94174618683755));
#73806=CARTESIAN_POINT('Ctrl Pts',(18.1272,40.8065483212471,3.94174618683755));
#73807=CARTESIAN_POINT('',(18.3,40.6979535758495,4.25934502892196));
#73808=CARTESIAN_POINT('Ctrl Pts',(18.3,40.6979535758495,4.25934502892196));
#73809=CARTESIAN_POINT('Ctrl Pts',(18.3,40.8065483212471,4.13165064565837));
#73810=CARTESIAN_POINT('Ctrl Pts',(18.3,40.8065483212471,3.94174618683755));
#73811=CARTESIAN_POINT('',(18.18,40.6979535758495,4.25934502892196));
#73812=CARTESIAN_POINT('',(18.3,40.6979535758495,4.25934502892196));
#73813=CARTESIAN_POINT('Ctrl Pts',(18.18,40.6979535758495,4.25934502892196));
#73814=CARTESIAN_POINT('Ctrl Pts',(18.18,40.8065483212471,4.13165064565837));
#73815=CARTESIAN_POINT('Ctrl Pts',(18.18,40.8065483212471,3.94174618683755));
#73816=CARTESIAN_POINT('Ctrl Pts',(18.3,40.39181458354,4.4230558168143));
#73817=CARTESIAN_POINT('Ctrl Pts',(18.1272,40.39181458354,4.4230558168143));
#73818=CARTESIAN_POINT('Ctrl Pts',(18.3,40.5893586814403,4.38703944943845));
#73819=CARTESIAN_POINT('Ctrl Pts',(18.1272,40.5893586814403,4.38703944943845));
#73820=CARTESIAN_POINT('Ctrl Pts',(18.3,40.6979535758495,4.25934502892196));
#73821=CARTESIAN_POINT('Ctrl Pts',(18.1272,40.6979535758495,4.25934502892196));
#73822=CARTESIAN_POINT('',(18.3,40.39181458354,4.4230558168143));
#73823=CARTESIAN_POINT('Ctrl Pts',(18.3,40.39181458354,4.4230558168143));
#73824=CARTESIAN_POINT('Ctrl Pts',(18.3,40.5893586814403,4.38703944943845));
#73825=CARTESIAN_POINT('Ctrl Pts',(18.3,40.6979535758495,4.25934502892196));
#73826=CARTESIAN_POINT('',(18.18,40.39181458354,4.4230558168143));
#73827=CARTESIAN_POINT('',(18.3,40.39181458354,4.4230558168143));
#73828=CARTESIAN_POINT('Ctrl Pts',(18.18,40.39181458354,4.4230558168143));
#73829=CARTESIAN_POINT('Ctrl Pts',(18.18,40.5893586814403,4.38703944943845));
#73830=CARTESIAN_POINT('Ctrl Pts',(18.18,40.6979535758495,4.25934502892196));
#73831=CARTESIAN_POINT('Origin',(18.3,40.356889539957,4.22660289369523));
#73832=CARTESIAN_POINT('',(18.3,40.356889539957,4.22660289369523));
#73833=CARTESIAN_POINT('',(18.3,40.9206979115535,7.39801776727049));
#73834=CARTESIAN_POINT('',(18.18,40.356889539957,4.22660289369523));
#73835=CARTESIAN_POINT('',(18.3,40.356889539957,4.22660289369523));
#73836=CARTESIAN_POINT('',(18.18,40.356889539957,4.22660289369523));
#73837=CARTESIAN_POINT('Ctrl Pts',(18.3,40.5729876697063,4.12837641350925));
#73838=CARTESIAN_POINT('Ctrl Pts',(18.1272,40.5729876697063,4.12837641350925));
#73839=CARTESIAN_POINT('Ctrl Pts',(18.3,40.5009548604488,4.20477477870882));
#73840=CARTESIAN_POINT('Ctrl Pts',(18.1272,40.5009548604488,4.20477477870882));
#73841=CARTESIAN_POINT('Ctrl Pts',(18.3,40.356889539957,4.22660289369523));
#73842=CARTESIAN_POINT('Ctrl Pts',(18.1272,40.356889539957,4.22660289369523));
#73843=CARTESIAN_POINT('',(18.3,40.5729876697063,4.12837641350925));
#73844=CARTESIAN_POINT('Ctrl Pts',(18.3,40.5729876697063,4.12837641350925));
#73845=CARTESIAN_POINT('Ctrl Pts',(18.3,40.5009548604488,4.20477477870882));
#73846=CARTESIAN_POINT('Ctrl Pts',(18.3,40.356889539957,4.22660289369523));
#73847=CARTESIAN_POINT('',(18.18,40.5729876697063,4.12837641350925));
#73848=CARTESIAN_POINT('',(18.3,40.5729876697063,4.12837641350925));
#73849=CARTESIAN_POINT('Ctrl Pts',(18.18,40.5729876697063,4.12837641350925));
#73850=CARTESIAN_POINT('Ctrl Pts',(18.18,40.5009548604488,4.20477477870882));
#73851=CARTESIAN_POINT('Ctrl Pts',(18.18,40.356889539957,4.22660289369523));
#73852=CARTESIAN_POINT('Ctrl Pts',(18.3,40.6450203299522,3.93738051913679));
#73853=CARTESIAN_POINT('Ctrl Pts',(18.1272,40.6450203299522,3.93738051913679));
#73854=CARTESIAN_POINT('Ctrl Pts',(18.3,40.6450203299522,4.05197804830968));
#73855=CARTESIAN_POINT('Ctrl Pts',(18.1272,40.6450203299522,4.05197804830968));
#73856=CARTESIAN_POINT('Ctrl Pts',(18.3,40.5729876697063,4.12837641350925));
#73857=CARTESIAN_POINT('Ctrl Pts',(18.1272,40.5729876697063,4.12837641350925));
#73858=CARTESIAN_POINT('',(18.3,40.6450203299522,3.93738051913679));
#73859=CARTESIAN_POINT('Ctrl Pts',(18.3,40.6450203299522,3.93738051913679));
#73860=CARTESIAN_POINT('Ctrl Pts',(18.3,40.6450203299522,4.05197804830968));
#73861=CARTESIAN_POINT('Ctrl Pts',(18.3,40.5729876697063,4.12837641350925));
#73862=CARTESIAN_POINT('',(18.18,40.6450203299522,3.93738051913679));
#73863=CARTESIAN_POINT('',(18.3,40.6450203299522,3.93738051913679));
#73864=CARTESIAN_POINT('Ctrl Pts',(18.18,40.6450203299522,3.93738051913679));
#73865=CARTESIAN_POINT('Ctrl Pts',(18.18,40.6450203299522,4.05197804830968));
#73866=CARTESIAN_POINT('Ctrl Pts',(18.18,40.5729876697063,4.12837641350925));
#73867=CARTESIAN_POINT('Ctrl Pts',(18.3,40.5740790307522,3.74856745861471));
#73868=CARTESIAN_POINT('Ctrl Pts',(18.1272,40.5740790307522,3.74856745861471));
#73869=CARTESIAN_POINT('Ctrl Pts',(18.3,40.6450203299522,3.82169162891805));
#73870=CARTESIAN_POINT('Ctrl Pts',(18.1272,40.6450203299522,3.82169162891805));
#73871=CARTESIAN_POINT('Ctrl Pts',(18.3,40.6450203299522,3.93738051913679));
#73872=CARTESIAN_POINT('Ctrl Pts',(18.1272,40.6450203299522,3.93738051913679));
#73873=CARTESIAN_POINT('',(18.3,40.5740790307522,3.74856745861471));
#73874=CARTESIAN_POINT('Ctrl Pts',(18.3,40.5740790307522,3.74856745861471));
#73875=CARTESIAN_POINT('Ctrl Pts',(18.3,40.6450203299522,3.82169162891805));
#73876=CARTESIAN_POINT('Ctrl Pts',(18.3,40.6450203299522,3.93738051913679));
#73877=CARTESIAN_POINT('',(18.18,40.5740790307522,3.74856745861471));
#73878=CARTESIAN_POINT('',(18.3,40.5740790307522,3.74856745861471));
#73879=CARTESIAN_POINT('Ctrl Pts',(18.18,40.5740790307522,3.74856745861471));
#73880=CARTESIAN_POINT('Ctrl Pts',(18.18,40.6450203299522,3.82169162891805));
#73881=CARTESIAN_POINT('Ctrl Pts',(18.18,40.6450203299522,3.93738051913679));
#73882=CARTESIAN_POINT('Ctrl Pts',(18.3,40.3950886666775,3.67544328831136));
#73883=CARTESIAN_POINT('Ctrl Pts',(18.1272,40.3950886666775,3.67544328831136));
#73884=CARTESIAN_POINT('Ctrl Pts',(18.3,40.5031377315521,3.67544328831136));
#73885=CARTESIAN_POINT('Ctrl Pts',(18.1272,40.5031377315521,3.67544328831136));
#73886=CARTESIAN_POINT('Ctrl Pts',(18.3,40.5740790307522,3.74856745861471));
#73887=CARTESIAN_POINT('Ctrl Pts',(18.1272,40.5740790307522,3.74856745861471));
#73888=CARTESIAN_POINT('',(18.3,40.3950886666775,3.67544328831136));
#73889=CARTESIAN_POINT('Ctrl Pts',(18.3,40.3950886666775,3.67544328831136));
#73890=CARTESIAN_POINT('Ctrl Pts',(18.3,40.5031377315521,3.67544328831136));
#73891=CARTESIAN_POINT('Ctrl Pts',(18.3,40.5740790307522,3.74856745861471));
#73892=CARTESIAN_POINT('',(18.18,40.3950886666775,3.67544328831136));
#73893=CARTESIAN_POINT('',(18.3,40.3950886666775,3.67544328831136));
#73894=CARTESIAN_POINT('Ctrl Pts',(18.18,40.3950886666775,3.67544328831136));
#73895=CARTESIAN_POINT('Ctrl Pts',(18.18,40.5031377315521,3.67544328831136));
#73896=CARTESIAN_POINT('Ctrl Pts',(18.18,40.5740790307522,3.74856745861471));
#73897=CARTESIAN_POINT('Ctrl Pts',(18.3,40.1931788265705,3.77585252784193));
#73898=CARTESIAN_POINT('Ctrl Pts',(18.1272,40.1931788265705,3.77585252784193));
#73899=CARTESIAN_POINT('Ctrl Pts',(18.3,40.2586630225181,3.67544328831136));
#73900=CARTESIAN_POINT('Ctrl Pts',(18.1272,40.2586630225181,3.67544328831136));
#73901=CARTESIAN_POINT('Ctrl Pts',(18.3,40.3950886666775,3.67544328831136));
#73902=CARTESIAN_POINT('Ctrl Pts',(18.1272,40.3950886666775,3.67544328831136));
#73903=CARTESIAN_POINT('',(18.3,40.1931788265705,3.77585252784193));
#73904=CARTESIAN_POINT('Ctrl Pts',(18.3,40.1931788265705,3.77585252784193));
#73905=CARTESIAN_POINT('Ctrl Pts',(18.3,40.2586630225181,3.67544328831136));
#73906=CARTESIAN_POINT('Ctrl Pts',(18.3,40.3950886666775,3.67544328831136));
#73907=CARTESIAN_POINT('',(18.18,40.1931788265705,3.77585252784193));
#73908=CARTESIAN_POINT('',(18.3,40.1931788265705,3.77585252784193));
#73909=CARTESIAN_POINT('Ctrl Pts',(18.18,40.1931788265705,3.77585252784193));
#73910=CARTESIAN_POINT('Ctrl Pts',(18.18,40.2586630225181,3.67544328831136));
#73911=CARTESIAN_POINT('Ctrl Pts',(18.18,40.3950886666775,3.67544328831136));
#73912=CARTESIAN_POINT('Ctrl Pts',(18.3,40.1276944816112,4.0017734285444));
#73913=CARTESIAN_POINT('Ctrl Pts',(18.1272,40.1276944816112,4.0017734285444));
#73914=CARTESIAN_POINT('Ctrl Pts',(18.3,40.1276944816112,3.87626184187829));
#73915=CARTESIAN_POINT('Ctrl Pts',(18.1272,40.1276944816112,3.87626184187829));
#73916=CARTESIAN_POINT('Ctrl Pts',(18.3,40.1931788265705,3.77585252784193));
#73917=CARTESIAN_POINT('Ctrl Pts',(18.1272,40.1931788265705,3.77585252784193));
#73918=CARTESIAN_POINT('',(18.3,40.1276944816112,4.0017734285444));
#73919=CARTESIAN_POINT('Ctrl Pts',(18.3,40.1276944816112,4.0017734285444));
#73920=CARTESIAN_POINT('Ctrl Pts',(18.3,40.1276944816112,3.87626184187829));
#73921=CARTESIAN_POINT('Ctrl Pts',(18.3,40.1931788265705,3.77585252784193));
#73922=CARTESIAN_POINT('',(18.18,40.1276944816112,4.0017734285444));
#73923=CARTESIAN_POINT('',(18.3,40.1276944816112,4.0017734285444));
#73924=CARTESIAN_POINT('Ctrl Pts',(18.18,40.1276944816112,4.0017734285444));
#73925=CARTESIAN_POINT('Ctrl Pts',(18.18,40.1276944816112,3.87626184187829));
#73926=CARTESIAN_POINT('Ctrl Pts',(18.18,40.1931788265705,3.77585252784193));
#73927=CARTESIAN_POINT('Ctrl Pts',(18.3,40.1298772037029,4.03342416547239));
#73928=CARTESIAN_POINT('Ctrl Pts',(18.1272,40.1298772037029,4.03342416547239));
#73929=CARTESIAN_POINT('Ctrl Pts',(18.3,40.1276944816112,4.01377884708345));
#73930=CARTESIAN_POINT('Ctrl Pts',(18.1272,40.1276944816112,4.01377884708345));
#73931=CARTESIAN_POINT('Ctrl Pts',(18.3,40.1276944816112,4.0017734285444));
#73932=CARTESIAN_POINT('Ctrl Pts',(18.1272,40.1276944816112,4.0017734285444));
#73933=CARTESIAN_POINT('',(18.3,40.1298772037029,4.03342416547239));
#73934=CARTESIAN_POINT('Ctrl Pts',(18.3,40.1298772037029,4.03342416547239));
#73935=CARTESIAN_POINT('Ctrl Pts',(18.3,40.1276944816112,4.01377884708345));
#73936=CARTESIAN_POINT('Ctrl Pts',(18.3,40.1276944816112,4.0017734285444));
#73937=CARTESIAN_POINT('',(18.18,40.1298772037029,4.03342416547239));
#73938=CARTESIAN_POINT('',(18.3,40.1298772037029,4.03342416547239));
#73939=CARTESIAN_POINT('Ctrl Pts',(18.18,40.1298772037029,4.03342416547239));
#73940=CARTESIAN_POINT('Ctrl Pts',(18.18,40.1276944816112,4.01377884708345));
#73941=CARTESIAN_POINT('Ctrl Pts',(18.18,40.1276944816112,4.0017734285444));
#73942=CARTESIAN_POINT('Origin',(18.3,39.9574353039265,4.05525228045881));
#73943=CARTESIAN_POINT('',(18.3,39.9574353039265,4.05525228045881));
#73944=CARTESIAN_POINT('',(18.3,54.6518279137828,2.19520033276317));
#73945=CARTESIAN_POINT('',(18.18,39.9574353039265,4.05525228045881));
#73946=CARTESIAN_POINT('',(18.3,39.9574353039265,4.05525228045881));
#73947=CARTESIAN_POINT('',(18.18,39.9574353039265,4.05525228045881));
#73948=CARTESIAN_POINT('Ctrl Pts',(18.3,39.9792634189129,3.91664383970201));
#73949=CARTESIAN_POINT('Ctrl Pts',(18.1272,39.9792634189129,3.91664383970201));
#73950=CARTESIAN_POINT('Ctrl Pts',(18.3,39.9792634189129,3.9723054882139));
#73951=CARTESIAN_POINT('Ctrl Pts',(18.1272,39.9792634189129,3.9723054882139));
#73952=CARTESIAN_POINT('Ctrl Pts',(18.3,39.9574353039265,4.05525228045881));
#73953=CARTESIAN_POINT('Ctrl Pts',(18.1272,39.9574353039265,4.05525228045881));
#73954=CARTESIAN_POINT('',(18.3,39.9792634189129,3.91664383970201));
#73955=CARTESIAN_POINT('Ctrl Pts',(18.3,39.9792634189129,3.91664383970201));
#73956=CARTESIAN_POINT('Ctrl Pts',(18.3,39.9792634189129,3.9723054882139));
#73957=CARTESIAN_POINT('Ctrl Pts',(18.3,39.9574353039265,4.05525228045881));
#73958=CARTESIAN_POINT('',(18.18,39.9792634189129,3.91664383970201));
#73959=CARTESIAN_POINT('',(18.3,39.9792634189129,3.91664383970201));
#73960=CARTESIAN_POINT('Ctrl Pts',(18.18,39.9792634189129,3.91664383970201));
#73961=CARTESIAN_POINT('Ctrl Pts',(18.18,39.9792634189129,3.9723054882139));
#73962=CARTESIAN_POINT('Ctrl Pts',(18.18,39.9574353039265,4.05525228045881));
#73963=CARTESIAN_POINT('Ctrl Pts',(18.3,39.8914052784443,3.69181437455118));
#73964=CARTESIAN_POINT('Ctrl Pts',(18.1272,39.8914052784443,3.69181437455118));
#73965=CARTESIAN_POINT('Ctrl Pts',(18.3,39.9792634189129,3.78021819554269));
#73966=CARTESIAN_POINT('Ctrl Pts',(18.1272,39.9792634189129,3.78021819554269));
#73967=CARTESIAN_POINT('Ctrl Pts',(18.3,39.9792634189129,3.91664383970201));
#73968=CARTESIAN_POINT('Ctrl Pts',(18.1272,39.9792634189129,3.91664383970201));
#73969=CARTESIAN_POINT('',(18.3,39.8914052784443,3.69181437455118));
#73970=CARTESIAN_POINT('Ctrl Pts',(18.3,39.8914052784443,3.69181437455118));
#73971=CARTESIAN_POINT('Ctrl Pts',(18.3,39.9792634189129,3.78021819554269));
#73972=CARTESIAN_POINT('Ctrl Pts',(18.3,39.9792634189129,3.91664383970201));
#73973=CARTESIAN_POINT('',(18.18,39.8914052784443,3.69181437455118));
#73974=CARTESIAN_POINT('',(18.3,39.8914052784443,3.69181437455118));
#73975=CARTESIAN_POINT('Ctrl Pts',(18.18,39.8914052784443,3.69181437455118));
#73976=CARTESIAN_POINT('Ctrl Pts',(18.18,39.9792634189129,3.78021819554269));
#73977=CARTESIAN_POINT('Ctrl Pts',(18.18,39.9792634189129,3.91664383970201));
#73978=CARTESIAN_POINT('Ctrl Pts',(18.3,39.6682130038738,3.60341055355966));
#73979=CARTESIAN_POINT('Ctrl Pts',(18.1272,39.6682130038738,3.60341055355966));
#73980=CARTESIAN_POINT('Ctrl Pts',(18.3,39.8035471379757,3.60341055355966));
#73981=CARTESIAN_POINT('Ctrl Pts',(18.1272,39.8035471379757,3.60341055355966));
#73982=CARTESIAN_POINT('Ctrl Pts',(18.3,39.8914052784443,3.69181437455118));
#73983=CARTESIAN_POINT('Ctrl Pts',(18.1272,39.8914052784443,3.69181437455118));
#73984=CARTESIAN_POINT('',(18.3,39.6682130038738,3.60341055355966));
#73985=CARTESIAN_POINT('Ctrl Pts',(18.3,39.6682130038738,3.60341055355966));
#73986=CARTESIAN_POINT('Ctrl Pts',(18.3,39.8035471379757,3.60341055355966));
#73987=CARTESIAN_POINT('Ctrl Pts',(18.3,39.8914052784443,3.69181437455118));
#73988=CARTESIAN_POINT('',(18.18,39.6682130038738,3.60341055355966));
#73989=CARTESIAN_POINT('',(18.3,39.6682130038738,3.60341055355966));
#73990=CARTESIAN_POINT('Ctrl Pts',(18.18,39.6682130038738,3.60341055355966));
#73991=CARTESIAN_POINT('Ctrl Pts',(18.18,39.8035471379757,3.60341055355966));
#73992=CARTESIAN_POINT('Ctrl Pts',(18.18,39.8914052784443,3.69181437455118));
#73993=CARTESIAN_POINT('Ctrl Pts',(18.3,39.4302864611149,3.69890851937234));
#73994=CARTESIAN_POINT('Ctrl Pts',(18.1272,39.4302864611149,3.69890851937234));
#73995=CARTESIAN_POINT('Ctrl Pts',(18.3,39.5263301074505,3.60341055355966));
#73996=CARTESIAN_POINT('Ctrl Pts',(18.1272,39.5263301074505,3.60341055355966));
#73997=CARTESIAN_POINT('Ctrl Pts',(18.3,39.6682130038738,3.60341055355966));
#73998=CARTESIAN_POINT('Ctrl Pts',(18.1272,39.6682130038738,3.60341055355966));
#73999=CARTESIAN_POINT('',(18.3,39.4302864611149,3.69890851937234));
#74000=CARTESIAN_POINT('Ctrl Pts',(18.3,39.4302864611149,3.69890851937234));
#74001=CARTESIAN_POINT('Ctrl Pts',(18.3,39.5263301074505,3.60341055355966));
#74002=CARTESIAN_POINT('Ctrl Pts',(18.3,39.6682130038738,3.60341055355966));
#74003=CARTESIAN_POINT('',(18.18,39.4302864611149,3.69890851937234));
#74004=CARTESIAN_POINT('',(18.3,39.4302864611149,3.69890851937234));
#74005=CARTESIAN_POINT('Ctrl Pts',(18.18,39.4302864611149,3.69890851937234));
#74006=CARTESIAN_POINT('Ctrl Pts',(18.18,39.5263301074505,3.60341055355966));
#74007=CARTESIAN_POINT('Ctrl Pts',(18.18,39.6682130038738,3.60341055355966));
#74008=CARTESIAN_POINT('Ctrl Pts',(18.3,39.3342428147793,3.93301485143602));
#74009=CARTESIAN_POINT('Ctrl Pts',(18.1272,39.3342428147793,3.93301485143602));
#74010=CARTESIAN_POINT('Ctrl Pts',(18.3,39.3342428147793,3.79440641067922));
#74011=CARTESIAN_POINT('Ctrl Pts',(18.1272,39.3342428147793,3.79440641067922));
#74012=CARTESIAN_POINT('Ctrl Pts',(18.3,39.4302864611149,3.69890851937234));
#74013=CARTESIAN_POINT('Ctrl Pts',(18.1272,39.4302864611149,3.69890851937234));
#74014=CARTESIAN_POINT('',(18.3,39.3342428147793,3.93301485143602));
#74015=CARTESIAN_POINT('Ctrl Pts',(18.3,39.3342428147793,3.93301485143602));
#74016=CARTESIAN_POINT('Ctrl Pts',(18.3,39.3342428147793,3.79440641067922));
#74017=CARTESIAN_POINT('Ctrl Pts',(18.3,39.4302864611149,3.69890851937234));
#74018=CARTESIAN_POINT('',(18.18,39.3342428147793,3.93301485143602));
#74019=CARTESIAN_POINT('',(18.3,39.3342428147793,3.93301485143602));
#74020=CARTESIAN_POINT('Ctrl Pts',(18.18,39.3342428147793,3.93301485143602));
#74021=CARTESIAN_POINT('Ctrl Pts',(18.18,39.3342428147793,3.79440641067922));
#74022=CARTESIAN_POINT('Ctrl Pts',(18.18,39.4302864611149,3.69890851937234));
#74023=CARTESIAN_POINT('Ctrl Pts',(18.3,39.4079126656055,4.13110492788255));
#74024=CARTESIAN_POINT('Ctrl Pts',(18.1272,39.4079126656055,4.13110492788255));
#74025=CARTESIAN_POINT('Ctrl Pts',(18.3,39.3342428147793,4.0497952517122));
#74026=CARTESIAN_POINT('Ctrl Pts',(18.1272,39.3342428147793,4.0497952517122));
#74027=CARTESIAN_POINT('Ctrl Pts',(18.3,39.3342428147793,3.93301485143602));
#74028=CARTESIAN_POINT('Ctrl Pts',(18.1272,39.3342428147793,3.93301485143602));
#74029=CARTESIAN_POINT('',(18.3,39.4079126656055,4.13110492788255));
#74030=CARTESIAN_POINT('Ctrl Pts',(18.3,39.4079126656055,4.13110492788255));
#74031=CARTESIAN_POINT('Ctrl Pts',(18.3,39.3342428147793,4.0497952517122));
#74032=CARTESIAN_POINT('Ctrl Pts',(18.3,39.3342428147793,3.93301485143602));
#74033=CARTESIAN_POINT('',(18.18,39.4079126656055,4.13110492788255));
#74034=CARTESIAN_POINT('',(18.3,39.4079126656055,4.13110492788255));
#74035=CARTESIAN_POINT('Ctrl Pts',(18.18,39.4079126656055,4.13110492788255));
#74036=CARTESIAN_POINT('Ctrl Pts',(18.18,39.3342428147793,4.0497952517122));
#74037=CARTESIAN_POINT('Ctrl Pts',(18.18,39.3342428147793,3.93301485143602));
#74038=CARTESIAN_POINT('Ctrl Pts',(18.3,39.6485676109791,4.24624817483127));
#74039=CARTESIAN_POINT('Ctrl Pts',(18.1272,39.6485676109791,4.24624817483127));
#74040=CARTESIAN_POINT('Ctrl Pts',(18.3,39.4815825164318,4.2124146413058));
#74041=CARTESIAN_POINT('Ctrl Pts',(18.1272,39.4815825164318,4.2124146413058));
#74042=CARTESIAN_POINT('Ctrl Pts',(18.3,39.4079126656055,4.13110492788255));
#74043=CARTESIAN_POINT('Ctrl Pts',(18.1272,39.4079126656055,4.13110492788255));
#74044=CARTESIAN_POINT('',(18.3,39.6485676109791,4.24624817483127));
#74045=CARTESIAN_POINT('Ctrl Pts',(18.3,39.6485676109791,4.24624817483127));
#74046=CARTESIAN_POINT('Ctrl Pts',(18.3,39.4815825164318,4.2124146413058));
#74047=CARTESIAN_POINT('Ctrl Pts',(18.3,39.4079126656055,4.13110492788255));
#74048=CARTESIAN_POINT('',(18.18,39.6485676109791,4.24624817483127));
#74049=CARTESIAN_POINT('',(18.3,39.6485676109791,4.24624817483127));
#74050=CARTESIAN_POINT('Ctrl Pts',(18.18,39.6485676109791,4.24624817483127));
#74051=CARTESIAN_POINT('Ctrl Pts',(18.18,39.4815825164318,4.2124146413058));
#74052=CARTESIAN_POINT('Ctrl Pts',(18.18,39.4079126656055,4.13110492788255));
#74053=CARTESIAN_POINT('Origin',(18.3,39.6223737537861,4.44270109795034));
#74054=CARTESIAN_POINT('',(18.3,39.6223737537861,4.44270109795034));
#74055=CARTESIAN_POINT('',(18.3,39.818427473701,2.97230572693353));
#74056=CARTESIAN_POINT('',(18.18,39.6223737537861,4.44270109795034));
#74057=CARTESIAN_POINT('',(18.3,39.6223737537861,4.44270109795034));
#74058=CARTESIAN_POINT('',(18.18,39.6223737537861,4.44270109795034));
#74059=CARTESIAN_POINT('Ctrl Pts',(18.3,39.2971350491047,4.28390165828168));
#74060=CARTESIAN_POINT('Ctrl Pts',(18.1272,39.2971350491047,4.28390165828168));
#74061=CARTESIAN_POINT('Ctrl Pts',(18.3,39.4226466357708,4.4230558168143));
#74062=CARTESIAN_POINT('Ctrl Pts',(18.1272,39.4226466357708,4.4230558168143));
#74063=CARTESIAN_POINT('Ctrl Pts',(18.3,39.6223737537861,4.44270109795034));
#74064=CARTESIAN_POINT('Ctrl Pts',(18.1272,39.6223737537861,4.44270109795034));
#74065=CARTESIAN_POINT('Ctrl Pts',(18.3,39.2971350491047,4.28390165828168));
#74066=CARTESIAN_POINT('Ctrl Pts',(18.3,39.4226466357708,4.4230558168143));
#74067=CARTESIAN_POINT('Ctrl Pts',(18.3,39.6223737537861,4.44270109795034));
#74068=CARTESIAN_POINT('Ctrl Pts',(18.18,39.2971350491047,4.28390165828168));
#74069=CARTESIAN_POINT('Ctrl Pts',(18.18,39.4226466357708,4.4230558168143));
#74070=CARTESIAN_POINT('Ctrl Pts',(18.18,39.6223737537861,4.44270109795034));
#74071=CARTESIAN_POINT('Origin',(18.18,39.9890859663486,3.29999992661178));
#74072=CARTESIAN_POINT('Origin',(18.3,70.,5.5));
#74073=CARTESIAN_POINT('Ctrl Pts',(18.3,30.643929117918,2.64843108169734));
#74074=CARTESIAN_POINT('Ctrl Pts',(18.1272,30.643929117918,2.64843108169734));
#74075=CARTESIAN_POINT('Ctrl Pts',(18.3,30.643929117918,2.78376536481082));
#74076=CARTESIAN_POINT('Ctrl Pts',(18.1272,30.643929117918,2.78376536481082));
#74077=CARTESIAN_POINT('Ctrl Pts',(18.3,30.5293315887451,2.86452936045825));
#74078=CARTESIAN_POINT('Ctrl Pts',(18.1272,30.5293315887451,2.86452936045825));
#74079=CARTESIAN_POINT('',(18.3,30.643929117918,2.64843108169734));
#74080=CARTESIAN_POINT('',(18.3,30.5293315887451,2.86452936045825));
#74081=CARTESIAN_POINT('Ctrl Pts',(18.3,30.643929117918,2.64843108169734));
#74082=CARTESIAN_POINT('Ctrl Pts',(18.3,30.643929117918,2.78376536481082));
#74083=CARTESIAN_POINT('Ctrl Pts',(18.3,30.5293315887451,2.86452936045825));
#74084=CARTESIAN_POINT('',(18.18,30.643929117918,2.64843108169734));
#74085=CARTESIAN_POINT('',(18.3,30.643929117918,2.64843108169734));
#74086=CARTESIAN_POINT('',(18.18,30.5293315887451,2.86452936045825));
#74087=CARTESIAN_POINT('Ctrl Pts',(18.18,30.643929117918,2.64843108169734));
#74088=CARTESIAN_POINT('Ctrl Pts',(18.18,30.643929117918,2.78376536481082));
#74089=CARTESIAN_POINT('Ctrl Pts',(18.18,30.5293315887451,2.86452936045825));
#74090=CARTESIAN_POINT('',(18.3,30.5293315887451,2.86452936045825));
#74091=CARTESIAN_POINT('Ctrl Pts',(18.3,30.514051938057,2.41869034282863));
#74092=CARTESIAN_POINT('Ctrl Pts',(18.1272,30.514051938057,2.41869034282863));
#74093=CARTESIAN_POINT('Ctrl Pts',(18.3,30.643929117918,2.51091407649219));
#74094=CARTESIAN_POINT('Ctrl Pts',(18.1272,30.643929117918,2.51091407649219));
#74095=CARTESIAN_POINT('Ctrl Pts',(18.3,30.643929117918,2.64843108169734));
#74096=CARTESIAN_POINT('Ctrl Pts',(18.1272,30.643929117918,2.64843108169734));
#74097=CARTESIAN_POINT('',(18.3,30.514051938057,2.41869034282863));
#74098=CARTESIAN_POINT('Ctrl Pts',(18.3,30.514051938057,2.41869034282863));
#74099=CARTESIAN_POINT('Ctrl Pts',(18.3,30.643929117918,2.51091407649219));
#74100=CARTESIAN_POINT('Ctrl Pts',(18.3,30.643929117918,2.64843108169734));
#74101=CARTESIAN_POINT('',(18.18,30.514051938057,2.41869034282863));
#74102=CARTESIAN_POINT('',(18.3,30.514051938057,2.41869034282863));
#74103=CARTESIAN_POINT('Ctrl Pts',(18.18,30.514051938057,2.41869034282863));
#74104=CARTESIAN_POINT('Ctrl Pts',(18.18,30.643929117918,2.51091407649219));
#74105=CARTESIAN_POINT('Ctrl Pts',(18.18,30.643929117918,2.64843108169734));
#74106=CARTESIAN_POINT('Ctrl Pts',(18.3,29.9890859663487,2.32646660916507));
#74107=CARTESIAN_POINT('Ctrl Pts',(18.1272,29.9890859663487,2.32646660916507));
#74108=CARTESIAN_POINT('Ctrl Pts',(18.3,30.3841746091843,2.32646660916507));
#74109=CARTESIAN_POINT('Ctrl Pts',(18.1272,30.3841746091843,2.32646660916507));
#74110=CARTESIAN_POINT('Ctrl Pts',(18.3,30.514051938057,2.41869034282863));
#74111=CARTESIAN_POINT('Ctrl Pts',(18.1272,30.514051938057,2.41869034282863));
#74112=CARTESIAN_POINT('',(18.3,29.9890859663487,2.32646660916507));
#74113=CARTESIAN_POINT('Ctrl Pts',(18.3,29.9890859663487,2.32646660916507));
#74114=CARTESIAN_POINT('Ctrl Pts',(18.3,30.3841746091843,2.32646660916507));
#74115=CARTESIAN_POINT('Ctrl Pts',(18.3,30.514051938057,2.41869034282863));
#74116=CARTESIAN_POINT('',(18.18,29.9890859663487,2.32646660916507));
#74117=CARTESIAN_POINT('',(18.3,29.9890859663487,2.32646660916507));
#74118=CARTESIAN_POINT('Ctrl Pts',(18.18,29.9890859663487,2.32646660916507));
#74119=CARTESIAN_POINT('Ctrl Pts',(18.18,30.3841746091843,2.32646660916507));
#74120=CARTESIAN_POINT('Ctrl Pts',(18.18,30.514051938057,2.41869034282863));
#74121=CARTESIAN_POINT('Ctrl Pts',(18.3,29.4652115046978,2.41869034282863));
#74122=CARTESIAN_POINT('Ctrl Pts',(18.1272,29.4652115046978,2.41869034282863));
#74123=CARTESIAN_POINT('Ctrl Pts',(18.3,29.5961801946163,2.32646660916507));
#74124=CARTESIAN_POINT('Ctrl Pts',(18.1272,29.5961801946163,2.32646660916507));
#74125=CARTESIAN_POINT('Ctrl Pts',(18.3,29.9890859663487,2.32646660916507));
#74126=CARTESIAN_POINT('Ctrl Pts',(18.1272,29.9890859663487,2.32646660916507));
#74127=CARTESIAN_POINT('',(18.3,29.4652115046978,2.41869034282863));
#74128=CARTESIAN_POINT('Ctrl Pts',(18.3,29.4652115046978,2.41869034282863));
#74129=CARTESIAN_POINT('Ctrl Pts',(18.3,29.5961801946163,2.32646660916507));
#74130=CARTESIAN_POINT('Ctrl Pts',(18.3,29.9890859663487,2.32646660916507));
#74131=CARTESIAN_POINT('',(18.18,29.4652115046978,2.41869034282863));
#74132=CARTESIAN_POINT('',(18.3,29.4652115046978,2.41869034282863));
#74133=CARTESIAN_POINT('Ctrl Pts',(18.18,29.4652115046978,2.41869034282863));
#74134=CARTESIAN_POINT('Ctrl Pts',(18.18,29.5961801946163,2.32646660916507));
#74135=CARTESIAN_POINT('Ctrl Pts',(18.18,29.9890859663487,2.32646660916507));
#74136=CARTESIAN_POINT('Ctrl Pts',(18.3,29.3342428147793,2.64624821059406));
#74137=CARTESIAN_POINT('Ctrl Pts',(18.1272,29.3342428147793,2.64624821059406));
#74138=CARTESIAN_POINT('Ctrl Pts',(18.3,29.3342428147793,2.51091407649219));
#74139=CARTESIAN_POINT('Ctrl Pts',(18.1272,29.3342428147793,2.51091407649219));
#74140=CARTESIAN_POINT('Ctrl Pts',(18.3,29.4652115046978,2.41869034282863));
#74141=CARTESIAN_POINT('Ctrl Pts',(18.1272,29.4652115046978,2.41869034282863));
#74142=CARTESIAN_POINT('',(18.3,29.3342428147793,2.64624821059406));
#74143=CARTESIAN_POINT('Ctrl Pts',(18.3,29.3342428147793,2.64624821059406));
#74144=CARTESIAN_POINT('Ctrl Pts',(18.3,29.3342428147793,2.51091407649219));
#74145=CARTESIAN_POINT('Ctrl Pts',(18.3,29.4652115046978,2.41869034282863));
#74146=CARTESIAN_POINT('',(18.18,29.3342428147793,2.64624821059406));
#74147=CARTESIAN_POINT('',(18.3,29.3342428147793,2.64624821059406));
#74148=CARTESIAN_POINT('Ctrl Pts',(18.18,29.3342428147793,2.64624821059406));
#74149=CARTESIAN_POINT('Ctrl Pts',(18.18,29.3342428147793,2.51091407649219));
#74150=CARTESIAN_POINT('Ctrl Pts',(18.18,29.4652115046978,2.41869034282863));
#74151=CARTESIAN_POINT('Ctrl Pts',(18.3,29.4646658241749,2.8738062273711));
#74152=CARTESIAN_POINT('Ctrl Pts',(18.1272,29.4646658241749,2.8738062273711));
#74153=CARTESIAN_POINT('Ctrl Pts',(18.3,29.3342428147793,2.78158249370754));
#74154=CARTESIAN_POINT('Ctrl Pts',(18.1272,29.3342428147793,2.78158249370754));
#74155=CARTESIAN_POINT('Ctrl Pts',(18.3,29.3342428147793,2.64624821059406));
#74156=CARTESIAN_POINT('Ctrl Pts',(18.1272,29.3342428147793,2.64624821059406));
#74157=CARTESIAN_POINT('',(18.3,29.4646658241749,2.8738062273711));
#74158=CARTESIAN_POINT('Ctrl Pts',(18.3,29.4646658241749,2.8738062273711));
#74159=CARTESIAN_POINT('Ctrl Pts',(18.3,29.3342428147793,2.78158249370754));
#74160=CARTESIAN_POINT('Ctrl Pts',(18.3,29.3342428147793,2.64624821059406));
#74161=CARTESIAN_POINT('',(18.18,29.4646658241749,2.8738062273711));
#74162=CARTESIAN_POINT('',(18.3,29.4646658241749,2.8738062273711));
#74163=CARTESIAN_POINT('Ctrl Pts',(18.18,29.4646658241749,2.8738062273711));
#74164=CARTESIAN_POINT('Ctrl Pts',(18.18,29.3342428147793,2.78158249370754));
#74165=CARTESIAN_POINT('Ctrl Pts',(18.18,29.3342428147793,2.64624821059406));
#74166=CARTESIAN_POINT('Ctrl Pts',(18.3,29.9890859663487,2.96602996103466));
#74167=CARTESIAN_POINT('Ctrl Pts',(18.1272,29.9890859663487,2.96602996103466));
#74168=CARTESIAN_POINT('Ctrl Pts',(18.3,29.5950888335705,2.96602996103466));
#74169=CARTESIAN_POINT('Ctrl Pts',(18.1272,29.5950888335705,2.96602996103466));
#74170=CARTESIAN_POINT('Ctrl Pts',(18.3,29.4646658241749,2.8738062273711));
#74171=CARTESIAN_POINT('Ctrl Pts',(18.1272,29.4646658241749,2.8738062273711));
#74172=CARTESIAN_POINT('',(18.3,29.9890859663487,2.96602996103466));
#74173=CARTESIAN_POINT('Ctrl Pts',(18.3,29.9890859663487,2.96602996103466));
#74174=CARTESIAN_POINT('Ctrl Pts',(18.3,29.5950888335705,2.96602996103466));
#74175=CARTESIAN_POINT('Ctrl Pts',(18.3,29.4646658241749,2.8738062273711));
#74176=CARTESIAN_POINT('',(18.18,29.9890859663487,2.96602996103466));
#74177=CARTESIAN_POINT('',(18.3,29.9890859663487,2.96602996103466));
#74178=CARTESIAN_POINT('Ctrl Pts',(18.18,29.9890859663487,2.96602996103466));
#74179=CARTESIAN_POINT('Ctrl Pts',(18.18,29.5950888335705,2.96602996103466));
#74180=CARTESIAN_POINT('Ctrl Pts',(18.18,29.4646658241749,2.8738062273711));
#74181=CARTESIAN_POINT('Ctrl Pts',(18.3,30.5293315887451,2.86452936045825));
#74182=CARTESIAN_POINT('Ctrl Pts',(18.1272,30.5293315887451,2.86452936045825));
#74183=CARTESIAN_POINT('Ctrl Pts',(18.3,30.3830830991268,2.96602996103466));
#74184=CARTESIAN_POINT('Ctrl Pts',(18.1272,30.3830830991268,2.96602996103466));
#74185=CARTESIAN_POINT('Ctrl Pts',(18.3,29.9890859663487,2.96602996103466));
#74186=CARTESIAN_POINT('Ctrl Pts',(18.1272,29.9890859663487,2.96602996103466));
#74187=CARTESIAN_POINT('Ctrl Pts',(18.3,30.5293315887451,2.86452936045825));
#74188=CARTESIAN_POINT('Ctrl Pts',(18.3,30.3830830991268,2.96602996103466));
#74189=CARTESIAN_POINT('Ctrl Pts',(18.3,29.9890859663487,2.96602996103466));
#74190=CARTESIAN_POINT('Ctrl Pts',(18.18,30.5293315887451,2.86452936045825));
#74191=CARTESIAN_POINT('Ctrl Pts',(18.18,30.3830830991268,2.96602996103466));
#74192=CARTESIAN_POINT('Ctrl Pts',(18.18,29.9890859663487,2.96602996103466));
#74193=CARTESIAN_POINT('Ctrl Pts',(18.3,29.1727148234844,2.64624821059406));
#74194=CARTESIAN_POINT('Ctrl Pts',(18.1272,29.1727148234844,2.64624821059406));
#74195=CARTESIAN_POINT('Ctrl Pts',(18.3,29.1727148234844,2.87762614004314));
#74196=CARTESIAN_POINT('Ctrl Pts',(18.1272,29.1727148234844,2.87762614004314));
#74197=CARTESIAN_POINT('Ctrl Pts',(18.3,29.3386085569859,3.00968619100749));
#74198=CARTESIAN_POINT('Ctrl Pts',(18.1272,29.3386085569859,3.00968619100749));
#74199=CARTESIAN_POINT('',(18.3,29.1727148234844,2.64624821059406));
#74200=CARTESIAN_POINT('',(18.3,29.3386085569859,3.00968619100749));
#74201=CARTESIAN_POINT('Ctrl Pts',(18.3,29.1727148234844,2.64624821059406));
#74202=CARTESIAN_POINT('Ctrl Pts',(18.3,29.1727148234844,2.87762614004314));
#74203=CARTESIAN_POINT('Ctrl Pts',(18.3,29.3386085569859,3.00968619100749));
#74204=CARTESIAN_POINT('',(18.18,29.1727148234844,2.64624821059406));
#74205=CARTESIAN_POINT('',(18.3,29.1727148234844,2.64624821059406));
#74206=CARTESIAN_POINT('',(18.18,29.3386085569859,3.00968619100749));
#74207=CARTESIAN_POINT('Ctrl Pts',(18.18,29.1727148234844,2.64624821059406));
#74208=CARTESIAN_POINT('Ctrl Pts',(18.18,29.1727148234844,2.87762614004314));
#74209=CARTESIAN_POINT('Ctrl Pts',(18.18,29.3386085569859,3.00968619100749));
#74210=CARTESIAN_POINT('',(18.3,29.3386085569859,3.00968619100749));
#74211=CARTESIAN_POINT('Ctrl Pts',(18.3,29.2671214282513,2.35538886897266));
#74212=CARTESIAN_POINT('Ctrl Pts',(18.1272,29.2671214282513,2.35538886897266));
#74213=CARTESIAN_POINT('Ctrl Pts',(18.3,29.1727148234844,2.47053207866847));
#74214=CARTESIAN_POINT('Ctrl Pts',(18.1272,29.1727148234844,2.47053207866847));
#74215=CARTESIAN_POINT('Ctrl Pts',(18.3,29.1727148234844,2.64624821059406));
#74216=CARTESIAN_POINT('Ctrl Pts',(18.1272,29.1727148234844,2.64624821059406));
#74217=CARTESIAN_POINT('',(18.3,29.2671214282513,2.35538886897266));
#74218=CARTESIAN_POINT('Ctrl Pts',(18.3,29.2671214282513,2.35538886897266));
#74219=CARTESIAN_POINT('Ctrl Pts',(18.3,29.1727148234844,2.47053207866847));
#74220=CARTESIAN_POINT('Ctrl Pts',(18.3,29.1727148234844,2.64624821059406));
#74221=CARTESIAN_POINT('',(18.18,29.2671214282513,2.35538886897266));
#74222=CARTESIAN_POINT('',(18.3,29.2671214282513,2.35538886897266));
#74223=CARTESIAN_POINT('Ctrl Pts',(18.18,29.2671214282513,2.35538886897266));
#74224=CARTESIAN_POINT('Ctrl Pts',(18.18,29.1727148234844,2.47053207866847));
#74225=CARTESIAN_POINT('Ctrl Pts',(18.18,29.1727148234844,2.64624821059406));
#74226=CARTESIAN_POINT('Ctrl Pts',(18.3,29.5345156133175,2.18240113966167));
#74227=CARTESIAN_POINT('Ctrl Pts',(18.1272,29.5345156133175,2.18240113966167));
#74228=CARTESIAN_POINT('Ctrl Pts',(18.3,29.3615280330181,2.24024551026523));
#74229=CARTESIAN_POINT('Ctrl Pts',(18.1272,29.3615280330181,2.24024551026523));
#74230=CARTESIAN_POINT('Ctrl Pts',(18.3,29.2671214282513,2.35538886897266));
#74231=CARTESIAN_POINT('Ctrl Pts',(18.1272,29.2671214282513,2.35538886897266));
#74232=CARTESIAN_POINT('',(18.3,29.5345156133175,2.18240113966167));
#74233=CARTESIAN_POINT('Ctrl Pts',(18.3,29.5345156133175,2.18240113966167));
#74234=CARTESIAN_POINT('Ctrl Pts',(18.3,29.3615280330181,2.24024551026523));
#74235=CARTESIAN_POINT('Ctrl Pts',(18.3,29.2671214282513,2.35538886897266));
#74236=CARTESIAN_POINT('',(18.18,29.5345156133175,2.18240113966167));
#74237=CARTESIAN_POINT('',(18.3,29.5345156133175,2.18240113966167));
#74238=CARTESIAN_POINT('Ctrl Pts',(18.18,29.5345156133175,2.18240113966167));
#74239=CARTESIAN_POINT('Ctrl Pts',(18.18,29.3615280330181,2.24024551026523));
#74240=CARTESIAN_POINT('Ctrl Pts',(18.18,29.2671214282513,2.35538886897266));
#74241=CARTESIAN_POINT('Ctrl Pts',(18.3,29.9890859663487,2.12455647103488));
#74242=CARTESIAN_POINT('Ctrl Pts',(18.1272,29.9890859663487,2.12455647103488));
#74243=CARTESIAN_POINT('Ctrl Pts',(18.3,29.7075034916401,2.12455647103488));
#74244=CARTESIAN_POINT('Ctrl Pts',(18.1272,29.7075034916401,2.12455647103488));
#74245=CARTESIAN_POINT('Ctrl Pts',(18.3,29.5345156133175,2.18240113966167));
#74246=CARTESIAN_POINT('Ctrl Pts',(18.1272,29.5345156133175,2.18240113966167));
#74247=CARTESIAN_POINT('',(18.3,29.9890859663487,2.12455647103488));
#74248=CARTESIAN_POINT('Ctrl Pts',(18.3,29.9890859663487,2.12455647103488));
#74249=CARTESIAN_POINT('Ctrl Pts',(18.3,29.7075034916401,2.12455647103488));
#74250=CARTESIAN_POINT('Ctrl Pts',(18.3,29.5345156133175,2.18240113966167));
#74251=CARTESIAN_POINT('',(18.18,29.9890859663487,2.12455647103488));
#74252=CARTESIAN_POINT('',(18.3,29.9890859663487,2.12455647103488));
#74253=CARTESIAN_POINT('Ctrl Pts',(18.18,29.9890859663487,2.12455647103488));
#74254=CARTESIAN_POINT('Ctrl Pts',(18.18,29.7075034916401,2.12455647103488));
#74255=CARTESIAN_POINT('Ctrl Pts',(18.18,29.5345156133175,2.18240113966167));
#74256=CARTESIAN_POINT('Ctrl Pts',(18.3,30.3672577679157,2.16057302467525));
#74257=CARTESIAN_POINT('Ctrl Pts',(18.1272,30.3672577679157,2.16057302467525));
#74258=CARTESIAN_POINT('Ctrl Pts',(18.3,30.2270122110844,2.12455647103488));
#74259=CARTESIAN_POINT('Ctrl Pts',(18.1272,30.2270122110844,2.12455647103488));
#74260=CARTESIAN_POINT('Ctrl Pts',(18.3,29.9890859663487,2.12455647103488));
#74261=CARTESIAN_POINT('Ctrl Pts',(18.1272,29.9890859663487,2.12455647103488));
#74262=CARTESIAN_POINT('',(18.3,30.3672577679157,2.16057302467525));
#74263=CARTESIAN_POINT('Ctrl Pts',(18.3,30.3672577679157,2.16057302467525));
#74264=CARTESIAN_POINT('Ctrl Pts',(18.3,30.2270122110844,2.12455647103488));
#74265=CARTESIAN_POINT('Ctrl Pts',(18.3,29.9890859663487,2.12455647103488));
#74266=CARTESIAN_POINT('',(18.18,30.3672577679157,2.16057302467525));
#74267=CARTESIAN_POINT('',(18.3,30.3672577679157,2.16057302467525));
#74268=CARTESIAN_POINT('Ctrl Pts',(18.18,30.3672577679157,2.16057302467525));
#74269=CARTESIAN_POINT('Ctrl Pts',(18.18,30.2270122110844,2.12455647103488));
#74270=CARTESIAN_POINT('Ctrl Pts',(18.18,29.9890859663487,2.12455647103488));
#74271=CARTESIAN_POINT('Ctrl Pts',(18.3,30.6051841616631,2.25989090315998));
#74272=CARTESIAN_POINT('Ctrl Pts',(18.1272,30.6051841616631,2.25989090315998));
#74273=CARTESIAN_POINT('Ctrl Pts',(18.3,30.5075034737587,2.19658928029239));
#74274=CARTESIAN_POINT('Ctrl Pts',(18.1272,30.5075034737587,2.19658928029239));
#74275=CARTESIAN_POINT('Ctrl Pts',(18.3,30.3672577679157,2.16057302467525));
#74276=CARTESIAN_POINT('Ctrl Pts',(18.1272,30.3672577679157,2.16057302467525));
#74277=CARTESIAN_POINT('',(18.3,30.6051841616631,2.25989090315998));
#74278=CARTESIAN_POINT('Ctrl Pts',(18.3,30.6051841616631,2.25989090315998));
#74279=CARTESIAN_POINT('Ctrl Pts',(18.3,30.5075034737587,2.19658928029239));
#74280=CARTESIAN_POINT('Ctrl Pts',(18.3,30.3672577679157,2.16057302467525));
#74281=CARTESIAN_POINT('',(18.18,30.6051841616631,2.25989090315998));
#74282=CARTESIAN_POINT('',(18.3,30.6051841616631,2.25989090315998));
#74283=CARTESIAN_POINT('Ctrl Pts',(18.18,30.6051841616631,2.25989090315998));
#74284=CARTESIAN_POINT('Ctrl Pts',(18.18,30.5075034737587,2.19658928029239));
#74285=CARTESIAN_POINT('Ctrl Pts',(18.18,30.3672577679157,2.16057302467525));
#74286=CARTESIAN_POINT('Ctrl Pts',(18.3,30.7547067344189,2.420327533409));
#74287=CARTESIAN_POINT('Ctrl Pts',(18.1272,30.7547067344189,2.420327533409));
#74288=CARTESIAN_POINT('Ctrl Pts',(18.3,30.702864998579,2.32319237701595));
#74289=CARTESIAN_POINT('Ctrl Pts',(18.1272,30.702864998579,2.32319237701595));
#74290=CARTESIAN_POINT('Ctrl Pts',(18.3,30.6051841616631,2.25989090315998));
#74291=CARTESIAN_POINT('Ctrl Pts',(18.1272,30.6051841616631,2.25989090315998));
#74292=CARTESIAN_POINT('',(18.3,30.7547067344189,2.420327533409));
#74293=CARTESIAN_POINT('Ctrl Pts',(18.3,30.7547067344189,2.420327533409));
#74294=CARTESIAN_POINT('Ctrl Pts',(18.3,30.702864998579,2.32319237701595));
#74295=CARTESIAN_POINT('Ctrl Pts',(18.3,30.6051841616631,2.25989090315998));
#74296=CARTESIAN_POINT('',(18.18,30.7547067344189,2.420327533409));
#74297=CARTESIAN_POINT('',(18.3,30.7547067344189,2.420327533409));
#74298=CARTESIAN_POINT('Ctrl Pts',(18.18,30.7547067344189,2.420327533409));
#74299=CARTESIAN_POINT('Ctrl Pts',(18.18,30.702864998579,2.32319237701595));
#74300=CARTESIAN_POINT('Ctrl Pts',(18.18,30.6051841616631,2.25989090315998));
#74301=CARTESIAN_POINT('Ctrl Pts',(18.3,30.8065484702587,2.64624821059406));
#74302=CARTESIAN_POINT('Ctrl Pts',(18.1272,30.8065484702587,2.64624821059406));
#74303=CARTESIAN_POINT('Ctrl Pts',(18.3,30.8065484702587,2.51746254079044));
#74304=CARTESIAN_POINT('Ctrl Pts',(18.1272,30.8065484702587,2.51746254079044));
#74305=CARTESIAN_POINT('Ctrl Pts',(18.3,30.7547067344189,2.420327533409));
#74306=CARTESIAN_POINT('Ctrl Pts',(18.1272,30.7547067344189,2.420327533409));
#74307=CARTESIAN_POINT('',(18.3,30.8065484702587,2.64624821059406));
#74308=CARTESIAN_POINT('Ctrl Pts',(18.3,30.8065484702587,2.64624821059406));
#74309=CARTESIAN_POINT('Ctrl Pts',(18.3,30.8065484702587,2.51746254079044));
#74310=CARTESIAN_POINT('Ctrl Pts',(18.3,30.7547067344189,2.420327533409));
#74311=CARTESIAN_POINT('',(18.18,30.8065484702587,2.64624821059406));
#74312=CARTESIAN_POINT('',(18.3,30.8065484702587,2.64624821059406));
#74313=CARTESIAN_POINT('Ctrl Pts',(18.18,30.8065484702587,2.64624821059406));
#74314=CARTESIAN_POINT('Ctrl Pts',(18.18,30.8065484702587,2.51746254079044));
#74315=CARTESIAN_POINT('Ctrl Pts',(18.18,30.7547067344189,2.420327533409));
#74316=CARTESIAN_POINT('Ctrl Pts',(18.3,30.7126876950264,2.93601634018123));
#74317=CARTESIAN_POINT('Ctrl Pts',(18.1272,30.7126876950264,2.93601634018123));
#74318=CARTESIAN_POINT('Ctrl Pts',(18.3,30.8065484702587,2.82087313048542));
#74319=CARTESIAN_POINT('Ctrl Pts',(18.1272,30.8065484702587,2.82087313048542));
#74320=CARTESIAN_POINT('Ctrl Pts',(18.3,30.8065484702587,2.64624821059406));
#74321=CARTESIAN_POINT('Ctrl Pts',(18.1272,30.8065484702587,2.64624821059406));
#74322=CARTESIAN_POINT('',(18.3,30.7126876950264,2.93601634018123));
#74323=CARTESIAN_POINT('Ctrl Pts',(18.3,30.7126876950264,2.93601634018123));
#74324=CARTESIAN_POINT('Ctrl Pts',(18.3,30.8065484702587,2.82087313048542));
#74325=CARTESIAN_POINT('Ctrl Pts',(18.3,30.8065484702587,2.64624821059406));
#74326=CARTESIAN_POINT('',(18.18,30.7126876950264,2.93601634018123));
#74327=CARTESIAN_POINT('',(18.3,30.7126876950264,2.93601634018123));
#74328=CARTESIAN_POINT('Ctrl Pts',(18.18,30.7126876950264,2.93601634018123));
#74329=CARTESIAN_POINT('Ctrl Pts',(18.18,30.8065484702587,2.82087313048542));
#74330=CARTESIAN_POINT('Ctrl Pts',(18.18,30.8065484702587,2.64624821059406));
#74331=CARTESIAN_POINT('Ctrl Pts',(18.3,30.4458390414715,3.10954975001514));
#74332=CARTESIAN_POINT('Ctrl Pts',(18.1272,30.4458390414715,3.10954975001514));
#74333=CARTESIAN_POINT('Ctrl Pts',(18.3,30.6188267707825,3.05115954987705));
#74334=CARTESIAN_POINT('Ctrl Pts',(18.1272,30.6188267707825,3.05115954987705));
#74335=CARTESIAN_POINT('Ctrl Pts',(18.3,30.7126876950264,2.93601634018123));
#74336=CARTESIAN_POINT('Ctrl Pts',(18.1272,30.7126876950264,2.93601634018123));
#74337=CARTESIAN_POINT('',(18.3,30.4458390414715,3.10954975001514));
#74338=CARTESIAN_POINT('Ctrl Pts',(18.3,30.4458390414715,3.10954975001514));
#74339=CARTESIAN_POINT('Ctrl Pts',(18.3,30.6188267707825,3.05115954987705));
#74340=CARTESIAN_POINT('Ctrl Pts',(18.3,30.7126876950264,2.93601634018123));
#74341=CARTESIAN_POINT('',(18.18,30.4458390414715,3.10954975001514));
#74342=CARTESIAN_POINT('',(18.3,30.4458390414715,3.10954975001514));
#74343=CARTESIAN_POINT('Ctrl Pts',(18.18,30.4458390414715,3.10954975001514));
#74344=CARTESIAN_POINT('Ctrl Pts',(18.18,30.6188267707825,3.05115954987705));
#74345=CARTESIAN_POINT('Ctrl Pts',(18.18,30.7126876950264,2.93601634018123));
#74346=CARTESIAN_POINT('Ctrl Pts',(18.3,29.9890859663487,3.16793995015323));
#74347=CARTESIAN_POINT('Ctrl Pts',(18.1272,29.9890859663487,3.16793995015323));
#74348=CARTESIAN_POINT('Ctrl Pts',(18.3,30.2728513121605,3.16793995015323));
#74349=CARTESIAN_POINT('Ctrl Pts',(18.1272,30.2728513121605,3.16793995015323));
#74350=CARTESIAN_POINT('Ctrl Pts',(18.3,30.4458390414715,3.10954975001514));
#74351=CARTESIAN_POINT('Ctrl Pts',(18.1272,30.4458390414715,3.10954975001514));
#74352=CARTESIAN_POINT('',(18.3,29.9890859663487,3.16793995015323));
#74353=CARTESIAN_POINT('Ctrl Pts',(18.3,29.9890859663487,3.16793995015323));
#74354=CARTESIAN_POINT('Ctrl Pts',(18.3,30.2728513121605,3.16793995015323));
#74355=CARTESIAN_POINT('Ctrl Pts',(18.3,30.4458390414715,3.10954975001514));
#74356=CARTESIAN_POINT('',(18.18,29.9890859663487,3.16793995015323));
#74357=CARTESIAN_POINT('',(18.3,29.9890859663487,3.16793995015323));
#74358=CARTESIAN_POINT('Ctrl Pts',(18.18,29.9890859663487,3.16793995015323));
#74359=CARTESIAN_POINT('Ctrl Pts',(18.18,30.2728513121605,3.16793995015323));
#74360=CARTESIAN_POINT('Ctrl Pts',(18.18,30.4458390414715,3.10954975001514));
#74361=CARTESIAN_POINT('Ctrl Pts',(18.3,29.3386085569859,3.00968619100749));
#74362=CARTESIAN_POINT('Ctrl Pts',(18.1272,29.3386085569859,3.00968619100749));
#74363=CARTESIAN_POINT('Ctrl Pts',(18.3,29.5383356750012,3.16793995015323));
#74364=CARTESIAN_POINT('Ctrl Pts',(18.1272,29.5383356750012,3.16793995015323));
#74365=CARTESIAN_POINT('Ctrl Pts',(18.3,29.9890859663487,3.16793995015323));
#74366=CARTESIAN_POINT('Ctrl Pts',(18.1272,29.9890859663487,3.16793995015323));
#74367=CARTESIAN_POINT('Ctrl Pts',(18.3,29.3386085569859,3.00968619100749));
#74368=CARTESIAN_POINT('Ctrl Pts',(18.3,29.5383356750012,3.16793995015323));
#74369=CARTESIAN_POINT('Ctrl Pts',(18.3,29.9890859663487,3.16793995015323));
#74370=CARTESIAN_POINT('Ctrl Pts',(18.18,29.3386085569859,3.00968619100749));
#74371=CARTESIAN_POINT('Ctrl Pts',(18.18,29.5383356750012,3.16793995015323));
#74372=CARTESIAN_POINT('Ctrl Pts',(18.18,29.9890859663487,3.16793995015323));
#74373=CARTESIAN_POINT('Origin',(18.18,29.9896316468716,3.29999987538904));
#74374=CARTESIAN_POINT('Origin',(18.3,30.4845838487148,3.78130966834724));
#74375=CARTESIAN_POINT('',(18.3,30.4845838487148,3.78130966834724));
#74376=CARTESIAN_POINT('',(18.3,29.7631649911404,4.28226457946002));
#74377=CARTESIAN_POINT('',(18.3,43.4120209624511,-5.19553234546084));
#74378=CARTESIAN_POINT('',(18.18,30.4845838487148,3.78130966834724));
#74379=CARTESIAN_POINT('',(18.3,30.4845838487148,3.78130966834724));
#74380=CARTESIAN_POINT('',(18.18,29.7631649911404,4.28226457946002));
#74381=CARTESIAN_POINT('',(18.18,30.4845838487148,3.78130966834724));
#74382=CARTESIAN_POINT('',(18.3,29.7631649911404,4.28226457946002));
#74383=CARTESIAN_POINT('Origin',(18.3,29.7631649911404,3.78130966834724));
#74384=CARTESIAN_POINT('',(18.3,29.7631649911404,3.78130966834724));
#74385=CARTESIAN_POINT('',(18.3,49.8815824955702,3.78130966834724));
#74386=CARTESIAN_POINT('',(18.18,29.7631649911404,3.78130966834724));
#74387=CARTESIAN_POINT('',(18.3,29.7631649911404,3.78130966834724));
#74388=CARTESIAN_POINT('',(18.18,29.7631649911404,3.78130966834724));
#74389=CARTESIAN_POINT('Origin',(18.3,29.7631649911404,4.28226457946002));
#74390=CARTESIAN_POINT('',(18.3,29.7631649911404,4.89113228973001));
#74391=CARTESIAN_POINT('',(18.18,29.7631649911404,4.28226457946002));
#74392=CARTESIAN_POINT('Origin',(18.3,29.5830832660198,3.58485670797527));
#74393=CARTESIAN_POINT('',(18.3,29.5830832660198,3.58485670797527));
#74394=CARTESIAN_POINT('',(18.3,29.2000000417233,3.58485670797527));
#74395=CARTESIAN_POINT('',(18.3,49.7915416330099,3.58485670797527));
#74396=CARTESIAN_POINT('',(18.18,29.5830832660198,3.58485670797527));
#74397=CARTESIAN_POINT('',(18.3,29.5830832660198,3.58485670797527));
#74398=CARTESIAN_POINT('',(18.18,29.2000000417233,3.58485670797527));
#74399=CARTESIAN_POINT('',(18.18,29.5830832660198,3.58485670797527));
#74400=CARTESIAN_POINT('',(18.3,29.2000000417233,3.58485670797527));
#74401=CARTESIAN_POINT('Origin',(18.3,29.5830832660198,3.36875842921436));
#74402=CARTESIAN_POINT('',(18.3,29.5830832660198,3.36875842921436));
#74403=CARTESIAN_POINT('',(18.3,29.5830832660198,4.43437921460718));
#74404=CARTESIAN_POINT('',(18.18,29.5830832660198,3.36875842921436));
#74405=CARTESIAN_POINT('',(18.3,29.5830832660198,3.36875842921436));
#74406=CARTESIAN_POINT('',(18.18,29.5830832660198,3.36875842921436));
#74407=CARTESIAN_POINT('Origin',(18.3,29.7631649911404,3.36875842921436));
#74408=CARTESIAN_POINT('',(18.3,29.7631649911404,3.36875842921436));
#74409=CARTESIAN_POINT('',(18.3,49.8815824955702,3.36875842921436));
#74410=CARTESIAN_POINT('',(18.18,29.7631649911404,3.36875842921436));
#74411=CARTESIAN_POINT('',(18.3,29.7631649911404,3.36875842921436));
#74412=CARTESIAN_POINT('',(18.18,29.7631649911404,3.36875842921436));
#74413=CARTESIAN_POINT('Origin',(18.3,29.7631649911404,3.58485670797527));
#74414=CARTESIAN_POINT('',(18.3,29.7631649911404,3.58485670797527));
#74415=CARTESIAN_POINT('',(18.3,29.7631649911404,4.54242835398763));
#74416=CARTESIAN_POINT('',(18.18,29.7631649911404,3.58485670797527));
#74417=CARTESIAN_POINT('',(18.3,29.7631649911404,3.58485670797527));
#74418=CARTESIAN_POINT('',(18.18,29.7631649911404,3.58485670797527));
#74419=CARTESIAN_POINT('Origin',(18.3,30.8000000059605,3.58485670797527));
#74420=CARTESIAN_POINT('',(18.3,30.8000000059605,3.58485670797527));
#74421=CARTESIAN_POINT('',(18.3,50.4000000029802,3.58485670797527));
#74422=CARTESIAN_POINT('',(18.18,30.8000000059605,3.58485670797527));
#74423=CARTESIAN_POINT('',(18.3,30.8000000059605,3.58485670797527));
#74424=CARTESIAN_POINT('',(18.18,30.8000000059605,3.58485670797527));
#74425=CARTESIAN_POINT('Origin',(18.3,30.8000000059605,3.74529326371849));
#74426=CARTESIAN_POINT('',(18.3,30.8000000059605,3.74529326371849));
#74427=CARTESIAN_POINT('',(18.3,30.8000000059605,4.62264663185924));
#74428=CARTESIAN_POINT('',(18.18,30.8000000059605,3.74529326371849));
#74429=CARTESIAN_POINT('',(18.3,30.8000000059605,3.74529326371849));
#74430=CARTESIAN_POINT('',(18.18,30.8000000059605,3.74529326371849));
#74431=CARTESIAN_POINT('Origin',(18.3,29.7631649911404,4.47544327974319));
#74432=CARTESIAN_POINT('',(18.3,29.7631649911404,4.47544327974319));
#74433=CARTESIAN_POINT('',(18.3,42.9709350156429,-4.8256059298212));
#74434=CARTESIAN_POINT('',(18.18,29.7631649911404,4.47544327974319));
#74435=CARTESIAN_POINT('',(18.3,29.7631649911404,4.47544327974319));
#74436=CARTESIAN_POINT('',(18.18,29.7631649911404,4.47544327974319));
#74437=CARTESIAN_POINT('Origin',(18.3,29.5830832660198,4.47544327974319));
#74438=CARTESIAN_POINT('',(18.3,29.5830832660198,4.47544327974319));
#74439=CARTESIAN_POINT('',(18.3,49.7915416330099,4.47544327974319));
#74440=CARTESIAN_POINT('',(18.18,29.5830832660198,4.47544327974319));
#74441=CARTESIAN_POINT('',(18.3,29.5830832660198,4.47544327974319));
#74442=CARTESIAN_POINT('',(18.18,29.5830832660198,4.47544327974319));
#74443=CARTESIAN_POINT('Origin',(18.3,29.5830832660198,3.78130966834724));
#74444=CARTESIAN_POINT('',(18.3,29.5830832660198,3.78130966834724));
#74445=CARTESIAN_POINT('',(18.3,29.5830832660198,4.64065483417362));
#74446=CARTESIAN_POINT('',(18.18,29.5830832660198,3.78130966834724));
#74447=CARTESIAN_POINT('',(18.3,29.5830832660198,3.78130966834724));
#74448=CARTESIAN_POINT('',(18.18,29.5830832660198,3.78130966834724));
#74449=CARTESIAN_POINT('Origin',(18.3,29.2000000417233,3.78130966834724));
#74450=CARTESIAN_POINT('',(18.3,29.2000000417233,3.78130966834724));
#74451=CARTESIAN_POINT('',(18.3,49.6000000208616,3.78130966834724));
#74452=CARTESIAN_POINT('',(18.18,29.2000000417233,3.78130966834724));
#74453=CARTESIAN_POINT('',(18.3,29.2000000417233,3.78130966834724));
#74454=CARTESIAN_POINT('',(18.18,29.2000000417233,3.78130966834724));
#74455=CARTESIAN_POINT('Origin',(18.3,29.2000000417233,3.58485670797527));
#74456=CARTESIAN_POINT('',(18.3,29.2000000417233,4.54242835398763));
#74457=CARTESIAN_POINT('',(18.18,29.2000000417233,3.58485670797527));
#74458=CARTESIAN_POINT('Origin',(18.18,29.9896316468716,3.29999987538904));
#74459=CARTESIAN_POINT('Origin',(18.3,70.,5.5));
#74460=CARTESIAN_POINT('Origin',(18.3,70.,5.5));
#74461=CARTESIAN_POINT('Origin',(18.3,111.08,8.));
#74462=CARTESIAN_POINT('',(18.3,111.08,8.));
#74463=CARTESIAN_POINT('',(18.3,110.92,8.));
#74464=CARTESIAN_POINT('',(18.3,90.54,8.));
#74465=CARTESIAN_POINT('',(18.18,111.08,8.));
#74466=CARTESIAN_POINT('',(18.3,111.08,8.));
#74467=CARTESIAN_POINT('',(18.18,110.92,8.));
#74468=CARTESIAN_POINT('',(18.18,110.92,8.));
#74469=CARTESIAN_POINT('',(18.3,110.92,8.));
#74470=CARTESIAN_POINT('Origin',(18.3,111.08,9.4));
#74471=CARTESIAN_POINT('',(18.3,111.08,9.4));
#74472=CARTESIAN_POINT('',(18.3,111.08,7.45));
#74473=CARTESIAN_POINT('',(18.18,111.08,9.4));
#74474=CARTESIAN_POINT('',(18.3,111.08,9.4));
#74475=CARTESIAN_POINT('',(18.18,111.08,8.));
#74476=CARTESIAN_POINT('Origin',(18.3,110.92,9.4));
#74477=CARTESIAN_POINT('',(18.3,110.92,9.4));
#74478=CARTESIAN_POINT('',(18.3,90.46,9.4));
#74479=CARTESIAN_POINT('',(18.18,110.92,9.4));
#74480=CARTESIAN_POINT('',(18.3,110.92,9.4));
#74481=CARTESIAN_POINT('',(18.18,111.08,9.4));
#74482=CARTESIAN_POINT('Origin',(18.3,110.92,8.));
#74483=CARTESIAN_POINT('',(18.3,110.92,6.75));
#74484=CARTESIAN_POINT('',(18.18,110.92,9.4));
#74485=CARTESIAN_POINT('Origin',(18.18,111.,8.7));
#74486=CARTESIAN_POINT('Origin',(18.3,109.08,8.));
#74487=CARTESIAN_POINT('',(18.3,109.08,8.));
#74488=CARTESIAN_POINT('',(18.3,108.92,8.));
#74489=CARTESIAN_POINT('',(18.3,89.54,8.));
#74490=CARTESIAN_POINT('',(18.18,109.08,8.));
#74491=CARTESIAN_POINT('',(18.3,109.08,8.));
#74492=CARTESIAN_POINT('',(18.18,108.92,8.));
#74493=CARTESIAN_POINT('',(18.18,108.92,8.));
#74494=CARTESIAN_POINT('',(18.3,108.92,8.));
#74495=CARTESIAN_POINT('Origin',(18.3,109.08,9.4));
#74496=CARTESIAN_POINT('',(18.3,109.08,9.4));
#74497=CARTESIAN_POINT('',(18.3,109.08,7.45));
#74498=CARTESIAN_POINT('',(18.18,109.08,9.4));
#74499=CARTESIAN_POINT('',(18.3,109.08,9.4));
#74500=CARTESIAN_POINT('',(18.18,109.08,8.));
#74501=CARTESIAN_POINT('Origin',(18.3,108.92,9.4));
#74502=CARTESIAN_POINT('',(18.3,108.92,9.4));
#74503=CARTESIAN_POINT('',(18.3,89.46,9.4));
#74504=CARTESIAN_POINT('',(18.18,108.92,9.4));
#74505=CARTESIAN_POINT('',(18.3,108.92,9.4));
#74506=CARTESIAN_POINT('',(18.18,109.08,9.4));
#74507=CARTESIAN_POINT('Origin',(18.3,108.92,8.));
#74508=CARTESIAN_POINT('',(18.3,108.92,6.75));
#74509=CARTESIAN_POINT('',(18.18,108.92,9.4));
#74510=CARTESIAN_POINT('Origin',(18.18,109.,8.7));
#74511=CARTESIAN_POINT('Origin',(18.3,107.08,8.));
#74512=CARTESIAN_POINT('',(18.3,107.08,8.));
#74513=CARTESIAN_POINT('',(18.3,106.92,8.));
#74514=CARTESIAN_POINT('',(18.3,88.54,8.));
#74515=CARTESIAN_POINT('',(18.18,107.08,8.));
#74516=CARTESIAN_POINT('',(18.3,107.08,8.));
#74517=CARTESIAN_POINT('',(18.18,106.92,8.));
#74518=CARTESIAN_POINT('',(18.18,106.92,8.));
#74519=CARTESIAN_POINT('',(18.3,106.92,8.));
#74520=CARTESIAN_POINT('Origin',(18.3,107.08,9.4));
#74521=CARTESIAN_POINT('',(18.3,107.08,9.4));
#74522=CARTESIAN_POINT('',(18.3,107.08,7.45));
#74523=CARTESIAN_POINT('',(18.18,107.08,9.4));
#74524=CARTESIAN_POINT('',(18.3,107.08,9.4));
#74525=CARTESIAN_POINT('',(18.18,107.08,8.));
#74526=CARTESIAN_POINT('Origin',(18.3,106.92,9.4));
#74527=CARTESIAN_POINT('',(18.3,106.92,9.4));
#74528=CARTESIAN_POINT('',(18.3,88.46,9.4));
#74529=CARTESIAN_POINT('',(18.18,106.92,9.4));
#74530=CARTESIAN_POINT('',(18.3,106.92,9.4));
#74531=CARTESIAN_POINT('',(18.18,107.08,9.4));
#74532=CARTESIAN_POINT('Origin',(18.3,106.92,8.));
#74533=CARTESIAN_POINT('',(18.3,106.92,6.75));
#74534=CARTESIAN_POINT('',(18.18,106.92,9.4));
#74535=CARTESIAN_POINT('Origin',(18.18,107.,8.7));
#74536=CARTESIAN_POINT('Origin',(18.3,105.08,7.2));
#74537=CARTESIAN_POINT('',(18.3,105.08,7.2));
#74538=CARTESIAN_POINT('',(18.3,104.92,7.2));
#74539=CARTESIAN_POINT('',(18.3,87.54,7.2));
#74540=CARTESIAN_POINT('',(18.18,105.08,7.2));
#74541=CARTESIAN_POINT('',(18.3,105.08,7.2));
#74542=CARTESIAN_POINT('',(18.18,104.92,7.2));
#74543=CARTESIAN_POINT('',(18.18,104.92,7.2));
#74544=CARTESIAN_POINT('',(18.3,104.92,7.2));
#74545=CARTESIAN_POINT('Origin',(18.3,105.08,9.4));
#74546=CARTESIAN_POINT('',(18.3,105.08,9.4));
#74547=CARTESIAN_POINT('',(18.3,105.08,7.45));
#74548=CARTESIAN_POINT('',(18.18,105.08,9.4));
#74549=CARTESIAN_POINT('',(18.3,105.08,9.4));
#74550=CARTESIAN_POINT('',(18.18,105.08,7.2));
#74551=CARTESIAN_POINT('Origin',(18.3,104.92,9.4));
#74552=CARTESIAN_POINT('',(18.3,104.92,9.4));
#74553=CARTESIAN_POINT('',(18.3,87.46,9.4));
#74554=CARTESIAN_POINT('',(18.18,104.92,9.4));
#74555=CARTESIAN_POINT('',(18.3,104.92,9.4));
#74556=CARTESIAN_POINT('',(18.18,105.08,9.4));
#74557=CARTESIAN_POINT('Origin',(18.3,104.92,7.2));
#74558=CARTESIAN_POINT('',(18.3,104.92,6.35));
#74559=CARTESIAN_POINT('',(18.18,104.92,9.4));
#74560=CARTESIAN_POINT('Origin',(18.18,105.,8.3));
#74561=CARTESIAN_POINT('Origin',(18.3,103.08,8.));
#74562=CARTESIAN_POINT('',(18.3,103.08,8.));
#74563=CARTESIAN_POINT('',(18.3,102.92,8.));
#74564=CARTESIAN_POINT('',(18.3,86.54,8.));
#74565=CARTESIAN_POINT('',(18.18,103.08,8.));
#74566=CARTESIAN_POINT('',(18.3,103.08,8.));
#74567=CARTESIAN_POINT('',(18.18,102.92,8.));
#74568=CARTESIAN_POINT('',(18.18,102.92,8.));
#74569=CARTESIAN_POINT('',(18.3,102.92,8.));
#74570=CARTESIAN_POINT('Origin',(18.3,103.08,9.4));
#74571=CARTESIAN_POINT('',(18.3,103.08,9.4));
#74572=CARTESIAN_POINT('',(18.3,103.08,7.45));
#74573=CARTESIAN_POINT('',(18.18,103.08,9.4));
#74574=CARTESIAN_POINT('',(18.3,103.08,9.4));
#74575=CARTESIAN_POINT('',(18.18,103.08,8.));
#74576=CARTESIAN_POINT('Origin',(18.3,102.92,9.4));
#74577=CARTESIAN_POINT('',(18.3,102.92,9.4));
#74578=CARTESIAN_POINT('',(18.3,86.46,9.4));
#74579=CARTESIAN_POINT('',(18.18,102.92,9.4));
#74580=CARTESIAN_POINT('',(18.3,102.92,9.4));
#74581=CARTESIAN_POINT('',(18.18,103.08,9.4));
#74582=CARTESIAN_POINT('Origin',(18.3,102.92,8.));
#74583=CARTESIAN_POINT('',(18.3,102.92,6.75));
#74584=CARTESIAN_POINT('',(18.18,102.92,9.4));
#74585=CARTESIAN_POINT('Origin',(18.18,103.,8.7));
#74586=CARTESIAN_POINT('Origin',(18.3,101.08,8.));
#74587=CARTESIAN_POINT('',(18.3,101.08,8.));
#74588=CARTESIAN_POINT('',(18.3,100.92,8.));
#74589=CARTESIAN_POINT('',(18.3,85.54,8.));
#74590=CARTESIAN_POINT('',(18.18,101.08,8.));
#74591=CARTESIAN_POINT('',(18.3,101.08,8.));
#74592=CARTESIAN_POINT('',(18.18,100.92,8.));
#74593=CARTESIAN_POINT('',(18.18,100.92,8.));
#74594=CARTESIAN_POINT('',(18.3,100.92,8.));
#74595=CARTESIAN_POINT('Origin',(18.3,101.08,9.4));
#74596=CARTESIAN_POINT('',(18.3,101.08,9.4));
#74597=CARTESIAN_POINT('',(18.3,101.08,7.45));
#74598=CARTESIAN_POINT('',(18.18,101.08,9.4));
#74599=CARTESIAN_POINT('',(18.3,101.08,9.4));
#74600=CARTESIAN_POINT('',(18.18,101.08,8.));
#74601=CARTESIAN_POINT('Origin',(18.3,100.92,9.4));
#74602=CARTESIAN_POINT('',(18.3,100.92,9.4));
#74603=CARTESIAN_POINT('',(18.3,85.46,9.4));
#74604=CARTESIAN_POINT('',(18.18,100.92,9.4));
#74605=CARTESIAN_POINT('',(18.3,100.92,9.4));
#74606=CARTESIAN_POINT('',(18.18,101.08,9.4));
#74607=CARTESIAN_POINT('Origin',(18.3,100.92,8.));
#74608=CARTESIAN_POINT('',(18.3,100.92,6.75));
#74609=CARTESIAN_POINT('',(18.18,100.92,9.4));
#74610=CARTESIAN_POINT('Origin',(18.18,101.,8.7));
#74611=CARTESIAN_POINT('Origin',(18.3,99.08,8.));
#74612=CARTESIAN_POINT('',(18.3,99.08,8.));
#74613=CARTESIAN_POINT('',(18.3,98.92,8.));
#74614=CARTESIAN_POINT('',(18.3,84.54,8.));
#74615=CARTESIAN_POINT('',(18.18,99.08,8.));
#74616=CARTESIAN_POINT('',(18.3,99.08,8.));
#74617=CARTESIAN_POINT('',(18.18,98.92,8.));
#74618=CARTESIAN_POINT('',(18.18,98.92,8.));
#74619=CARTESIAN_POINT('',(18.3,98.92,8.));
#74620=CARTESIAN_POINT('Origin',(18.3,99.08,9.4));
#74621=CARTESIAN_POINT('',(18.3,99.08,9.4));
#74622=CARTESIAN_POINT('',(18.3,99.08,7.45));
#74623=CARTESIAN_POINT('',(18.18,99.08,9.4));
#74624=CARTESIAN_POINT('',(18.3,99.08,9.4));
#74625=CARTESIAN_POINT('',(18.18,99.08,8.));
#74626=CARTESIAN_POINT('Origin',(18.3,98.92,9.4));
#74627=CARTESIAN_POINT('',(18.3,98.92,9.4));
#74628=CARTESIAN_POINT('',(18.3,84.46,9.4));
#74629=CARTESIAN_POINT('',(18.18,98.92,9.4));
#74630=CARTESIAN_POINT('',(18.3,98.92,9.4));
#74631=CARTESIAN_POINT('',(18.18,99.08,9.4));
#74632=CARTESIAN_POINT('Origin',(18.3,98.92,8.));
#74633=CARTESIAN_POINT('',(18.3,98.92,6.75));
#74634=CARTESIAN_POINT('',(18.18,98.92,9.4));
#74635=CARTESIAN_POINT('Origin',(18.18,99.,8.7));
#74636=CARTESIAN_POINT('Origin',(18.3,97.08,8.));
#74637=CARTESIAN_POINT('',(18.3,97.08,8.));
#74638=CARTESIAN_POINT('',(18.3,96.92,8.));
#74639=CARTESIAN_POINT('',(18.3,83.54,8.));
#74640=CARTESIAN_POINT('',(18.18,97.08,8.));
#74641=CARTESIAN_POINT('',(18.3,97.08,8.));
#74642=CARTESIAN_POINT('',(18.18,96.92,8.));
#74643=CARTESIAN_POINT('',(18.18,96.92,8.));
#74644=CARTESIAN_POINT('',(18.3,96.92,8.));
#74645=CARTESIAN_POINT('Origin',(18.3,97.08,9.4));
#74646=CARTESIAN_POINT('',(18.3,97.08,9.4));
#74647=CARTESIAN_POINT('',(18.3,97.08,7.45));
#74648=CARTESIAN_POINT('',(18.18,97.08,9.4));
#74649=CARTESIAN_POINT('',(18.3,97.08,9.4));
#74650=CARTESIAN_POINT('',(18.18,97.08,8.));
#74651=CARTESIAN_POINT('Origin',(18.3,96.92,9.4));
#74652=CARTESIAN_POINT('',(18.3,96.92,9.4));
#74653=CARTESIAN_POINT('',(18.3,83.46,9.4));
#74654=CARTESIAN_POINT('',(18.18,96.92,9.4));
#74655=CARTESIAN_POINT('',(18.3,96.92,9.4));
#74656=CARTESIAN_POINT('',(18.18,97.08,9.4));
#74657=CARTESIAN_POINT('Origin',(18.3,96.92,8.));
#74658=CARTESIAN_POINT('',(18.3,96.92,6.75));
#74659=CARTESIAN_POINT('',(18.18,96.92,9.4));
#74660=CARTESIAN_POINT('Origin',(18.18,97.,8.7));
#74661=CARTESIAN_POINT('Origin',(18.3,95.08,7.2));
#74662=CARTESIAN_POINT('',(18.3,95.08,7.2));
#74663=CARTESIAN_POINT('',(18.3,94.92,7.2));
#74664=CARTESIAN_POINT('',(18.3,82.54,7.2));
#74665=CARTESIAN_POINT('',(18.18,95.08,7.2));
#74666=CARTESIAN_POINT('',(18.3,95.08,7.2));
#74667=CARTESIAN_POINT('',(18.18,94.92,7.2));
#74668=CARTESIAN_POINT('',(18.18,94.92,7.2));
#74669=CARTESIAN_POINT('',(18.3,94.92,7.2));
#74670=CARTESIAN_POINT('Origin',(18.3,95.08,9.4));
#74671=CARTESIAN_POINT('',(18.3,95.08,9.4));
#74672=CARTESIAN_POINT('',(18.3,95.08,7.45));
#74673=CARTESIAN_POINT('',(18.18,95.08,9.4));
#74674=CARTESIAN_POINT('',(18.3,95.08,9.4));
#74675=CARTESIAN_POINT('',(18.18,95.08,7.2));
#74676=CARTESIAN_POINT('Origin',(18.3,94.92,9.4));
#74677=CARTESIAN_POINT('',(18.3,94.92,9.4));
#74678=CARTESIAN_POINT('',(18.3,82.46,9.4));
#74679=CARTESIAN_POINT('',(18.18,94.92,9.4));
#74680=CARTESIAN_POINT('',(18.3,94.92,9.4));
#74681=CARTESIAN_POINT('',(18.18,95.08,9.4));
#74682=CARTESIAN_POINT('Origin',(18.3,94.92,7.2));
#74683=CARTESIAN_POINT('',(18.3,94.92,6.35));
#74684=CARTESIAN_POINT('',(18.18,94.92,9.4));
#74685=CARTESIAN_POINT('Origin',(18.18,95.,8.3));
#74686=CARTESIAN_POINT('Origin',(18.3,93.08,8.));
#74687=CARTESIAN_POINT('',(18.3,93.08,8.));
#74688=CARTESIAN_POINT('',(18.3,92.92,8.));
#74689=CARTESIAN_POINT('',(18.3,81.54,8.));
#74690=CARTESIAN_POINT('',(18.18,93.08,8.));
#74691=CARTESIAN_POINT('',(18.3,93.08,8.));
#74692=CARTESIAN_POINT('',(18.18,92.92,8.));
#74693=CARTESIAN_POINT('',(18.18,92.92,8.));
#74694=CARTESIAN_POINT('',(18.3,92.92,8.));
#74695=CARTESIAN_POINT('Origin',(18.3,93.08,9.4));
#74696=CARTESIAN_POINT('',(18.3,93.08,9.4));
#74697=CARTESIAN_POINT('',(18.3,93.08,7.45));
#74698=CARTESIAN_POINT('',(18.18,93.08,9.4));
#74699=CARTESIAN_POINT('',(18.3,93.08,9.4));
#74700=CARTESIAN_POINT('',(18.18,93.08,8.));
#74701=CARTESIAN_POINT('Origin',(18.3,92.92,9.4));
#74702=CARTESIAN_POINT('',(18.3,92.92,9.4));
#74703=CARTESIAN_POINT('',(18.3,81.46,9.4));
#74704=CARTESIAN_POINT('',(18.18,92.92,9.4));
#74705=CARTESIAN_POINT('',(18.3,92.92,9.4));
#74706=CARTESIAN_POINT('',(18.18,93.08,9.4));
#74707=CARTESIAN_POINT('Origin',(18.3,92.92,8.));
#74708=CARTESIAN_POINT('',(18.3,92.92,6.75));
#74709=CARTESIAN_POINT('',(18.18,92.92,9.4));
#74710=CARTESIAN_POINT('Origin',(18.18,93.,8.7));
#74711=CARTESIAN_POINT('Origin',(18.3,91.08,8.));
#74712=CARTESIAN_POINT('',(18.3,91.08,8.));
#74713=CARTESIAN_POINT('',(18.3,90.92,8.));
#74714=CARTESIAN_POINT('',(18.3,80.54,8.));
#74715=CARTESIAN_POINT('',(18.18,91.08,8.));
#74716=CARTESIAN_POINT('',(18.3,91.08,8.));
#74717=CARTESIAN_POINT('',(18.18,90.92,8.));
#74718=CARTESIAN_POINT('',(18.18,90.92,8.));
#74719=CARTESIAN_POINT('',(18.3,90.92,8.));
#74720=CARTESIAN_POINT('Origin',(18.3,91.08,9.4));
#74721=CARTESIAN_POINT('',(18.3,91.08,9.4));
#74722=CARTESIAN_POINT('',(18.3,91.08,7.45));
#74723=CARTESIAN_POINT('',(18.18,91.08,9.4));
#74724=CARTESIAN_POINT('',(18.3,91.08,9.4));
#74725=CARTESIAN_POINT('',(18.18,91.08,8.));
#74726=CARTESIAN_POINT('Origin',(18.3,90.92,9.4));
#74727=CARTESIAN_POINT('',(18.3,90.92,9.4));
#74728=CARTESIAN_POINT('',(18.3,80.46,9.4));
#74729=CARTESIAN_POINT('',(18.18,90.92,9.4));
#74730=CARTESIAN_POINT('',(18.3,90.92,9.4));
#74731=CARTESIAN_POINT('',(18.18,91.08,9.4));
#74732=CARTESIAN_POINT('Origin',(18.3,90.92,8.));
#74733=CARTESIAN_POINT('',(18.3,90.92,6.75));
#74734=CARTESIAN_POINT('',(18.18,90.92,9.4));
#74735=CARTESIAN_POINT('Origin',(18.18,91.,8.7));
#74736=CARTESIAN_POINT('Origin',(18.3,89.08,8.));
#74737=CARTESIAN_POINT('',(18.3,89.08,8.));
#74738=CARTESIAN_POINT('',(18.3,88.92,8.));
#74739=CARTESIAN_POINT('',(18.3,79.54,8.));
#74740=CARTESIAN_POINT('',(18.18,89.08,8.));
#74741=CARTESIAN_POINT('',(18.3,89.08,8.));
#74742=CARTESIAN_POINT('',(18.18,88.92,8.));
#74743=CARTESIAN_POINT('',(18.18,88.92,8.));
#74744=CARTESIAN_POINT('',(18.3,88.92,8.));
#74745=CARTESIAN_POINT('Origin',(18.3,89.08,9.4));
#74746=CARTESIAN_POINT('',(18.3,89.08,9.4));
#74747=CARTESIAN_POINT('',(18.3,89.08,7.45));
#74748=CARTESIAN_POINT('',(18.18,89.08,9.4));
#74749=CARTESIAN_POINT('',(18.3,89.08,9.4));
#74750=CARTESIAN_POINT('',(18.18,89.08,8.));
#74751=CARTESIAN_POINT('Origin',(18.3,88.92,9.4));
#74752=CARTESIAN_POINT('',(18.3,88.92,9.4));
#74753=CARTESIAN_POINT('',(18.3,79.46,9.4));
#74754=CARTESIAN_POINT('',(18.18,88.92,9.4));
#74755=CARTESIAN_POINT('',(18.3,88.92,9.4));
#74756=CARTESIAN_POINT('',(18.18,89.08,9.4));
#74757=CARTESIAN_POINT('Origin',(18.3,88.92,8.));
#74758=CARTESIAN_POINT('',(18.3,88.92,6.75));
#74759=CARTESIAN_POINT('',(18.18,88.92,9.4));
#74760=CARTESIAN_POINT('Origin',(18.18,89.,8.7));
#74761=CARTESIAN_POINT('Origin',(18.3,87.08,8.));
#74762=CARTESIAN_POINT('',(18.3,87.08,8.));
#74763=CARTESIAN_POINT('',(18.3,86.92,8.));
#74764=CARTESIAN_POINT('',(18.3,78.54,8.));
#74765=CARTESIAN_POINT('',(18.18,87.08,8.));
#74766=CARTESIAN_POINT('',(18.3,87.08,8.));
#74767=CARTESIAN_POINT('',(18.18,86.92,8.));
#74768=CARTESIAN_POINT('',(18.18,86.92,8.));
#74769=CARTESIAN_POINT('',(18.3,86.92,8.));
#74770=CARTESIAN_POINT('Origin',(18.3,87.08,9.4));
#74771=CARTESIAN_POINT('',(18.3,87.08,9.4));
#74772=CARTESIAN_POINT('',(18.3,87.08,7.45));
#74773=CARTESIAN_POINT('',(18.18,87.08,9.4));
#74774=CARTESIAN_POINT('',(18.3,87.08,9.4));
#74775=CARTESIAN_POINT('',(18.18,87.08,8.));
#74776=CARTESIAN_POINT('Origin',(18.3,86.92,9.4));
#74777=CARTESIAN_POINT('',(18.3,86.92,9.4));
#74778=CARTESIAN_POINT('',(18.3,78.46,9.4));
#74779=CARTESIAN_POINT('',(18.18,86.92,9.4));
#74780=CARTESIAN_POINT('',(18.3,86.92,9.4));
#74781=CARTESIAN_POINT('',(18.18,87.08,9.4));
#74782=CARTESIAN_POINT('Origin',(18.3,86.92,8.));
#74783=CARTESIAN_POINT('',(18.3,86.92,6.75));
#74784=CARTESIAN_POINT('',(18.18,86.92,9.4));
#74785=CARTESIAN_POINT('Origin',(18.18,87.,8.7));
#74786=CARTESIAN_POINT('Origin',(18.3,85.08,7.2));
#74787=CARTESIAN_POINT('',(18.3,85.08,7.2));
#74788=CARTESIAN_POINT('',(18.3,84.92,7.2));
#74789=CARTESIAN_POINT('',(18.3,77.54,7.2));
#74790=CARTESIAN_POINT('',(18.18,85.08,7.2));
#74791=CARTESIAN_POINT('',(18.3,85.08,7.2));
#74792=CARTESIAN_POINT('',(18.18,84.92,7.2));
#74793=CARTESIAN_POINT('',(18.18,84.92,7.2));
#74794=CARTESIAN_POINT('',(18.3,84.92,7.2));
#74795=CARTESIAN_POINT('Origin',(18.3,85.08,9.4));
#74796=CARTESIAN_POINT('',(18.3,85.08,9.4));
#74797=CARTESIAN_POINT('',(18.3,85.08,7.45));
#74798=CARTESIAN_POINT('',(18.18,85.08,9.4));
#74799=CARTESIAN_POINT('',(18.3,85.08,9.4));
#74800=CARTESIAN_POINT('',(18.18,85.08,7.2));
#74801=CARTESIAN_POINT('Origin',(18.3,84.92,9.4));
#74802=CARTESIAN_POINT('',(18.3,84.92,9.4));
#74803=CARTESIAN_POINT('',(18.3,77.46,9.4));
#74804=CARTESIAN_POINT('',(18.18,84.92,9.4));
#74805=CARTESIAN_POINT('',(18.3,84.92,9.4));
#74806=CARTESIAN_POINT('',(18.18,85.08,9.4));
#74807=CARTESIAN_POINT('Origin',(18.3,84.92,7.2));
#74808=CARTESIAN_POINT('',(18.3,84.92,6.35));
#74809=CARTESIAN_POINT('',(18.18,84.92,9.4));
#74810=CARTESIAN_POINT('Origin',(18.18,85.,8.3));
#74811=CARTESIAN_POINT('Origin',(18.3,83.08,8.));
#74812=CARTESIAN_POINT('',(18.3,83.08,8.));
#74813=CARTESIAN_POINT('',(18.3,82.92,8.));
#74814=CARTESIAN_POINT('',(18.3,76.54,8.));
#74815=CARTESIAN_POINT('',(18.18,83.08,8.));
#74816=CARTESIAN_POINT('',(18.3,83.08,8.));
#74817=CARTESIAN_POINT('',(18.18,82.92,8.));
#74818=CARTESIAN_POINT('',(18.18,82.92,8.));
#74819=CARTESIAN_POINT('',(18.3,82.92,8.));
#74820=CARTESIAN_POINT('Origin',(18.3,83.08,9.4));
#74821=CARTESIAN_POINT('',(18.3,83.08,9.4));
#74822=CARTESIAN_POINT('',(18.3,83.08,7.45));
#74823=CARTESIAN_POINT('',(18.18,83.08,9.4));
#74824=CARTESIAN_POINT('',(18.3,83.08,9.4));
#74825=CARTESIAN_POINT('',(18.18,83.08,8.));
#74826=CARTESIAN_POINT('Origin',(18.3,82.92,9.4));
#74827=CARTESIAN_POINT('',(18.3,82.92,9.4));
#74828=CARTESIAN_POINT('',(18.3,76.46,9.4));
#74829=CARTESIAN_POINT('',(18.18,82.92,9.4));
#74830=CARTESIAN_POINT('',(18.3,82.92,9.4));
#74831=CARTESIAN_POINT('',(18.18,83.08,9.4));
#74832=CARTESIAN_POINT('Origin',(18.3,82.92,8.));
#74833=CARTESIAN_POINT('',(18.3,82.92,6.75));
#74834=CARTESIAN_POINT('',(18.18,82.92,9.4));
#74835=CARTESIAN_POINT('Origin',(18.18,83.,8.7));
#74836=CARTESIAN_POINT('Origin',(18.3,81.08,8.));
#74837=CARTESIAN_POINT('',(18.3,81.08,8.));
#74838=CARTESIAN_POINT('',(18.3,80.92,8.));
#74839=CARTESIAN_POINT('',(18.3,75.54,8.));
#74840=CARTESIAN_POINT('',(18.18,81.08,8.));
#74841=CARTESIAN_POINT('',(18.3,81.08,8.));
#74842=CARTESIAN_POINT('',(18.18,80.92,8.));
#74843=CARTESIAN_POINT('',(18.18,80.92,8.));
#74844=CARTESIAN_POINT('',(18.3,80.92,8.));
#74845=CARTESIAN_POINT('Origin',(18.3,81.08,9.4));
#74846=CARTESIAN_POINT('',(18.3,81.08,9.4));
#74847=CARTESIAN_POINT('',(18.3,81.08,7.45));
#74848=CARTESIAN_POINT('',(18.18,81.08,9.4));
#74849=CARTESIAN_POINT('',(18.3,81.08,9.4));
#74850=CARTESIAN_POINT('',(18.18,81.08,8.));
#74851=CARTESIAN_POINT('Origin',(18.3,80.92,9.4));
#74852=CARTESIAN_POINT('',(18.3,80.92,9.4));
#74853=CARTESIAN_POINT('',(18.3,75.46,9.4));
#74854=CARTESIAN_POINT('',(18.18,80.92,9.4));
#74855=CARTESIAN_POINT('',(18.3,80.92,9.4));
#74856=CARTESIAN_POINT('',(18.18,81.08,9.4));
#74857=CARTESIAN_POINT('Origin',(18.3,80.92,8.));
#74858=CARTESIAN_POINT('',(18.3,80.92,6.75));
#74859=CARTESIAN_POINT('',(18.18,80.92,9.4));
#74860=CARTESIAN_POINT('Origin',(18.18,81.,8.7));
#74861=CARTESIAN_POINT('Origin',(18.3,79.08,8.));
#74862=CARTESIAN_POINT('',(18.3,79.08,8.));
#74863=CARTESIAN_POINT('',(18.3,78.92,8.));
#74864=CARTESIAN_POINT('',(18.3,74.54,8.));
#74865=CARTESIAN_POINT('',(18.18,79.08,8.));
#74866=CARTESIAN_POINT('',(18.3,79.08,8.));
#74867=CARTESIAN_POINT('',(18.18,78.92,8.));
#74868=CARTESIAN_POINT('',(18.18,78.92,8.));
#74869=CARTESIAN_POINT('',(18.3,78.92,8.));
#74870=CARTESIAN_POINT('Origin',(18.3,79.08,9.4));
#74871=CARTESIAN_POINT('',(18.3,79.08,9.4));
#74872=CARTESIAN_POINT('',(18.3,79.08,7.45));
#74873=CARTESIAN_POINT('',(18.18,79.08,9.4));
#74874=CARTESIAN_POINT('',(18.3,79.08,9.4));
#74875=CARTESIAN_POINT('',(18.18,79.08,8.));
#74876=CARTESIAN_POINT('Origin',(18.3,78.92,9.4));
#74877=CARTESIAN_POINT('',(18.3,78.92,9.4));
#74878=CARTESIAN_POINT('',(18.3,74.46,9.4));
#74879=CARTESIAN_POINT('',(18.18,78.92,9.4));
#74880=CARTESIAN_POINT('',(18.3,78.92,9.4));
#74881=CARTESIAN_POINT('',(18.18,79.08,9.4));
#74882=CARTESIAN_POINT('Origin',(18.3,78.92,8.));
#74883=CARTESIAN_POINT('',(18.3,78.92,6.75));
#74884=CARTESIAN_POINT('',(18.18,78.92,9.4));
#74885=CARTESIAN_POINT('Origin',(18.18,79.,8.7));
#74886=CARTESIAN_POINT('Origin',(18.3,77.08,8.));
#74887=CARTESIAN_POINT('',(18.3,77.08,8.));
#74888=CARTESIAN_POINT('',(18.3,76.92,8.));
#74889=CARTESIAN_POINT('',(18.3,73.54,8.));
#74890=CARTESIAN_POINT('',(18.18,77.08,8.));
#74891=CARTESIAN_POINT('',(18.3,77.08,8.));
#74892=CARTESIAN_POINT('',(18.18,76.92,8.));
#74893=CARTESIAN_POINT('',(18.18,76.92,8.));
#74894=CARTESIAN_POINT('',(18.3,76.92,8.));
#74895=CARTESIAN_POINT('Origin',(18.3,77.08,9.4));
#74896=CARTESIAN_POINT('',(18.3,77.08,9.4));
#74897=CARTESIAN_POINT('',(18.3,77.08,7.45));
#74898=CARTESIAN_POINT('',(18.18,77.08,9.4));
#74899=CARTESIAN_POINT('',(18.3,77.08,9.4));
#74900=CARTESIAN_POINT('',(18.18,77.08,8.));
#74901=CARTESIAN_POINT('Origin',(18.3,76.92,9.4));
#74902=CARTESIAN_POINT('',(18.3,76.92,9.4));
#74903=CARTESIAN_POINT('',(18.3,73.46,9.4));
#74904=CARTESIAN_POINT('',(18.18,76.92,9.4));
#74905=CARTESIAN_POINT('',(18.3,76.92,9.4));
#74906=CARTESIAN_POINT('',(18.18,77.08,9.4));
#74907=CARTESIAN_POINT('Origin',(18.3,76.92,8.));
#74908=CARTESIAN_POINT('',(18.3,76.92,6.75));
#74909=CARTESIAN_POINT('',(18.18,76.92,9.4));
#74910=CARTESIAN_POINT('Origin',(18.18,77.,8.7));
#74911=CARTESIAN_POINT('Origin',(18.3,75.08,7.2));
#74912=CARTESIAN_POINT('',(18.3,75.08,7.2));
#74913=CARTESIAN_POINT('',(18.3,74.92,7.2));
#74914=CARTESIAN_POINT('',(18.3,72.54,7.2));
#74915=CARTESIAN_POINT('',(18.18,75.08,7.2));
#74916=CARTESIAN_POINT('',(18.3,75.08,7.2));
#74917=CARTESIAN_POINT('',(18.18,74.92,7.2));
#74918=CARTESIAN_POINT('',(18.18,74.92,7.2));
#74919=CARTESIAN_POINT('',(18.3,74.92,7.2));
#74920=CARTESIAN_POINT('Origin',(18.3,75.08,9.4));
#74921=CARTESIAN_POINT('',(18.3,75.08,9.4));
#74922=CARTESIAN_POINT('',(18.3,75.08,7.45));
#74923=CARTESIAN_POINT('',(18.18,75.08,9.4));
#74924=CARTESIAN_POINT('',(18.3,75.08,9.4));
#74925=CARTESIAN_POINT('',(18.18,75.08,7.2));
#74926=CARTESIAN_POINT('Origin',(18.3,74.92,9.4));
#74927=CARTESIAN_POINT('',(18.3,74.92,9.4));
#74928=CARTESIAN_POINT('',(18.3,72.46,9.4));
#74929=CARTESIAN_POINT('',(18.18,74.92,9.4));
#74930=CARTESIAN_POINT('',(18.3,74.92,9.4));
#74931=CARTESIAN_POINT('',(18.18,75.08,9.4));
#74932=CARTESIAN_POINT('Origin',(18.3,74.92,7.2));
#74933=CARTESIAN_POINT('',(18.3,74.92,6.35));
#74934=CARTESIAN_POINT('',(18.18,74.92,9.4));
#74935=CARTESIAN_POINT('Origin',(18.18,75.,8.3));
#74936=CARTESIAN_POINT('Origin',(18.3,73.08,8.));
#74937=CARTESIAN_POINT('',(18.3,73.08,8.));
#74938=CARTESIAN_POINT('',(18.3,72.92,8.));
#74939=CARTESIAN_POINT('',(18.3,71.54,8.));
#74940=CARTESIAN_POINT('',(18.18,73.08,8.));
#74941=CARTESIAN_POINT('',(18.3,73.08,8.));
#74942=CARTESIAN_POINT('',(18.18,72.92,8.));
#74943=CARTESIAN_POINT('',(18.18,72.92,8.));
#74944=CARTESIAN_POINT('',(18.3,72.92,8.));
#74945=CARTESIAN_POINT('Origin',(18.3,73.08,9.4));
#74946=CARTESIAN_POINT('',(18.3,73.08,9.4));
#74947=CARTESIAN_POINT('',(18.3,73.08,7.45));
#74948=CARTESIAN_POINT('',(18.18,73.08,9.4));
#74949=CARTESIAN_POINT('',(18.3,73.08,9.4));
#74950=CARTESIAN_POINT('',(18.18,73.08,8.));
#74951=CARTESIAN_POINT('Origin',(18.3,72.92,9.4));
#74952=CARTESIAN_POINT('',(18.3,72.92,9.4));
#74953=CARTESIAN_POINT('',(18.3,71.46,9.4));
#74954=CARTESIAN_POINT('',(18.18,72.92,9.4));
#74955=CARTESIAN_POINT('',(18.3,72.92,9.4));
#74956=CARTESIAN_POINT('',(18.18,73.08,9.4));
#74957=CARTESIAN_POINT('Origin',(18.3,72.92,8.));
#74958=CARTESIAN_POINT('',(18.3,72.92,6.75));
#74959=CARTESIAN_POINT('',(18.18,72.92,9.4));
#74960=CARTESIAN_POINT('Origin',(18.18,73.,8.7));
#74961=CARTESIAN_POINT('Origin',(18.3,71.08,8.));
#74962=CARTESIAN_POINT('',(18.3,71.08,8.));
#74963=CARTESIAN_POINT('',(18.3,70.92,8.));
#74964=CARTESIAN_POINT('',(18.3,70.54,8.));
#74965=CARTESIAN_POINT('',(18.18,71.08,8.));
#74966=CARTESIAN_POINT('',(18.3,71.08,8.));
#74967=CARTESIAN_POINT('',(18.18,70.92,8.));
#74968=CARTESIAN_POINT('',(18.18,70.92,8.));
#74969=CARTESIAN_POINT('',(18.3,70.92,8.));
#74970=CARTESIAN_POINT('Origin',(18.3,71.08,9.4));
#74971=CARTESIAN_POINT('',(18.3,71.08,9.4));
#74972=CARTESIAN_POINT('',(18.3,71.08,7.45));
#74973=CARTESIAN_POINT('',(18.18,71.08,9.4));
#74974=CARTESIAN_POINT('',(18.3,71.08,9.4));
#74975=CARTESIAN_POINT('',(18.18,71.08,8.));
#74976=CARTESIAN_POINT('Origin',(18.3,70.92,9.4));
#74977=CARTESIAN_POINT('',(18.3,70.92,9.4));
#74978=CARTESIAN_POINT('',(18.3,70.46,9.4));
#74979=CARTESIAN_POINT('',(18.18,70.92,9.4));
#74980=CARTESIAN_POINT('',(18.3,70.92,9.4));
#74981=CARTESIAN_POINT('',(18.18,71.08,9.4));
#74982=CARTESIAN_POINT('Origin',(18.3,70.92,8.));
#74983=CARTESIAN_POINT('',(18.3,70.92,6.75));
#74984=CARTESIAN_POINT('',(18.18,70.92,9.4));
#74985=CARTESIAN_POINT('Origin',(18.18,71.,8.7));
#74986=CARTESIAN_POINT('Origin',(18.3,70.08,6.4));
#74987=CARTESIAN_POINT('',(18.3,70.08,6.4));
#74988=CARTESIAN_POINT('',(18.3,69.92,6.4));
#74989=CARTESIAN_POINT('',(18.3,70.04,6.4));
#74990=CARTESIAN_POINT('',(18.18,70.08,6.4));
#74991=CARTESIAN_POINT('',(18.3,70.08,6.4));
#74992=CARTESIAN_POINT('',(18.18,69.92,6.4));
#74993=CARTESIAN_POINT('',(18.18,69.92,6.4));
#74994=CARTESIAN_POINT('',(18.3,69.92,6.4));
#74995=CARTESIAN_POINT('Origin',(18.3,70.08,9.4));
#74996=CARTESIAN_POINT('',(18.3,70.08,9.4));
#74997=CARTESIAN_POINT('',(18.3,70.08,7.45));
#74998=CARTESIAN_POINT('',(18.18,70.08,9.4));
#74999=CARTESIAN_POINT('',(18.3,70.08,9.4));
#75000=CARTESIAN_POINT('',(18.18,70.08,6.4));
#75001=CARTESIAN_POINT('Origin',(18.3,69.92,9.4));
#75002=CARTESIAN_POINT('',(18.3,69.92,9.4));
#75003=CARTESIAN_POINT('',(18.3,69.96,9.4));
#75004=CARTESIAN_POINT('',(18.18,69.92,9.4));
#75005=CARTESIAN_POINT('',(18.3,69.92,9.4));
#75006=CARTESIAN_POINT('',(18.18,70.08,9.4));
#75007=CARTESIAN_POINT('Origin',(18.3,69.92,6.4));
#75008=CARTESIAN_POINT('',(18.3,69.92,5.95));
#75009=CARTESIAN_POINT('',(18.18,69.92,9.4));
#75010=CARTESIAN_POINT('Origin',(18.18,70.,7.9));
#75011=CARTESIAN_POINT('Origin',(18.3,68.08,8.));
#75012=CARTESIAN_POINT('',(18.3,68.08,8.));
#75013=CARTESIAN_POINT('',(18.3,67.92,8.));
#75014=CARTESIAN_POINT('',(18.3,69.04,8.));
#75015=CARTESIAN_POINT('',(18.18,68.08,8.));
#75016=CARTESIAN_POINT('',(18.3,68.08,8.));
#75017=CARTESIAN_POINT('',(18.18,67.92,8.));
#75018=CARTESIAN_POINT('',(18.18,67.92,8.));
#75019=CARTESIAN_POINT('',(18.3,67.92,8.));
#75020=CARTESIAN_POINT('Origin',(18.3,68.08,9.4));
#75021=CARTESIAN_POINT('',(18.3,68.08,9.4));
#75022=CARTESIAN_POINT('',(18.3,68.08,7.45));
#75023=CARTESIAN_POINT('',(18.18,68.08,9.4));
#75024=CARTESIAN_POINT('',(18.3,68.08,9.4));
#75025=CARTESIAN_POINT('',(18.18,68.08,8.));
#75026=CARTESIAN_POINT('Origin',(18.3,67.92,9.4));
#75027=CARTESIAN_POINT('',(18.3,67.92,9.4));
#75028=CARTESIAN_POINT('',(18.3,68.96,9.4));
#75029=CARTESIAN_POINT('',(18.18,67.92,9.4));
#75030=CARTESIAN_POINT('',(18.3,67.92,9.4));
#75031=CARTESIAN_POINT('',(18.18,68.08,9.4));
#75032=CARTESIAN_POINT('Origin',(18.3,67.92,8.));
#75033=CARTESIAN_POINT('',(18.3,67.92,6.75));
#75034=CARTESIAN_POINT('',(18.18,67.92,9.4));
#75035=CARTESIAN_POINT('Origin',(18.18,68.,8.7));
#75036=CARTESIAN_POINT('Origin',(18.3,66.08,8.));
#75037=CARTESIAN_POINT('',(18.3,66.08,8.));
#75038=CARTESIAN_POINT('',(18.3,65.92,8.));
#75039=CARTESIAN_POINT('',(18.3,68.04,8.));
#75040=CARTESIAN_POINT('',(18.18,66.08,8.));
#75041=CARTESIAN_POINT('',(18.3,66.08,8.));
#75042=CARTESIAN_POINT('',(18.18,65.92,8.));
#75043=CARTESIAN_POINT('',(18.18,65.92,8.));
#75044=CARTESIAN_POINT('',(18.3,65.92,8.));
#75045=CARTESIAN_POINT('Origin',(18.3,66.08,9.4));
#75046=CARTESIAN_POINT('',(18.3,66.08,9.4));
#75047=CARTESIAN_POINT('',(18.3,66.08,7.45));
#75048=CARTESIAN_POINT('',(18.18,66.08,9.4));
#75049=CARTESIAN_POINT('',(18.3,66.08,9.4));
#75050=CARTESIAN_POINT('',(18.18,66.08,8.));
#75051=CARTESIAN_POINT('Origin',(18.3,65.92,9.4));
#75052=CARTESIAN_POINT('',(18.3,65.92,9.4));
#75053=CARTESIAN_POINT('',(18.3,67.96,9.4));
#75054=CARTESIAN_POINT('',(18.18,65.92,9.4));
#75055=CARTESIAN_POINT('',(18.3,65.92,9.4));
#75056=CARTESIAN_POINT('',(18.18,66.08,9.4));
#75057=CARTESIAN_POINT('Origin',(18.3,65.92,8.));
#75058=CARTESIAN_POINT('',(18.3,65.92,6.75));
#75059=CARTESIAN_POINT('',(18.18,65.92,9.4));
#75060=CARTESIAN_POINT('Origin',(18.18,66.,8.7));
#75061=CARTESIAN_POINT('Origin',(18.3,64.08,8.));
#75062=CARTESIAN_POINT('',(18.3,64.08,8.));
#75063=CARTESIAN_POINT('',(18.3,63.92,8.));
#75064=CARTESIAN_POINT('',(18.3,67.04,8.));
#75065=CARTESIAN_POINT('',(18.18,64.08,8.));
#75066=CARTESIAN_POINT('',(18.3,64.08,8.));
#75067=CARTESIAN_POINT('',(18.18,63.92,8.));
#75068=CARTESIAN_POINT('',(18.18,63.92,8.));
#75069=CARTESIAN_POINT('',(18.3,63.92,8.));
#75070=CARTESIAN_POINT('Origin',(18.3,64.08,9.4));
#75071=CARTESIAN_POINT('',(18.3,64.08,9.4));
#75072=CARTESIAN_POINT('',(18.3,64.08,7.45));
#75073=CARTESIAN_POINT('',(18.18,64.08,9.4));
#75074=CARTESIAN_POINT('',(18.3,64.08,9.4));
#75075=CARTESIAN_POINT('',(18.18,64.08,8.));
#75076=CARTESIAN_POINT('Origin',(18.3,63.92,9.4));
#75077=CARTESIAN_POINT('',(18.3,63.92,9.4));
#75078=CARTESIAN_POINT('',(18.3,66.96,9.4));
#75079=CARTESIAN_POINT('',(18.18,63.92,9.4));
#75080=CARTESIAN_POINT('',(18.3,63.92,9.4));
#75081=CARTESIAN_POINT('',(18.18,64.08,9.4));
#75082=CARTESIAN_POINT('Origin',(18.3,63.92,8.));
#75083=CARTESIAN_POINT('',(18.3,63.92,6.75));
#75084=CARTESIAN_POINT('',(18.18,63.92,9.4));
#75085=CARTESIAN_POINT('Origin',(18.18,64.,8.7));
#75086=CARTESIAN_POINT('Origin',(18.3,62.08,8.));
#75087=CARTESIAN_POINT('',(18.3,62.08,8.));
#75088=CARTESIAN_POINT('',(18.3,61.92,8.));
#75089=CARTESIAN_POINT('',(18.3,66.04,8.));
#75090=CARTESIAN_POINT('',(18.18,62.08,8.));
#75091=CARTESIAN_POINT('',(18.3,62.08,8.));
#75092=CARTESIAN_POINT('',(18.18,61.92,8.));
#75093=CARTESIAN_POINT('',(18.18,61.92,8.));
#75094=CARTESIAN_POINT('',(18.3,61.92,8.));
#75095=CARTESIAN_POINT('Origin',(18.3,62.08,9.4));
#75096=CARTESIAN_POINT('',(18.3,62.08,9.4));
#75097=CARTESIAN_POINT('',(18.3,62.08,7.45));
#75098=CARTESIAN_POINT('',(18.18,62.08,9.4));
#75099=CARTESIAN_POINT('',(18.3,62.08,9.4));
#75100=CARTESIAN_POINT('',(18.18,62.08,8.));
#75101=CARTESIAN_POINT('Origin',(18.3,61.92,9.4));
#75102=CARTESIAN_POINT('',(18.3,61.92,9.4));
#75103=CARTESIAN_POINT('',(18.3,65.96,9.4));
#75104=CARTESIAN_POINT('',(18.18,61.92,9.4));
#75105=CARTESIAN_POINT('',(18.3,61.92,9.4));
#75106=CARTESIAN_POINT('',(18.18,62.08,9.4));
#75107=CARTESIAN_POINT('Origin',(18.3,61.92,8.));
#75108=CARTESIAN_POINT('',(18.3,61.92,6.75));
#75109=CARTESIAN_POINT('',(18.18,61.92,9.4));
#75110=CARTESIAN_POINT('Origin',(18.18,62.,8.7));
#75111=CARTESIAN_POINT('Origin',(18.3,60.08,6.4));
#75112=CARTESIAN_POINT('',(18.3,60.08,6.4));
#75113=CARTESIAN_POINT('',(18.3,59.92,6.4));
#75114=CARTESIAN_POINT('',(18.3,65.04,6.4));
#75115=CARTESIAN_POINT('',(18.18,60.08,6.4));
#75116=CARTESIAN_POINT('',(18.3,60.08,6.4));
#75117=CARTESIAN_POINT('',(18.18,59.92,6.4));
#75118=CARTESIAN_POINT('',(18.18,59.92,6.4));
#75119=CARTESIAN_POINT('',(18.3,59.92,6.4));
#75120=CARTESIAN_POINT('Origin',(18.3,60.08,9.4));
#75121=CARTESIAN_POINT('',(18.3,60.08,9.4));
#75122=CARTESIAN_POINT('',(18.3,60.08,7.45));
#75123=CARTESIAN_POINT('',(18.18,60.08,9.4));
#75124=CARTESIAN_POINT('',(18.3,60.08,9.4));
#75125=CARTESIAN_POINT('',(18.18,60.08,6.4));
#75126=CARTESIAN_POINT('Origin',(18.3,59.92,9.4));
#75127=CARTESIAN_POINT('',(18.3,59.92,9.4));
#75128=CARTESIAN_POINT('',(18.3,64.96,9.4));
#75129=CARTESIAN_POINT('',(18.18,59.92,9.4));
#75130=CARTESIAN_POINT('',(18.3,59.92,9.4));
#75131=CARTESIAN_POINT('',(18.18,60.08,9.4));
#75132=CARTESIAN_POINT('Origin',(18.3,59.92,6.4));
#75133=CARTESIAN_POINT('',(18.3,59.92,5.95));
#75134=CARTESIAN_POINT('',(18.18,59.92,9.4));
#75135=CARTESIAN_POINT('Origin',(18.18,60.,7.9));
#75136=CARTESIAN_POINT('Origin',(18.3,58.08,8.));
#75137=CARTESIAN_POINT('',(18.3,58.08,8.));
#75138=CARTESIAN_POINT('',(18.3,57.92,8.));
#75139=CARTESIAN_POINT('',(18.3,64.04,8.));
#75140=CARTESIAN_POINT('',(18.18,58.08,8.));
#75141=CARTESIAN_POINT('',(18.3,58.08,8.));
#75142=CARTESIAN_POINT('',(18.18,57.92,8.));
#75143=CARTESIAN_POINT('',(18.18,57.92,8.));
#75144=CARTESIAN_POINT('',(18.3,57.92,8.));
#75145=CARTESIAN_POINT('Origin',(18.3,58.08,9.4));
#75146=CARTESIAN_POINT('',(18.3,58.08,9.4));
#75147=CARTESIAN_POINT('',(18.3,58.08,7.45));
#75148=CARTESIAN_POINT('',(18.18,58.08,9.4));
#75149=CARTESIAN_POINT('',(18.3,58.08,9.4));
#75150=CARTESIAN_POINT('',(18.18,58.08,8.));
#75151=CARTESIAN_POINT('Origin',(18.3,57.92,9.4));
#75152=CARTESIAN_POINT('',(18.3,57.92,9.4));
#75153=CARTESIAN_POINT('',(18.3,63.96,9.4));
#75154=CARTESIAN_POINT('',(18.18,57.92,9.4));
#75155=CARTESIAN_POINT('',(18.3,57.92,9.4));
#75156=CARTESIAN_POINT('',(18.18,58.08,9.4));
#75157=CARTESIAN_POINT('Origin',(18.3,57.92,8.));
#75158=CARTESIAN_POINT('',(18.3,57.92,6.75));
#75159=CARTESIAN_POINT('',(18.18,57.92,9.4));
#75160=CARTESIAN_POINT('Origin',(18.18,58.,8.7));
#75161=CARTESIAN_POINT('Origin',(18.3,56.08,8.));
#75162=CARTESIAN_POINT('',(18.3,56.08,8.));
#75163=CARTESIAN_POINT('',(18.3,55.92,8.));
#75164=CARTESIAN_POINT('',(18.3,63.04,8.));
#75165=CARTESIAN_POINT('',(18.18,56.08,8.));
#75166=CARTESIAN_POINT('',(18.3,56.08,8.));
#75167=CARTESIAN_POINT('',(18.18,55.92,8.));
#75168=CARTESIAN_POINT('',(18.18,55.92,8.));
#75169=CARTESIAN_POINT('',(18.3,55.92,8.));
#75170=CARTESIAN_POINT('Origin',(18.3,56.08,9.4));
#75171=CARTESIAN_POINT('',(18.3,56.08,9.4));
#75172=CARTESIAN_POINT('',(18.3,56.08,7.45));
#75173=CARTESIAN_POINT('',(18.18,56.08,9.4));
#75174=CARTESIAN_POINT('',(18.3,56.08,9.4));
#75175=CARTESIAN_POINT('',(18.18,56.08,8.));
#75176=CARTESIAN_POINT('Origin',(18.3,55.92,9.4));
#75177=CARTESIAN_POINT('',(18.3,55.92,9.4));
#75178=CARTESIAN_POINT('',(18.3,62.96,9.4));
#75179=CARTESIAN_POINT('',(18.18,55.92,9.4));
#75180=CARTESIAN_POINT('',(18.3,55.92,9.4));
#75181=CARTESIAN_POINT('',(18.18,56.08,9.4));
#75182=CARTESIAN_POINT('Origin',(18.3,55.92,8.));
#75183=CARTESIAN_POINT('',(18.3,55.92,6.75));
#75184=CARTESIAN_POINT('',(18.18,55.92,9.4));
#75185=CARTESIAN_POINT('Origin',(18.18,56.,8.7));
#75186=CARTESIAN_POINT('Origin',(18.3,54.08,8.));
#75187=CARTESIAN_POINT('',(18.3,54.08,8.));
#75188=CARTESIAN_POINT('',(18.3,53.92,8.));
#75189=CARTESIAN_POINT('',(18.3,62.04,8.));
#75190=CARTESIAN_POINT('',(18.18,54.08,8.));
#75191=CARTESIAN_POINT('',(18.3,54.08,8.));
#75192=CARTESIAN_POINT('',(18.18,53.92,8.));
#75193=CARTESIAN_POINT('',(18.18,53.92,8.));
#75194=CARTESIAN_POINT('',(18.3,53.92,8.));
#75195=CARTESIAN_POINT('Origin',(18.3,54.08,9.4));
#75196=CARTESIAN_POINT('',(18.3,54.08,9.4));
#75197=CARTESIAN_POINT('',(18.3,54.08,7.45));
#75198=CARTESIAN_POINT('',(18.18,54.08,9.4));
#75199=CARTESIAN_POINT('',(18.3,54.08,9.4));
#75200=CARTESIAN_POINT('',(18.18,54.08,8.));
#75201=CARTESIAN_POINT('Origin',(18.3,53.92,9.4));
#75202=CARTESIAN_POINT('',(18.3,53.92,9.4));
#75203=CARTESIAN_POINT('',(18.3,61.96,9.4));
#75204=CARTESIAN_POINT('',(18.18,53.92,9.4));
#75205=CARTESIAN_POINT('',(18.3,53.92,9.4));
#75206=CARTESIAN_POINT('',(18.18,54.08,9.4));
#75207=CARTESIAN_POINT('Origin',(18.3,53.92,8.));
#75208=CARTESIAN_POINT('',(18.3,53.92,6.75));
#75209=CARTESIAN_POINT('',(18.18,53.92,9.4));
#75210=CARTESIAN_POINT('Origin',(18.18,54.,8.7));
#75211=CARTESIAN_POINT('Origin',(18.3,52.08,8.));
#75212=CARTESIAN_POINT('',(18.3,52.08,8.));
#75213=CARTESIAN_POINT('',(18.3,51.92,8.));
#75214=CARTESIAN_POINT('',(18.3,61.04,8.));
#75215=CARTESIAN_POINT('',(18.18,52.08,8.));
#75216=CARTESIAN_POINT('',(18.3,52.08,8.));
#75217=CARTESIAN_POINT('',(18.18,51.92,8.));
#75218=CARTESIAN_POINT('',(18.18,51.92,8.));
#75219=CARTESIAN_POINT('',(18.3,51.92,8.));
#75220=CARTESIAN_POINT('Origin',(18.3,52.08,9.4));
#75221=CARTESIAN_POINT('',(18.3,52.08,9.4));
#75222=CARTESIAN_POINT('',(18.3,52.08,7.45));
#75223=CARTESIAN_POINT('',(18.18,52.08,9.4));
#75224=CARTESIAN_POINT('',(18.3,52.08,9.4));
#75225=CARTESIAN_POINT('',(18.18,52.08,8.));
#75226=CARTESIAN_POINT('Origin',(18.3,51.92,9.4));
#75227=CARTESIAN_POINT('',(18.3,51.92,9.4));
#75228=CARTESIAN_POINT('',(18.3,60.96,9.4));
#75229=CARTESIAN_POINT('',(18.18,51.92,9.4));
#75230=CARTESIAN_POINT('',(18.3,51.92,9.4));
#75231=CARTESIAN_POINT('',(18.18,52.08,9.4));
#75232=CARTESIAN_POINT('Origin',(18.3,51.92,8.));
#75233=CARTESIAN_POINT('',(18.3,51.92,6.75));
#75234=CARTESIAN_POINT('',(18.18,51.92,9.4));
#75235=CARTESIAN_POINT('Origin',(18.18,52.,8.7));
#75236=CARTESIAN_POINT('Origin',(18.3,50.08,6.4));
#75237=CARTESIAN_POINT('',(18.3,50.08,6.4));
#75238=CARTESIAN_POINT('',(18.3,49.92,6.4));
#75239=CARTESIAN_POINT('',(18.3,60.04,6.4));
#75240=CARTESIAN_POINT('',(18.18,50.08,6.4));
#75241=CARTESIAN_POINT('',(18.3,50.08,6.4));
#75242=CARTESIAN_POINT('',(18.18,49.92,6.4));
#75243=CARTESIAN_POINT('',(18.18,49.92,6.4));
#75244=CARTESIAN_POINT('',(18.3,49.92,6.4));
#75245=CARTESIAN_POINT('Origin',(18.3,50.08,9.4));
#75246=CARTESIAN_POINT('',(18.3,50.08,9.4));
#75247=CARTESIAN_POINT('',(18.3,50.08,7.45));
#75248=CARTESIAN_POINT('',(18.18,50.08,9.4));
#75249=CARTESIAN_POINT('',(18.3,50.08,9.4));
#75250=CARTESIAN_POINT('',(18.18,50.08,6.4));
#75251=CARTESIAN_POINT('Origin',(18.3,49.92,9.4));
#75252=CARTESIAN_POINT('',(18.3,49.92,9.4));
#75253=CARTESIAN_POINT('',(18.3,59.96,9.4));
#75254=CARTESIAN_POINT('',(18.18,49.92,9.4));
#75255=CARTESIAN_POINT('',(18.3,49.92,9.4));
#75256=CARTESIAN_POINT('',(18.18,50.08,9.4));
#75257=CARTESIAN_POINT('Origin',(18.3,49.92,6.4));
#75258=CARTESIAN_POINT('',(18.3,49.92,5.95));
#75259=CARTESIAN_POINT('',(18.18,49.92,9.4));
#75260=CARTESIAN_POINT('Origin',(18.18,50.,7.9));
#75261=CARTESIAN_POINT('Origin',(18.3,48.08,8.));
#75262=CARTESIAN_POINT('',(18.3,48.08,8.));
#75263=CARTESIAN_POINT('',(18.3,47.92,8.));
#75264=CARTESIAN_POINT('',(18.3,59.04,8.));
#75265=CARTESIAN_POINT('',(18.18,48.08,8.));
#75266=CARTESIAN_POINT('',(18.3,48.08,8.));
#75267=CARTESIAN_POINT('',(18.18,47.92,8.));
#75268=CARTESIAN_POINT('',(18.18,47.92,8.));
#75269=CARTESIAN_POINT('',(18.3,47.92,8.));
#75270=CARTESIAN_POINT('Origin',(18.3,48.08,9.4));
#75271=CARTESIAN_POINT('',(18.3,48.08,9.4));
#75272=CARTESIAN_POINT('',(18.3,48.08,7.45));
#75273=CARTESIAN_POINT('',(18.18,48.08,9.4));
#75274=CARTESIAN_POINT('',(18.3,48.08,9.4));
#75275=CARTESIAN_POINT('',(18.18,48.08,8.));
#75276=CARTESIAN_POINT('Origin',(18.3,47.92,9.4));
#75277=CARTESIAN_POINT('',(18.3,47.92,9.4));
#75278=CARTESIAN_POINT('',(18.3,58.96,9.4));
#75279=CARTESIAN_POINT('',(18.18,47.92,9.4));
#75280=CARTESIAN_POINT('',(18.3,47.92,9.4));
#75281=CARTESIAN_POINT('',(18.18,48.08,9.4));
#75282=CARTESIAN_POINT('Origin',(18.3,47.92,8.));
#75283=CARTESIAN_POINT('',(18.3,47.92,6.75));
#75284=CARTESIAN_POINT('',(18.18,47.92,9.4));
#75285=CARTESIAN_POINT('Origin',(18.18,48.,8.7));
#75286=CARTESIAN_POINT('Origin',(18.3,46.08,8.));
#75287=CARTESIAN_POINT('',(18.3,46.08,8.));
#75288=CARTESIAN_POINT('',(18.3,45.92,8.));
#75289=CARTESIAN_POINT('',(18.3,58.04,8.));
#75290=CARTESIAN_POINT('',(18.18,46.08,8.));
#75291=CARTESIAN_POINT('',(18.3,46.08,8.));
#75292=CARTESIAN_POINT('',(18.18,45.92,8.));
#75293=CARTESIAN_POINT('',(18.18,45.92,8.));
#75294=CARTESIAN_POINT('',(18.3,45.92,8.));
#75295=CARTESIAN_POINT('Origin',(18.3,46.08,9.4));
#75296=CARTESIAN_POINT('',(18.3,46.08,9.4));
#75297=CARTESIAN_POINT('',(18.3,46.08,7.45));
#75298=CARTESIAN_POINT('',(18.18,46.08,9.4));
#75299=CARTESIAN_POINT('',(18.3,46.08,9.4));
#75300=CARTESIAN_POINT('',(18.18,46.08,8.));
#75301=CARTESIAN_POINT('Origin',(18.3,45.92,9.4));
#75302=CARTESIAN_POINT('',(18.3,45.92,9.4));
#75303=CARTESIAN_POINT('',(18.3,57.96,9.4));
#75304=CARTESIAN_POINT('',(18.18,45.92,9.4));
#75305=CARTESIAN_POINT('',(18.3,45.92,9.4));
#75306=CARTESIAN_POINT('',(18.18,46.08,9.4));
#75307=CARTESIAN_POINT('Origin',(18.3,45.92,8.));
#75308=CARTESIAN_POINT('',(18.3,45.92,6.75));
#75309=CARTESIAN_POINT('',(18.18,45.92,9.4));
#75310=CARTESIAN_POINT('Origin',(18.18,46.,8.7));
#75311=CARTESIAN_POINT('Origin',(18.3,44.08,8.));
#75312=CARTESIAN_POINT('',(18.3,44.08,8.));
#75313=CARTESIAN_POINT('',(18.3,43.92,8.));
#75314=CARTESIAN_POINT('',(18.3,57.04,8.));
#75315=CARTESIAN_POINT('',(18.18,44.08,8.));
#75316=CARTESIAN_POINT('',(18.3,44.08,8.));
#75317=CARTESIAN_POINT('',(18.18,43.92,8.));
#75318=CARTESIAN_POINT('',(18.18,43.92,8.));
#75319=CARTESIAN_POINT('',(18.3,43.92,8.));
#75320=CARTESIAN_POINT('Origin',(18.3,44.08,9.4));
#75321=CARTESIAN_POINT('',(18.3,44.08,9.4));
#75322=CARTESIAN_POINT('',(18.3,44.08,7.45));
#75323=CARTESIAN_POINT('',(18.18,44.08,9.4));
#75324=CARTESIAN_POINT('',(18.3,44.08,9.4));
#75325=CARTESIAN_POINT('',(18.18,44.08,8.));
#75326=CARTESIAN_POINT('Origin',(18.3,43.92,9.4));
#75327=CARTESIAN_POINT('',(18.3,43.92,9.4));
#75328=CARTESIAN_POINT('',(18.3,56.96,9.4));
#75329=CARTESIAN_POINT('',(18.18,43.92,9.4));
#75330=CARTESIAN_POINT('',(18.3,43.92,9.4));
#75331=CARTESIAN_POINT('',(18.18,44.08,9.4));
#75332=CARTESIAN_POINT('Origin',(18.3,43.92,8.));
#75333=CARTESIAN_POINT('',(18.3,43.92,6.75));
#75334=CARTESIAN_POINT('',(18.18,43.92,9.4));
#75335=CARTESIAN_POINT('Origin',(18.18,44.,8.7));
#75336=CARTESIAN_POINT('Origin',(18.3,42.08,8.));
#75337=CARTESIAN_POINT('',(18.3,42.08,8.));
#75338=CARTESIAN_POINT('',(18.3,41.92,8.));
#75339=CARTESIAN_POINT('',(18.3,56.04,8.));
#75340=CARTESIAN_POINT('',(18.18,42.08,8.));
#75341=CARTESIAN_POINT('',(18.3,42.08,8.));
#75342=CARTESIAN_POINT('',(18.18,41.92,8.));
#75343=CARTESIAN_POINT('',(18.18,41.92,8.));
#75344=CARTESIAN_POINT('',(18.3,41.92,8.));
#75345=CARTESIAN_POINT('Origin',(18.3,42.08,9.4));
#75346=CARTESIAN_POINT('',(18.3,42.08,9.4));
#75347=CARTESIAN_POINT('',(18.3,42.08,7.45));
#75348=CARTESIAN_POINT('',(18.18,42.08,9.4));
#75349=CARTESIAN_POINT('',(18.3,42.08,9.4));
#75350=CARTESIAN_POINT('',(18.18,42.08,8.));
#75351=CARTESIAN_POINT('Origin',(18.3,41.92,9.4));
#75352=CARTESIAN_POINT('',(18.3,41.92,9.4));
#75353=CARTESIAN_POINT('',(18.3,55.96,9.4));
#75354=CARTESIAN_POINT('',(18.18,41.92,9.4));
#75355=CARTESIAN_POINT('',(18.3,41.92,9.4));
#75356=CARTESIAN_POINT('',(18.18,42.08,9.4));
#75357=CARTESIAN_POINT('Origin',(18.3,41.92,8.));
#75358=CARTESIAN_POINT('',(18.3,41.92,6.75));
#75359=CARTESIAN_POINT('',(18.18,41.92,9.4));
#75360=CARTESIAN_POINT('Origin',(18.18,42.,8.7));
#75361=CARTESIAN_POINT('Origin',(18.3,40.08,6.4));
#75362=CARTESIAN_POINT('',(18.3,40.08,6.4));
#75363=CARTESIAN_POINT('',(18.3,39.92,6.4));
#75364=CARTESIAN_POINT('',(18.3,55.04,6.4));
#75365=CARTESIAN_POINT('',(18.18,40.08,6.4));
#75366=CARTESIAN_POINT('',(18.3,40.08,6.4));
#75367=CARTESIAN_POINT('',(18.18,39.92,6.4));
#75368=CARTESIAN_POINT('',(18.18,39.92,6.4));
#75369=CARTESIAN_POINT('',(18.3,39.92,6.4));
#75370=CARTESIAN_POINT('Origin',(18.3,40.08,9.4));
#75371=CARTESIAN_POINT('',(18.3,40.08,9.4));
#75372=CARTESIAN_POINT('',(18.3,40.08,7.45));
#75373=CARTESIAN_POINT('',(18.18,40.08,9.4));
#75374=CARTESIAN_POINT('',(18.3,40.08,9.4));
#75375=CARTESIAN_POINT('',(18.18,40.08,6.4));
#75376=CARTESIAN_POINT('Origin',(18.3,39.92,9.4));
#75377=CARTESIAN_POINT('',(18.3,39.92,9.4));
#75378=CARTESIAN_POINT('',(18.3,54.96,9.4));
#75379=CARTESIAN_POINT('',(18.18,39.92,9.4));
#75380=CARTESIAN_POINT('',(18.3,39.92,9.4));
#75381=CARTESIAN_POINT('',(18.18,40.08,9.4));
#75382=CARTESIAN_POINT('Origin',(18.3,39.92,6.4));
#75383=CARTESIAN_POINT('',(18.3,39.92,5.95));
#75384=CARTESIAN_POINT('',(18.18,39.92,9.4));
#75385=CARTESIAN_POINT('Origin',(18.18,40.,7.9));
#75386=CARTESIAN_POINT('Origin',(18.3,38.08,8.));
#75387=CARTESIAN_POINT('',(18.3,38.08,8.));
#75388=CARTESIAN_POINT('',(18.3,37.92,8.));
#75389=CARTESIAN_POINT('',(18.3,54.04,8.));
#75390=CARTESIAN_POINT('',(18.18,38.08,8.));
#75391=CARTESIAN_POINT('',(18.3,38.08,8.));
#75392=CARTESIAN_POINT('',(18.18,37.92,8.));
#75393=CARTESIAN_POINT('',(18.18,37.92,8.));
#75394=CARTESIAN_POINT('',(18.3,37.92,8.));
#75395=CARTESIAN_POINT('Origin',(18.3,38.08,9.4));
#75396=CARTESIAN_POINT('',(18.3,38.08,9.4));
#75397=CARTESIAN_POINT('',(18.3,38.08,7.45));
#75398=CARTESIAN_POINT('',(18.18,38.08,9.4));
#75399=CARTESIAN_POINT('',(18.3,38.08,9.4));
#75400=CARTESIAN_POINT('',(18.18,38.08,8.));
#75401=CARTESIAN_POINT('Origin',(18.3,37.92,9.4));
#75402=CARTESIAN_POINT('',(18.3,37.92,9.4));
#75403=CARTESIAN_POINT('',(18.3,53.96,9.4));
#75404=CARTESIAN_POINT('',(18.18,37.92,9.4));
#75405=CARTESIAN_POINT('',(18.3,37.92,9.4));
#75406=CARTESIAN_POINT('',(18.18,38.08,9.4));
#75407=CARTESIAN_POINT('Origin',(18.3,37.92,8.));
#75408=CARTESIAN_POINT('',(18.3,37.92,6.75));
#75409=CARTESIAN_POINT('',(18.18,37.92,9.4));
#75410=CARTESIAN_POINT('Origin',(18.18,38.,8.7));
#75411=CARTESIAN_POINT('Origin',(18.3,36.08,8.));
#75412=CARTESIAN_POINT('',(18.3,36.08,8.));
#75413=CARTESIAN_POINT('',(18.3,35.92,8.));
#75414=CARTESIAN_POINT('',(18.3,53.04,8.));
#75415=CARTESIAN_POINT('',(18.18,36.08,8.));
#75416=CARTESIAN_POINT('',(18.3,36.08,8.));
#75417=CARTESIAN_POINT('',(18.18,35.92,8.));
#75418=CARTESIAN_POINT('',(18.18,35.92,8.));
#75419=CARTESIAN_POINT('',(18.3,35.92,8.));
#75420=CARTESIAN_POINT('Origin',(18.3,36.08,9.4));
#75421=CARTESIAN_POINT('',(18.3,36.08,9.4));
#75422=CARTESIAN_POINT('',(18.3,36.08,7.45));
#75423=CARTESIAN_POINT('',(18.18,36.08,9.4));
#75424=CARTESIAN_POINT('',(18.3,36.08,9.4));
#75425=CARTESIAN_POINT('',(18.18,36.08,8.));
#75426=CARTESIAN_POINT('Origin',(18.3,35.92,9.4));
#75427=CARTESIAN_POINT('',(18.3,35.92,9.4));
#75428=CARTESIAN_POINT('',(18.3,52.96,9.4));
#75429=CARTESIAN_POINT('',(18.18,35.92,9.4));
#75430=CARTESIAN_POINT('',(18.3,35.92,9.4));
#75431=CARTESIAN_POINT('',(18.18,36.08,9.4));
#75432=CARTESIAN_POINT('Origin',(18.3,35.92,8.));
#75433=CARTESIAN_POINT('',(18.3,35.92,6.75));
#75434=CARTESIAN_POINT('',(18.18,35.92,9.4));
#75435=CARTESIAN_POINT('Origin',(18.18,36.,8.7));
#75436=CARTESIAN_POINT('Origin',(18.3,34.08,8.));
#75437=CARTESIAN_POINT('',(18.3,34.08,8.));
#75438=CARTESIAN_POINT('',(18.3,33.92,8.));
#75439=CARTESIAN_POINT('',(18.3,52.04,8.));
#75440=CARTESIAN_POINT('',(18.18,34.08,8.));
#75441=CARTESIAN_POINT('',(18.3,34.08,8.));
#75442=CARTESIAN_POINT('',(18.18,33.92,8.));
#75443=CARTESIAN_POINT('',(18.18,33.92,8.));
#75444=CARTESIAN_POINT('',(18.3,33.92,8.));
#75445=CARTESIAN_POINT('Origin',(18.3,34.08,9.4));
#75446=CARTESIAN_POINT('',(18.3,34.08,9.4));
#75447=CARTESIAN_POINT('',(18.3,34.08,7.45));
#75448=CARTESIAN_POINT('',(18.18,34.08,9.4));
#75449=CARTESIAN_POINT('',(18.3,34.08,9.4));
#75450=CARTESIAN_POINT('',(18.18,34.08,8.));
#75451=CARTESIAN_POINT('Origin',(18.3,33.92,9.4));
#75452=CARTESIAN_POINT('',(18.3,33.92,9.4));
#75453=CARTESIAN_POINT('',(18.3,51.96,9.4));
#75454=CARTESIAN_POINT('',(18.18,33.92,9.4));
#75455=CARTESIAN_POINT('',(18.3,33.92,9.4));
#75456=CARTESIAN_POINT('',(18.18,34.08,9.4));
#75457=CARTESIAN_POINT('Origin',(18.3,33.92,8.));
#75458=CARTESIAN_POINT('',(18.3,33.92,6.75));
#75459=CARTESIAN_POINT('',(18.18,33.92,9.4));
#75460=CARTESIAN_POINT('Origin',(18.18,34.,8.7));
#75461=CARTESIAN_POINT('Origin',(18.3,32.08,8.));
#75462=CARTESIAN_POINT('',(18.3,32.08,8.));
#75463=CARTESIAN_POINT('',(18.3,31.92,8.));
#75464=CARTESIAN_POINT('',(18.3,51.04,8.));
#75465=CARTESIAN_POINT('',(18.18,32.08,8.));
#75466=CARTESIAN_POINT('',(18.3,32.08,8.));
#75467=CARTESIAN_POINT('',(18.18,31.92,8.));
#75468=CARTESIAN_POINT('',(18.18,31.92,8.));
#75469=CARTESIAN_POINT('',(18.3,31.92,8.));
#75470=CARTESIAN_POINT('Origin',(18.3,32.08,9.4));
#75471=CARTESIAN_POINT('',(18.3,32.08,9.4));
#75472=CARTESIAN_POINT('',(18.3,32.08,7.45));
#75473=CARTESIAN_POINT('',(18.18,32.08,9.4));
#75474=CARTESIAN_POINT('',(18.3,32.08,9.4));
#75475=CARTESIAN_POINT('',(18.18,32.08,8.));
#75476=CARTESIAN_POINT('Origin',(18.3,31.92,9.4));
#75477=CARTESIAN_POINT('',(18.3,31.92,9.4));
#75478=CARTESIAN_POINT('',(18.3,50.96,9.4));
#75479=CARTESIAN_POINT('',(18.18,31.92,9.4));
#75480=CARTESIAN_POINT('',(18.3,31.92,9.4));
#75481=CARTESIAN_POINT('',(18.18,32.08,9.4));
#75482=CARTESIAN_POINT('Origin',(18.3,31.92,8.));
#75483=CARTESIAN_POINT('',(18.3,31.92,6.75));
#75484=CARTESIAN_POINT('',(18.18,31.92,9.4));
#75485=CARTESIAN_POINT('Origin',(18.18,32.,8.7));
#75486=CARTESIAN_POINT('Origin',(18.3,30.08,6.4));
#75487=CARTESIAN_POINT('',(18.3,30.08,6.4));
#75488=CARTESIAN_POINT('',(18.3,29.92,6.4));
#75489=CARTESIAN_POINT('',(18.3,50.04,6.4));
#75490=CARTESIAN_POINT('',(18.18,30.08,6.4));
#75491=CARTESIAN_POINT('',(18.3,30.08,6.4));
#75492=CARTESIAN_POINT('',(18.18,29.92,6.4));
#75493=CARTESIAN_POINT('',(18.18,29.92,6.4));
#75494=CARTESIAN_POINT('',(18.3,29.92,6.4));
#75495=CARTESIAN_POINT('Origin',(18.3,30.08,9.4));
#75496=CARTESIAN_POINT('',(18.3,30.08,9.4));
#75497=CARTESIAN_POINT('',(18.3,30.08,7.45));
#75498=CARTESIAN_POINT('',(18.18,30.08,9.4));
#75499=CARTESIAN_POINT('',(18.3,30.08,9.4));
#75500=CARTESIAN_POINT('',(18.18,30.08,6.4));
#75501=CARTESIAN_POINT('Origin',(18.3,29.92,9.4));
#75502=CARTESIAN_POINT('',(18.3,29.92,9.4));
#75503=CARTESIAN_POINT('',(18.3,49.96,9.4));
#75504=CARTESIAN_POINT('',(18.18,29.92,9.4));
#75505=CARTESIAN_POINT('',(18.3,29.92,9.4));
#75506=CARTESIAN_POINT('',(18.18,30.08,9.4));
#75507=CARTESIAN_POINT('Origin',(18.3,29.92,6.4));
#75508=CARTESIAN_POINT('',(18.3,29.92,5.95));
#75509=CARTESIAN_POINT('',(18.18,29.92,9.4));
#75510=CARTESIAN_POINT('Origin',(18.18,30.,7.9));
#75511=CARTESIAN_POINT('Origin',(18.3,29.08,8.));
#75512=CARTESIAN_POINT('',(18.3,29.08,8.));
#75513=CARTESIAN_POINT('',(18.3,28.92,8.));
#75514=CARTESIAN_POINT('',(18.3,49.54,8.));
#75515=CARTESIAN_POINT('',(18.18,29.08,8.));
#75516=CARTESIAN_POINT('',(18.3,29.08,8.));
#75517=CARTESIAN_POINT('',(18.18,28.92,8.));
#75518=CARTESIAN_POINT('',(18.18,28.92,8.));
#75519=CARTESIAN_POINT('',(18.3,28.92,8.));
#75520=CARTESIAN_POINT('Origin',(18.3,29.08,9.4));
#75521=CARTESIAN_POINT('',(18.3,29.08,9.4));
#75522=CARTESIAN_POINT('',(18.3,29.08,7.45));
#75523=CARTESIAN_POINT('',(18.18,29.08,9.4));
#75524=CARTESIAN_POINT('',(18.3,29.08,9.4));
#75525=CARTESIAN_POINT('',(18.18,29.08,8.));
#75526=CARTESIAN_POINT('Origin',(18.3,28.92,9.4));
#75527=CARTESIAN_POINT('',(18.3,28.92,9.4));
#75528=CARTESIAN_POINT('',(18.3,49.46,9.4));
#75529=CARTESIAN_POINT('',(18.18,28.92,9.4));
#75530=CARTESIAN_POINT('',(18.3,28.92,9.4));
#75531=CARTESIAN_POINT('',(18.18,29.08,9.4));
#75532=CARTESIAN_POINT('Origin',(18.3,28.92,8.));
#75533=CARTESIAN_POINT('',(18.3,28.92,6.75));
#75534=CARTESIAN_POINT('',(18.18,28.92,9.4));
#75535=CARTESIAN_POINT('Origin',(18.18,29.,8.7));
#75536=CARTESIAN_POINT('Origin',(18.3,31.08,8.));
#75537=CARTESIAN_POINT('',(18.3,31.08,8.));
#75538=CARTESIAN_POINT('',(18.3,30.92,8.));
#75539=CARTESIAN_POINT('',(18.3,50.54,8.));
#75540=CARTESIAN_POINT('',(18.18,31.08,8.));
#75541=CARTESIAN_POINT('',(18.3,31.08,8.));
#75542=CARTESIAN_POINT('',(18.18,30.92,8.));
#75543=CARTESIAN_POINT('',(18.18,30.92,8.));
#75544=CARTESIAN_POINT('',(18.3,30.92,8.));
#75545=CARTESIAN_POINT('Origin',(18.3,31.08,9.4));
#75546=CARTESIAN_POINT('',(18.3,31.08,9.4));
#75547=CARTESIAN_POINT('',(18.3,31.08,7.45));
#75548=CARTESIAN_POINT('',(18.18,31.08,9.4));
#75549=CARTESIAN_POINT('',(18.3,31.08,9.4));
#75550=CARTESIAN_POINT('',(18.18,31.08,8.));
#75551=CARTESIAN_POINT('Origin',(18.3,30.92,9.4));
#75552=CARTESIAN_POINT('',(18.3,30.92,9.4));
#75553=CARTESIAN_POINT('',(18.3,50.46,9.4));
#75554=CARTESIAN_POINT('',(18.18,30.92,9.4));
#75555=CARTESIAN_POINT('',(18.3,30.92,9.4));
#75556=CARTESIAN_POINT('',(18.18,31.08,9.4));
#75557=CARTESIAN_POINT('Origin',(18.3,30.92,8.));
#75558=CARTESIAN_POINT('',(18.3,30.92,6.75));
#75559=CARTESIAN_POINT('',(18.18,30.92,9.4));
#75560=CARTESIAN_POINT('Origin',(18.18,31.,8.7));
#75561=CARTESIAN_POINT('Origin',(18.3,33.08,8.));
#75562=CARTESIAN_POINT('',(18.3,33.08,8.));
#75563=CARTESIAN_POINT('',(18.3,32.92,8.));
#75564=CARTESIAN_POINT('',(18.3,51.54,8.));
#75565=CARTESIAN_POINT('',(18.18,33.08,8.));
#75566=CARTESIAN_POINT('',(18.3,33.08,8.));
#75567=CARTESIAN_POINT('',(18.18,32.92,8.));
#75568=CARTESIAN_POINT('',(18.18,32.92,8.));
#75569=CARTESIAN_POINT('',(18.3,32.92,8.));
#75570=CARTESIAN_POINT('Origin',(18.3,33.08,9.4));
#75571=CARTESIAN_POINT('',(18.3,33.08,9.4));
#75572=CARTESIAN_POINT('',(18.3,33.08,7.45));
#75573=CARTESIAN_POINT('',(18.18,33.08,9.4));
#75574=CARTESIAN_POINT('',(18.3,33.08,9.4));
#75575=CARTESIAN_POINT('',(18.18,33.08,8.));
#75576=CARTESIAN_POINT('Origin',(18.3,32.92,9.4));
#75577=CARTESIAN_POINT('',(18.3,32.92,9.4));
#75578=CARTESIAN_POINT('',(18.3,51.46,9.4));
#75579=CARTESIAN_POINT('',(18.18,32.92,9.4));
#75580=CARTESIAN_POINT('',(18.3,32.92,9.4));
#75581=CARTESIAN_POINT('',(18.18,33.08,9.4));
#75582=CARTESIAN_POINT('Origin',(18.3,32.92,8.));
#75583=CARTESIAN_POINT('',(18.3,32.92,6.75));
#75584=CARTESIAN_POINT('',(18.18,32.92,9.4));
#75585=CARTESIAN_POINT('Origin',(18.18,33.,8.7));
#75586=CARTESIAN_POINT('Origin',(18.3,35.08,7.2));
#75587=CARTESIAN_POINT('',(18.3,35.08,7.2));
#75588=CARTESIAN_POINT('',(18.3,34.92,7.2));
#75589=CARTESIAN_POINT('',(18.3,52.54,7.2));
#75590=CARTESIAN_POINT('',(18.18,35.08,7.2));
#75591=CARTESIAN_POINT('',(18.3,35.08,7.2));
#75592=CARTESIAN_POINT('',(18.18,34.92,7.2));
#75593=CARTESIAN_POINT('',(18.18,34.92,7.2));
#75594=CARTESIAN_POINT('',(18.3,34.92,7.2));
#75595=CARTESIAN_POINT('Origin',(18.3,35.08,9.4));
#75596=CARTESIAN_POINT('',(18.3,35.08,9.4));
#75597=CARTESIAN_POINT('',(18.3,35.08,7.45));
#75598=CARTESIAN_POINT('',(18.18,35.08,9.4));
#75599=CARTESIAN_POINT('',(18.3,35.08,9.4));
#75600=CARTESIAN_POINT('',(18.18,35.08,7.2));
#75601=CARTESIAN_POINT('Origin',(18.3,34.92,9.4));
#75602=CARTESIAN_POINT('',(18.3,34.92,9.4));
#75603=CARTESIAN_POINT('',(18.3,52.46,9.4));
#75604=CARTESIAN_POINT('',(18.18,34.92,9.4));
#75605=CARTESIAN_POINT('',(18.3,34.92,9.4));
#75606=CARTESIAN_POINT('',(18.18,35.08,9.4));
#75607=CARTESIAN_POINT('Origin',(18.3,34.92,7.2));
#75608=CARTESIAN_POINT('',(18.3,34.92,6.35));
#75609=CARTESIAN_POINT('',(18.18,34.92,9.4));
#75610=CARTESIAN_POINT('Origin',(18.18,35.,8.3));
#75611=CARTESIAN_POINT('Origin',(18.3,37.08,8.));
#75612=CARTESIAN_POINT('',(18.3,37.08,8.));
#75613=CARTESIAN_POINT('',(18.3,36.92,8.));
#75614=CARTESIAN_POINT('',(18.3,53.54,8.));
#75615=CARTESIAN_POINT('',(18.18,37.08,8.));
#75616=CARTESIAN_POINT('',(18.3,37.08,8.));
#75617=CARTESIAN_POINT('',(18.18,36.92,8.));
#75618=CARTESIAN_POINT('',(18.18,36.92,8.));
#75619=CARTESIAN_POINT('',(18.3,36.92,8.));
#75620=CARTESIAN_POINT('Origin',(18.3,37.08,9.4));
#75621=CARTESIAN_POINT('',(18.3,37.08,9.4));
#75622=CARTESIAN_POINT('',(18.3,37.08,7.45));
#75623=CARTESIAN_POINT('',(18.18,37.08,9.4));
#75624=CARTESIAN_POINT('',(18.3,37.08,9.4));
#75625=CARTESIAN_POINT('',(18.18,37.08,8.));
#75626=CARTESIAN_POINT('Origin',(18.3,36.92,9.4));
#75627=CARTESIAN_POINT('',(18.3,36.92,9.4));
#75628=CARTESIAN_POINT('',(18.3,53.46,9.4));
#75629=CARTESIAN_POINT('',(18.18,36.92,9.4));
#75630=CARTESIAN_POINT('',(18.3,36.92,9.4));
#75631=CARTESIAN_POINT('',(18.18,37.08,9.4));
#75632=CARTESIAN_POINT('Origin',(18.3,36.92,8.));
#75633=CARTESIAN_POINT('',(18.3,36.92,6.75));
#75634=CARTESIAN_POINT('',(18.18,36.92,9.4));
#75635=CARTESIAN_POINT('Origin',(18.18,37.,8.7));
#75636=CARTESIAN_POINT('Origin',(18.3,39.08,8.));
#75637=CARTESIAN_POINT('',(18.3,39.08,8.));
#75638=CARTESIAN_POINT('',(18.3,38.92,8.));
#75639=CARTESIAN_POINT('',(18.3,54.54,8.));
#75640=CARTESIAN_POINT('',(18.18,39.08,8.));
#75641=CARTESIAN_POINT('',(18.3,39.08,8.));
#75642=CARTESIAN_POINT('',(18.18,38.92,8.));
#75643=CARTESIAN_POINT('',(18.18,38.92,8.));
#75644=CARTESIAN_POINT('',(18.3,38.92,8.));
#75645=CARTESIAN_POINT('Origin',(18.3,39.08,9.4));
#75646=CARTESIAN_POINT('',(18.3,39.08,9.4));
#75647=CARTESIAN_POINT('',(18.3,39.08,7.45));
#75648=CARTESIAN_POINT('',(18.18,39.08,9.4));
#75649=CARTESIAN_POINT('',(18.3,39.08,9.4));
#75650=CARTESIAN_POINT('',(18.18,39.08,8.));
#75651=CARTESIAN_POINT('Origin',(18.3,38.92,9.4));
#75652=CARTESIAN_POINT('',(18.3,38.92,9.4));
#75653=CARTESIAN_POINT('',(18.3,54.46,9.4));
#75654=CARTESIAN_POINT('',(18.18,38.92,9.4));
#75655=CARTESIAN_POINT('',(18.3,38.92,9.4));
#75656=CARTESIAN_POINT('',(18.18,39.08,9.4));
#75657=CARTESIAN_POINT('Origin',(18.3,38.92,8.));
#75658=CARTESIAN_POINT('',(18.3,38.92,6.75));
#75659=CARTESIAN_POINT('',(18.18,38.92,9.4));
#75660=CARTESIAN_POINT('Origin',(18.18,39.,8.7));
#75661=CARTESIAN_POINT('Origin',(18.3,41.08,8.));
#75662=CARTESIAN_POINT('',(18.3,41.08,8.));
#75663=CARTESIAN_POINT('',(18.3,40.92,8.));
#75664=CARTESIAN_POINT('',(18.3,55.54,8.));
#75665=CARTESIAN_POINT('',(18.18,41.08,8.));
#75666=CARTESIAN_POINT('',(18.3,41.08,8.));
#75667=CARTESIAN_POINT('',(18.18,40.92,8.));
#75668=CARTESIAN_POINT('',(18.18,40.92,8.));
#75669=CARTESIAN_POINT('',(18.3,40.92,8.));
#75670=CARTESIAN_POINT('Origin',(18.3,41.08,9.4));
#75671=CARTESIAN_POINT('',(18.3,41.08,9.4));
#75672=CARTESIAN_POINT('',(18.3,41.08,7.45));
#75673=CARTESIAN_POINT('',(18.18,41.08,9.4));
#75674=CARTESIAN_POINT('',(18.3,41.08,9.4));
#75675=CARTESIAN_POINT('',(18.18,41.08,8.));
#75676=CARTESIAN_POINT('Origin',(18.3,40.92,9.4));
#75677=CARTESIAN_POINT('',(18.3,40.92,9.4));
#75678=CARTESIAN_POINT('',(18.3,55.46,9.4));
#75679=CARTESIAN_POINT('',(18.18,40.92,9.4));
#75680=CARTESIAN_POINT('',(18.3,40.92,9.4));
#75681=CARTESIAN_POINT('',(18.18,41.08,9.4));
#75682=CARTESIAN_POINT('Origin',(18.3,40.92,8.));
#75683=CARTESIAN_POINT('',(18.3,40.92,6.75));
#75684=CARTESIAN_POINT('',(18.18,40.92,9.4));
#75685=CARTESIAN_POINT('Origin',(18.18,41.,8.7));
#75686=CARTESIAN_POINT('Origin',(18.3,43.08,8.));
#75687=CARTESIAN_POINT('',(18.3,43.08,8.));
#75688=CARTESIAN_POINT('',(18.3,42.92,8.));
#75689=CARTESIAN_POINT('',(18.3,56.54,8.));
#75690=CARTESIAN_POINT('',(18.18,43.08,8.));
#75691=CARTESIAN_POINT('',(18.3,43.08,8.));
#75692=CARTESIAN_POINT('',(18.18,42.92,8.));
#75693=CARTESIAN_POINT('',(18.18,42.92,8.));
#75694=CARTESIAN_POINT('',(18.3,42.92,8.));
#75695=CARTESIAN_POINT('Origin',(18.3,43.08,9.4));
#75696=CARTESIAN_POINT('',(18.3,43.08,9.4));
#75697=CARTESIAN_POINT('',(18.3,43.08,7.45));
#75698=CARTESIAN_POINT('',(18.18,43.08,9.4));
#75699=CARTESIAN_POINT('',(18.3,43.08,9.4));
#75700=CARTESIAN_POINT('',(18.18,43.08,8.));
#75701=CARTESIAN_POINT('Origin',(18.3,42.92,9.4));
#75702=CARTESIAN_POINT('',(18.3,42.92,9.4));
#75703=CARTESIAN_POINT('',(18.3,56.46,9.4));
#75704=CARTESIAN_POINT('',(18.18,42.92,9.4));
#75705=CARTESIAN_POINT('',(18.3,42.92,9.4));
#75706=CARTESIAN_POINT('',(18.18,43.08,9.4));
#75707=CARTESIAN_POINT('Origin',(18.3,42.92,8.));
#75708=CARTESIAN_POINT('',(18.3,42.92,6.75));
#75709=CARTESIAN_POINT('',(18.18,42.92,9.4));
#75710=CARTESIAN_POINT('Origin',(18.18,43.,8.7));
#75711=CARTESIAN_POINT('Origin',(18.3,45.08,7.2));
#75712=CARTESIAN_POINT('',(18.3,45.08,7.2));
#75713=CARTESIAN_POINT('',(18.3,44.92,7.2));
#75714=CARTESIAN_POINT('',(18.3,57.54,7.2));
#75715=CARTESIAN_POINT('',(18.18,45.08,7.2));
#75716=CARTESIAN_POINT('',(18.3,45.08,7.2));
#75717=CARTESIAN_POINT('',(18.18,44.92,7.2));
#75718=CARTESIAN_POINT('',(18.18,44.92,7.2));
#75719=CARTESIAN_POINT('',(18.3,44.92,7.2));
#75720=CARTESIAN_POINT('Origin',(18.3,45.08,9.4));
#75721=CARTESIAN_POINT('',(18.3,45.08,9.4));
#75722=CARTESIAN_POINT('',(18.3,45.08,7.45));
#75723=CARTESIAN_POINT('',(18.18,45.08,9.4));
#75724=CARTESIAN_POINT('',(18.3,45.08,9.4));
#75725=CARTESIAN_POINT('',(18.18,45.08,7.2));
#75726=CARTESIAN_POINT('Origin',(18.3,44.92,9.4));
#75727=CARTESIAN_POINT('',(18.3,44.92,9.4));
#75728=CARTESIAN_POINT('',(18.3,57.46,9.4));
#75729=CARTESIAN_POINT('',(18.18,44.92,9.4));
#75730=CARTESIAN_POINT('',(18.3,44.92,9.4));
#75731=CARTESIAN_POINT('',(18.18,45.08,9.4));
#75732=CARTESIAN_POINT('Origin',(18.3,44.92,7.2));
#75733=CARTESIAN_POINT('',(18.3,44.92,6.35));
#75734=CARTESIAN_POINT('',(18.18,44.92,9.4));
#75735=CARTESIAN_POINT('Origin',(18.18,45.,8.3));
#75736=CARTESIAN_POINT('Origin',(18.3,47.08,8.));
#75737=CARTESIAN_POINT('',(18.3,47.08,8.));
#75738=CARTESIAN_POINT('',(18.3,46.92,8.));
#75739=CARTESIAN_POINT('',(18.3,58.54,8.));
#75740=CARTESIAN_POINT('',(18.18,47.08,8.));
#75741=CARTESIAN_POINT('',(18.3,47.08,8.));
#75742=CARTESIAN_POINT('',(18.18,46.92,8.));
#75743=CARTESIAN_POINT('',(18.18,46.92,8.));
#75744=CARTESIAN_POINT('',(18.3,46.92,8.));
#75745=CARTESIAN_POINT('Origin',(18.3,47.08,9.4));
#75746=CARTESIAN_POINT('',(18.3,47.08,9.4));
#75747=CARTESIAN_POINT('',(18.3,47.08,7.45));
#75748=CARTESIAN_POINT('',(18.18,47.08,9.4));
#75749=CARTESIAN_POINT('',(18.3,47.08,9.4));
#75750=CARTESIAN_POINT('',(18.18,47.08,8.));
#75751=CARTESIAN_POINT('Origin',(18.3,46.92,9.4));
#75752=CARTESIAN_POINT('',(18.3,46.92,9.4));
#75753=CARTESIAN_POINT('',(18.3,58.46,9.4));
#75754=CARTESIAN_POINT('',(18.18,46.92,9.4));
#75755=CARTESIAN_POINT('',(18.3,46.92,9.4));
#75756=CARTESIAN_POINT('',(18.18,47.08,9.4));
#75757=CARTESIAN_POINT('Origin',(18.3,46.92,8.));
#75758=CARTESIAN_POINT('',(18.3,46.92,6.75));
#75759=CARTESIAN_POINT('',(18.18,46.92,9.4));
#75760=CARTESIAN_POINT('Origin',(18.18,47.,8.7));
#75761=CARTESIAN_POINT('Origin',(18.3,49.08,8.));
#75762=CARTESIAN_POINT('',(18.3,49.08,8.));
#75763=CARTESIAN_POINT('',(18.3,48.92,8.));
#75764=CARTESIAN_POINT('',(18.3,59.54,8.));
#75765=CARTESIAN_POINT('',(18.18,49.08,8.));
#75766=CARTESIAN_POINT('',(18.3,49.08,8.));
#75767=CARTESIAN_POINT('',(18.18,48.92,8.));
#75768=CARTESIAN_POINT('',(18.18,48.92,8.));
#75769=CARTESIAN_POINT('',(18.3,48.92,8.));
#75770=CARTESIAN_POINT('Origin',(18.3,49.08,9.4));
#75771=CARTESIAN_POINT('',(18.3,49.08,9.4));
#75772=CARTESIAN_POINT('',(18.3,49.08,7.45));
#75773=CARTESIAN_POINT('',(18.18,49.08,9.4));
#75774=CARTESIAN_POINT('',(18.3,49.08,9.4));
#75775=CARTESIAN_POINT('',(18.18,49.08,8.));
#75776=CARTESIAN_POINT('Origin',(18.3,48.92,9.4));
#75777=CARTESIAN_POINT('',(18.3,48.92,9.4));
#75778=CARTESIAN_POINT('',(18.3,59.46,9.4));
#75779=CARTESIAN_POINT('',(18.18,48.92,9.4));
#75780=CARTESIAN_POINT('',(18.3,48.92,9.4));
#75781=CARTESIAN_POINT('',(18.18,49.08,9.4));
#75782=CARTESIAN_POINT('Origin',(18.3,48.92,8.));
#75783=CARTESIAN_POINT('',(18.3,48.92,6.75));
#75784=CARTESIAN_POINT('',(18.18,48.92,9.4));
#75785=CARTESIAN_POINT('Origin',(18.18,49.,8.7));
#75786=CARTESIAN_POINT('Origin',(18.3,51.08,8.));
#75787=CARTESIAN_POINT('',(18.3,51.08,8.));
#75788=CARTESIAN_POINT('',(18.3,50.92,8.));
#75789=CARTESIAN_POINT('',(18.3,60.54,8.));
#75790=CARTESIAN_POINT('',(18.18,51.08,8.));
#75791=CARTESIAN_POINT('',(18.3,51.08,8.));
#75792=CARTESIAN_POINT('',(18.18,50.92,8.));
#75793=CARTESIAN_POINT('',(18.18,50.92,8.));
#75794=CARTESIAN_POINT('',(18.3,50.92,8.));
#75795=CARTESIAN_POINT('Origin',(18.3,51.08,9.4));
#75796=CARTESIAN_POINT('',(18.3,51.08,9.4));
#75797=CARTESIAN_POINT('',(18.3,51.08,7.45));
#75798=CARTESIAN_POINT('',(18.18,51.08,9.4));
#75799=CARTESIAN_POINT('',(18.3,51.08,9.4));
#75800=CARTESIAN_POINT('',(18.18,51.08,8.));
#75801=CARTESIAN_POINT('Origin',(18.3,50.92,9.4));
#75802=CARTESIAN_POINT('',(18.3,50.92,9.4));
#75803=CARTESIAN_POINT('',(18.3,60.46,9.4));
#75804=CARTESIAN_POINT('',(18.18,50.92,9.4));
#75805=CARTESIAN_POINT('',(18.3,50.92,9.4));
#75806=CARTESIAN_POINT('',(18.18,51.08,9.4));
#75807=CARTESIAN_POINT('Origin',(18.3,50.92,8.));
#75808=CARTESIAN_POINT('',(18.3,50.92,6.75));
#75809=CARTESIAN_POINT('',(18.18,50.92,9.4));
#75810=CARTESIAN_POINT('Origin',(18.18,51.,8.7));
#75811=CARTESIAN_POINT('Origin',(18.3,53.08,8.));
#75812=CARTESIAN_POINT('',(18.3,53.08,8.));
#75813=CARTESIAN_POINT('',(18.3,52.92,8.));
#75814=CARTESIAN_POINT('',(18.3,61.54,8.));
#75815=CARTESIAN_POINT('',(18.18,53.08,8.));
#75816=CARTESIAN_POINT('',(18.3,53.08,8.));
#75817=CARTESIAN_POINT('',(18.18,52.92,8.));
#75818=CARTESIAN_POINT('',(18.18,52.92,8.));
#75819=CARTESIAN_POINT('',(18.3,52.92,8.));
#75820=CARTESIAN_POINT('Origin',(18.3,53.08,9.4));
#75821=CARTESIAN_POINT('',(18.3,53.08,9.4));
#75822=CARTESIAN_POINT('',(18.3,53.08,7.45));
#75823=CARTESIAN_POINT('',(18.18,53.08,9.4));
#75824=CARTESIAN_POINT('',(18.3,53.08,9.4));
#75825=CARTESIAN_POINT('',(18.18,53.08,8.));
#75826=CARTESIAN_POINT('Origin',(18.3,52.92,9.4));
#75827=CARTESIAN_POINT('',(18.3,52.92,9.4));
#75828=CARTESIAN_POINT('',(18.3,61.46,9.4));
#75829=CARTESIAN_POINT('',(18.18,52.92,9.4));
#75830=CARTESIAN_POINT('',(18.3,52.92,9.4));
#75831=CARTESIAN_POINT('',(18.18,53.08,9.4));
#75832=CARTESIAN_POINT('Origin',(18.3,52.92,8.));
#75833=CARTESIAN_POINT('',(18.3,52.92,6.75));
#75834=CARTESIAN_POINT('',(18.18,52.92,9.4));
#75835=CARTESIAN_POINT('Origin',(18.18,53.,8.7));
#75836=CARTESIAN_POINT('Origin',(18.3,55.08,7.2));
#75837=CARTESIAN_POINT('',(18.3,55.08,7.2));
#75838=CARTESIAN_POINT('',(18.3,54.92,7.2));
#75839=CARTESIAN_POINT('',(18.3,62.54,7.2));
#75840=CARTESIAN_POINT('',(18.18,55.08,7.2));
#75841=CARTESIAN_POINT('',(18.3,55.08,7.2));
#75842=CARTESIAN_POINT('',(18.18,54.92,7.2));
#75843=CARTESIAN_POINT('',(18.18,54.92,7.2));
#75844=CARTESIAN_POINT('',(18.3,54.92,7.2));
#75845=CARTESIAN_POINT('Origin',(18.3,55.08,9.4));
#75846=CARTESIAN_POINT('',(18.3,55.08,9.4));
#75847=CARTESIAN_POINT('',(18.3,55.08,7.45));
#75848=CARTESIAN_POINT('',(18.18,55.08,9.4));
#75849=CARTESIAN_POINT('',(18.3,55.08,9.4));
#75850=CARTESIAN_POINT('',(18.18,55.08,7.2));
#75851=CARTESIAN_POINT('Origin',(18.3,54.92,9.4));
#75852=CARTESIAN_POINT('',(18.3,54.92,9.4));
#75853=CARTESIAN_POINT('',(18.3,62.46,9.4));
#75854=CARTESIAN_POINT('',(18.18,54.92,9.4));
#75855=CARTESIAN_POINT('',(18.3,54.92,9.4));
#75856=CARTESIAN_POINT('',(18.18,55.08,9.4));
#75857=CARTESIAN_POINT('Origin',(18.3,54.92,7.2));
#75858=CARTESIAN_POINT('',(18.3,54.92,6.35));
#75859=CARTESIAN_POINT('',(18.18,54.92,9.4));
#75860=CARTESIAN_POINT('Origin',(18.18,55.,8.3));
#75861=CARTESIAN_POINT('Origin',(18.3,57.08,8.));
#75862=CARTESIAN_POINT('',(18.3,57.08,8.));
#75863=CARTESIAN_POINT('',(18.3,56.92,8.));
#75864=CARTESIAN_POINT('',(18.3,63.54,8.));
#75865=CARTESIAN_POINT('',(18.18,57.08,8.));
#75866=CARTESIAN_POINT('',(18.3,57.08,8.));
#75867=CARTESIAN_POINT('',(18.18,56.92,8.));
#75868=CARTESIAN_POINT('',(18.18,56.92,8.));
#75869=CARTESIAN_POINT('',(18.3,56.92,8.));
#75870=CARTESIAN_POINT('Origin',(18.3,57.08,9.4));
#75871=CARTESIAN_POINT('',(18.3,57.08,9.4));
#75872=CARTESIAN_POINT('',(18.3,57.08,7.45));
#75873=CARTESIAN_POINT('',(18.18,57.08,9.4));
#75874=CARTESIAN_POINT('',(18.3,57.08,9.4));
#75875=CARTESIAN_POINT('',(18.18,57.08,8.));
#75876=CARTESIAN_POINT('Origin',(18.3,56.92,9.4));
#75877=CARTESIAN_POINT('',(18.3,56.92,9.4));
#75878=CARTESIAN_POINT('',(18.3,63.46,9.4));
#75879=CARTESIAN_POINT('',(18.18,56.92,9.4));
#75880=CARTESIAN_POINT('',(18.3,56.92,9.4));
#75881=CARTESIAN_POINT('',(18.18,57.08,9.4));
#75882=CARTESIAN_POINT('Origin',(18.3,56.92,8.));
#75883=CARTESIAN_POINT('',(18.3,56.92,6.75));
#75884=CARTESIAN_POINT('',(18.18,56.92,9.4));
#75885=CARTESIAN_POINT('Origin',(18.18,57.,8.7));
#75886=CARTESIAN_POINT('Origin',(18.3,59.08,8.));
#75887=CARTESIAN_POINT('',(18.3,59.08,8.));
#75888=CARTESIAN_POINT('',(18.3,58.92,8.));
#75889=CARTESIAN_POINT('',(18.3,64.54,8.));
#75890=CARTESIAN_POINT('',(18.18,59.08,8.));
#75891=CARTESIAN_POINT('',(18.3,59.08,8.));
#75892=CARTESIAN_POINT('',(18.18,58.92,8.));
#75893=CARTESIAN_POINT('',(18.18,58.92,8.));
#75894=CARTESIAN_POINT('',(18.3,58.92,8.));
#75895=CARTESIAN_POINT('Origin',(18.3,59.08,9.4));
#75896=CARTESIAN_POINT('',(18.3,59.08,9.4));
#75897=CARTESIAN_POINT('',(18.3,59.08,7.45));
#75898=CARTESIAN_POINT('',(18.18,59.08,9.4));
#75899=CARTESIAN_POINT('',(18.3,59.08,9.4));
#75900=CARTESIAN_POINT('',(18.18,59.08,8.));
#75901=CARTESIAN_POINT('Origin',(18.3,58.92,9.4));
#75902=CARTESIAN_POINT('',(18.3,58.92,9.4));
#75903=CARTESIAN_POINT('',(18.3,64.46,9.4));
#75904=CARTESIAN_POINT('',(18.18,58.92,9.4));
#75905=CARTESIAN_POINT('',(18.3,58.92,9.4));
#75906=CARTESIAN_POINT('',(18.18,59.08,9.4));
#75907=CARTESIAN_POINT('Origin',(18.3,58.92,8.));
#75908=CARTESIAN_POINT('',(18.3,58.92,6.75));
#75909=CARTESIAN_POINT('',(18.18,58.92,9.4));
#75910=CARTESIAN_POINT('Origin',(18.18,59.,8.7));
#75911=CARTESIAN_POINT('Origin',(18.3,61.08,8.));
#75912=CARTESIAN_POINT('',(18.3,61.08,8.));
#75913=CARTESIAN_POINT('',(18.3,60.92,8.));
#75914=CARTESIAN_POINT('',(18.3,65.54,8.));
#75915=CARTESIAN_POINT('',(18.18,61.08,8.));
#75916=CARTESIAN_POINT('',(18.3,61.08,8.));
#75917=CARTESIAN_POINT('',(18.18,60.92,8.));
#75918=CARTESIAN_POINT('',(18.18,60.92,8.));
#75919=CARTESIAN_POINT('',(18.3,60.92,8.));
#75920=CARTESIAN_POINT('Origin',(18.3,61.08,9.4));
#75921=CARTESIAN_POINT('',(18.3,61.08,9.4));
#75922=CARTESIAN_POINT('',(18.3,61.08,7.45));
#75923=CARTESIAN_POINT('',(18.18,61.08,9.4));
#75924=CARTESIAN_POINT('',(18.3,61.08,9.4));
#75925=CARTESIAN_POINT('',(18.18,61.08,8.));
#75926=CARTESIAN_POINT('Origin',(18.3,60.92,9.4));
#75927=CARTESIAN_POINT('',(18.3,60.92,9.4));
#75928=CARTESIAN_POINT('',(18.3,65.46,9.4));
#75929=CARTESIAN_POINT('',(18.18,60.92,9.4));
#75930=CARTESIAN_POINT('',(18.3,60.92,9.4));
#75931=CARTESIAN_POINT('',(18.18,61.08,9.4));
#75932=CARTESIAN_POINT('Origin',(18.3,60.92,8.));
#75933=CARTESIAN_POINT('',(18.3,60.92,6.75));
#75934=CARTESIAN_POINT('',(18.18,60.92,9.4));
#75935=CARTESIAN_POINT('Origin',(18.18,61.,8.7));
#75936=CARTESIAN_POINT('Origin',(18.3,63.08,8.));
#75937=CARTESIAN_POINT('',(18.3,63.08,8.));
#75938=CARTESIAN_POINT('',(18.3,62.92,8.));
#75939=CARTESIAN_POINT('',(18.3,66.54,8.));
#75940=CARTESIAN_POINT('',(18.18,63.08,8.));
#75941=CARTESIAN_POINT('',(18.3,63.08,8.));
#75942=CARTESIAN_POINT('',(18.18,62.92,8.));
#75943=CARTESIAN_POINT('',(18.18,62.92,8.));
#75944=CARTESIAN_POINT('',(18.3,62.92,8.));
#75945=CARTESIAN_POINT('Origin',(18.3,63.08,9.4));
#75946=CARTESIAN_POINT('',(18.3,63.08,9.4));
#75947=CARTESIAN_POINT('',(18.3,63.08,7.45));
#75948=CARTESIAN_POINT('',(18.18,63.08,9.4));
#75949=CARTESIAN_POINT('',(18.3,63.08,9.4));
#75950=CARTESIAN_POINT('',(18.18,63.08,8.));
#75951=CARTESIAN_POINT('Origin',(18.3,62.92,9.4));
#75952=CARTESIAN_POINT('',(18.3,62.92,9.4));
#75953=CARTESIAN_POINT('',(18.3,66.46,9.4));
#75954=CARTESIAN_POINT('',(18.18,62.92,9.4));
#75955=CARTESIAN_POINT('',(18.3,62.92,9.4));
#75956=CARTESIAN_POINT('',(18.18,63.08,9.4));
#75957=CARTESIAN_POINT('Origin',(18.3,62.92,8.));
#75958=CARTESIAN_POINT('',(18.3,62.92,6.75));
#75959=CARTESIAN_POINT('',(18.18,62.92,9.4));
#75960=CARTESIAN_POINT('Origin',(18.18,63.,8.7));
#75961=CARTESIAN_POINT('Origin',(18.3,65.08,7.2));
#75962=CARTESIAN_POINT('',(18.3,65.08,7.2));
#75963=CARTESIAN_POINT('',(18.3,64.92,7.2));
#75964=CARTESIAN_POINT('',(18.3,67.54,7.2));
#75965=CARTESIAN_POINT('',(18.18,65.08,7.2));
#75966=CARTESIAN_POINT('',(18.3,65.08,7.2));
#75967=CARTESIAN_POINT('',(18.18,64.92,7.2));
#75968=CARTESIAN_POINT('',(18.18,64.92,7.2));
#75969=CARTESIAN_POINT('',(18.3,64.92,7.2));
#75970=CARTESIAN_POINT('Origin',(18.3,65.08,9.4));
#75971=CARTESIAN_POINT('',(18.3,65.08,9.4));
#75972=CARTESIAN_POINT('',(18.3,65.08,7.45));
#75973=CARTESIAN_POINT('',(18.18,65.08,9.4));
#75974=CARTESIAN_POINT('',(18.3,65.08,9.4));
#75975=CARTESIAN_POINT('',(18.18,65.08,7.2));
#75976=CARTESIAN_POINT('Origin',(18.3,64.92,9.4));
#75977=CARTESIAN_POINT('',(18.3,64.92,9.4));
#75978=CARTESIAN_POINT('',(18.3,67.46,9.4));
#75979=CARTESIAN_POINT('',(18.18,64.92,9.4));
#75980=CARTESIAN_POINT('',(18.3,64.92,9.4));
#75981=CARTESIAN_POINT('',(18.18,65.08,9.4));
#75982=CARTESIAN_POINT('Origin',(18.3,64.92,7.2));
#75983=CARTESIAN_POINT('',(18.3,64.92,6.35));
#75984=CARTESIAN_POINT('',(18.18,64.92,9.4));
#75985=CARTESIAN_POINT('Origin',(18.18,65.,8.3));
#75986=CARTESIAN_POINT('Origin',(18.3,67.08,8.));
#75987=CARTESIAN_POINT('',(18.3,67.08,8.));
#75988=CARTESIAN_POINT('',(18.3,66.92,8.));
#75989=CARTESIAN_POINT('',(18.3,68.54,8.));
#75990=CARTESIAN_POINT('',(18.18,67.08,8.));
#75991=CARTESIAN_POINT('',(18.3,67.08,8.));
#75992=CARTESIAN_POINT('',(18.18,66.92,8.));
#75993=CARTESIAN_POINT('',(18.18,66.92,8.));
#75994=CARTESIAN_POINT('',(18.3,66.92,8.));
#75995=CARTESIAN_POINT('Origin',(18.3,67.08,9.4));
#75996=CARTESIAN_POINT('',(18.3,67.08,9.4));
#75997=CARTESIAN_POINT('',(18.3,67.08,7.45));
#75998=CARTESIAN_POINT('',(18.18,67.08,9.4));
#75999=CARTESIAN_POINT('',(18.3,67.08,9.4));
#76000=CARTESIAN_POINT('',(18.18,67.08,8.));
#76001=CARTESIAN_POINT('Origin',(18.3,66.92,9.4));
#76002=CARTESIAN_POINT('',(18.3,66.92,9.4));
#76003=CARTESIAN_POINT('',(18.3,68.46,9.4));
#76004=CARTESIAN_POINT('',(18.18,66.92,9.4));
#76005=CARTESIAN_POINT('',(18.3,66.92,9.4));
#76006=CARTESIAN_POINT('',(18.18,67.08,9.4));
#76007=CARTESIAN_POINT('Origin',(18.3,66.92,8.));
#76008=CARTESIAN_POINT('',(18.3,66.92,6.75));
#76009=CARTESIAN_POINT('',(18.18,66.92,9.4));
#76010=CARTESIAN_POINT('Origin',(18.18,67.,8.7));
#76011=CARTESIAN_POINT('Origin',(18.3,69.08,8.));
#76012=CARTESIAN_POINT('',(18.3,69.08,8.));
#76013=CARTESIAN_POINT('',(18.3,68.92,8.));
#76014=CARTESIAN_POINT('',(18.3,69.54,8.));
#76015=CARTESIAN_POINT('',(18.18,69.08,8.));
#76016=CARTESIAN_POINT('',(18.3,69.08,8.));
#76017=CARTESIAN_POINT('',(18.18,68.92,8.));
#76018=CARTESIAN_POINT('',(18.18,68.92,8.));
#76019=CARTESIAN_POINT('',(18.3,68.92,8.));
#76020=CARTESIAN_POINT('Origin',(18.3,69.08,9.4));
#76021=CARTESIAN_POINT('',(18.3,69.08,9.4));
#76022=CARTESIAN_POINT('',(18.3,69.08,7.45));
#76023=CARTESIAN_POINT('',(18.18,69.08,9.4));
#76024=CARTESIAN_POINT('',(18.3,69.08,9.4));
#76025=CARTESIAN_POINT('',(18.18,69.08,8.));
#76026=CARTESIAN_POINT('Origin',(18.3,68.92,9.4));
#76027=CARTESIAN_POINT('',(18.3,68.92,9.4));
#76028=CARTESIAN_POINT('',(18.3,69.46,9.4));
#76029=CARTESIAN_POINT('',(18.18,68.92,9.4));
#76030=CARTESIAN_POINT('',(18.3,68.92,9.4));
#76031=CARTESIAN_POINT('',(18.18,69.08,9.4));
#76032=CARTESIAN_POINT('Origin',(18.3,68.92,8.));
#76033=CARTESIAN_POINT('',(18.3,68.92,6.75));
#76034=CARTESIAN_POINT('',(18.18,68.92,9.4));
#76035=CARTESIAN_POINT('Origin',(18.18,69.,8.7));
#76036=CARTESIAN_POINT('Origin',(18.3,28.08,8.));
#76037=CARTESIAN_POINT('',(18.3,28.08,8.));
#76038=CARTESIAN_POINT('',(18.3,27.92,8.));
#76039=CARTESIAN_POINT('',(18.3,49.04,8.));
#76040=CARTESIAN_POINT('',(18.18,28.08,8.));
#76041=CARTESIAN_POINT('',(18.3,28.08,8.));
#76042=CARTESIAN_POINT('',(18.18,27.92,8.));
#76043=CARTESIAN_POINT('',(18.18,27.92,8.));
#76044=CARTESIAN_POINT('',(18.3,27.92,8.));
#76045=CARTESIAN_POINT('Origin',(18.3,28.08,9.4));
#76046=CARTESIAN_POINT('',(18.3,28.08,9.4));
#76047=CARTESIAN_POINT('',(18.3,28.08,7.45));
#76048=CARTESIAN_POINT('',(18.18,28.08,9.4));
#76049=CARTESIAN_POINT('',(18.3,28.08,9.4));
#76050=CARTESIAN_POINT('',(18.18,28.08,8.));
#76051=CARTESIAN_POINT('Origin',(18.3,27.92,9.4));
#76052=CARTESIAN_POINT('',(18.3,27.92,9.4));
#76053=CARTESIAN_POINT('',(18.3,48.96,9.4));
#76054=CARTESIAN_POINT('',(18.18,27.92,9.4));
#76055=CARTESIAN_POINT('',(18.3,27.92,9.4));
#76056=CARTESIAN_POINT('',(18.18,28.08,9.4));
#76057=CARTESIAN_POINT('Origin',(18.3,27.92,8.));
#76058=CARTESIAN_POINT('',(18.3,27.92,6.75));
#76059=CARTESIAN_POINT('',(18.18,27.92,9.4));
#76060=CARTESIAN_POINT('Origin',(18.18,28.,8.7));
#76061=CARTESIAN_POINT('Origin',(18.3,72.08,8.));
#76062=CARTESIAN_POINT('',(18.3,72.08,8.));
#76063=CARTESIAN_POINT('',(18.3,71.92,8.));
#76064=CARTESIAN_POINT('',(18.3,71.04,8.));
#76065=CARTESIAN_POINT('',(18.18,72.08,8.));
#76066=CARTESIAN_POINT('',(18.3,72.08,8.));
#76067=CARTESIAN_POINT('',(18.18,71.92,8.));
#76068=CARTESIAN_POINT('',(18.18,71.92,8.));
#76069=CARTESIAN_POINT('',(18.3,71.92,8.));
#76070=CARTESIAN_POINT('Origin',(18.3,72.08,9.4));
#76071=CARTESIAN_POINT('',(18.3,72.08,9.4));
#76072=CARTESIAN_POINT('',(18.3,72.08,7.45));
#76073=CARTESIAN_POINT('',(18.18,72.08,9.4));
#76074=CARTESIAN_POINT('',(18.3,72.08,9.4));
#76075=CARTESIAN_POINT('',(18.18,72.08,8.));
#76076=CARTESIAN_POINT('Origin',(18.3,71.92,9.4));
#76077=CARTESIAN_POINT('',(18.3,71.92,9.4));
#76078=CARTESIAN_POINT('',(18.3,70.96,9.4));
#76079=CARTESIAN_POINT('',(18.18,71.92,9.4));
#76080=CARTESIAN_POINT('',(18.3,71.92,9.4));
#76081=CARTESIAN_POINT('',(18.18,72.08,9.4));
#76082=CARTESIAN_POINT('Origin',(18.3,71.92,8.));
#76083=CARTESIAN_POINT('',(18.3,71.92,6.75));
#76084=CARTESIAN_POINT('',(18.18,71.92,9.4));
#76085=CARTESIAN_POINT('Origin',(18.18,72.,8.7));
#76086=CARTESIAN_POINT('Origin',(18.3,74.08,8.));
#76087=CARTESIAN_POINT('',(18.3,74.08,8.));
#76088=CARTESIAN_POINT('',(18.3,73.92,8.));
#76089=CARTESIAN_POINT('',(18.3,72.04,8.));
#76090=CARTESIAN_POINT('',(18.18,74.08,8.));
#76091=CARTESIAN_POINT('',(18.3,74.08,8.));
#76092=CARTESIAN_POINT('',(18.18,73.92,8.));
#76093=CARTESIAN_POINT('',(18.18,73.92,8.));
#76094=CARTESIAN_POINT('',(18.3,73.92,8.));
#76095=CARTESIAN_POINT('Origin',(18.3,74.08,9.4));
#76096=CARTESIAN_POINT('',(18.3,74.08,9.4));
#76097=CARTESIAN_POINT('',(18.3,74.08,7.45));
#76098=CARTESIAN_POINT('',(18.18,74.08,9.4));
#76099=CARTESIAN_POINT('',(18.3,74.08,9.4));
#76100=CARTESIAN_POINT('',(18.18,74.08,8.));
#76101=CARTESIAN_POINT('Origin',(18.3,73.92,9.4));
#76102=CARTESIAN_POINT('',(18.3,73.92,9.4));
#76103=CARTESIAN_POINT('',(18.3,71.96,9.4));
#76104=CARTESIAN_POINT('',(18.18,73.92,9.4));
#76105=CARTESIAN_POINT('',(18.3,73.92,9.4));
#76106=CARTESIAN_POINT('',(18.18,74.08,9.4));
#76107=CARTESIAN_POINT('Origin',(18.3,73.92,8.));
#76108=CARTESIAN_POINT('',(18.3,73.92,6.75));
#76109=CARTESIAN_POINT('',(18.18,73.92,9.4));
#76110=CARTESIAN_POINT('Origin',(18.18,74.,8.7));
#76111=CARTESIAN_POINT('Origin',(18.3,76.08,8.));
#76112=CARTESIAN_POINT('',(18.3,76.08,8.));
#76113=CARTESIAN_POINT('',(18.3,75.92,8.));
#76114=CARTESIAN_POINT('',(18.3,73.04,8.));
#76115=CARTESIAN_POINT('',(18.18,76.08,8.));
#76116=CARTESIAN_POINT('',(18.3,76.08,8.));
#76117=CARTESIAN_POINT('',(18.18,75.92,8.));
#76118=CARTESIAN_POINT('',(18.18,75.92,8.));
#76119=CARTESIAN_POINT('',(18.3,75.92,8.));
#76120=CARTESIAN_POINT('Origin',(18.3,76.08,9.4));
#76121=CARTESIAN_POINT('',(18.3,76.08,9.4));
#76122=CARTESIAN_POINT('',(18.3,76.08,7.45));
#76123=CARTESIAN_POINT('',(18.18,76.08,9.4));
#76124=CARTESIAN_POINT('',(18.3,76.08,9.4));
#76125=CARTESIAN_POINT('',(18.18,76.08,8.));
#76126=CARTESIAN_POINT('Origin',(18.3,75.92,9.4));
#76127=CARTESIAN_POINT('',(18.3,75.92,9.4));
#76128=CARTESIAN_POINT('',(18.3,72.96,9.4));
#76129=CARTESIAN_POINT('',(18.18,75.92,9.4));
#76130=CARTESIAN_POINT('',(18.3,75.92,9.4));
#76131=CARTESIAN_POINT('',(18.18,76.08,9.4));
#76132=CARTESIAN_POINT('Origin',(18.3,75.92,8.));
#76133=CARTESIAN_POINT('',(18.3,75.92,6.75));
#76134=CARTESIAN_POINT('',(18.18,75.92,9.4));
#76135=CARTESIAN_POINT('Origin',(18.18,76.,8.7));
#76136=CARTESIAN_POINT('Origin',(18.3,78.08,8.));
#76137=CARTESIAN_POINT('',(18.3,78.08,8.));
#76138=CARTESIAN_POINT('',(18.3,77.92,8.));
#76139=CARTESIAN_POINT('',(18.3,74.04,8.));
#76140=CARTESIAN_POINT('',(18.18,78.08,8.));
#76141=CARTESIAN_POINT('',(18.3,78.08,8.));
#76142=CARTESIAN_POINT('',(18.18,77.92,8.));
#76143=CARTESIAN_POINT('',(18.18,77.92,8.));
#76144=CARTESIAN_POINT('',(18.3,77.92,8.));
#76145=CARTESIAN_POINT('Origin',(18.3,78.08,9.4));
#76146=CARTESIAN_POINT('',(18.3,78.08,9.4));
#76147=CARTESIAN_POINT('',(18.3,78.08,7.45));
#76148=CARTESIAN_POINT('',(18.18,78.08,9.4));
#76149=CARTESIAN_POINT('',(18.3,78.08,9.4));
#76150=CARTESIAN_POINT('',(18.18,78.08,8.));
#76151=CARTESIAN_POINT('Origin',(18.3,77.92,9.4));
#76152=CARTESIAN_POINT('',(18.3,77.92,9.4));
#76153=CARTESIAN_POINT('',(18.3,73.96,9.4));
#76154=CARTESIAN_POINT('',(18.18,77.92,9.4));
#76155=CARTESIAN_POINT('',(18.3,77.92,9.4));
#76156=CARTESIAN_POINT('',(18.18,78.08,9.4));
#76157=CARTESIAN_POINT('Origin',(18.3,77.92,8.));
#76158=CARTESIAN_POINT('',(18.3,77.92,6.75));
#76159=CARTESIAN_POINT('',(18.18,77.92,9.4));
#76160=CARTESIAN_POINT('Origin',(18.18,78.,8.7));
#76161=CARTESIAN_POINT('Origin',(18.3,80.08,6.4));
#76162=CARTESIAN_POINT('',(18.3,80.08,6.4));
#76163=CARTESIAN_POINT('',(18.3,79.92,6.4));
#76164=CARTESIAN_POINT('',(18.3,75.04,6.4));
#76165=CARTESIAN_POINT('',(18.18,80.08,6.4));
#76166=CARTESIAN_POINT('',(18.3,80.08,6.4));
#76167=CARTESIAN_POINT('',(18.18,79.92,6.4));
#76168=CARTESIAN_POINT('',(18.18,79.92,6.4));
#76169=CARTESIAN_POINT('',(18.3,79.92,6.4));
#76170=CARTESIAN_POINT('Origin',(18.3,80.08,9.4));
#76171=CARTESIAN_POINT('',(18.3,80.08,9.4));
#76172=CARTESIAN_POINT('',(18.3,80.08,7.45));
#76173=CARTESIAN_POINT('',(18.18,80.08,9.4));
#76174=CARTESIAN_POINT('',(18.3,80.08,9.4));
#76175=CARTESIAN_POINT('',(18.18,80.08,6.4));
#76176=CARTESIAN_POINT('Origin',(18.3,79.92,9.4));
#76177=CARTESIAN_POINT('',(18.3,79.92,9.4));
#76178=CARTESIAN_POINT('',(18.3,74.96,9.4));
#76179=CARTESIAN_POINT('',(18.18,79.92,9.4));
#76180=CARTESIAN_POINT('',(18.3,79.92,9.4));
#76181=CARTESIAN_POINT('',(18.18,80.08,9.4));
#76182=CARTESIAN_POINT('Origin',(18.3,79.92,6.4));
#76183=CARTESIAN_POINT('',(18.3,79.92,5.95));
#76184=CARTESIAN_POINT('',(18.18,79.92,9.4));
#76185=CARTESIAN_POINT('Origin',(18.18,80.,7.9));
#76186=CARTESIAN_POINT('Origin',(18.3,82.08,8.));
#76187=CARTESIAN_POINT('',(18.3,82.08,8.));
#76188=CARTESIAN_POINT('',(18.3,81.92,8.));
#76189=CARTESIAN_POINT('',(18.3,76.04,8.));
#76190=CARTESIAN_POINT('',(18.18,82.08,8.));
#76191=CARTESIAN_POINT('',(18.3,82.08,8.));
#76192=CARTESIAN_POINT('',(18.18,81.92,8.));
#76193=CARTESIAN_POINT('',(18.18,81.92,8.));
#76194=CARTESIAN_POINT('',(18.3,81.92,8.));
#76195=CARTESIAN_POINT('Origin',(18.3,82.08,9.4));
#76196=CARTESIAN_POINT('',(18.3,82.08,9.4));
#76197=CARTESIAN_POINT('',(18.3,82.08,7.45));
#76198=CARTESIAN_POINT('',(18.18,82.08,9.4));
#76199=CARTESIAN_POINT('',(18.3,82.08,9.4));
#76200=CARTESIAN_POINT('',(18.18,82.08,8.));
#76201=CARTESIAN_POINT('Origin',(18.3,81.92,9.4));
#76202=CARTESIAN_POINT('',(18.3,81.92,9.4));
#76203=CARTESIAN_POINT('',(18.3,75.96,9.4));
#76204=CARTESIAN_POINT('',(18.18,81.92,9.4));
#76205=CARTESIAN_POINT('',(18.3,81.92,9.4));
#76206=CARTESIAN_POINT('',(18.18,82.08,9.4));
#76207=CARTESIAN_POINT('Origin',(18.3,81.92,8.));
#76208=CARTESIAN_POINT('',(18.3,81.92,6.75));
#76209=CARTESIAN_POINT('',(18.18,81.92,9.4));
#76210=CARTESIAN_POINT('Origin',(18.18,82.,8.7));
#76211=CARTESIAN_POINT('Origin',(18.3,84.08,8.));
#76212=CARTESIAN_POINT('',(18.3,84.08,8.));
#76213=CARTESIAN_POINT('',(18.3,83.92,8.));
#76214=CARTESIAN_POINT('',(18.3,77.04,8.));
#76215=CARTESIAN_POINT('',(18.18,84.08,8.));
#76216=CARTESIAN_POINT('',(18.3,84.08,8.));
#76217=CARTESIAN_POINT('',(18.18,83.92,8.));
#76218=CARTESIAN_POINT('',(18.18,83.92,8.));
#76219=CARTESIAN_POINT('',(18.3,83.92,8.));
#76220=CARTESIAN_POINT('Origin',(18.3,84.08,9.4));
#76221=CARTESIAN_POINT('',(18.3,84.08,9.4));
#76222=CARTESIAN_POINT('',(18.3,84.08,7.45));
#76223=CARTESIAN_POINT('',(18.18,84.08,9.4));
#76224=CARTESIAN_POINT('',(18.3,84.08,9.4));
#76225=CARTESIAN_POINT('',(18.18,84.08,8.));
#76226=CARTESIAN_POINT('Origin',(18.3,83.92,9.4));
#76227=CARTESIAN_POINT('',(18.3,83.92,9.4));
#76228=CARTESIAN_POINT('',(18.3,76.96,9.4));
#76229=CARTESIAN_POINT('',(18.18,83.92,9.4));
#76230=CARTESIAN_POINT('',(18.3,83.92,9.4));
#76231=CARTESIAN_POINT('',(18.18,84.08,9.4));
#76232=CARTESIAN_POINT('Origin',(18.3,83.92,8.));
#76233=CARTESIAN_POINT('',(18.3,83.92,6.75));
#76234=CARTESIAN_POINT('',(18.18,83.92,9.4));
#76235=CARTESIAN_POINT('Origin',(18.18,84.,8.7));
#76236=CARTESIAN_POINT('Origin',(18.3,86.08,8.));
#76237=CARTESIAN_POINT('',(18.3,86.08,8.));
#76238=CARTESIAN_POINT('',(18.3,85.92,8.));
#76239=CARTESIAN_POINT('',(18.3,78.04,8.));
#76240=CARTESIAN_POINT('',(18.18,86.08,8.));
#76241=CARTESIAN_POINT('',(18.3,86.08,8.));
#76242=CARTESIAN_POINT('',(18.18,85.92,8.));
#76243=CARTESIAN_POINT('',(18.18,85.92,8.));
#76244=CARTESIAN_POINT('',(18.3,85.92,8.));
#76245=CARTESIAN_POINT('Origin',(18.3,86.08,9.4));
#76246=CARTESIAN_POINT('',(18.3,86.08,9.4));
#76247=CARTESIAN_POINT('',(18.3,86.08,7.45));
#76248=CARTESIAN_POINT('',(18.18,86.08,9.4));
#76249=CARTESIAN_POINT('',(18.3,86.08,9.4));
#76250=CARTESIAN_POINT('',(18.18,86.08,8.));
#76251=CARTESIAN_POINT('Origin',(18.3,85.92,9.4));
#76252=CARTESIAN_POINT('',(18.3,85.92,9.4));
#76253=CARTESIAN_POINT('',(18.3,77.96,9.4));
#76254=CARTESIAN_POINT('',(18.18,85.92,9.4));
#76255=CARTESIAN_POINT('',(18.3,85.92,9.4));
#76256=CARTESIAN_POINT('',(18.18,86.08,9.4));
#76257=CARTESIAN_POINT('Origin',(18.3,85.92,8.));
#76258=CARTESIAN_POINT('',(18.3,85.92,6.75));
#76259=CARTESIAN_POINT('',(18.18,85.92,9.4));
#76260=CARTESIAN_POINT('Origin',(18.18,86.,8.7));
#76261=CARTESIAN_POINT('Origin',(18.3,88.08,8.));
#76262=CARTESIAN_POINT('',(18.3,88.08,8.));
#76263=CARTESIAN_POINT('',(18.3,87.92,8.));
#76264=CARTESIAN_POINT('',(18.3,79.04,8.));
#76265=CARTESIAN_POINT('',(18.18,88.08,8.));
#76266=CARTESIAN_POINT('',(18.3,88.08,8.));
#76267=CARTESIAN_POINT('',(18.18,87.92,8.));
#76268=CARTESIAN_POINT('',(18.18,87.92,8.));
#76269=CARTESIAN_POINT('',(18.3,87.92,8.));
#76270=CARTESIAN_POINT('Origin',(18.3,88.08,9.4));
#76271=CARTESIAN_POINT('',(18.3,88.08,9.4));
#76272=CARTESIAN_POINT('',(18.3,88.08,7.45));
#76273=CARTESIAN_POINT('',(18.18,88.08,9.4));
#76274=CARTESIAN_POINT('',(18.3,88.08,9.4));
#76275=CARTESIAN_POINT('',(18.18,88.08,8.));
#76276=CARTESIAN_POINT('Origin',(18.3,87.92,9.4));
#76277=CARTESIAN_POINT('',(18.3,87.92,9.4));
#76278=CARTESIAN_POINT('',(18.3,78.96,9.4));
#76279=CARTESIAN_POINT('',(18.18,87.92,9.4));
#76280=CARTESIAN_POINT('',(18.3,87.92,9.4));
#76281=CARTESIAN_POINT('',(18.18,88.08,9.4));
#76282=CARTESIAN_POINT('Origin',(18.3,87.92,8.));
#76283=CARTESIAN_POINT('',(18.3,87.92,6.75));
#76284=CARTESIAN_POINT('',(18.18,87.92,9.4));
#76285=CARTESIAN_POINT('Origin',(18.18,88.,8.7));
#76286=CARTESIAN_POINT('Origin',(18.3,90.08,6.4));
#76287=CARTESIAN_POINT('',(18.3,90.08,6.4));
#76288=CARTESIAN_POINT('',(18.3,89.92,6.4));
#76289=CARTESIAN_POINT('',(18.3,80.04,6.4));
#76290=CARTESIAN_POINT('',(18.18,90.08,6.4));
#76291=CARTESIAN_POINT('',(18.3,90.08,6.4));
#76292=CARTESIAN_POINT('',(18.18,89.92,6.4));
#76293=CARTESIAN_POINT('',(18.18,89.92,6.4));
#76294=CARTESIAN_POINT('',(18.3,89.92,6.4));
#76295=CARTESIAN_POINT('Origin',(18.3,90.08,9.4));
#76296=CARTESIAN_POINT('',(18.3,90.08,9.4));
#76297=CARTESIAN_POINT('',(18.3,90.08,7.45));
#76298=CARTESIAN_POINT('',(18.18,90.08,9.4));
#76299=CARTESIAN_POINT('',(18.3,90.08,9.4));
#76300=CARTESIAN_POINT('',(18.18,90.08,6.4));
#76301=CARTESIAN_POINT('Origin',(18.3,89.92,9.4));
#76302=CARTESIAN_POINT('',(18.3,89.92,9.4));
#76303=CARTESIAN_POINT('',(18.3,79.96,9.4));
#76304=CARTESIAN_POINT('',(18.18,89.92,9.4));
#76305=CARTESIAN_POINT('',(18.3,89.92,9.4));
#76306=CARTESIAN_POINT('',(18.18,90.08,9.4));
#76307=CARTESIAN_POINT('Origin',(18.3,89.92,6.4));
#76308=CARTESIAN_POINT('',(18.3,89.92,5.95));
#76309=CARTESIAN_POINT('',(18.18,89.92,9.4));
#76310=CARTESIAN_POINT('Origin',(18.18,90.,7.9));
#76311=CARTESIAN_POINT('Origin',(18.3,92.08,8.));
#76312=CARTESIAN_POINT('',(18.3,92.08,8.));
#76313=CARTESIAN_POINT('',(18.3,91.92,8.));
#76314=CARTESIAN_POINT('',(18.3,81.04,8.));
#76315=CARTESIAN_POINT('',(18.18,92.08,8.));
#76316=CARTESIAN_POINT('',(18.3,92.08,8.));
#76317=CARTESIAN_POINT('',(18.18,91.92,8.));
#76318=CARTESIAN_POINT('',(18.18,91.92,8.));
#76319=CARTESIAN_POINT('',(18.3,91.92,8.));
#76320=CARTESIAN_POINT('Origin',(18.3,92.08,9.4));
#76321=CARTESIAN_POINT('',(18.3,92.08,9.4));
#76322=CARTESIAN_POINT('',(18.3,92.08,7.45));
#76323=CARTESIAN_POINT('',(18.18,92.08,9.4));
#76324=CARTESIAN_POINT('',(18.3,92.08,9.4));
#76325=CARTESIAN_POINT('',(18.18,92.08,8.));
#76326=CARTESIAN_POINT('Origin',(18.3,91.92,9.4));
#76327=CARTESIAN_POINT('',(18.3,91.92,9.4));
#76328=CARTESIAN_POINT('',(18.3,80.96,9.4));
#76329=CARTESIAN_POINT('',(18.18,91.92,9.4));
#76330=CARTESIAN_POINT('',(18.3,91.92,9.4));
#76331=CARTESIAN_POINT('',(18.18,92.08,9.4));
#76332=CARTESIAN_POINT('Origin',(18.3,91.92,8.));
#76333=CARTESIAN_POINT('',(18.3,91.92,6.75));
#76334=CARTESIAN_POINT('',(18.18,91.92,9.4));
#76335=CARTESIAN_POINT('Origin',(18.18,92.,8.7));
#76336=CARTESIAN_POINT('Origin',(18.3,94.08,8.));
#76337=CARTESIAN_POINT('',(18.3,94.08,8.));
#76338=CARTESIAN_POINT('',(18.3,93.92,8.));
#76339=CARTESIAN_POINT('',(18.3,82.04,8.));
#76340=CARTESIAN_POINT('',(18.18,94.08,8.));
#76341=CARTESIAN_POINT('',(18.3,94.08,8.));
#76342=CARTESIAN_POINT('',(18.18,93.92,8.));
#76343=CARTESIAN_POINT('',(18.18,93.92,8.));
#76344=CARTESIAN_POINT('',(18.3,93.92,8.));
#76345=CARTESIAN_POINT('Origin',(18.3,94.08,9.4));
#76346=CARTESIAN_POINT('',(18.3,94.08,9.4));
#76347=CARTESIAN_POINT('',(18.3,94.08,7.45));
#76348=CARTESIAN_POINT('',(18.18,94.08,9.4));
#76349=CARTESIAN_POINT('',(18.3,94.08,9.4));
#76350=CARTESIAN_POINT('',(18.18,94.08,8.));
#76351=CARTESIAN_POINT('Origin',(18.3,93.92,9.4));
#76352=CARTESIAN_POINT('',(18.3,93.92,9.4));
#76353=CARTESIAN_POINT('',(18.3,81.96,9.4));
#76354=CARTESIAN_POINT('',(18.18,93.92,9.4));
#76355=CARTESIAN_POINT('',(18.3,93.92,9.4));
#76356=CARTESIAN_POINT('',(18.18,94.08,9.4));
#76357=CARTESIAN_POINT('Origin',(18.3,93.92,8.));
#76358=CARTESIAN_POINT('',(18.3,93.92,6.75));
#76359=CARTESIAN_POINT('',(18.18,93.92,9.4));
#76360=CARTESIAN_POINT('Origin',(18.18,94.,8.7));
#76361=CARTESIAN_POINT('Origin',(18.3,96.08,8.));
#76362=CARTESIAN_POINT('',(18.3,96.08,8.));
#76363=CARTESIAN_POINT('',(18.3,95.92,8.));
#76364=CARTESIAN_POINT('',(18.3,83.04,8.));
#76365=CARTESIAN_POINT('',(18.18,96.08,8.));
#76366=CARTESIAN_POINT('',(18.3,96.08,8.));
#76367=CARTESIAN_POINT('',(18.18,95.92,8.));
#76368=CARTESIAN_POINT('',(18.18,95.92,8.));
#76369=CARTESIAN_POINT('',(18.3,95.92,8.));
#76370=CARTESIAN_POINT('Origin',(18.3,96.08,9.4));
#76371=CARTESIAN_POINT('',(18.3,96.08,9.4));
#76372=CARTESIAN_POINT('',(18.3,96.08,7.45));
#76373=CARTESIAN_POINT('',(18.18,96.08,9.4));
#76374=CARTESIAN_POINT('',(18.3,96.08,9.4));
#76375=CARTESIAN_POINT('',(18.18,96.08,8.));
#76376=CARTESIAN_POINT('Origin',(18.3,95.92,9.4));
#76377=CARTESIAN_POINT('',(18.3,95.92,9.4));
#76378=CARTESIAN_POINT('',(18.3,82.96,9.4));
#76379=CARTESIAN_POINT('',(18.18,95.92,9.4));
#76380=CARTESIAN_POINT('',(18.3,95.92,9.4));
#76381=CARTESIAN_POINT('',(18.18,96.08,9.4));
#76382=CARTESIAN_POINT('Origin',(18.3,95.92,8.));
#76383=CARTESIAN_POINT('',(18.3,95.92,6.75));
#76384=CARTESIAN_POINT('',(18.18,95.92,9.4));
#76385=CARTESIAN_POINT('Origin',(18.18,96.,8.7));
#76386=CARTESIAN_POINT('Origin',(18.3,98.08,8.));
#76387=CARTESIAN_POINT('',(18.3,98.08,8.));
#76388=CARTESIAN_POINT('',(18.3,97.92,8.));
#76389=CARTESIAN_POINT('',(18.3,84.04,8.));
#76390=CARTESIAN_POINT('',(18.18,98.08,8.));
#76391=CARTESIAN_POINT('',(18.3,98.08,8.));
#76392=CARTESIAN_POINT('',(18.18,97.92,8.));
#76393=CARTESIAN_POINT('',(18.18,97.92,8.));
#76394=CARTESIAN_POINT('',(18.3,97.92,8.));
#76395=CARTESIAN_POINT('Origin',(18.3,98.08,9.4));
#76396=CARTESIAN_POINT('',(18.3,98.08,9.4));
#76397=CARTESIAN_POINT('',(18.3,98.08,7.45));
#76398=CARTESIAN_POINT('',(18.18,98.08,9.4));
#76399=CARTESIAN_POINT('',(18.3,98.08,9.4));
#76400=CARTESIAN_POINT('',(18.18,98.08,8.));
#76401=CARTESIAN_POINT('Origin',(18.3,97.92,9.4));
#76402=CARTESIAN_POINT('',(18.3,97.92,9.4));
#76403=CARTESIAN_POINT('',(18.3,83.96,9.4));
#76404=CARTESIAN_POINT('',(18.18,97.92,9.4));
#76405=CARTESIAN_POINT('',(18.3,97.92,9.4));
#76406=CARTESIAN_POINT('',(18.18,98.08,9.4));
#76407=CARTESIAN_POINT('Origin',(18.3,97.92,8.));
#76408=CARTESIAN_POINT('',(18.3,97.92,6.75));
#76409=CARTESIAN_POINT('',(18.18,97.92,9.4));
#76410=CARTESIAN_POINT('Origin',(18.18,98.,8.7));
#76411=CARTESIAN_POINT('Origin',(18.3,100.08,6.4));
#76412=CARTESIAN_POINT('',(18.3,100.08,6.4));
#76413=CARTESIAN_POINT('',(18.3,99.92,6.4));
#76414=CARTESIAN_POINT('',(18.3,85.04,6.4));
#76415=CARTESIAN_POINT('',(18.18,100.08,6.4));
#76416=CARTESIAN_POINT('',(18.3,100.08,6.4));
#76417=CARTESIAN_POINT('',(18.18,99.92,6.4));
#76418=CARTESIAN_POINT('',(18.18,99.92,6.4));
#76419=CARTESIAN_POINT('',(18.3,99.92,6.4));
#76420=CARTESIAN_POINT('Origin',(18.3,100.08,9.4));
#76421=CARTESIAN_POINT('',(18.3,100.08,9.4));
#76422=CARTESIAN_POINT('',(18.3,100.08,7.45));
#76423=CARTESIAN_POINT('',(18.18,100.08,9.4));
#76424=CARTESIAN_POINT('',(18.3,100.08,9.4));
#76425=CARTESIAN_POINT('',(18.18,100.08,6.4));
#76426=CARTESIAN_POINT('Origin',(18.3,99.92,9.4));
#76427=CARTESIAN_POINT('',(18.3,99.92,9.4));
#76428=CARTESIAN_POINT('',(18.3,84.96,9.4));
#76429=CARTESIAN_POINT('',(18.18,99.92,9.4));
#76430=CARTESIAN_POINT('',(18.3,99.92,9.4));
#76431=CARTESIAN_POINT('',(18.18,100.08,9.4));
#76432=CARTESIAN_POINT('Origin',(18.3,99.92,6.4));
#76433=CARTESIAN_POINT('',(18.3,99.92,5.95));
#76434=CARTESIAN_POINT('',(18.18,99.92,9.4));
#76435=CARTESIAN_POINT('Origin',(18.18,100.,7.9));
#76436=CARTESIAN_POINT('Origin',(18.3,102.08,8.));
#76437=CARTESIAN_POINT('',(18.3,102.08,8.));
#76438=CARTESIAN_POINT('',(18.3,101.92,8.));
#76439=CARTESIAN_POINT('',(18.3,86.04,8.));
#76440=CARTESIAN_POINT('',(18.18,102.08,8.));
#76441=CARTESIAN_POINT('',(18.3,102.08,8.));
#76442=CARTESIAN_POINT('',(18.18,101.92,8.));
#76443=CARTESIAN_POINT('',(18.18,101.92,8.));
#76444=CARTESIAN_POINT('',(18.3,101.92,8.));
#76445=CARTESIAN_POINT('Origin',(18.3,102.08,9.4));
#76446=CARTESIAN_POINT('',(18.3,102.08,9.4));
#76447=CARTESIAN_POINT('',(18.3,102.08,7.45));
#76448=CARTESIAN_POINT('',(18.18,102.08,9.4));
#76449=CARTESIAN_POINT('',(18.3,102.08,9.4));
#76450=CARTESIAN_POINT('',(18.18,102.08,8.));
#76451=CARTESIAN_POINT('Origin',(18.3,101.92,9.4));
#76452=CARTESIAN_POINT('',(18.3,101.92,9.4));
#76453=CARTESIAN_POINT('',(18.3,85.96,9.4));
#76454=CARTESIAN_POINT('',(18.18,101.92,9.4));
#76455=CARTESIAN_POINT('',(18.3,101.92,9.4));
#76456=CARTESIAN_POINT('',(18.18,102.08,9.4));
#76457=CARTESIAN_POINT('Origin',(18.3,101.92,8.));
#76458=CARTESIAN_POINT('',(18.3,101.92,6.75));
#76459=CARTESIAN_POINT('',(18.18,101.92,9.4));
#76460=CARTESIAN_POINT('Origin',(18.18,102.,8.7));
#76461=CARTESIAN_POINT('Origin',(18.3,104.08,8.));
#76462=CARTESIAN_POINT('',(18.3,104.08,8.));
#76463=CARTESIAN_POINT('',(18.3,103.92,8.));
#76464=CARTESIAN_POINT('',(18.3,87.04,8.));
#76465=CARTESIAN_POINT('',(18.18,104.08,8.));
#76466=CARTESIAN_POINT('',(18.3,104.08,8.));
#76467=CARTESIAN_POINT('',(18.18,103.92,8.));
#76468=CARTESIAN_POINT('',(18.18,103.92,8.));
#76469=CARTESIAN_POINT('',(18.3,103.92,8.));
#76470=CARTESIAN_POINT('Origin',(18.3,104.08,9.4));
#76471=CARTESIAN_POINT('',(18.3,104.08,9.4));
#76472=CARTESIAN_POINT('',(18.3,104.08,7.45));
#76473=CARTESIAN_POINT('',(18.18,104.08,9.4));
#76474=CARTESIAN_POINT('',(18.3,104.08,9.4));
#76475=CARTESIAN_POINT('',(18.18,104.08,8.));
#76476=CARTESIAN_POINT('Origin',(18.3,103.92,9.4));
#76477=CARTESIAN_POINT('',(18.3,103.92,9.4));
#76478=CARTESIAN_POINT('',(18.3,86.96,9.4));
#76479=CARTESIAN_POINT('',(18.18,103.92,9.4));
#76480=CARTESIAN_POINT('',(18.3,103.92,9.4));
#76481=CARTESIAN_POINT('',(18.18,104.08,9.4));
#76482=CARTESIAN_POINT('Origin',(18.3,103.92,8.));
#76483=CARTESIAN_POINT('',(18.3,103.92,6.75));
#76484=CARTESIAN_POINT('',(18.18,103.92,9.4));
#76485=CARTESIAN_POINT('Origin',(18.18,104.,8.7));
#76486=CARTESIAN_POINT('Origin',(18.3,106.08,8.));
#76487=CARTESIAN_POINT('',(18.3,106.08,8.));
#76488=CARTESIAN_POINT('',(18.3,105.92,8.));
#76489=CARTESIAN_POINT('',(18.3,88.04,8.));
#76490=CARTESIAN_POINT('',(18.18,106.08,8.));
#76491=CARTESIAN_POINT('',(18.3,106.08,8.));
#76492=CARTESIAN_POINT('',(18.18,105.92,8.));
#76493=CARTESIAN_POINT('',(18.18,105.92,8.));
#76494=CARTESIAN_POINT('',(18.3,105.92,8.));
#76495=CARTESIAN_POINT('Origin',(18.3,106.08,9.4));
#76496=CARTESIAN_POINT('',(18.3,106.08,9.4));
#76497=CARTESIAN_POINT('',(18.3,106.08,7.45));
#76498=CARTESIAN_POINT('',(18.18,106.08,9.4));
#76499=CARTESIAN_POINT('',(18.3,106.08,9.4));
#76500=CARTESIAN_POINT('',(18.18,106.08,8.));
#76501=CARTESIAN_POINT('Origin',(18.3,105.92,9.4));
#76502=CARTESIAN_POINT('',(18.3,105.92,9.4));
#76503=CARTESIAN_POINT('',(18.3,87.96,9.4));
#76504=CARTESIAN_POINT('',(18.18,105.92,9.4));
#76505=CARTESIAN_POINT('',(18.3,105.92,9.4));
#76506=CARTESIAN_POINT('',(18.18,106.08,9.4));
#76507=CARTESIAN_POINT('Origin',(18.3,105.92,8.));
#76508=CARTESIAN_POINT('',(18.3,105.92,6.75));
#76509=CARTESIAN_POINT('',(18.18,105.92,9.4));
#76510=CARTESIAN_POINT('Origin',(18.18,106.,8.7));
#76511=CARTESIAN_POINT('Origin',(18.3,108.08,8.));
#76512=CARTESIAN_POINT('',(18.3,108.08,8.));
#76513=CARTESIAN_POINT('',(18.3,107.92,8.));
#76514=CARTESIAN_POINT('',(18.3,89.04,8.));
#76515=CARTESIAN_POINT('',(18.18,108.08,8.));
#76516=CARTESIAN_POINT('',(18.3,108.08,8.));
#76517=CARTESIAN_POINT('',(18.18,107.92,8.));
#76518=CARTESIAN_POINT('',(18.18,107.92,8.));
#76519=CARTESIAN_POINT('',(18.3,107.92,8.));
#76520=CARTESIAN_POINT('Origin',(18.3,108.08,9.4));
#76521=CARTESIAN_POINT('',(18.3,108.08,9.4));
#76522=CARTESIAN_POINT('',(18.3,108.08,7.45));
#76523=CARTESIAN_POINT('',(18.18,108.08,9.4));
#76524=CARTESIAN_POINT('',(18.3,108.08,9.4));
#76525=CARTESIAN_POINT('',(18.18,108.08,8.));
#76526=CARTESIAN_POINT('Origin',(18.3,107.92,9.4));
#76527=CARTESIAN_POINT('',(18.3,107.92,9.4));
#76528=CARTESIAN_POINT('',(18.3,88.96,9.4));
#76529=CARTESIAN_POINT('',(18.18,107.92,9.4));
#76530=CARTESIAN_POINT('',(18.3,107.92,9.4));
#76531=CARTESIAN_POINT('',(18.18,108.08,9.4));
#76532=CARTESIAN_POINT('Origin',(18.3,107.92,8.));
#76533=CARTESIAN_POINT('',(18.3,107.92,6.75));
#76534=CARTESIAN_POINT('',(18.18,107.92,9.4));
#76535=CARTESIAN_POINT('Origin',(18.18,108.,8.7));
#76536=CARTESIAN_POINT('Origin',(18.3,110.08,6.4));
#76537=CARTESIAN_POINT('',(18.3,110.08,6.4));
#76538=CARTESIAN_POINT('',(18.3,109.92,6.4));
#76539=CARTESIAN_POINT('',(18.3,90.04,6.4));
#76540=CARTESIAN_POINT('',(18.18,110.08,6.4));
#76541=CARTESIAN_POINT('',(18.3,110.08,6.4));
#76542=CARTESIAN_POINT('',(18.18,109.92,6.4));
#76543=CARTESIAN_POINT('',(18.18,109.92,6.4));
#76544=CARTESIAN_POINT('',(18.3,109.92,6.4));
#76545=CARTESIAN_POINT('Origin',(18.3,110.08,9.4));
#76546=CARTESIAN_POINT('',(18.3,110.08,9.4));
#76547=CARTESIAN_POINT('',(18.3,110.08,7.45));
#76548=CARTESIAN_POINT('',(18.18,110.08,9.4));
#76549=CARTESIAN_POINT('',(18.3,110.08,9.4));
#76550=CARTESIAN_POINT('',(18.18,110.08,6.4));
#76551=CARTESIAN_POINT('Origin',(18.3,109.92,9.4));
#76552=CARTESIAN_POINT('',(18.3,109.92,9.4));
#76553=CARTESIAN_POINT('',(18.3,89.96,9.4));
#76554=CARTESIAN_POINT('',(18.18,109.92,9.4));
#76555=CARTESIAN_POINT('',(18.3,109.92,9.4));
#76556=CARTESIAN_POINT('',(18.18,110.08,9.4));
#76557=CARTESIAN_POINT('Origin',(18.3,109.92,6.4));
#76558=CARTESIAN_POINT('',(18.3,109.92,5.95));
#76559=CARTESIAN_POINT('',(18.18,109.92,9.4));
#76560=CARTESIAN_POINT('Origin',(18.18,110.,7.9));
#76561=CARTESIAN_POINT('Origin',(18.3,112.08,8.));
#76562=CARTESIAN_POINT('',(18.3,112.08,8.));
#76563=CARTESIAN_POINT('',(18.3,111.92,8.));
#76564=CARTESIAN_POINT('',(18.3,91.04,8.));
#76565=CARTESIAN_POINT('',(18.18,112.08,8.));
#76566=CARTESIAN_POINT('',(18.3,112.08,8.));
#76567=CARTESIAN_POINT('',(18.18,111.92,8.));
#76568=CARTESIAN_POINT('',(18.18,111.92,8.));
#76569=CARTESIAN_POINT('',(18.3,111.92,8.));
#76570=CARTESIAN_POINT('Origin',(18.3,112.08,9.4));
#76571=CARTESIAN_POINT('',(18.3,112.08,9.4));
#76572=CARTESIAN_POINT('',(18.3,112.08,7.45));
#76573=CARTESIAN_POINT('',(18.18,112.08,9.4));
#76574=CARTESIAN_POINT('',(18.3,112.08,9.4));
#76575=CARTESIAN_POINT('',(18.18,112.08,8.));
#76576=CARTESIAN_POINT('Origin',(18.3,111.92,9.4));
#76577=CARTESIAN_POINT('',(18.3,111.92,9.4));
#76578=CARTESIAN_POINT('',(18.3,90.96,9.4));
#76579=CARTESIAN_POINT('',(18.18,111.92,9.4));
#76580=CARTESIAN_POINT('',(18.3,111.92,9.4));
#76581=CARTESIAN_POINT('',(18.18,112.08,9.4));
#76582=CARTESIAN_POINT('Origin',(18.3,111.92,8.));
#76583=CARTESIAN_POINT('',(18.3,111.92,6.75));
#76584=CARTESIAN_POINT('',(18.18,111.92,9.4));
#76585=CARTESIAN_POINT('Origin',(18.18,112.,8.7));
#76586=CARTESIAN_POINT('Origin',(17.5,15.,5.5));
#76587=CARTESIAN_POINT('',(17.5,15.,6.6));
#76588=CARTESIAN_POINT('Origin',(17.5,15.,5.5));
#76589=CARTESIAN_POINT('',(18.3,15.,6.6));
#76590=CARTESIAN_POINT('',(17.5,15.,6.6));
#76591=CARTESIAN_POINT('Origin',(18.3,15.,5.5));
#76592=CARTESIAN_POINT('Origin',(17.5,125.,5.5));
#76593=CARTESIAN_POINT('',(17.5,125.,6.6));
#76594=CARTESIAN_POINT('Origin',(17.5,125.,5.5));
#76595=CARTESIAN_POINT('',(18.3,125.,6.6));
#76596=CARTESIAN_POINT('',(17.5,125.,6.6));
#76597=CARTESIAN_POINT('Origin',(18.3,125.,5.5));
#76598=CARTESIAN_POINT('Origin',(17.5,11.,9.2));
#76599=CARTESIAN_POINT('',(17.5,11.,9.2));
#76600=CARTESIAN_POINT('',(17.5,11.,1.8));
#76601=CARTESIAN_POINT('',(17.5,11.,9.2));
#76602=CARTESIAN_POINT('',(18.3,11.,1.8));
#76603=CARTESIAN_POINT('',(17.5,11.,1.8));
#76604=CARTESIAN_POINT('',(18.3,11.,9.2));
#76605=CARTESIAN_POINT('',(18.3,11.,9.2));
#76606=CARTESIAN_POINT('',(17.5,11.,9.2));
#76607=CARTESIAN_POINT('Origin',(17.5,11.8,9.2));
#76608=CARTESIAN_POINT('',(17.5,11.8,10.));
#76609=CARTESIAN_POINT('Origin',(17.5,11.8,9.2));
#76610=CARTESIAN_POINT('',(18.3,11.8,10.));
#76611=CARTESIAN_POINT('Origin',(18.3,11.8,9.2));
#76612=CARTESIAN_POINT('',(17.5,11.8,10.));
#76613=CARTESIAN_POINT('Origin',(17.5,128.2,10.));
#76614=CARTESIAN_POINT('',(17.5,128.2,10.));
#76615=CARTESIAN_POINT('',(17.5,128.2,10.));
#76616=CARTESIAN_POINT('',(18.3,128.2,10.));
#76617=CARTESIAN_POINT('',(18.3,128.2,10.));
#76618=CARTESIAN_POINT('',(17.5,128.2,10.));
#76619=CARTESIAN_POINT('Origin',(17.5,128.2,9.19999999999997));
#76620=CARTESIAN_POINT('',(17.5,129.,9.2));
#76621=CARTESIAN_POINT('Origin',(17.5,128.2,9.19999999999997));
#76622=CARTESIAN_POINT('',(18.3,129.,9.2));
#76623=CARTESIAN_POINT('Origin',(18.3,128.2,9.19999999999997));
#76624=CARTESIAN_POINT('',(17.5,129.,9.2));
#76625=CARTESIAN_POINT('Origin',(17.5,129.,1.8));
#76626=CARTESIAN_POINT('',(17.5,129.,1.8));
#76627=CARTESIAN_POINT('',(17.5,129.,1.8));
#76628=CARTESIAN_POINT('',(18.3,129.,1.8));
#76629=CARTESIAN_POINT('',(18.3,129.,1.8));
#76630=CARTESIAN_POINT('',(17.5,129.,1.8));
#76631=CARTESIAN_POINT('Origin',(17.5,128.2,1.80000000000003));
#76632=CARTESIAN_POINT('',(17.5,128.2,1.));
#76633=CARTESIAN_POINT('Origin',(17.5,128.2,1.80000000000003));
#76634=CARTESIAN_POINT('',(18.3,128.2,1.));
#76635=CARTESIAN_POINT('Origin',(18.3,128.2,1.80000000000003));
#76636=CARTESIAN_POINT('',(17.5,128.2,1.));
#76637=CARTESIAN_POINT('Origin',(17.5,11.8,1.));
#76638=CARTESIAN_POINT('',(17.5,11.8,1.));
#76639=CARTESIAN_POINT('',(17.5,11.8,1.));
#76640=CARTESIAN_POINT('',(18.3,11.8,1.));
#76641=CARTESIAN_POINT('',(18.3,11.8,1.));
#76642=CARTESIAN_POINT('',(17.5,11.8,1.));
#76643=CARTESIAN_POINT('Origin',(17.5,11.8,1.8));
#76644=CARTESIAN_POINT('Origin',(17.5,11.8,1.8));
#76645=CARTESIAN_POINT('Origin',(18.3,11.8,1.8));
#76646=CARTESIAN_POINT('Origin',(18.3,70.,5.5));
#76647=CARTESIAN_POINT('Origin',(17.5,70.,5.5));
#76648=CARTESIAN_POINT('',(0.,0.,0.));
#76649=CARTESIAN_POINT('Origin',(19.2,73.67,9.4));
#76650=CARTESIAN_POINT('',(19.2,73.67,9.4));
#76651=CARTESIAN_POINT('',(19.2,73.53,9.4));
#76652=CARTESIAN_POINT('',(19.2,68.835,9.4));
#76653=CARTESIAN_POINT('',(19.1,73.67,9.4));
#76654=CARTESIAN_POINT('',(19.2,73.67,9.4));
#76655=CARTESIAN_POINT('',(19.1,73.53,9.4));
#76656=CARTESIAN_POINT('',(19.1,73.53,9.4));
#76657=CARTESIAN_POINT('',(19.2,73.53,9.4));
#76658=CARTESIAN_POINT('Origin',(19.2,73.67,10.8));
#76659=CARTESIAN_POINT('',(19.2,73.67,10.8));
#76660=CARTESIAN_POINT('',(19.2,73.67,18.55));
#76661=CARTESIAN_POINT('',(19.1,73.67,10.8));
#76662=CARTESIAN_POINT('',(19.2,73.67,10.8));
#76663=CARTESIAN_POINT('',(19.1,73.67,9.4));
#76664=CARTESIAN_POINT('Origin',(19.2,73.53,10.8));
#76665=CARTESIAN_POINT('',(19.2,73.53,10.8));
#76666=CARTESIAN_POINT('',(19.2,68.765,10.8));
#76667=CARTESIAN_POINT('',(19.1,73.53,10.8));
#76668=CARTESIAN_POINT('',(19.2,73.53,10.8));
#76669=CARTESIAN_POINT('',(19.1,73.67,10.8));
#76670=CARTESIAN_POINT('Origin',(19.2,73.53,9.4));
#76671=CARTESIAN_POINT('',(19.2,73.53,17.85));
#76672=CARTESIAN_POINT('',(19.1,73.53,10.8));
#76673=CARTESIAN_POINT('Origin',(19.1,73.6,10.1));
#76674=CARTESIAN_POINT('Origin',(19.2,71.87,9.4));
#76675=CARTESIAN_POINT('',(19.2,71.87,9.4));
#76676=CARTESIAN_POINT('',(19.2,71.73,9.4));
#76677=CARTESIAN_POINT('',(19.2,67.935,9.4));
#76678=CARTESIAN_POINT('',(19.1,71.87,9.4));
#76679=CARTESIAN_POINT('',(19.2,71.87,9.4));
#76680=CARTESIAN_POINT('',(19.1,71.73,9.4));
#76681=CARTESIAN_POINT('',(19.1,71.73,9.4));
#76682=CARTESIAN_POINT('',(19.2,71.73,9.4));
#76683=CARTESIAN_POINT('Origin',(19.2,71.87,10.8));
#76684=CARTESIAN_POINT('',(19.2,71.87,10.8));
#76685=CARTESIAN_POINT('',(19.2,71.87,18.55));
#76686=CARTESIAN_POINT('',(19.1,71.87,10.8));
#76687=CARTESIAN_POINT('',(19.2,71.87,10.8));
#76688=CARTESIAN_POINT('',(19.1,71.87,9.4));
#76689=CARTESIAN_POINT('Origin',(19.2,71.73,10.8));
#76690=CARTESIAN_POINT('',(19.2,71.73,10.8));
#76691=CARTESIAN_POINT('',(19.2,67.865,10.8));
#76692=CARTESIAN_POINT('',(19.1,71.73,10.8));
#76693=CARTESIAN_POINT('',(19.2,71.73,10.8));
#76694=CARTESIAN_POINT('',(19.1,71.87,10.8));
#76695=CARTESIAN_POINT('Origin',(19.2,71.73,9.4));
#76696=CARTESIAN_POINT('',(19.2,71.73,17.85));
#76697=CARTESIAN_POINT('',(19.1,71.73,10.8));
#76698=CARTESIAN_POINT('Origin',(19.1,71.8,10.1));
#76699=CARTESIAN_POINT('Origin',(19.2,65.57,9.4));
#76700=CARTESIAN_POINT('',(19.2,65.57,9.4));
#76701=CARTESIAN_POINT('',(19.2,65.43,9.4));
#76702=CARTESIAN_POINT('',(19.2,64.785,9.4));
#76703=CARTESIAN_POINT('',(19.1,65.57,9.4));
#76704=CARTESIAN_POINT('',(19.2,65.57,9.4));
#76705=CARTESIAN_POINT('',(19.1,65.43,9.4));
#76706=CARTESIAN_POINT('',(19.1,65.43,9.4));
#76707=CARTESIAN_POINT('',(19.2,65.43,9.4));
#76708=CARTESIAN_POINT('Origin',(19.2,65.57,11.6));
#76709=CARTESIAN_POINT('',(19.2,65.57,11.6));
#76710=CARTESIAN_POINT('',(19.2,65.57,18.95));
#76711=CARTESIAN_POINT('',(19.1,65.57,11.6));
#76712=CARTESIAN_POINT('',(19.2,65.57,11.6));
#76713=CARTESIAN_POINT('',(19.1,65.57,9.4));
#76714=CARTESIAN_POINT('Origin',(19.2,65.43,11.6));
#76715=CARTESIAN_POINT('',(19.2,65.43,11.6));
#76716=CARTESIAN_POINT('',(19.2,64.715,11.6));
#76717=CARTESIAN_POINT('',(19.1,65.43,11.6));
#76718=CARTESIAN_POINT('',(19.2,65.43,11.6));
#76719=CARTESIAN_POINT('',(19.1,65.57,11.6));
#76720=CARTESIAN_POINT('Origin',(19.2,65.43,9.4));
#76721=CARTESIAN_POINT('',(19.2,65.43,17.85));
#76722=CARTESIAN_POINT('',(19.1,65.43,11.6));
#76723=CARTESIAN_POINT('Origin',(19.1,65.5,10.5));
#76724=CARTESIAN_POINT('Origin',(19.2,69.17,9.4));
#76725=CARTESIAN_POINT('',(19.2,69.17,9.4));
#76726=CARTESIAN_POINT('',(19.2,69.03,9.4));
#76727=CARTESIAN_POINT('',(19.2,66.585,9.4));
#76728=CARTESIAN_POINT('',(19.1,69.17,9.4));
#76729=CARTESIAN_POINT('',(19.2,69.17,9.4));
#76730=CARTESIAN_POINT('',(19.1,69.03,9.4));
#76731=CARTESIAN_POINT('',(19.1,69.03,9.4));
#76732=CARTESIAN_POINT('',(19.2,69.03,9.4));
#76733=CARTESIAN_POINT('Origin',(19.2,69.17,10.8));
#76734=CARTESIAN_POINT('',(19.2,69.17,10.8));
#76735=CARTESIAN_POINT('',(19.2,69.17,18.55));
#76736=CARTESIAN_POINT('',(19.1,69.17,10.8));
#76737=CARTESIAN_POINT('',(19.2,69.17,10.8));
#76738=CARTESIAN_POINT('',(19.1,69.17,9.4));
#76739=CARTESIAN_POINT('Origin',(19.2,69.03,10.8));
#76740=CARTESIAN_POINT('',(19.2,69.03,10.8));
#76741=CARTESIAN_POINT('',(19.2,66.515,10.8));
#76742=CARTESIAN_POINT('',(19.1,69.03,10.8));
#76743=CARTESIAN_POINT('',(19.2,69.03,10.8));
#76744=CARTESIAN_POINT('',(19.1,69.17,10.8));
#76745=CARTESIAN_POINT('Origin',(19.2,69.03,9.4));
#76746=CARTESIAN_POINT('',(19.2,69.03,17.85));
#76747=CARTESIAN_POINT('',(19.1,69.03,10.8));
#76748=CARTESIAN_POINT('Origin',(19.1,69.1,10.1));
#76749=CARTESIAN_POINT('Origin',(19.2,67.37,9.4));
#76750=CARTESIAN_POINT('',(19.2,67.37,9.4));
#76751=CARTESIAN_POINT('',(19.2,67.23,9.4));
#76752=CARTESIAN_POINT('',(19.2,65.685,9.4));
#76753=CARTESIAN_POINT('',(19.1,67.37,9.4));
#76754=CARTESIAN_POINT('',(19.2,67.37,9.4));
#76755=CARTESIAN_POINT('',(19.1,67.23,9.4));
#76756=CARTESIAN_POINT('',(19.1,67.23,9.4));
#76757=CARTESIAN_POINT('',(19.2,67.23,9.4));
#76758=CARTESIAN_POINT('Origin',(19.2,67.37,10.8));
#76759=CARTESIAN_POINT('',(19.2,67.37,10.8));
#76760=CARTESIAN_POINT('',(19.2,67.37,18.55));
#76761=CARTESIAN_POINT('',(19.1,67.37,10.8));
#76762=CARTESIAN_POINT('',(19.2,67.37,10.8));
#76763=CARTESIAN_POINT('',(19.1,67.37,9.4));
#76764=CARTESIAN_POINT('Origin',(19.2,67.23,10.8));
#76765=CARTESIAN_POINT('',(19.2,67.23,10.8));
#76766=CARTESIAN_POINT('',(19.2,65.615,10.8));
#76767=CARTESIAN_POINT('',(19.1,67.23,10.8));
#76768=CARTESIAN_POINT('',(19.2,67.23,10.8));
#76769=CARTESIAN_POINT('',(19.1,67.37,10.8));
#76770=CARTESIAN_POINT('Origin',(19.2,67.23,9.4));
#76771=CARTESIAN_POINT('',(19.2,67.23,17.85));
#76772=CARTESIAN_POINT('',(19.1,67.23,10.8));
#76773=CARTESIAN_POINT('Origin',(19.1,67.3,10.1));
#76774=CARTESIAN_POINT('Origin',(19.2,66.47,9.4));
#76775=CARTESIAN_POINT('',(19.2,66.47,9.4));
#76776=CARTESIAN_POINT('',(19.2,66.33,9.4));
#76777=CARTESIAN_POINT('',(19.2,65.235,9.4));
#76778=CARTESIAN_POINT('',(19.1,66.47,9.4));
#76779=CARTESIAN_POINT('',(19.2,66.47,9.4));
#76780=CARTESIAN_POINT('',(19.1,66.33,9.4));
#76781=CARTESIAN_POINT('',(19.1,66.33,9.4));
#76782=CARTESIAN_POINT('',(19.2,66.33,9.4));
#76783=CARTESIAN_POINT('Origin',(19.2,66.47,10.8));
#76784=CARTESIAN_POINT('',(19.2,66.47,10.8));
#76785=CARTESIAN_POINT('',(19.2,66.47,18.55));
#76786=CARTESIAN_POINT('',(19.1,66.47,10.8));
#76787=CARTESIAN_POINT('',(19.2,66.47,10.8));
#76788=CARTESIAN_POINT('',(19.1,66.47,9.4));
#76789=CARTESIAN_POINT('Origin',(19.2,66.33,10.8));
#76790=CARTESIAN_POINT('',(19.2,66.33,10.8));
#76791=CARTESIAN_POINT('',(19.2,65.165,10.8));
#76792=CARTESIAN_POINT('',(19.1,66.33,10.8));
#76793=CARTESIAN_POINT('',(19.2,66.33,10.8));
#76794=CARTESIAN_POINT('',(19.1,66.47,10.8));
#76795=CARTESIAN_POINT('Origin',(19.2,66.33,9.4));
#76796=CARTESIAN_POINT('',(19.2,66.33,17.85));
#76797=CARTESIAN_POINT('',(19.1,66.33,10.8));
#76798=CARTESIAN_POINT('Origin',(19.1,66.4,10.1));
#76799=CARTESIAN_POINT('Origin',(19.2,68.27,9.4));
#76800=CARTESIAN_POINT('',(19.2,68.27,9.4));
#76801=CARTESIAN_POINT('',(19.2,68.13,9.4));
#76802=CARTESIAN_POINT('',(19.2,66.135,9.4));
#76803=CARTESIAN_POINT('',(19.1,68.27,9.4));
#76804=CARTESIAN_POINT('',(19.2,68.27,9.4));
#76805=CARTESIAN_POINT('',(19.1,68.13,9.4));
#76806=CARTESIAN_POINT('',(19.1,68.13,9.4));
#76807=CARTESIAN_POINT('',(19.2,68.13,9.4));
#76808=CARTESIAN_POINT('Origin',(19.2,68.27,10.8));
#76809=CARTESIAN_POINT('',(19.2,68.27,10.8));
#76810=CARTESIAN_POINT('',(19.2,68.27,18.55));
#76811=CARTESIAN_POINT('',(19.1,68.27,10.8));
#76812=CARTESIAN_POINT('',(19.2,68.27,10.8));
#76813=CARTESIAN_POINT('',(19.1,68.27,9.4));
#76814=CARTESIAN_POINT('Origin',(19.2,68.13,10.8));
#76815=CARTESIAN_POINT('',(19.2,68.13,10.8));
#76816=CARTESIAN_POINT('',(19.2,66.065,10.8));
#76817=CARTESIAN_POINT('',(19.1,68.13,10.8));
#76818=CARTESIAN_POINT('',(19.2,68.13,10.8));
#76819=CARTESIAN_POINT('',(19.1,68.27,10.8));
#76820=CARTESIAN_POINT('Origin',(19.2,68.13,9.4));
#76821=CARTESIAN_POINT('',(19.2,68.13,17.85));
#76822=CARTESIAN_POINT('',(19.1,68.13,10.8));
#76823=CARTESIAN_POINT('Origin',(19.1,68.2,10.1));
#76824=CARTESIAN_POINT('Origin',(19.2,70.07,9.4));
#76825=CARTESIAN_POINT('',(19.2,70.07,9.4));
#76826=CARTESIAN_POINT('',(19.2,69.93,9.4));
#76827=CARTESIAN_POINT('',(19.2,67.035,9.4));
#76828=CARTESIAN_POINT('',(19.1,70.07,9.4));
#76829=CARTESIAN_POINT('',(19.2,70.07,9.4));
#76830=CARTESIAN_POINT('',(19.1,69.93,9.4));
#76831=CARTESIAN_POINT('',(19.1,69.93,9.4));
#76832=CARTESIAN_POINT('',(19.2,69.93,9.4));
#76833=CARTESIAN_POINT('Origin',(19.2,70.07,11.6));
#76834=CARTESIAN_POINT('',(19.2,70.07,11.6));
#76835=CARTESIAN_POINT('',(19.2,70.07,18.95));
#76836=CARTESIAN_POINT('',(19.1,70.07,11.6));
#76837=CARTESIAN_POINT('',(19.2,70.07,11.6));
#76838=CARTESIAN_POINT('',(19.1,70.07,9.4));
#76839=CARTESIAN_POINT('Origin',(19.2,69.93,11.6));
#76840=CARTESIAN_POINT('',(19.2,69.93,11.6));
#76841=CARTESIAN_POINT('',(19.2,66.965,11.6));
#76842=CARTESIAN_POINT('',(19.1,69.93,11.6));
#76843=CARTESIAN_POINT('',(19.2,69.93,11.6));
#76844=CARTESIAN_POINT('',(19.1,70.07,11.6));
#76845=CARTESIAN_POINT('Origin',(19.2,69.93,9.4));
#76846=CARTESIAN_POINT('',(19.2,69.93,17.85));
#76847=CARTESIAN_POINT('',(19.1,69.93,11.6));
#76848=CARTESIAN_POINT('Origin',(19.1,70.,10.5));
#76849=CARTESIAN_POINT('Origin',(19.2,70.97,9.4));
#76850=CARTESIAN_POINT('',(19.2,70.97,9.4));
#76851=CARTESIAN_POINT('',(19.2,70.83,9.4));
#76852=CARTESIAN_POINT('',(19.2,67.485,9.4));
#76853=CARTESIAN_POINT('',(19.1,70.97,9.4));
#76854=CARTESIAN_POINT('',(19.2,70.97,9.4));
#76855=CARTESIAN_POINT('',(19.1,70.83,9.4));
#76856=CARTESIAN_POINT('',(19.1,70.83,9.4));
#76857=CARTESIAN_POINT('',(19.2,70.83,9.4));
#76858=CARTESIAN_POINT('Origin',(19.2,70.97,10.8));
#76859=CARTESIAN_POINT('',(19.2,70.97,10.8));
#76860=CARTESIAN_POINT('',(19.2,70.97,18.55));
#76861=CARTESIAN_POINT('',(19.1,70.97,10.8));
#76862=CARTESIAN_POINT('',(19.2,70.97,10.8));
#76863=CARTESIAN_POINT('',(19.1,70.97,9.4));
#76864=CARTESIAN_POINT('Origin',(19.2,70.83,10.8));
#76865=CARTESIAN_POINT('',(19.2,70.83,10.8));
#76866=CARTESIAN_POINT('',(19.2,67.415,10.8));
#76867=CARTESIAN_POINT('',(19.1,70.83,10.8));
#76868=CARTESIAN_POINT('',(19.2,70.83,10.8));
#76869=CARTESIAN_POINT('',(19.1,70.97,10.8));
#76870=CARTESIAN_POINT('Origin',(19.2,70.83,9.4));
#76871=CARTESIAN_POINT('',(19.2,70.83,17.85));
#76872=CARTESIAN_POINT('',(19.1,70.83,10.8));
#76873=CARTESIAN_POINT('Origin',(19.1,70.9,10.1));
#76874=CARTESIAN_POINT('Origin',(19.2,72.77,9.4));
#76875=CARTESIAN_POINT('',(19.2,72.77,9.4));
#76876=CARTESIAN_POINT('',(19.2,72.63,9.4));
#76877=CARTESIAN_POINT('',(19.2,68.385,9.4));
#76878=CARTESIAN_POINT('',(19.1,72.77,9.4));
#76879=CARTESIAN_POINT('',(19.2,72.77,9.4));
#76880=CARTESIAN_POINT('',(19.1,72.63,9.4));
#76881=CARTESIAN_POINT('',(19.1,72.63,9.4));
#76882=CARTESIAN_POINT('',(19.2,72.63,9.4));
#76883=CARTESIAN_POINT('Origin',(19.2,72.77,10.8));
#76884=CARTESIAN_POINT('',(19.2,72.77,10.8));
#76885=CARTESIAN_POINT('',(19.2,72.77,18.55));
#76886=CARTESIAN_POINT('',(19.1,72.77,10.8));
#76887=CARTESIAN_POINT('',(19.2,72.77,10.8));
#76888=CARTESIAN_POINT('',(19.1,72.77,9.4));
#76889=CARTESIAN_POINT('Origin',(19.2,72.63,10.8));
#76890=CARTESIAN_POINT('',(19.2,72.63,10.8));
#76891=CARTESIAN_POINT('',(19.2,68.315,10.8));
#76892=CARTESIAN_POINT('',(19.1,72.63,10.8));
#76893=CARTESIAN_POINT('',(19.2,72.63,10.8));
#76894=CARTESIAN_POINT('',(19.1,72.77,10.8));
#76895=CARTESIAN_POINT('Origin',(19.2,72.63,9.4));
#76896=CARTESIAN_POINT('',(19.2,72.63,17.85));
#76897=CARTESIAN_POINT('',(19.1,72.63,10.8));
#76898=CARTESIAN_POINT('Origin',(19.1,72.7,10.1));
#76899=CARTESIAN_POINT('Origin',(19.2,74.57,9.4));
#76900=CARTESIAN_POINT('',(19.2,74.57,9.4));
#76901=CARTESIAN_POINT('',(19.2,74.43,9.4));
#76902=CARTESIAN_POINT('',(19.2,69.285,9.4));
#76903=CARTESIAN_POINT('',(19.1,74.57,9.4));
#76904=CARTESIAN_POINT('',(19.2,74.57,9.4));
#76905=CARTESIAN_POINT('',(19.1,74.43,9.4));
#76906=CARTESIAN_POINT('',(19.1,74.43,9.4));
#76907=CARTESIAN_POINT('',(19.2,74.43,9.4));
#76908=CARTESIAN_POINT('Origin',(19.2,74.57,11.6));
#76909=CARTESIAN_POINT('',(19.2,74.57,11.6));
#76910=CARTESIAN_POINT('',(19.2,74.57,18.95));
#76911=CARTESIAN_POINT('',(19.1,74.57,11.6));
#76912=CARTESIAN_POINT('',(19.2,74.57,11.6));
#76913=CARTESIAN_POINT('',(19.1,74.57,9.4));
#76914=CARTESIAN_POINT('Origin',(19.2,74.43,11.6));
#76915=CARTESIAN_POINT('',(19.2,74.43,11.6));
#76916=CARTESIAN_POINT('',(19.2,69.215,11.6));
#76917=CARTESIAN_POINT('',(19.1,74.43,11.6));
#76918=CARTESIAN_POINT('',(19.2,74.43,11.6));
#76919=CARTESIAN_POINT('',(19.1,74.57,11.6));
#76920=CARTESIAN_POINT('Origin',(19.2,74.43,9.4));
#76921=CARTESIAN_POINT('',(19.2,74.43,17.85));
#76922=CARTESIAN_POINT('',(19.1,74.43,11.6));
#76923=CARTESIAN_POINT('Origin',(19.1,74.5,10.5));
#76924=CARTESIAN_POINT('Origin',(12.5,67.,21.5));
#76925=CARTESIAN_POINT('',(12.5,67.,22.6));
#76926=CARTESIAN_POINT('Origin',(12.5,67.,21.5));
#76927=CARTESIAN_POINT('',(13.3,67.,22.6));
#76928=CARTESIAN_POINT('',(12.5,67.,22.6));
#76929=CARTESIAN_POINT('Origin',(13.3,67.,21.5));
#76930=CARTESIAN_POINT('Origin',(12.5,73.,21.5));
#76931=CARTESIAN_POINT('',(12.5,73.,22.6));
#76932=CARTESIAN_POINT('Origin',(12.5,73.,21.5));
#76933=CARTESIAN_POINT('',(13.3,73.,22.6));
#76934=CARTESIAN_POINT('',(12.5,73.,22.6));
#76935=CARTESIAN_POINT('Origin',(13.3,73.,21.5));
#76936=CARTESIAN_POINT('Origin',(12.5,64.,17.));
#76937=CARTESIAN_POINT('',(12.5,64.,26.3));
#76938=CARTESIAN_POINT('',(12.5,64.,17.));
#76939=CARTESIAN_POINT('',(12.5,64.,26.3));
#76940=CARTESIAN_POINT('',(12.5,76.,26.3));
#76941=CARTESIAN_POINT('',(12.5,64.,26.3));
#76942=CARTESIAN_POINT('',(12.5,76.,17.));
#76943=CARTESIAN_POINT('',(12.5,76.,26.3));
#76944=CARTESIAN_POINT('',(12.5,64.,17.));
#76945=CARTESIAN_POINT('Origin',(13.3,64.,17.));
#76946=CARTESIAN_POINT('',(13.3,64.,17.));
#76947=CARTESIAN_POINT('',(12.5,64.,17.));
#76948=CARTESIAN_POINT('',(13.3,76.,17.));
#76949=CARTESIAN_POINT('',(12.5,76.,17.));
#76950=CARTESIAN_POINT('',(13.3,64.,17.));
#76951=CARTESIAN_POINT('Origin',(13.3,64.,25.5));
#76952=CARTESIAN_POINT('',(13.3,64.,25.5));
#76953=CARTESIAN_POINT('',(13.3,64.,17.));
#76954=CARTESIAN_POINT('',(13.3,76.,25.5));
#76955=CARTESIAN_POINT('',(13.3,76.,17.));
#76956=CARTESIAN_POINT('',(13.3,64.,25.5));
#76957=CARTESIAN_POINT('Origin',(18.4,64.,25.5));
#76958=CARTESIAN_POINT('',(18.4,64.,25.5));
#76959=CARTESIAN_POINT('',(13.3,64.,25.5));
#76960=CARTESIAN_POINT('',(18.4,76.,25.5));
#76961=CARTESIAN_POINT('',(13.3,76.,25.5));
#76962=CARTESIAN_POINT('',(18.4,64.,25.5));
#76963=CARTESIAN_POINT('Origin',(18.4,64.,9.));
#76964=CARTESIAN_POINT('',(18.4,64.,9.));
#76965=CARTESIAN_POINT('',(18.4,64.,25.5));
#76966=CARTESIAN_POINT('',(18.4,76.,9.));
#76967=CARTESIAN_POINT('',(18.4,76.,25.5));
#76968=CARTESIAN_POINT('',(18.4,64.,9.));
#76969=CARTESIAN_POINT('Origin',(19.2,64.,9.));
#76970=CARTESIAN_POINT('',(19.2,64.,9.));
#76971=CARTESIAN_POINT('',(18.4,64.,9.));
#76972=CARTESIAN_POINT('',(19.2,76.,9.));
#76973=CARTESIAN_POINT('',(18.4,76.,9.));
#76974=CARTESIAN_POINT('',(19.2,64.,9.));
#76975=CARTESIAN_POINT('Origin',(19.2,64.,26.3));
#76976=CARTESIAN_POINT('',(19.2,64.,26.3));
#76977=CARTESIAN_POINT('',(19.2,64.,9.));
#76978=CARTESIAN_POINT('',(19.2,76.,26.3));
#76979=CARTESIAN_POINT('',(19.2,76.,9.));
#76980=CARTESIAN_POINT('',(19.2,64.,26.3));
#76981=CARTESIAN_POINT('Origin',(12.5,64.,26.3));
#76982=CARTESIAN_POINT('',(19.2,64.,26.3));
#76983=CARTESIAN_POINT('',(19.2,76.,26.3));
#76984=CARTESIAN_POINT('Origin',(15.85,76.,17.65));
#76985=CARTESIAN_POINT('Origin',(15.85,64.,17.65));
#76986=CARTESIAN_POINT('',(0.,0.,0.));
#76987=CARTESIAN_POINT('Origin',(10.,0.15,11.));
#76988=CARTESIAN_POINT('',(7.76393202250021,0.3,13.));
#76989=CARTESIAN_POINT('',(7.37511905031866,0.,13.));
#76990=CARTESIAN_POINT('Ctrl Pts',(7.76393202250021,0.3,13.));
#76991=CARTESIAN_POINT('Ctrl Pts',(7.57878298812804,0.16199805772513,13.));
#76992=CARTESIAN_POINT('Ctrl Pts',(7.37511905031866,3.46944695195361E-16,
13.));
#76993=CARTESIAN_POINT('',(12.6248809496813,0.,13.));
#76994=CARTESIAN_POINT('Origin',(10.,0.,11.));
#76995=CARTESIAN_POINT('',(12.2360679774998,0.3,13.));
#76996=CARTESIAN_POINT('Ctrl Pts',(12.6248809496813,3.46944695195361E-16,
13.));
#76997=CARTESIAN_POINT('Ctrl Pts',(12.421217011872,0.161998057725131,13.));
#76998=CARTESIAN_POINT('Ctrl Pts',(12.2360679774998,0.3,13.));
#76999=CARTESIAN_POINT('Origin',(10.,0.3,11.));
#77000=CARTESIAN_POINT('Origin',(0.,0.,0.800000000000001));
#77001=CARTESIAN_POINT('',(-7.37511905031866,0.,13.));
#77002=CARTESIAN_POINT('',(17.5,0.,13.));
#77003=CARTESIAN_POINT('',(-12.6248809496813,0.,13.));
#77004=CARTESIAN_POINT('Origin',(-10.,0.,11.));
#77005=CARTESIAN_POINT('',(-17.5,0.,13.));
#77006=CARTESIAN_POINT('',(17.5,0.,13.));
#77007=CARTESIAN_POINT('',(-17.5,0.,-11.4));
#77008=CARTESIAN_POINT('',(-17.5,0.,13.));
#77009=CARTESIAN_POINT('',(17.5,0.,-11.4));
#77010=CARTESIAN_POINT('',(-17.5,0.,-11.4));
#77011=CARTESIAN_POINT('',(17.5,0.,13.));
#77012=CARTESIAN_POINT('',(17.5,0.,-11.4));
#77013=CARTESIAN_POINT('',(17.5,0.,13.));
#77014=CARTESIAN_POINT('',(12.25,0.,-5.));
#77015=CARTESIAN_POINT('',(12.25,0.,-9.));
#77016=CARTESIAN_POINT('',(12.25,0.,-4.1));
#77017=CARTESIAN_POINT('',(7.75,0.,-9.));
#77018=CARTESIAN_POINT('Origin',(10.,0.,-9.));
#77019=CARTESIAN_POINT('',(7.75,0.,-5.));
#77020=CARTESIAN_POINT('',(7.75,0.,-2.1));
#77021=CARTESIAN_POINT('Origin',(10.,0.,-5.));
#77022=CARTESIAN_POINT('',(-7.75,0.,-5.));
#77023=CARTESIAN_POINT('',(-7.75,0.,-9.));
#77024=CARTESIAN_POINT('',(-7.75,0.,-4.1));
#77025=CARTESIAN_POINT('',(-12.25,0.,-9.));
#77026=CARTESIAN_POINT('Origin',(-10.,0.,-9.));
#77027=CARTESIAN_POINT('',(-12.25,0.,-5.));
#77028=CARTESIAN_POINT('',(-12.25,0.,-2.1));
#77029=CARTESIAN_POINT('Origin',(-10.,0.,-5.));
#77030=CARTESIAN_POINT('Origin',(-10.,0.15,11.));
#77031=CARTESIAN_POINT('',(-12.2360679774998,0.3,13.));
#77032=CARTESIAN_POINT('Ctrl Pts',(-12.2360679774998,0.3,13.));
#77033=CARTESIAN_POINT('Ctrl Pts',(-12.421217011872,0.161998057725133,13.));
#77034=CARTESIAN_POINT('Ctrl Pts',(-12.6248809496813,3.46944695195361E-16,
13.));
#77035=CARTESIAN_POINT('',(-7.76393202250021,0.3,13.));
#77036=CARTESIAN_POINT('Ctrl Pts',(-7.37511905031866,3.46944695195361E-16,
13.));
#77037=CARTESIAN_POINT('Ctrl Pts',(-7.57878298812804,0.161998057725129,
13.));
#77038=CARTESIAN_POINT('Ctrl Pts',(-7.76393202250021,0.3,13.));
#77039=CARTESIAN_POINT('Origin',(-10.,0.3,11.));
#77040=CARTESIAN_POINT('Origin',(-17.5,0.,13.));
#77041=CARTESIAN_POINT('',(17.5,9.5,13.));
#77042=CARTESIAN_POINT('',(17.5,0.,13.));
#77043=CARTESIAN_POINT('',(-17.5,9.5,13.));
#77044=CARTESIAN_POINT('',(-8.75,9.5,13.));
#77045=CARTESIAN_POINT('',(-17.5,0.,13.));
#77046=CARTESIAN_POINT('',(-12.2360679774998,3.5,13.));
#77047=CARTESIAN_POINT('',(-12.2360679774998,0.,13.));
#77048=CARTESIAN_POINT('',(-7.76393202250021,3.5,13.));
#77049=CARTESIAN_POINT('',(-13.75,3.5,13.));
#77050=CARTESIAN_POINT('',(-7.76393202250021,0.,13.));
#77051=CARTESIAN_POINT('',(7.76393202250021,3.5,13.));
#77052=CARTESIAN_POINT('',(7.76393202250021,0.,13.));
#77053=CARTESIAN_POINT('',(12.2360679774998,3.5,13.));
#77054=CARTESIAN_POINT('',(-3.75,3.5,13.));
#77055=CARTESIAN_POINT('',(12.2360679774998,0.,13.));
#77056=CARTESIAN_POINT('Origin',(-10.,0.,11.));
#77057=CARTESIAN_POINT('Origin',(-10.,3.5,11.));
#77058=CARTESIAN_POINT('Origin',(-10.,3.5,11.));
#77059=CARTESIAN_POINT('',(-11.7,3.5,11.));
#77060=CARTESIAN_POINT('Origin',(-10.,3.5,11.));
#77061=CARTESIAN_POINT('Origin',(10.,0.,11.));
#77062=CARTESIAN_POINT('Origin',(10.,3.5,11.));
#77063=CARTESIAN_POINT('Origin',(10.,3.5,11.));
#77064=CARTESIAN_POINT('',(8.3,3.5,11.));
#77065=CARTESIAN_POINT('Origin',(10.,3.5,11.));
#77066=CARTESIAN_POINT('Origin',(-10.,0.,11.));
#77067=CARTESIAN_POINT('',(-11.7,10.,11.));
#77068=CARTESIAN_POINT('',(-11.7,0.,11.));
#77069=CARTESIAN_POINT('',(-10.8,10.,12.5));
#77070=CARTESIAN_POINT('Origin',(-10.,10.,11.));
#77071=CARTESIAN_POINT('',(-9.2,10.,12.5));
#77072=CARTESIAN_POINT('Origin',(-10.,11.5,11.));
#77073=CARTESIAN_POINT('Origin',(-10.,10.,11.));
#77074=CARTESIAN_POINT('Origin',(10.,0.,11.));
#77075=CARTESIAN_POINT('',(8.3,10.,11.));
#77076=CARTESIAN_POINT('',(8.3,0.,11.));
#77077=CARTESIAN_POINT('',(9.2,10.,12.5));
#77078=CARTESIAN_POINT('Origin',(10.,10.,11.));
#77079=CARTESIAN_POINT('',(10.8,10.,12.5));
#77080=CARTESIAN_POINT('Origin',(10.,11.5,11.));
#77081=CARTESIAN_POINT('Origin',(10.,10.,11.));
#77082=CARTESIAN_POINT('Origin',(-8.75,9.75,12.75));
#77083=CARTESIAN_POINT('',(-17.,10.,12.5));
#77084=CARTESIAN_POINT('',(-8.75,10.,12.5));
#77085=CARTESIAN_POINT('',(-17.,10.,12.5));
#77086=CARTESIAN_POINT('',(17.,10.,12.5));
#77087=CARTESIAN_POINT('',(17.,10.,12.5));
#77088=CARTESIAN_POINT('',(-8.75,10.,12.5));
#77089=CARTESIAN_POINT('',(-8.75,10.,12.5));
#77090=CARTESIAN_POINT('Origin',(-7.75,10.,-9.));
#77091=CARTESIAN_POINT('',(-7.75,10.,-9.));
#77092=CARTESIAN_POINT('',(-7.75,10.,-5.));
#77093=CARTESIAN_POINT('',(-7.75,10.,-4.1));
#77094=CARTESIAN_POINT('',(-7.75,10.,-9.));
#77095=CARTESIAN_POINT('',(-7.75,10.,-5.));
#77096=CARTESIAN_POINT('Origin',(-10.,10.,-9.));
#77097=CARTESIAN_POINT('',(-11.2051970793194,10.,-10.9));
#77098=CARTESIAN_POINT('',(-8.79480292068061,10.,-10.9));
#77099=CARTESIAN_POINT('Origin',(-10.,11.9,-9.));
#77100=CARTESIAN_POINT('',(-12.25,10.,-9.));
#77101=CARTESIAN_POINT('Origin',(-10.,10.,-9.));
#77102=CARTESIAN_POINT('',(-12.25,10.,-9.));
#77103=CARTESIAN_POINT('Origin',(-10.,10.,-9.));
#77104=CARTESIAN_POINT('Origin',(-12.25,10.,-5.));
#77105=CARTESIAN_POINT('',(-12.25,10.,-5.));
#77106=CARTESIAN_POINT('',(-12.25,10.,-2.1));
#77107=CARTESIAN_POINT('',(-12.25,10.,-5.));
#77108=CARTESIAN_POINT('Origin',(-10.,10.,-5.));
#77109=CARTESIAN_POINT('Origin',(-10.,10.,-5.));
#77110=CARTESIAN_POINT('Origin',(12.25,10.,-9.));
#77111=CARTESIAN_POINT('',(12.25,10.,-9.));
#77112=CARTESIAN_POINT('',(12.25,10.,-5.));
#77113=CARTESIAN_POINT('',(12.25,10.,-4.1));
#77114=CARTESIAN_POINT('',(12.25,10.,-9.));
#77115=CARTESIAN_POINT('',(12.25,10.,-5.));
#77116=CARTESIAN_POINT('Origin',(10.,10.,-9.));
#77117=CARTESIAN_POINT('',(8.79480292068061,10.,-10.9));
#77118=CARTESIAN_POINT('',(11.2051970793194,10.,-10.9));
#77119=CARTESIAN_POINT('Origin',(10.,11.9,-9.));
#77120=CARTESIAN_POINT('',(7.75,10.,-9.));
#77121=CARTESIAN_POINT('Origin',(10.,10.,-9.));
#77122=CARTESIAN_POINT('',(7.75,10.,-9.));
#77123=CARTESIAN_POINT('Origin',(10.,10.,-9.));
#77124=CARTESIAN_POINT('Origin',(7.75,10.,-5.));
#77125=CARTESIAN_POINT('',(7.75,10.,-5.));
#77126=CARTESIAN_POINT('',(7.75,10.,-2.1));
#77127=CARTESIAN_POINT('',(7.75,10.,-5.));
#77128=CARTESIAN_POINT('Origin',(10.,10.,-5.));
#77129=CARTESIAN_POINT('Origin',(10.,10.,-5.));
#77130=CARTESIAN_POINT('Origin',(0.,10.,0.800000000000001));
#77131=CARTESIAN_POINT('',(17.,10.,-10.9));
#77132=CARTESIAN_POINT('',(17.,10.,6.9));
#77133=CARTESIAN_POINT('',(8.75,10.,-10.9));
#77134=CARTESIAN_POINT('',(8.75,10.,-10.9));
#77135=CARTESIAN_POINT('',(-17.,10.,-10.9));
#77136=CARTESIAN_POINT('',(8.75,10.,-10.9));
#77137=CARTESIAN_POINT('',(-17.,10.,-5.3));
#77138=CARTESIAN_POINT('Origin',(17.25,9.75,6.9));
#77139=CARTESIAN_POINT('',(17.5,9.5,-11.4));
#77140=CARTESIAN_POINT('',(17.5,9.5,6.9));
#77141=CARTESIAN_POINT('',(17.,10.,-10.9));
#77142=CARTESIAN_POINT('Origin',(-17.25,9.75,-5.3));
#77143=CARTESIAN_POINT('',(-17.5,9.5,-11.4));
#77144=CARTESIAN_POINT('',(-17.,10.,-10.9));
#77145=CARTESIAN_POINT('',(-17.5,9.5,-5.3));
#77146=CARTESIAN_POINT('Origin',(8.75,9.75,-11.15));
#77147=CARTESIAN_POINT('',(8.75,9.5,-11.4));
#77148=CARTESIAN_POINT('Origin',(17.5,0.,-11.4));
#77149=CARTESIAN_POINT('',(17.5,0.,-11.4));
#77150=CARTESIAN_POINT('',(-17.5,0.,-11.4));
#77151=CARTESIAN_POINT('Origin',(17.5,0.,13.));
#77152=CARTESIAN_POINT('Origin',(-17.5,0.,-11.4));
#77153=CARTESIAN_POINT('',(0.,0.,0.));
#77154=CARTESIAN_POINT('Origin',(4.2,139.,13.3));
#77155=CARTESIAN_POINT('',(2.2251969548064,137.5365,13.2999999724982));
#77156=CARTESIAN_POINT('',(2.15284495415709,137.536500503216,13.3012136364406));
#77157=CARTESIAN_POINT('',(4.2,137.5365,13.3));
#77158=CARTESIAN_POINT('',(2.0641830960939,139.63445579128,14.6190127185149));
#77159=CARTESIAN_POINT('Ctrl Pts',(2.06484487113285,139.634380960677,14.6188605107176));
#77160=CARTESIAN_POINT('Ctrl Pts',(2.07154330550746,139.516436019972,14.6755928369821));
#77161=CARTESIAN_POINT('Ctrl Pts',(2.07762498273557,139.391404855929,14.7162526547379));
#77162=CARTESIAN_POINT('Ctrl Pts',(2.08649714863426,139.216238221626,14.7482044865399));
#77163=CARTESIAN_POINT('Ctrl Pts',(2.08889178538834,139.169476945985,14.7544181785645));
#77164=CARTESIAN_POINT('Ctrl Pts',(2.09231151530127,139.104262707784,14.7598960496728));
#77165=CARTESIAN_POINT('Ctrl Pts',(2.0932777214869,139.085999063756,14.7610856612976));
#77166=CARTESIAN_POINT('Ctrl Pts',(2.09497000815552,139.054327780598,14.7625527123752));
#77167=CARTESIAN_POINT('Ctrl Pts',(2.09569109521671,139.040929560602,14.7629889606482));
#77168=CARTESIAN_POINT('Ctrl Pts',(2.09719470100381,139.013204014515,14.7635105533602));
#77169=CARTESIAN_POINT('Ctrl Pts',(2.09797795278032,138.998877684261,14.7635696792124));
#77170=CARTESIAN_POINT('Ctrl Pts',(2.10004847387981,138.961322163813,14.7631732683632));
#77171=CARTESIAN_POINT('Ctrl Pts',(2.10134607908924,138.938101320443,14.7623749368849));
#77172=CARTESIAN_POINT('Ctrl Pts',(2.10859075663927,138.810212841032,14.7549267336709));
#77173=CARTESIAN_POINT('Ctrl Pts',(2.11486128108125,138.706487368182,14.7375936245252));
#77174=CARTESIAN_POINT('Ctrl Pts',(2.12411026253069,138.558087782332,14.6960558892612));
#77175=CARTESIAN_POINT('Ctrl Pts',(2.12705998570955,138.511352950434,14.6803922987276));
#77176=CARTESIAN_POINT('Ctrl Pts',(2.13161267157336,138.438928683095,14.6519784229804));
#77177=CARTESIAN_POINT('Ctrl Pts',(2.13325897783698,138.412670772443,14.6407800921261));
#77178=CARTESIAN_POINT('Ctrl Pts',(2.13547313520369,138.377006577717,14.6243212348215));
#77179=CARTESIAN_POINT('Ctrl Pts',(2.13607302496145,138.367306999997,14.6197147868878));
#77180=CARTESIAN_POINT('Ctrl Pts',(2.13708688600052,138.35083225505,14.6116673391423));
#77181=CARTESIAN_POINT('Ctrl Pts',(2.13750388562067,138.34403167401,14.6082796086849));
#77182=CARTESIAN_POINT('Ctrl Pts',(2.13839379691369,138.329459608557,14.6008782900398));
#77183=CARTESIAN_POINT('Ctrl Pts',(2.13886569620043,138.32169726621,14.5968477748556));
#77184=CARTESIAN_POINT('Ctrl Pts',(2.14022664500463,138.299229529139,14.5849247132341));
#77185=CARTESIAN_POINT('Ctrl Pts',(2.141105259426,138.284622015765,14.576849700171));
#77186=CARTESIAN_POINT('Ctrl Pts',(2.14568093691103,138.208274242917,14.5329231190416));
#77187=CARTESIAN_POINT('Ctrl Pts',(2.14917413717831,138.149075567429,14.4928363322984));
#77188=CARTESIAN_POINT('Ctrl Pts',(2.15615714477518,138.036536945863,14.4039717549171));
#77189=CARTESIAN_POINT('Ctrl Pts',(2.15963902309474,137.983408114186,14.355251232627));
#77190=CARTESIAN_POINT('Ctrl Pts',(2.16542259001683,137.904256023087,14.2711189460665));
#77191=CARTESIAN_POINT('Ctrl Pts',(2.16764235849417,137.875861400932,14.2381038600084));
#77192=CARTESIAN_POINT('Ctrl Pts',(2.17085156010389,137.837997571907,14.189887014097));
#77193=CARTESIAN_POINT('Ctrl Pts',(2.17179187459467,137.827269832423,14.1757011239281));
#77194=CARTESIAN_POINT('Ctrl Pts',(2.17345236454698,137.808982294968,14.1505796158621));
#77195=CARTESIAN_POINT('Ctrl Pts',(2.17416803256024,137.801307917839,14.1397297975067));
#77196=CARTESIAN_POINT('Ctrl Pts',(2.17567344767817,137.78560227226,14.1168715144026));
#77197=CARTESIAN_POINT('Ctrl Pts',(2.17646413874395,137.77759894815,14.1048456744472));
#77198=CARTESIAN_POINT('Ctrl Pts',(2.1785851962511,137.756786226949,14.0725456746905));
#77199=CARTESIAN_POINT('Ctrl Pts',(2.17992696594011,137.744295305875,14.0520724240382));
#77200=CARTESIAN_POINT('Ctrl Pts',(2.18788516733776,137.674136401513,13.9304544687656));
#77201=CARTESIAN_POINT('Ctrl Pts',(2.19491253895104,137.628208659697,13.8230369797022));
#77202=CARTESIAN_POINT('Ctrl Pts',(2.20453657899678,137.583225008379,13.6694411294335));
#77203=CARTESIAN_POINT('Ctrl Pts',(2.20714717172512,137.572834993177,13.6270145557349));
#77204=CARTESIAN_POINT('Ctrl Pts',(2.21124977622621,137.559208651109,13.5581771932772));
#77205=CARTESIAN_POINT('Ctrl Pts',(2.21277752855814,137.554767735982,13.5320324223786));
#77206=CARTESIAN_POINT('Ctrl Pts',(2.21485710674279,137.549579562116,13.4955008800206));
#77207=CARTESIAN_POINT('Ctrl Pts',(2.21543707823911,137.548229115306,13.4852062414051));
#77208=CARTESIAN_POINT('Ctrl Pts',(2.21642385112219,137.546096418386,13.4674882740937));
#77209=CARTESIAN_POINT('Ctrl Pts',(2.21683344472635,137.545261207564,13.4600718632937));
#77210=CARTESIAN_POINT('Ctrl Pts',(2.21771407477505,137.543574175518,13.4439859076296));
#77211=CARTESIAN_POINT('Ctrl Pts',(2.21818400497777,137.542742965998,13.4353147014655));
#77212=CARTESIAN_POINT('Ctrl Pts',(2.21952396927374,137.540575546037,13.4103604037126));
#77213=CARTESIAN_POINT('Ctrl Pts',(2.22038400700859,137.539434464801,13.3940612374598));
#77214=CARTESIAN_POINT('Ctrl Pts',(2.22258002585803,137.537188697747,13.3518461985471));
#77215=CARTESIAN_POINT('Ctrl Pts',(2.22389800731999,137.536499999513,13.3259217714187));
#77216=CARTESIAN_POINT('Ctrl Pts',(2.22519695480639,137.5365,13.2999999724982));
#77217=CARTESIAN_POINT('',(2.0635,138.365992905425,14.6190402776368));
#77218=CARTESIAN_POINT('Origin',(2.0635,139.,13.3));
#77219=CARTESIAN_POINT('Ctrl Pts',(2.0635,138.365992905425,14.6190402776369));
#77220=CARTESIAN_POINT('Ctrl Pts',(2.0665728961224,138.315057965225,14.5945579976066));
#77221=CARTESIAN_POINT('Ctrl Pts',(2.0696457922448,138.265498495672,14.5671001288649));
#77222=CARTESIAN_POINT('Ctrl Pts',(2.0727186883672,138.217668754599,14.5368468265996));
#77223=CARTESIAN_POINT('Ctrl Pts',(2.07578984658353,138.169866064098,14.5066106343814));
#77224=CARTESIAN_POINT('Ctrl Pts',(2.07886100479987,138.123791580139,14.4735824089652));
#77225=CARTESIAN_POINT('Ctrl Pts',(2.08193216301621,138.079773340259,14.4379873218545));
#77226=CARTESIAN_POINT('Ctrl Pts',(2.08500244800625,138.035767616141,14.4024023555399));
#77227=CARTESIAN_POINT('Ctrl Pts',(2.08807273299629,137.993817360905,14.3642522881152));
#77228=CARTESIAN_POINT('Ctrl Pts',(2.09114301798633,137.95421850133,14.3238033536967));
#77229=CARTESIAN_POINT('Ctrl Pts',(2.09421341287704,137.914618224317,14.2833529714109));
#77230=CARTESIAN_POINT('Ctrl Pts',(2.09728380776776,137.877369856597,14.2406039136272));
#77231=CARTESIAN_POINT('Ctrl Pts',(2.10035420265847,137.842731963572,14.1958587733915));
#77232=CARTESIAN_POINT('Ctrl Pts',(2.10342569040786,137.808081741735,14.1510977068281));
#77233=CARTESIAN_POINT('Ctrl Pts',(2.10649717815726,137.776044142247,14.1043395398346));
#77234=CARTESIAN_POINT('Ctrl Pts',(2.10956866590665,137.74683581807,14.0559178415192));
#77235=CARTESIAN_POINT('Ctrl Pts',(2.1126447961947,137.717583345654,14.0074229540446));
#77236=CARTESIAN_POINT('Ctrl Pts',(2.11572092648275,137.691168941285,13.9572599420295));
#77237=CARTESIAN_POINT('Ctrl Pts',(2.1187970567708,137.66776399032,13.9057883000785));
#77238=CARTESIAN_POINT('Ctrl Pts',(2.12187565596135,137.644340254539,13.854275346982));
#77239=CARTESIAN_POINT('Ctrl Pts',(2.12495425515191,137.623930962426,13.8014521348082));
#77240=CARTESIAN_POINT('Ctrl Pts',(2.12803285434246,137.606658688541,13.7476965934434));
#77241=CARTESIAN_POINT('Ctrl Pts',(2.13111793264504,137.589350064032,13.6938279200492));
#77242=CARTESIAN_POINT('Ctrl Pts',(2.13420301094762,137.575191770299,13.6390234789101));
#77243=CARTESIAN_POINT('Ctrl Pts',(2.13728808925019,137.5642558315,13.5836739900301));
#77244=CARTESIAN_POINT('Ctrl Pts',(2.13910859425859,137.557802532945,13.551012251223));
#77245=CARTESIAN_POINT('Ctrl Pts',(2.14092909926698,137.552470335605,13.5181608773554));
#77246=CARTESIAN_POINT('Ctrl Pts',(2.14274960427537,137.548265548371,13.4852007882095));
#77247=CARTESIAN_POINT('Ctrl Pts',(2.14611472090261,137.540493199836,13.4242756363922));
#77248=CARTESIAN_POINT('Ctrl Pts',(2.14947983752985,137.536551593288,13.3628221147701));
#77249=CARTESIAN_POINT('Ctrl Pts',(2.15284495415709,137.536500503216,13.3012136364406));
#77250=CARTESIAN_POINT('Origin',(4.2,139.,13.3));
#77251=CARTESIAN_POINT('',(2.72330048309449,137.536992130936,13.300479477908));
#77252=CARTESIAN_POINT('',(2.65378340881734,137.537042726446,13.3005506582616));
#77253=CARTESIAN_POINT('',(4.2,137.5365,13.3));
#77254=CARTESIAN_POINT('Ctrl Pts',(2.22519695480639,137.5365,13.2999999724982));
#77255=CARTESIAN_POINT('Ctrl Pts',(2.22748597883763,137.536500000858,13.2543202038524));
#77256=CARTESIAN_POINT('Ctrl Pts',(2.22971638608312,137.538638685949,13.2086486214609));
#77257=CARTESIAN_POINT('Ctrl Pts',(2.23545370680436,137.549673160254,13.0911733936797));
#77258=CARTESIAN_POINT('Ctrl Pts',(2.23894358657392,137.56175428192,13.0198120653719));
#77259=CARTESIAN_POINT('Ctrl Pts',(2.24473778427457,137.589490539063,12.907323702418));
#77260=CARTESIAN_POINT('Ctrl Pts',(2.24695836509237,137.601808176735,12.865499360933));
#77261=CARTESIAN_POINT('Ctrl Pts',(2.25016330812179,137.621720741502,12.8075660116011));
#77262=CARTESIAN_POINT('Ctrl Pts',(2.25109779072504,137.627771127863,12.7909490853336));
#77263=CARTESIAN_POINT('Ctrl Pts',(2.25274516472884,137.638846575935,12.7621647322052));
#77264=CARTESIAN_POINT('Ctrl Pts',(2.25345351216668,137.643737526163,12.7499477247201));
#77265=CARTESIAN_POINT('Ctrl Pts',(2.25494028833314,137.654264288147,12.7246474670605));
#77266=CARTESIAN_POINT('Ctrl Pts',(2.25571959888999,137.659927685746,12.711577264534));
#77267=CARTESIAN_POINT('Ctrl Pts',(2.25780079451095,137.675428976039,12.6771877600644));
#77268=CARTESIAN_POINT('Ctrl Pts',(2.25911363643615,137.68559037694,12.6560196150069));
#77269=CARTESIAN_POINT('Ctrl Pts',(2.26708123642232,137.749500719644,12.5307023464671));
#77270=CARTESIAN_POINT('Ctrl Pts',(2.27415966659373,137.815086893494,12.4330859538698));
#77271=CARTESIAN_POINT('Ctrl Pts',(2.28385895071946,137.920311904295,12.3110407886912));
#77272=CARTESIAN_POINT('Ctrl Pts',(2.28649165609938,137.950520369593,12.2790398775774));
#77273=CARTESIAN_POINT('Ctrl Pts',(2.29062106322069,138.001237787505,12.2299468122273));
#77274=CARTESIAN_POINT('Ctrl Pts',(2.29215454654415,138.020852036895,12.211970028329));
#77275=CARTESIAN_POINT('Ctrl Pts',(2.29423675454051,138.048753122294,12.1877642157909));
#77276=CARTESIAN_POINT('Ctrl Pts',(2.29481417212436,138.056631474004,12.1810742210004));
#77277=CARTESIAN_POINT('Ctrl Pts',(2.29579641297636,138.07029174004,12.1697212936527));
#77278=CARTESIAN_POINT('Ctrl Pts',(2.29620401253249,138.076039314993,12.1650180339266));
#77279=CARTESIAN_POINT('Ctrl Pts',(2.29708235201722,138.088600276358,12.1548980203329));
#77280=CARTESIAN_POINT('Ctrl Pts',(2.29755196526253,138.095426486923,12.1494980368316));
#77281=CARTESIAN_POINT('Ctrl Pts',(2.29888510429663,138.115104798427,12.1342146113771));
#77282=CARTESIAN_POINT('Ctrl Pts',(2.2997388719371,138.12807384151,12.1244831321404));
#77283=CARTESIAN_POINT('Ctrl Pts',(2.3039489445032,138.193667498271,12.076947107172));
#77284=CARTESIAN_POINT('Ctrl Pts',(2.30713589812369,138.248604495764,12.0424481197653));
#77285=CARTESIAN_POINT('Ctrl Pts',(2.31327779702413,138.359536887051,11.9826593606305));
#77286=CARTESIAN_POINT('Ctrl Pts',(2.31623035240831,138.415191331578,11.9570264076628));
#77287=CARTESIAN_POINT('Ctrl Pts',(2.3221087692099,138.526330276767,11.9140611365669));
#77288=CARTESIAN_POINT('Ctrl Pts',(2.32502237779676,138.581562981292,11.8963978043222));
#77289=CARTESIAN_POINT('Ctrl Pts',(2.32904944521308,138.656459309778,11.8772606827653));
#77290=CARTESIAN_POINT('Ctrl Pts',(2.33006939111661,138.675317164604,11.8728390488385));
#77291=CARTESIAN_POINT('Ctrl Pts',(2.33182061866858,138.707461216137,11.8659722361271));
#77292=CARTESIAN_POINT('Ctrl Pts',(2.33254569395921,138.720703866693,11.8633343392351));
#77293=CARTESIAN_POINT('Ctrl Pts',(2.3340259433531,138.747591822371,11.8583641405755));
#77294=CARTESIAN_POINT('Ctrl Pts',(2.33478133960006,138.761237481902,11.8560414546064));
#77295=CARTESIAN_POINT('Ctrl Pts',(2.33670725600901,138.79582469885,11.8506578873227));
#77296=CARTESIAN_POINT('Ctrl Pts',(2.33788578600493,138.81680299418,11.8478571336295));
#77297=CARTESIAN_POINT('Ctrl Pts',(2.34371292345557,138.919586945369,11.8363973788373));
#77298=CARTESIAN_POINT('Ctrl Pts',(2.3485574759316,139.001952206167,11.8341924141317));
#77299=CARTESIAN_POINT('Ctrl Pts',(2.35776999673555,139.155291462259,11.8430140649857));
#77300=CARTESIAN_POINT('Ctrl Pts',(2.36210085406627,139.226131638434,11.8523162681797));
#77301=CARTESIAN_POINT('Ctrl Pts',(2.36839126025368,139.330413340426,11.8738537033917));
#77302=CARTESIAN_POINT('Ctrl Pts',(2.37043534614109,139.364550994105,11.882195656608));
#77303=CARTESIAN_POINT('Ctrl Pts',(2.37306907709964,139.409344510914,11.8948666630384));
#77304=CARTESIAN_POINT('Ctrl Pts',(2.37370902267679,139.420295105406,11.8981031905725));
#77305=CARTESIAN_POINT('Ctrl Pts',(2.37476487930829,139.438497302472,11.903715442248));
#77306=CARTESIAN_POINT('Ctrl Pts',(2.37518463184687,139.445770127091,11.9060202821745));
#77307=CARTESIAN_POINT('Ctrl Pts',(2.37605246938255,139.460891057036,11.9109427237289));
#77308=CARTESIAN_POINT('Ctrl Pts',(2.37650000128357,139.468735521553,11.9135701601655));
#77309=CARTESIAN_POINT('Ctrl Pts',(2.37772541824389,139.490326547998,11.9210060911159));
#77310=CARTESIAN_POINT('Ctrl Pts',(2.3784956971696,139.504024589974,11.9259535783716));
#77311=CARTESIAN_POINT('Ctrl Pts',(2.38434251093767,139.60869592036,11.9655349895755));
#77312=CARTESIAN_POINT('Ctrl Pts',(2.38900748988419,139.696093046544,12.0089669629706));
#77313=CARTESIAN_POINT('Ctrl Pts',(2.39760626119889,139.845744994916,12.1029839665974));
#77314=CARTESIAN_POINT('Ctrl Pts',(2.40150115951419,139.909403070161,12.1506016419536));
#77315=CARTESIAN_POINT('Ctrl Pts',(2.40684657404106,139.987187405098,12.2193105111532));
#77316=CARTESIAN_POINT('Ctrl Pts',(2.40812101239358,140.005083667629,12.2359344589578));
#77317=CARTESIAN_POINT('Ctrl Pts',(2.4101812790993,140.03291814835,12.2631190121901));
#77318=CARTESIAN_POINT('Ctrl Pts',(2.4109548070105,140.043130219096,12.2733932546015));
#77319=CARTESIAN_POINT('Ctrl Pts',(2.41244528595526,140.06234281667,12.2933054923245));
#77320=CARTESIAN_POINT('Ctrl Pts',(2.41316101199145,140.071368915085,12.3029168922141));
#77321=CARTESIAN_POINT('Ctrl Pts',(2.41483577592686,140.092021011334,12.3255124068903));
#77322=CARTESIAN_POINT('Ctrl Pts',(2.41579886511404,140.103547215887,12.3385846560322));
#77323=CARTESIAN_POINT('Ctrl Pts',(2.41907814192734,140.14161005561,12.3833394642116));
#77324=CARTESIAN_POINT('Ctrl Pts',(2.42143774752584,140.167035759087,12.4159371473718));
#77325=CARTESIAN_POINT('Ctrl Pts',(2.42766446925053,140.229219391161,12.5030262103607));
#77326=CARTESIAN_POINT('Ctrl Pts',(2.43159587364131,140.263746584658,12.5589933090611));
#77327=CARTESIAN_POINT('Ctrl Pts',(2.44049739430663,140.33271927143,12.6897241365367));
#77328=CARTESIAN_POINT('Ctrl Pts',(2.4454679399433,140.364862743131,12.7654640632126));
#77329=CARTESIAN_POINT('Ctrl Pts',(2.45109231771666,140.395450064994,12.8586329154602));
#77330=CARTESIAN_POINT('Ctrl Pts',(2.45199516489703,140.400169710514,12.8738420352965));
#77331=CARTESIAN_POINT('Ctrl Pts',(2.45336820299642,140.407067033628,12.8974216555631));
#77332=CARTESIAN_POINT('Ctrl Pts',(2.45384745113161,140.40942020479,12.9057391034271));
#77333=CARTESIAN_POINT('Ctrl Pts',(2.45473312315506,140.413670089769,12.9212851135362));
#77334=CARTESIAN_POINT('Ctrl Pts',(2.45514049794269,140.415585249132,12.9285077499075));
#77335=CARTESIAN_POINT('Ctrl Pts',(2.45611397160794,140.420063501894,12.9459342246824));
#77336=CARTESIAN_POINT('Ctrl Pts',(2.45667704562606,140.422572019983,12.9561515107088));
#77337=CARTESIAN_POINT('Ctrl Pts',(2.45870326266731,140.431285559853,12.993370809746));
#77338=CARTESIAN_POINT('Ctrl Pts',(2.46013392939336,140.436834013943,13.0205218929193));
#77339=CARTESIAN_POINT('Ctrl Pts',(2.46391819628186,140.449690327572,13.0940148453703));
#77340=CARTESIAN_POINT('Ctrl Pts',(2.46622290348314,140.455547010517,13.1405782999316));
#77341=CARTESIAN_POINT('Ctrl Pts',(2.47406375811669,140.467924889942,13.3009016006718));
#77342=CARTESIAN_POINT('Ctrl Pts',(2.479520579716,140.463406430134,13.4150838475486));
#77343=CARTESIAN_POINT('Ctrl Pts',(2.48657384780218,140.44219234876,13.5498421181231));
#77344=CARTESIAN_POINT('Ctrl Pts',(2.48775310321166,140.438175405704,13.5720133927024));
#77345=CARTESIAN_POINT('Ctrl Pts',(2.48969622194985,140.430816082615,13.6078900142765));
#77346=CARTESIAN_POINT('Ctrl Pts',(2.49045021101467,140.427784483891,13.6216556727881));
#77347=CARTESIAN_POINT('Ctrl Pts',(2.49192856304666,140.421504766341,13.6483296896206));
#77348=CARTESIAN_POINT('Ctrl Pts',(2.4926521625319,140.418278439744,13.661241781066));
#77349=CARTESIAN_POINT('Ctrl Pts',(2.49438700710972,140.410186030904,13.6918472905395));
#77350=CARTESIAN_POINT('Ctrl Pts',(2.49540324434179,140.405162478517,13.7094964061111));
#77351=CARTESIAN_POINT('Ctrl Pts',(2.49914145775699,140.3856708096,13.7733879170323));
#77352=CARTESIAN_POINT('Ctrl Pts',(2.5019255108253,140.369241751737,13.8189951850368));
#77353=CARTESIAN_POINT('Ctrl Pts',(2.50997773036562,140.316356776344,13.945703482937));
#77354=CARTESIAN_POINT('Ctrl Pts',(2.51537525337801,140.27473480582,14.024415152914));
#77355=CARTESIAN_POINT('Ctrl Pts',(2.52399775337936,140.196231888673,14.1449160293077));
#77356=CARTESIAN_POINT('Ctrl Pts',(2.52725565082794,140.163653140279,14.1892503616524));
#77357=CARTESIAN_POINT('Ctrl Pts',(2.53112444036924,140.120359529895,14.2416987678188));
#77358=CARTESIAN_POINT('Ctrl Pts',(2.53185814070649,140.111930261071,14.2516370969016));
#77359=CARTESIAN_POINT('Ctrl Pts',(2.53302452797269,140.098152677373,14.2674481868343));
#77360=CARTESIAN_POINT('Ctrl Pts',(2.53346280805793,140.092887508867,14.2733921080965));
#77361=CARTESIAN_POINT('Ctrl Pts',(2.53432576684646,140.082337840558,14.2851082601725));
#77362=CARTESIAN_POINT('Ctrl Pts',(2.53475052174912,140.077054923951,14.2908815171046));
#77363=CARTESIAN_POINT('Ctrl Pts',(2.53584371726522,140.063232632713,14.3057455798949));
#77364=CARTESIAN_POINT('Ctrl Pts',(2.53650706107763,140.054622723902,14.3147702861604));
#77365=CARTESIAN_POINT('Ctrl Pts',(2.53969122706636,140.01228302441,14.3580287634261));
#77366=CARTESIAN_POINT('Ctrl Pts',(2.54211057309605,139.976993619402,14.3906997831747));
#77367=CARTESIAN_POINT('Ctrl Pts',(2.54746373958457,139.893965405756,14.4602978588967));
#77368=CARTESIAN_POINT('Ctrl Pts',(2.55036831553376,139.845424159169,14.4961285860499));
#77369=CARTESIAN_POINT('Ctrl Pts',(2.55716828842193,139.728267435862,14.571903765268));
#77370=CARTESIAN_POINT('Ctrl Pts',(2.56108155800638,139.658343009659,14.6094638059892));
#77371=CARTESIAN_POINT('Ctrl Pts',(2.56627800431265,139.566583289732,14.6495377101254));
#77372=CARTESIAN_POINT('Ctrl Pts',(2.5673747304241,139.547262904707,14.6574873519514));
#77373=CARTESIAN_POINT('Ctrl Pts',(2.56921771023866,139.514929433858,14.6699889563101));
#77374=CARTESIAN_POINT('Ctrl Pts',(2.5699560558399,139.502010069577,14.6747755942725));
#77375=CARTESIAN_POINT('Ctrl Pts',(2.57143120423961,139.476280225902,14.6838974857424));
#77376=CARTESIAN_POINT('Ctrl Pts',(2.57216771077682,139.463473410209,14.6882389871584));
#77377=CARTESIAN_POINT('Ctrl Pts',(2.57398306513389,139.432014746243,14.6984196248955));
#77378=CARTESIAN_POINT('Ctrl Pts',(2.57506814285162,139.413302941079,14.7040636791332));
#77379=CARTESIAN_POINT('Ctrl Pts',(2.57953817834046,139.336618770665,14.7255282611144));
#77380=CARTESIAN_POINT('Ctrl Pts',(2.58302264742412,139.27781679373,14.7381444641175));
#77381=CARTESIAN_POINT('Ctrl Pts',(2.59009978778521,139.15970191813,14.7559714410965));
#77382=CARTESIAN_POINT('Ctrl Pts',(2.5936839870074,139.100509770264,14.7612511146981));
#77383=CARTESIAN_POINT('Ctrl Pts',(2.60110886981884,138.977218876787,14.7647202482106));
#77384=CARTESIAN_POINT('Ctrl Pts',(2.60494005927591,138.913220346021,14.7623251564652));
#77385=CARTESIAN_POINT('Ctrl Pts',(2.60953934019143,138.833500429977,14.7540878445661));
#77386=CARTESIAN_POINT('Ctrl Pts',(2.61045635642689,138.817448698174,14.7521599885751));
#77387=CARTESIAN_POINT('Ctrl Pts',(2.61184622426581,138.79281680752,14.748786727065));
#77388=CARTESIAN_POINT('Ctrl Pts',(2.61232845875939,138.784212517125,14.747530181319));
#77389=CARTESIAN_POINT('Ctrl Pts',(2.61321669327177,138.768244032571,14.7450526398145));
#77390=CARTESIAN_POINT('Ctrl Pts',(2.61362370017114,138.760877554038,14.7438519376105));
#77391=CARTESIAN_POINT('Ctrl Pts',(2.61459236001744,138.743233843288,14.7408373563039));
#77392=CARTESIAN_POINT('Ctrl Pts',(2.61515107908305,138.732966345954,14.7389698352756));
#77393=CARTESIAN_POINT('Ctrl Pts',(2.61713938730934,138.696149582923,14.7318657110777));
#77394=CARTESIAN_POINT('Ctrl Pts',(2.61853810773955,138.669725479143,14.7260025953688));
#77395=CARTESIAN_POINT('Ctrl Pts',(2.62220547837201,138.599681121623,14.7084091027784));
#77396=CARTESIAN_POINT('Ctrl Pts',(2.6244288972829,138.556414814728,14.6953866860314));
#77397=CARTESIAN_POINT('Ctrl Pts',(2.63237037328822,138.402966457918,14.6413409779586));
#77398=CARTESIAN_POINT('Ctrl Pts',(2.6379887583654,138.297230528857,14.5890920157521));
#77399=CARTESIAN_POINT('Ctrl Pts',(2.64521164228452,138.180458135184,14.5127110224938));
#77400=CARTESIAN_POINT('Ctrl Pts',(2.64636500163808,138.162309689367,14.5002465450273));
#77401=CARTESIAN_POINT('Ctrl Pts',(2.64827679819217,138.133093147334,14.4791949350024));
#77402=CARTESIAN_POINT('Ctrl Pts',(2.64902600158494,138.121854683969,14.4708496792317));
#77403=CARTESIAN_POINT('Ctrl Pts',(2.65050324866083,138.100117631428,14.4542195549148));
#77404=CARTESIAN_POINT('Ctrl Pts',(2.6512306706349,138.089609467871,14.4459494406902));
#77405=CARTESIAN_POINT('Ctrl Pts',(2.65298892542883,138.064685122948,14.425774329069));
#77406=CARTESIAN_POINT('Ctrl Pts',(2.6540250975836,138.050381128817,14.4137350282089));
#77407=CARTESIAN_POINT('Ctrl Pts',(2.65795219338977,137.997616345733,14.3675686866497));
#77408=CARTESIAN_POINT('Ctrl Pts',(2.66091385203213,137.960735266399,14.3316994883801));
#77409=CARTESIAN_POINT('Ctrl Pts',(2.66994083637004,137.856492796377,14.2190447339856));
#77410=CARTESIAN_POINT('Ctrl Pts',(2.6761834058447,137.795199824031,14.1370819223044));
#77411=CARTESIAN_POINT('Ctrl Pts',(2.68460271814688,137.722590502865,14.015287168761));
#77412=CARTESIAN_POINT('Ctrl Pts',(2.68692730425134,137.703642274769,13.9803439403179));
#77413=CARTESIAN_POINT('Ctrl Pts',(2.68986908455229,137.680797122219,13.9337847011799));
#77414=CARTESIAN_POINT('Ctrl Pts',(2.69055017515359,137.675591118539,13.9228325735292));
#77415=CARTESIAN_POINT('Ctrl Pts',(2.69161145163983,137.667600250298,13.9054684069714));
#77416=CARTESIAN_POINT('Ctrl Pts',(2.69199684122509,137.664724277442,13.8990991852561));
#77417=CARTESIAN_POINT('Ctrl Pts',(2.69280690817822,137.658731287118,13.8855693585572));
#77418=CARTESIAN_POINT('Ctrl Pts',(2.69323084901377,137.655625743929,13.8784039226315));
#77419=CARTESIAN_POINT('Ctrl Pts',(2.69431925404384,137.647739328723,13.8598008509167));
#77420=CARTESIAN_POINT('Ctrl Pts',(2.69497870638576,137.643046049485,13.8483264650811));
#77421=CARTESIAN_POINT('Ctrl Pts',(2.69809933896348,137.621293000266,13.793152918644));
#77422=CARTESIAN_POINT('Ctrl Pts',(2.70046390778229,137.606193741402,13.7487066123177));
#77423=CARTESIAN_POINT('Ctrl Pts',(2.70952833111271,137.555655267457,13.572558774906));
#77424=CARTESIAN_POINT('Ctrl Pts',(2.71592526133157,137.536552809664,13.436905793067));
#77425=CARTESIAN_POINT('Ctrl Pts',(2.72296469855451,137.536500109331,13.300565695148));
#77426=CARTESIAN_POINT('Ctrl Pts',(2.1523578980801,137.536219494403,13.3011848097323));
#77427=CARTESIAN_POINT('Ctrl Pts',(2.15550554832557,137.536293154548,13.2472840551289));
#77428=CARTESIAN_POINT('Ctrl Pts',(2.15869901612957,137.539374600405,13.1932720094472));
#77429=CARTESIAN_POINT('Ctrl Pts',(2.1618777162065,137.545442632201,13.1395110595447));
#77430=CARTESIAN_POINT('Ctrl Pts',(2.16505245649291,137.551503104888,13.0858170810754));
#77431=CARTESIAN_POINT('Ctrl Pts',(2.16821217235941,137.56054245299,13.0323735512194));
#77432=CARTESIAN_POINT('Ctrl Pts',(2.17131609025905,137.572501951759,12.9795326602491));
#77433=CARTESIAN_POINT('Ctrl Pts',(2.1744174825726,137.584451719361,12.9267347646876));
#77434=CARTESIAN_POINT('Ctrl Pts',(2.17746166119412,137.599319909126,12.8745368755472));
#77435=CARTESIAN_POINT('Ctrl Pts',(2.18039406670322,137.617070160124,12.8233094345982));
#77436=CARTESIAN_POINT('Ctrl Pts',(2.18316172764799,137.633823189777,12.7749599866193));
#77437=CARTESIAN_POINT('Ctrl Pts',(2.18592960702013,137.652981000612,12.7274166011582));
#77438=CARTESIAN_POINT('Ctrl Pts',(2.18862949130611,137.674558624412,12.6809911398357));
#77439=CARTESIAN_POINT('Ctrl Pts',(2.18878910882343,137.675834296395,12.6782464604008));
#77440=CARTESIAN_POINT('Ctrl Pts',(2.18894848868499,137.677118421965,12.6755057029054));
#77441=CARTESIAN_POINT('Ctrl Pts',(2.18910761679543,137.678411002512,12.6727689372519));
#77442=CARTESIAN_POINT('Ctrl Pts',(2.19196056412663,137.701585187226,12.6237025074072));
#77443=CARTESIAN_POINT('Ctrl Pts',(2.19472252007874,137.727492198735,12.575928224394));
#77444=CARTESIAN_POINT('Ctrl Pts',(2.1974438794689,137.755931673586,12.5297545626452));
#77445=CARTESIAN_POINT('Ctrl Pts',(2.20016620731441,137.784381269248,12.4835644689875));
#77446=CARTESIAN_POINT('Ctrl Pts',(2.20284819104804,137.815365953895,12.4389751052157));
#77447=CARTESIAN_POINT('Ctrl Pts',(2.20553720782205,137.848684385416,12.3962928570608));
#77448=CARTESIAN_POINT('Ctrl Pts',(2.20823134953414,137.882066317804,12.3535292617455));
#77449=CARTESIAN_POINT('Ctrl Pts',(2.2109330428732,137.917791187923,12.3126805278709));
#77450=CARTESIAN_POINT('Ctrl Pts',(2.21370375737088,137.955614718014,12.2740340050254));
#77451=CARTESIAN_POINT('Ctrl Pts',(2.21602203639286,137.987261968722,12.2416981496855));
#77452=CARTESIAN_POINT('Ctrl Pts',(2.21838912584427,138.020377776731,12.2109039054139));
#77453=CARTESIAN_POINT('Ctrl Pts',(2.22084375255782,138.054794553718,12.1818038527325));
#77454=CARTESIAN_POINT('Ctrl Pts',(2.2208448905864,138.054810510228,12.1817903611937));
#77455=CARTESIAN_POINT('Ctrl Pts',(2.2208460286338,138.054826467018,12.1817768700183));
#77456=CARTESIAN_POINT('Ctrl Pts',(2.22084716670001,138.054842424087,12.1817633792064));
#77457=CARTESIAN_POINT('Ctrl Pts',(2.22357929346152,138.093150157043,12.1493763284752));
#77458=CARTESIAN_POINT('Ctrl Pts',(2.22642812310337,138.133235441837,12.1189543861747));
#77459=CARTESIAN_POINT('Ctrl Pts',(2.22933369529822,138.174856196594,12.0906687998612));
#77460=CARTESIAN_POINT('Ctrl Pts',(2.22961559730069,138.178894290753,12.0879244992939));
#77461=CARTESIAN_POINT('Ctrl Pts',(2.22989803342686,138.182946797967,12.0852003090169));
#77462=CARTESIAN_POINT('Ctrl Pts',(2.23018094891673,138.187013471129,12.0824963851001));
#77463=CARTESIAN_POINT('Ctrl Pts',(2.23337406614028,138.232911856263,12.0519786285997));
#77464=CARTESIAN_POINT('Ctrl Pts',(2.23662760472992,138.280620606839,12.024041912797));
#77465=CARTESIAN_POINT('Ctrl Pts',(2.23987572411306,138.329805024634,11.9988660921796));
#77466=CARTESIAN_POINT('Ctrl Pts',(2.2431205475994,138.378939534544,11.9737158177004));
#77467=CARTESIAN_POINT('Ctrl Pts',(2.24635961740638,138.429546607901,11.9513204831712));
#77468=CARTESIAN_POINT('Ctrl Pts',(2.24954747105379,138.481282391603,11.9318213807645));
#77469=CARTESIAN_POINT('Ctrl Pts',(2.25273335069003,138.532986139011,11.9123343527659));
#77470=CARTESIAN_POINT('Ctrl Pts',(2.25586793486043,138.585817172414,11.8957398310716));
#77471=CARTESIAN_POINT('Ctrl Pts',(2.25892958794811,138.63942303065,11.8821445272637));
#77472=CARTESIAN_POINT('Ctrl Pts',(2.26199055592287,138.693016893385,11.8685522657072));
#77473=CARTESIAN_POINT('Ctrl Pts',(2.26497862342163,138.747385219049,11.8579579099369));
#77474=CARTESIAN_POINT('Ctrl Pts',(2.26789695879374,138.802166817994,11.8504345673539));
#77475=CARTESIAN_POINT('Ctrl Pts',(2.27081790052231,138.856997342219,11.8429045056964));
#77476=CARTESIAN_POINT('Ctrl Pts',(2.27366910740785,138.912241854974,11.8384511263189));
#77477=CARTESIAN_POINT('Ctrl Pts',(2.27647771075072,138.967529489259,11.8371125396387));
#77478=CARTESIAN_POINT('Ctrl Pts',(2.27928753489876,139.022841155215,11.83577337112));
#77479=CARTESIAN_POINT('Ctrl Pts',(2.28205500254431,139.078195919884,11.8375520422158));
#77480=CARTESIAN_POINT('Ctrl Pts',(2.2848282455957,139.133214302515,11.8424476371093));
#77481=CARTESIAN_POINT('Ctrl Pts',(2.28760671021388,139.188336275835,11.8473524496138));
#77482=CARTESIAN_POINT('Ctrl Pts',(2.29039147921724,139.243120415904,11.8553864709964));
#77483=CARTESIAN_POINT('Ctrl Pts',(2.29324613297757,139.297178632503,11.8665029888428));
#77484=CARTESIAN_POINT('Ctrl Pts',(2.2955148416726,139.340140881634,11.875337734775));
#77485=CARTESIAN_POINT('Ctrl Pts',(2.29782816447982,139.382644379702,11.8861186741655));
#77486=CARTESIAN_POINT('Ctrl Pts',(2.30022080660466,139.424493347728,11.8987979320856));
#77487=CARTESIAN_POINT('Ctrl Pts',(2.30022183019628,139.424511251055,11.8988033563746));
#77488=CARTESIAN_POINT('Ctrl Pts',(2.30022285380242,139.424529154262,11.8988087810107));
#77489=CARTESIAN_POINT('Ctrl Pts',(2.30022387742307,139.424547057349,11.8988142059941));
#77490=CARTESIAN_POINT('Ctrl Pts',(2.30298533681397,139.472844880835,11.9134493847729));
#77491=CARTESIAN_POINT('Ctrl Pts',(2.30585969637305,139.520448031779,11.9306718051708));
#77492=CARTESIAN_POINT('Ctrl Pts',(2.3087869074351,139.56707767681,11.9503691296638));
#77493=CARTESIAN_POINT('Ctrl Pts',(2.30905673505877,139.571375954606,11.9521848109207));
#77494=CARTESIAN_POINT('Ctrl Pts',(2.30932701176075,139.575665940011,11.9540214911148));
#77495=CARTESIAN_POINT('Ctrl Pts',(2.30959769050828,139.579947402644,11.9558790635485));
#77496=CARTESIAN_POINT('Ctrl Pts',(2.31279923135007,139.630587793168,11.9778501051142));
#77497=CARTESIAN_POINT('Ctrl Pts',(2.31605639029282,139.680039512358,12.0027484103807));
#77498=CARTESIAN_POINT('Ctrl Pts',(2.31930454869308,139.727969586401,12.0303902103241));
#77499=CARTESIAN_POINT('Ctrl Pts',(2.32254956202045,139.775853251508,12.0580052457243));
#77500=CARTESIAN_POINT('Ctrl Pts',(2.3257852564346,139.822218447312,12.0883581874517));
#77501=CARTESIAN_POINT('Ctrl Pts',(2.3289675118827,139.866759328631,12.1212366597246));
#77502=CARTESIAN_POINT('Ctrl Pts',(2.33214793458404,139.911274557654,12.1540961963981));
#77503=CARTESIAN_POINT('Ctrl Pts',(2.33527484322847,139.953967669826,12.1894782608107));
#77504=CARTESIAN_POINT('Ctrl Pts',(2.33832795525588,139.994557015017,12.227144403972));
#77505=CARTESIAN_POINT('Ctrl Pts',(2.34138050668152,140.035138907334,12.2648036310075));
#77506=CARTESIAN_POINT('Ctrl Pts',(2.34435929156306,140.073617767386,12.3047461053593));
#77507=CARTESIAN_POINT('Ctrl Pts',(2.34726876744892,140.109735338471,12.3467076749523));
#77508=CARTESIAN_POINT('Ctrl Pts',(2.35018098300326,140.145886919177,12.3887087570877));
#77509=CARTESIAN_POINT('Ctrl Pts',(2.35302388710834,140.179672592426,12.4327328225378));
#77510=CARTESIAN_POINT('Ctrl Pts',(2.35582576337124,140.210858209603,12.4784883848673));
#77511=CARTESIAN_POINT('Ctrl Pts',(2.35862893969711,140.242058296822,12.5242651776534));
#77512=CARTESIAN_POINT('Ctrl Pts',(2.36139134364931,140.270655589927,12.5717752126333));
#77513=CARTESIAN_POINT('Ctrl Pts',(2.36416200661037,140.296444117614,12.6206983103048));
#77514=CARTESIAN_POINT('Ctrl Pts',(2.36693796007643,140.322281887789,12.6697148252908));
#77515=CARTESIAN_POINT('Ctrl Pts',(2.36972272487537,140.345299592945,12.7201499427997));
#77516=CARTESIAN_POINT('Ctrl Pts',(2.37258035955952,140.365325280923,12.7716510616305));
#77517=CARTESIAN_POINT('Ctrl Pts',(2.37481409186371,140.380978795489,12.8119080313098));
#77518=CARTESIAN_POINT('Ctrl Pts',(2.37709280050146,140.394804689715,12.852815702604));
#77519=CARTESIAN_POINT('Ctrl Pts',(2.37944946662814,140.406739886195,12.8941922688946));
#77520=CARTESIAN_POINT('Ctrl Pts',(2.37945051133745,140.406745177063,12.8942106111127));
#77521=CARTESIAN_POINT('Ctrl Pts',(2.37945155606208,140.406750467561,12.8942289534231));
#77522=CARTESIAN_POINT('Ctrl Pts',(2.37945260080203,140.406755757687,12.894247295826));
#77523=CARTESIAN_POINT('Ctrl Pts',(2.38220585907322,140.4206971066,12.9425859971643));
#77524=CARTESIAN_POINT('Ctrl Pts',(2.38507288664342,140.432105939502,12.9917488432394));
#77525=CARTESIAN_POINT('Ctrl Pts',(2.38799344305808,140.440924128759,13.0414426716851));
#77526=CARTESIAN_POINT('Ctrl Pts',(2.38826395906563,140.441740911937,13.0460455535206));
#77527=CARTESIAN_POINT('Ctrl Pts',(2.38853493431624,140.442535483363,13.050652956791));
#77528=CARTESIAN_POINT('Ctrl Pts',(2.38880632093915,140.443307806116,13.0552646279701));
#77529=CARTESIAN_POINT('Ctrl Pts',(2.39200187028919,140.45240182646,13.1095665780098));
#77530=CARTESIAN_POINT('Ctrl Pts',(2.39525383070685,140.458409324209,13.1644657791954));
#77531=CARTESIAN_POINT('Ctrl Pts',(2.39849724748783,140.461302303971,13.219584694723));
#77532=CARTESIAN_POINT('Ctrl Pts',(2.40173739340044,140.464192366268,13.2746480248204));
#77533=CARTESIAN_POINT('Ctrl Pts',(2.40496867820619,140.463974544526,13.3299306654181));
#77534=CARTESIAN_POINT('Ctrl Pts',(2.40814662138283,140.460659602981,13.3850621023334));
#77535=CARTESIAN_POINT('Ctrl Pts',(2.41132262401351,140.457346685637,13.440159874365));
#77536=CARTESIAN_POINT('Ctrl Pts',(2.41444521352809,140.450940560639,13.495106652687));
#77537=CARTESIAN_POINT('Ctrl Pts',(2.41749370942239,140.441487057421,13.5495379157152));
#77538=CARTESIAN_POINT('Ctrl Pts',(2.42054155654786,140.43203556606,13.6039575948973));
#77539=CARTESIAN_POINT('Ctrl Pts',(2.4235153433608,140.419537968165,13.6578619456573));
#77540=CARTESIAN_POINT('Ctrl Pts',(2.42641909641369,140.40407440464,13.7108920333125));
#77541=CARTESIAN_POINT('Ctrl Pts',(2.42932552104518,140.388596613966,13.7639709109456));
#77542=CARTESIAN_POINT('Ctrl Pts',(2.43216190823954,140.370147239321,13.8161738155769));
#77543=CARTESIAN_POINT('Ctrl Pts',(2.43495610334391,140.348842442441,13.8671471737924));
#77544=CARTESIAN_POINT('Ctrl Pts',(2.43775154983969,140.327528104124,13.9181433606294));
#77545=CARTESIAN_POINT('Ctrl Pts',(2.44050505464395,140.303355499708,13.9679087012849));
#77546=CARTESIAN_POINT('Ctrl Pts',(2.44326526369745,140.276480081452,14.0160976886114));
#77547=CARTESIAN_POINT('Ctrl Pts',(2.44603076905287,140.249553094518,14.0643791411901));
#77548=CARTESIAN_POINT('Ctrl Pts',(2.44880351661884,140.219912496511,14.1110777927002));
#77549=CARTESIAN_POINT('Ctrl Pts',(2.45164733848727,140.187759233284,14.155859031342));
#77550=CARTESIAN_POINT('Ctrl Pts',(2.45393344763572,140.161911668768,14.1918580509974));
#77551=CARTESIAN_POINT('Ctrl Pts',(2.45626596845874,140.134441103001,14.2266180351326));
#77552=CARTESIAN_POINT('Ctrl Pts',(2.45868078854869,140.105475601412,14.2599747072367));
#77553=CARTESIAN_POINT('Ctrl Pts',(2.45868184863585,140.105462885783,14.2599893505552));
#77554=CARTESIAN_POINT('Ctrl Pts',(2.45868290873886,140.105450169866,14.2600039936037));
#77555=CARTESIAN_POINT('Ctrl Pts',(2.45868396885773,140.105437453661,14.2600186363824));
#77556=CARTESIAN_POINT('Ctrl Pts',(2.46143468376256,140.072442422951,14.2980125919953));
#77557=CARTESIAN_POINT('Ctrl Pts',(2.46429959910621,140.037378642723,14.3343270654957));
#77558=CARTESIAN_POINT('Ctrl Pts',(2.46721859668257,140.0004607922,14.3687541847263));
#77559=CARTESIAN_POINT('Ctrl Pts',(2.46749158409374,139.99700819994,14.371973841443));
#77560=CARTESIAN_POINT('Ctrl Pts',(2.46776504451716,139.993539428748,14.3751769845194));
#77561=CARTESIAN_POINT('Ctrl Pts',(2.46803892877915,139.9900546772,14.378363440494));
#77562=CARTESIAN_POINT('Ctrl Pts',(2.4712356635498,139.949381195785,14.4155552620871));
#77563=CARTESIAN_POINT('Ctrl Pts',(2.47448950913879,139.906525063113,14.4504752560248));
#77564=CARTESIAN_POINT('Ctrl Pts',(2.4777354034318,139.861788895216,14.4828945695633));
#77565=CARTESIAN_POINT('Ctrl Pts',(2.48097805793362,139.817097379371,14.5152815247449));
#77566=CARTESIAN_POINT('Ctrl Pts',(2.48421243948382,139.770529740384,14.5451731131655));
#77567=CARTESIAN_POINT('Ctrl Pts',(2.48739394460498,139.722403678361,14.5723769424731));
#77568=CARTESIAN_POINT('Ctrl Pts',(2.49057353314209,139.674306608165,14.599564383806));
#77569=CARTESIAN_POINT('Ctrl Pts',(2.49370017089743,139.624653040574,14.6240674304793));
#77570=CARTESIAN_POINT('Ctrl Pts',(2.4967530713209,139.573774622569,14.6457264304736));
#77571=CARTESIAN_POINT('Ctrl Pts',(2.49980534061447,139.522906722723,14.6673809528759));
#77572=CARTESIAN_POINT('Ctrl Pts',(2.50278390429222,139.470814490295,14.6861925675373));
#77573=CARTESIAN_POINT('Ctrl Pts',(2.50569271488533,139.417843475775,14.7020334705389));
#77574=CARTESIAN_POINT('Ctrl Pts',(2.50860420241418,139.364823712807,14.7178889516912));
#77575=CARTESIAN_POINT('Ctrl Pts',(2.51144593371271,139.310923545508,14.7307680641669));
#77576=CARTESIAN_POINT('Ctrl Pts',(2.5142457157691,139.256503576921,14.7405761469619));
#77577=CARTESIAN_POINT('Ctrl Pts',(2.51704675672904,139.202059138753,14.7503886398967));
#77578=CARTESIAN_POINT('Ctrl Pts',(2.51980609950029,139.147094440689,14.7571269926452));
#77579=CARTESIAN_POINT('Ctrl Pts',(2.52257238304002,139.091984679983,14.7607339012244));
#77580=CARTESIAN_POINT('Ctrl Pts',(2.52534394446532,139.036769773508,14.764347691546));
#77581=CARTESIAN_POINT('Ctrl Pts',(2.52812298668982,138.981409352939,14.7648175137342));
#77582=CARTESIAN_POINT('Ctrl Pts',(2.53097335002254,138.926294221959,14.7621301847635));
#77583=CARTESIAN_POINT('Ctrl Pts',(2.53324011254487,138.882463699763,14.7599930759515));
#77584=CARTESIAN_POINT('Ctrl Pts',(2.53555245154774,138.838788669781,14.7558599980584));
#77585=CARTESIAN_POINT('Ctrl Pts',(2.53794511405316,138.795470381661,14.7497484762756));
#77586=CARTESIAN_POINT('Ctrl Pts',(2.53794616090957,138.795451428705,14.7497458023148));
#77587=CARTESIAN_POINT('Ctrl Pts',(2.53794720778136,138.795432475817,14.7497431279756));
#77588=CARTESIAN_POINT('Ctrl Pts',(2.53794825466852,138.795413522996,14.7497404532578));
#77589=CARTESIAN_POINT('Ctrl Pts',(2.54070220430138,138.745556084026,14.7427043197617));
#77590=CARTESIAN_POINT('Ctrl Pts',(2.5435699260012,138.695983868955,14.7330159221944));
#77591=CARTESIAN_POINT('Ctrl Pts',(2.54649128200699,138.646988471565,14.7207425410881));
#77592=CARTESIAN_POINT('Ctrl Pts',(2.54676281372437,138.642434488972,14.7196017652829));
#77593=CARTESIAN_POINT('Ctrl Pts',(2.54703480879779,138.637885514961,14.7184386845662));
#77594=CARTESIAN_POINT('Ctrl Pts',(2.54730721893744,138.633341798781,14.7172533700387));
#77595=CARTESIAN_POINT('Ctrl Pts',(2.55050471805701,138.58000851059,14.7033403704606));
#77596=CARTESIAN_POINT('Ctrl Pts',(2.55375877581914,138.527395326826,14.6863601882844));
#77597=CARTESIAN_POINT('Ctrl Pts',(2.55700446481932,138.475858827517,14.6664423511454));
#77598=CARTESIAN_POINT('Ctrl Pts',(2.56024692677543,138.424373568654,14.646544317425));
#77599=CARTESIAN_POINT('Ctrl Pts',(2.56348070031214,138.37396267069,14.623714777597));
#77600=CARTESIAN_POINT('Ctrl Pts',(2.5666613306184,138.324960354391,14.5981157372378));
#77601=CARTESIAN_POINT('Ctrl Pts',(2.56984005670062,138.275987375481,14.5725320228685));
#77602=CARTESIAN_POINT('Ctrl Pts',(2.57296556587356,138.228421212674,14.5441822324541));
#77603=CARTESIAN_POINT('Ctrl Pts',(2.57601722018781,138.182576216969,14.5132578854509));
#77604=CARTESIAN_POINT('Ctrl Pts',(2.57906825454379,138.136740534896,14.4823398208777));
#77605=CARTESIAN_POINT('Ctrl Pts',(2.58204546584293,138.092625358433,14.4488482348586));
#77606=CARTESIAN_POINT('Ctrl Pts',(2.58495294617121,138.050525882716,14.413003646619));
#77607=CARTESIAN_POINT('Ctrl Pts',(2.58786311642032,138.008387457722,14.3771258959521));
#77608=CARTESIAN_POINT('Ctrl Pts',(2.59070355255766,137.968268619983,14.3388906818389));
#77609=CARTESIAN_POINT('Ctrl Pts',(2.5935021841686,137.930444939341,14.2985491993314));
#77610=CARTESIAN_POINT('Ctrl Pts',(2.59630208209884,137.892604144315,14.2581894631898));
#77611=CARTESIAN_POINT('Ctrl Pts',(2.59906042738604,137.857060881683,14.2157213699025));
#77612=CARTESIAN_POINT('Ctrl Pts',(2.60182595290597,137.824067298388,14.1714287029391));
#77613=CARTESIAN_POINT('Ctrl Pts',(2.60459676467958,137.791010648436,14.1270513713172));
#77614=CARTESIAN_POINT('Ctrl Pts',(2.60737529898325,137.760513964324,14.0808422637597));
#77615=CARTESIAN_POINT('Ctrl Pts',(2.6102254451594,137.732800829309,14.0331222855858));
#77616=CARTESIAN_POINT('Ctrl Pts',(2.61249014724905,137.71078020619,13.9952043937973));
#77617=CARTESIAN_POINT('Ctrl Pts',(2.61480053283759,137.690516653433,13.9563332651505));
#77618=CARTESIAN_POINT('Ctrl Pts',(2.61719125755502,137.67210465407,13.9166869331431));
#77619=CARTESIAN_POINT('Ctrl Pts',(2.61719230777412,137.672096565881,13.9166695169452));
#77620=CARTESIAN_POINT('Ctrl Pts',(2.61719335800871,137.672088478049,13.9166521005974));
#77621=CARTESIAN_POINT('Ctrl Pts',(2.61719440825882,137.672080390573,13.9166346840999));
#77622=CARTESIAN_POINT('Ctrl Pts',(2.62005550770341,137.650048427832,13.8691885269283));
#77623=CARTESIAN_POINT('Ctrl Pts',(2.62303773388409,137.630602442131,13.8204822350955));
#77624=CARTESIAN_POINT('Ctrl Pts',(2.62607496753421,137.61383739867,13.7708069211651));
#77625=CARTESIAN_POINT('Ctrl Pts',(2.62650186804912,137.611480976178,13.7638247724277));
#77626=CARTESIAN_POINT('Ctrl Pts',(2.62692985528643,137.609177515152,13.756823563917));
#77627=CARTESIAN_POINT('Ctrl Pts',(2.62735874564581,137.606927273515,13.7498041862546));
#77628=CARTESIAN_POINT('Ctrl Pts',(2.63065497843165,137.589633062772,13.6958568258598));
#77629=CARTESIAN_POINT('Ctrl Pts',(2.63400382996392,137.575481918602,13.6408301187835));
#77630=CARTESIAN_POINT('Ctrl Pts',(2.63733875522186,137.564555143265,13.5850899660694));
#77631=CARTESIAN_POINT('Ctrl Pts',(2.63751513242926,137.563977249018,13.5821419862152));
#77632=CARTESIAN_POINT('Ctrl Pts',(2.63769147068306,137.563408376539,13.5791920225578));
#77633=CARTESIAN_POINT('Ctrl Pts',(2.63786776013896,137.562848538649,13.5762401332085));
#77634=CARTESIAN_POINT('Ctrl Pts',(2.64136237790394,137.551750770921,13.5177242968082));
#77635=CARTESIAN_POINT('Ctrl Pts',(2.64483743486126,137.544201557004,13.4584462153631));
#77636=CARTESIAN_POINT('Ctrl Pts',(2.64824438977004,137.54026214309,13.3988283257318));
#77637=CARTESIAN_POINT('Ctrl Pts',(2.65011196726024,137.538102689575,13.3661478143456));
#77638=CARTESIAN_POINT('Ctrl Pts',(2.65195961351415,137.537027408895,13.3333652157989));
#77639=CARTESIAN_POINT('Ctrl Pts',(2.65378340881734,137.537042726446,13.3005506582616));
#77640=CARTESIAN_POINT('Origin',(4.2,139.,13.3));
#77641=CARTESIAN_POINT('',(3.22385647472349,137.536631187551,13.2999996886484));
#77642=CARTESIAN_POINT('',(3.1529262221125,137.5365,13.3000000000405));
#77643=CARTESIAN_POINT('',(4.2,137.5365,13.3));
#77644=CARTESIAN_POINT('Ctrl Pts',(3.22385647472349,137.536631187551,13.2999996886484));
#77645=CARTESIAN_POINT('Ctrl Pts',(3.22068411944641,137.536760431405,13.354271285598));
#77646=CARTESIAN_POINT('Ctrl Pts',(3.21753929924093,137.539896871394,13.4085937059785));
#77647=CARTESIAN_POINT('Ctrl Pts',(3.21445595208442,137.546016699963,13.4626125813809));
#77648=CARTESIAN_POINT('Ctrl Pts',(3.21134941699173,137.552182551956,13.5170376991468));
#77649=CARTESIAN_POINT('Ctrl Pts',(3.2083053657435,137.561376771111,13.5711546984878));
#77650=CARTESIAN_POINT('Ctrl Pts',(3.20533500370354,137.573539915795,13.6246062603118));
#77651=CARTESIAN_POINT('Ctrl Pts',(3.20236504498896,137.585701408928,13.6780505643094));
#77652=CARTESIAN_POINT('Ctrl Pts',(3.19946871180647,137.600831087743,13.730829527396));
#77653=CARTESIAN_POINT('Ctrl Pts',(3.19663342159315,137.618834381317,13.7825917897771));
#77654=CARTESIAN_POINT('Ctrl Pts',(3.19379538095205,137.636855139331,13.8344042651358));
#77655=CARTESIAN_POINT('Ctrl Pts',(3.19101832874183,137.657755277935,13.8851979101551));
#77656=CARTESIAN_POINT('Ctrl Pts',(3.18826740825234,137.681402812034,13.9346279494016));
#77657=CARTESIAN_POINT('Ctrl Pts',(3.18551498551653,137.705063259781,13.9840849818293));
#77658=CARTESIAN_POINT('Ctrl Pts',(3.18278837109439,137.731474407983,14.0321766444765));
#77659=CARTESIAN_POINT('Ctrl Pts',(3.18003428613028,137.760463205269,14.0785683654693));
#77660=CARTESIAN_POINT('Ctrl Pts',(3.17743948609428,137.787775409948,14.1222769804435));
#77661=CARTESIAN_POINT('Ctrl Pts',(3.17481977800385,137.817376122555,14.1644767214396));
#77662=CARTESIAN_POINT('Ctrl Pts',(3.17212111534149,137.849081944602,14.2048998818061));
#77663=CARTESIAN_POINT('Ctrl Pts',(3.17195027196522,137.851089134964,14.207458937924));
#77664=CARTESIAN_POINT('Ctrl Pts',(3.17177911215989,137.853104763532,14.2100108912797));
#77665=CARTESIAN_POINT('Ctrl Pts',(3.171607622213,137.855128784553,14.2125556809621));
#77666=CARTESIAN_POINT('Ctrl Pts',(3.17028440112709,137.870746185698,14.2321913472384));
#77667=CARTESIAN_POINT('Ctrl Pts',(3.16894142083759,137.886862460427,14.251399619855));
#77668=CARTESIAN_POINT('Ctrl Pts',(3.16757219701131,137.903452644182,14.2701512175302));
#77669=CARTESIAN_POINT('Ctrl Pts',(3.16757114655029,137.90346537208,14.2701656036532));
#77670=CARTESIAN_POINT('Ctrl Pts',(3.16757009607383,137.903478100257,14.2701799895075));
#77671=CARTESIAN_POINT('Ctrl Pts',(3.16756904558192,137.903490828713,14.2701943750933));
#77672=CARTESIAN_POINT('Ctrl Pts',(3.16481615624691,137.936846659555,14.3078928334693));
#77673=CARTESIAN_POINT('Ctrl Pts',(3.16194936692662,137.972256761486,14.3438918429709));
#77674=CARTESIAN_POINT('Ctrl Pts',(3.15902882320879,138.00950437876,14.377985337582));
#77675=CARTESIAN_POINT('Ctrl Pts',(3.15875699094376,138.012971234644,14.3811586206273));
#77676=CARTESIAN_POINT('Ctrl Pts',(3.15848469299766,138.016453972372,14.3843153897995));
#77677=CARTESIAN_POINT('Ctrl Pts',(3.15821197786757,138.019952394499,14.3874554757464));
#77678=CARTESIAN_POINT('Ctrl Pts',(3.15501496723241,138.060964027196,14.4242663712924));
#77679=CARTESIAN_POINT('Ctrl Pts',(3.15176125240872,138.104136728251,14.4587859943268));
#77680=CARTESIAN_POINT('Ctrl Pts',(3.14851580474113,138.149165919676,14.4907883258101));
#77681=CARTESIAN_POINT('Ctrl Pts',(3.14527359382322,138.194150202591,14.5227587407299));
#77682=CARTESIAN_POINT('Ctrl Pts',(3.14203997002484,138.240987117066,14.552217206911));
#77683=CARTESIAN_POINT('Ctrl Pts',(3.13885943606447,138.2893573173,14.5789742687615));
#77684=CARTESIAN_POINT('Ctrl Pts',(3.13568081490621,138.337698427254,14.6057152386712));
#77685=CARTESIAN_POINT('Ctrl Pts',(3.13255535717331,138.387570931696,14.6297581791116));
#77686=CARTESIAN_POINT('Ctrl Pts',(3.12950375096041,138.438641819003,14.6509464862624));
#77687=CARTESIAN_POINT('Ctrl Pts',(3.126452771915,138.489702210198,14.6721304387827));
#77688=CARTESIAN_POINT('Ctrl Pts',(3.1234756124121,138.541960479639,14.6904608938436));
#77689=CARTESIAN_POINT('Ctrl Pts',(3.1205682308823,138.595069988531,14.7058132196658));
#77690=CARTESIAN_POINT('Ctrl Pts',(3.11765816577949,138.648228518594,14.7211797160009));
#77691=CARTESIAN_POINT('Ctrl Pts',(3.11481788186344,138.702239862291,14.7335623955975));
#77692=CARTESIAN_POINT('Ctrl Pts',(3.11201949749925,138.756742619446,14.7428699123261));
#77693=CARTESIAN_POINT('Ctrl Pts',(3.10921985102585,138.811269958082,14.7521816268706));
#77694=CARTESIAN_POINT('Ctrl Pts',(3.10646185266845,138.866289141069,14.7584150555775));
#77695=CARTESIAN_POINT('Ctrl Pts',(3.10369680928727,138.921424509622,14.7615163550724));
#77696=CARTESIAN_POINT('Ctrl Pts',(3.10092648080941,138.976665263774,14.764623582383));
#77697=CARTESIAN_POINT('Ctrl Pts',(3.09814856626772,139.032022539742,14.7645861327575));
#77698=CARTESIAN_POINT('Ctrl Pts',(3.09529919866355,139.087105474071,14.7613944447161));
#77699=CARTESIAN_POINT('Ctrl Pts',(3.09303102401316,139.130952998388,14.7588537736223));
#77700=CARTESIAN_POINT('Ctrl Pts',(3.09071710096498,139.17462632544,14.7543150943676));
#77701=CARTESIAN_POINT('Ctrl Pts',(3.08832258410537,139.217923813411,14.7477978745243));
#77702=CARTESIAN_POINT('Ctrl Pts',(3.08832153365373,139.217942807605,14.7477950154823));
#77703=CARTESIAN_POINT('Ctrl Pts',(3.08832048318658,139.217961801727,14.7477921560598));
#77704=CARTESIAN_POINT('Ctrl Pts',(3.08831943270391,139.217980795777,14.7477892962568));
#77705=CARTESIAN_POINT('Ctrl Pts',(3.08556654185288,139.267756530636,14.7402949075103));
#77706=CARTESIAN_POINT('Ctrl Pts',(3.0826997512446,139.317223062877,14.7301523923613));
#77707=CARTESIAN_POINT('Ctrl Pts',(3.07977920653119,139.366089589428,14.7174316092589));
#77708=CARTESIAN_POINT('Ctrl Pts',(3.07950737589646,139.37063785704,14.7162476182968));
#77709=CARTESIAN_POINT('Ctrl Pts',(3.07923507958909,139.375180901625,14.7150413192777));
#77710=CARTESIAN_POINT('Ctrl Pts',(3.0789623661053,139.379718473696,14.7138127858175));
#77711=CARTESIAN_POINT('Ctrl Pts',(3.0757653562098,139.432912260124,14.6994107343506));
#77712=CARTESIAN_POINT('Ctrl Pts',(3.07251164249836,139.485358235846,14.6819491181184));
#77713=CARTESIAN_POINT('Ctrl Pts',(3.06926619619694,139.53670109826,14.661560649424));
#77714=CARTESIAN_POINT('Ctrl Pts',(3.06602398663132,139.587992755612,14.6411925144774));
#77715=CARTESIAN_POINT('Ctrl Pts',(3.0627903644374,139.638183685255,14.6179036707393));
#77716=CARTESIAN_POINT('Ctrl Pts',(3.05960983216241,139.68694123977,14.5918591061032));
#77717=CARTESIAN_POINT('Ctrl Pts',(3.05643121267842,139.735669471203,14.5658302048229));
#77718=CARTESIAN_POINT('Ctrl Pts',(3.05330575669995,139.782966131404,14.537049004985));
#77719=CARTESIAN_POINT('Ctrl Pts',(3.05025415211496,139.828518712385,14.5057098269839));
#77720=CARTESIAN_POINT('Ctrl Pts',(3.04720317468954,139.874061931492,14.474377089747));
#77721=CARTESIAN_POINT('Ctrl Pts',(3.04422601667987,139.917861750206,14.4404874154542));
#77722=CARTESIAN_POINT('Ctrl Pts',(3.04131863629093,139.95962508268,14.4042639462185));
#77723=CARTESIAN_POINT('Ctrl Pts',(3.03840857232731,140.00142696361,14.3680070419409));
#77724=CARTESIAN_POINT('Ctrl Pts',(3.03556828919654,140.041188441112,14.3294119289375));
#77725=CARTESIAN_POINT('Ctrl Pts',(3.03276990503546,140.078636337172,14.2887322372334));
#77726=CARTESIAN_POINT('Ctrl Pts',(3.02997025876238,140.116101122779,14.2480341983959));
#77727=CARTESIAN_POINT('Ctrl Pts',(3.02721226002056,140.151249940328,14.2052495210673));
#77728=CARTESIAN_POINT('Ctrl Pts',(3.02444721546737,140.183833332194,14.1606641943811));
#77729=CARTESIAN_POINT('Ctrl Pts',(3.02167688582266,140.216479003784,14.1159936475375));
#77730=CARTESIAN_POINT('Ctrl Pts',(3.0188989693198,140.246548902012,14.0695153461368));
#77731=CARTESIAN_POINT('Ctrl Pts',(3.01604959882231,140.27382246456,14.0215521186743));
#77732=CARTESIAN_POINT('Ctrl Pts',(3.01378142952579,140.295532894015,13.9833722049044));
#77733=CARTESIAN_POINT('Ctrl Pts',(3.0114675115503,140.315471807703,13.9442520438436));
#77734=CARTESIAN_POINT('Ctrl Pts',(3.00907299981926,140.333545898687,13.9043714450552));
#77735=CARTESIAN_POINT('Ctrl Pts',(3.00907194934552,140.333553827802,13.9043539494123));
#77736=CARTESIAN_POINT('Ctrl Pts',(3.00907089885626,140.333561756558,13.9043364536229));
#77737=CARTESIAN_POINT('Ctrl Pts',(3.00906984835148,140.333569684956,13.9043189576868));
#77738=CARTESIAN_POINT('Ctrl Pts',(3.00631696071253,140.354346352467,13.8584701931279));
#77739=CARTESIAN_POINT('Ctrl Pts',(3.00345017312882,140.372732489355,13.811440968349));
#77740=CARTESIAN_POINT('Ctrl Pts',(3.00052963124722,140.388628595016,13.7635133215497));
#77741=CARTESIAN_POINT('Ctrl Pts',(3.00025780009716,140.390108134382,13.7590524276891));
#77742=CARTESIAN_POINT('Ctrl Pts',(2.99998550327013,140.391566111854,13.754583786826));
#77743=CARTESIAN_POINT('Ctrl Pts',(2.99971278926276,140.39300245355,13.7501076483702));
#77744=CARTESIAN_POINT('Ctrl Pts',(2.99651578162392,140.409840588926,13.697634183683));
#77745=CARTESIAN_POINT('Ctrl Pts',(2.99326206992987,140.423704400013,13.6441246280831));
#77746=CARTESIAN_POINT('Ctrl Pts',(2.99001662553576,140.434512062875,13.5899493279236));
#77747=CARTESIAN_POINT('Ctrl Pts',(2.98677441787933,140.44530894707,13.5358280577253));
#77748=CARTESIAN_POINT('Ctrl Pts',(2.98354079748535,140.453056136228,13.4810423815984));
#77749=CARTESIAN_POINT('Ctrl Pts',(2.98036026710783,140.457711212427,13.4259611832007));
#77750=CARTESIAN_POINT('Ctrl Pts',(2.97718164951125,140.462363489049,13.3709131108083));
#77751=CARTESIAN_POINT('Ctrl Pts',(2.97405619551912,140.463927505734,13.3155698631984));
#77752=CARTESIAN_POINT('Ctrl Pts',(2.97100459329227,140.462396412643,13.2602993722482));
#77753=CARTESIAN_POINT('Ctrl Pts',(2.96795361820384,140.46086563421,13.2050402400026));
#77754=CARTESIAN_POINT('Ctrl Pts',(2.96497646290531,140.456240988816,13.1498538608409));
#77755=CARTESIAN_POINT('Ctrl Pts',(2.96206908591755,140.448550375984,13.09510753903));
#77756=CARTESIAN_POINT('Ctrl Pts',(2.9591590252783,140.440852664339,13.0403106836803));
#77757=CARTESIAN_POINT('Ctrl Pts',(2.9563187461703,140.430083150869,12.9859547730942));
#77758=CARTESIAN_POINT('Ctrl Pts',(2.95352036704958,140.41630614684,12.932406982302));
#77759=CARTESIAN_POINT('Ctrl Pts',(2.95072072578499,140.402522929014,12.8788350400229));
#77760=CARTESIAN_POINT('Ctrl Pts',(2.94796273307699,140.385729194159,12.8260721004516));
#77761=CARTESIAN_POINT('Ctrl Pts',(2.94519769584247,140.366029308712,12.7744830271846));
#77762=CARTESIAN_POINT('Ctrl Pts',(2.94242737340597,140.346291768121,12.7227953445142));
#77763=CARTESIAN_POINT('Ctrl Pts',(2.93964946540878,140.323636487067,12.6722863488327));
#77764=CARTESIAN_POINT('Ctrl Pts',(2.93680010481051,140.298214460992,12.623316685582));
#77765=CARTESIAN_POINT('Ctrl Pts',(2.9345318977506,140.277977493071,12.5843348396288));
#77766=CARTESIAN_POINT('Ctrl Pts',(2.93221794105132,140.255988081874,12.5463284777213));
#77767=CARTESIAN_POINT('Ctrl Pts',(2.92982338745721,140.232346399278,12.5094736904392));
#77768=CARTESIAN_POINT('Ctrl Pts',(2.92982233699319,140.232336027935,12.5094575226541));
#77769=CARTESIAN_POINT('Ctrl Pts',(2.92982128651367,140.232325656274,12.5094413550901));
#77770=CARTESIAN_POINT('Ctrl Pts',(2.92982023601862,140.232315284295,12.5094251877472));
#77771=CARTESIAN_POINT('Ctrl Pts',(2.92706734763268,140.205134860668,12.4670576479171));
#77772=CARTESIAN_POINT('Ctrl Pts',(2.92420055875117,140.175663861234,12.4260544440134));
#77773=CARTESIAN_POINT('Ctrl Pts',(2.92128001475791,140.144084878576,12.3866524428245));
#77774=CARTESIAN_POINT('Ctrl Pts',(2.92100817781079,140.141145585671,12.3829850028755));
#77775=CARTESIAN_POINT('Ctrl Pts',(2.92073587516046,140.138188065819,12.3793314465479));
#77776=CARTESIAN_POINT('Ctrl Pts',(2.92046315530633,140.135212488172,12.3756919714781));
#77777=CARTESIAN_POINT('Ctrl Pts',(2.91726613944558,140.100330653251,12.3330274593544));
#77778=CARTESIAN_POINT('Ctrl Pts',(2.91401241847817,140.062961948118,12.2922957355906));
#77779=CARTESIAN_POINT('Ctrl Pts',(2.91076696397492,140.023372690231,12.2537668521489));
#77780=CARTESIAN_POINT('Ctrl Pts',(2.90752474626434,139.983822915941,12.2152763947604));
#77781=CARTESIAN_POINT('Ctrl Pts',(2.90429111498613,139.942057221426,12.1789840897379));
#77782=CARTESIAN_POINT('Ctrl Pts',(2.90111057316057,139.898362124081,12.1451261224966));
#77783=CARTESIAN_POINT('Ctrl Pts',(2.89793194418588,139.854693305971,12.1112885182142));
#77784=CARTESIAN_POINT('Ctrl Pts',(2.89480647825229,139.809097471513,12.0798822067063));
#77785=CARTESIAN_POINT('Ctrl Pts',(2.89175486378769,139.761879679908,12.0511130056982));
#77786=CARTESIAN_POINT('Ctrl Pts',(2.88870387654282,139.714671593307,12.0223497178258));
#77787=CARTESIAN_POINT('Ctrl Pts',(2.88572670878814,139.665842222438,11.9962224953458));
#77788=CARTESIAN_POINT('Ctrl Pts',(2.88281931929704,139.615714995229,11.9729076517383));
#77789=CARTESIAN_POINT('Ctrl Pts',(2.87990924633403,139.565541501427,11.9495712889198));
#77790=CARTESIAN_POINT('Ctrl Pts',(2.87706895484425,139.51406772366,11.9290526836133));
#77791=CARTESIAN_POINT('Ctrl Pts',(2.87427056353783,139.461636780811,11.9114975209264));
#77792=CARTESIAN_POINT('Ctrl Pts',(2.87147091017097,139.409182191871,11.8939344409492));
#77793=CARTESIAN_POINT('Ctrl Pts',(2.86871290555125,139.355769533193,11.879337823445));
#77794=CARTESIAN_POINT('Ctrl Pts',(2.86594785687873,139.301761764499,11.8678184808448));
#77795=CARTESIAN_POINT('Ctrl Pts',(2.86317752323033,139.247650768054,11.8562771207486));
#77796=CARTESIAN_POINT('Ctrl Pts',(2.86039960449443,139.192942405235,11.847825383046));
#77797=CARTESIAN_POINT('Ctrl Pts',(2.85755023400243,139.138021450999,11.8425326536085));
#77798=CARTESIAN_POINT('Ctrl Pts',(2.85528208892008,139.094303481496,11.8383195552138));
#77799=CARTESIAN_POINT('Ctrl Pts',(2.85296819755423,139.050451267159,11.836107494406));
#77800=CARTESIAN_POINT('Ctrl Pts',(2.85057371610521,139.00666704191,11.8359081545861));
#77801=CARTESIAN_POINT('Ctrl Pts',(2.8505726657136,139.006647835003,11.8359080671414));
#77802=CARTESIAN_POINT('Ctrl Pts',(2.85057161530649,139.006628628109,11.8359079800836));
#77803=CARTESIAN_POINT('Ctrl Pts',(2.85057056488386,139.006609421227,11.8359078934127));
#77804=CARTESIAN_POINT('Ctrl Pts',(2.84781766447786,138.95627288889,11.8356807503924));
#77805=CARTESIAN_POINT('Ctrl Pts',(2.8449508656128,138.905835826224,11.8381178567553));
#77806=CARTESIAN_POINT('Ctrl Pts',(2.84203031428587,138.855596313128,11.843194772491));
#77807=CARTESIAN_POINT('Ctrl Pts',(2.8417584925555,138.850920418115,11.8436672915005));
#77808=CARTESIAN_POINT('Ctrl Pts',(2.84148620519934,138.846246263447,11.8441626542865));
#77809=CARTESIAN_POINT('Ctrl Pts',(2.8412135007088,138.841574106924,11.8446808263642));
#77810=CARTESIAN_POINT('Ctrl Pts',(2.83801649368961,138.786800835056,11.8507555329688));
#77811=CARTESIAN_POINT('Ctrl Pts',(2.83476278494475,138.732297363719,11.8599683052966));
#77812=CARTESIAN_POINT('Ctrl Pts',(2.83151734501095,138.678435145453,11.8722424839325));
#77813=CARTESIAN_POINT('Ctrl Pts',(2.82827514173831,138.62462664371,11.8845044215908));
#77814=CARTESIAN_POINT('Ctrl Pts',(2.82504152722837,138.571457979768,11.8998213288386));
#77815=CARTESIAN_POINT('Ctrl Pts',(2.8218610030209,138.519283168349,11.9180811785138));
#77816=CARTESIAN_POINT('Ctrl Pts',(2.81868239155011,138.467139734359,11.936330046891));
#77817=CARTESIAN_POINT('Ctrl Pts',(2.81555694396305,138.415988895149,11.957518199297));
#77818=CARTESIAN_POINT('Ctrl Pts',(2.81250534692587,138.366169262362,11.9815015347655));
#77819=CARTESIAN_POINT('Ctrl Pts',(2.80945437701603,138.316359867904,12.0054799414688));
#77820=CARTESIAN_POINT('Ctrl Pts',(2.80647722567327,138.267881168738,12.0322523984068));
#77821=CARTESIAN_POINT('Ctrl Pts',(2.80356984975818,138.221057003936,12.0616433454123));
#77822=CARTESIAN_POINT('Ctrl Pts',(2.80065979029537,138.174189619789,12.0910614206638));
#77823=CARTESIAN_POINT('Ctrl Pts',(2.79781950945779,138.128979964023,12.1231029482391));
#77824=CARTESIAN_POINT('Ctrl Pts',(2.79502112402402,138.085736878694,12.1575591876438));
#77825=CARTESIAN_POINT('Ctrl Pts',(2.79222147647836,138.042474290116,12.1920309673058));
#77826=CARTESIAN_POINT('Ctrl Pts',(2.78946347288055,138.001180314522,12.2289198602271));
#77827=CARTESIAN_POINT('Ctrl Pts',(2.78669841868601,137.962145316382,12.2679815116619));
#77828=CARTESIAN_POINT('Ctrl Pts',(2.78392807947884,137.923035708326,12.3071178239556));
#77829=CARTESIAN_POINT('Ctrl Pts',(2.78115014858955,137.886194213387,12.3484355025929));
#77830=CARTESIAN_POINT('Ctrl Pts',(2.77830075810428,137.851888291559,12.3916493575631));
#77831=CARTESIAN_POINT('Ctrl Pts',(2.77603263486686,137.824580676515,12.4260477136829));
#77832=CARTESIAN_POINT('Ctrl Pts',(2.77371876190569,137.798879365393,12.4616467894858));
#77833=CARTESIAN_POINT('Ctrl Pts',(2.77132429694915,137.7749041258,12.4982832225735));
#77834=CARTESIAN_POINT('Ctrl Pts',(2.7713232463534,137.774893606421,12.4982992971795));
#77835=CARTESIAN_POINT('Ctrl Pts',(2.77132219574214,137.774883087374,12.4983153719853));
#77836=CARTESIAN_POINT('Ctrl Pts',(2.77132114511536,137.774872568658,12.498331446991));
#77837=CARTESIAN_POINT('Ctrl Pts',(2.76853889632218,137.747017116706,12.5409009551319));
#77838=CARTESIAN_POINT('Ctrl Pts',(2.76564074785638,137.721394723939,12.5850279057137));
#77839=CARTESIAN_POINT('Ctrl Pts',(2.76268845048957,137.698146050023,12.6304457161441));
#77840=CARTESIAN_POINT('Ctrl Pts',(2.76238418499472,137.69575002808,12.6351265022738));
#77841=CARTESIAN_POINT('Ctrl Pts',(2.76207934435818,137.693379216241,12.639820953662));
#77842=CARTESIAN_POINT('Ctrl Pts',(2.76177399617581,137.691033766025,12.6445287472006));
#77843=CARTESIAN_POINT('Ctrl Pts',(2.75849865503538,137.665875110983,12.6950272624956));
#77844=CARTESIAN_POINT('Ctrl Pts',(2.75516560230959,137.643634301116,12.747067073688));
#77845=CARTESIAN_POINT('Ctrl Pts',(2.75184352051216,137.624454846283,12.8002776550356));
#77846=CARTESIAN_POINT('Ctrl Pts',(2.74854042393741,137.605384999293,12.8531841455156));
#77847=CARTESIAN_POINT('Ctrl Pts',(2.7452485086563,137.589341192048,12.9072480674698));
#77848=CARTESIAN_POINT('Ctrl Pts',(2.74201324571513,137.576426943074,12.9620999662645));
#77849=CARTESIAN_POINT('Ctrl Pts',(2.73875008977143,137.563401353171,13.0174247738086));
#77850=CARTESIAN_POINT('Ctrl Pts',(2.73554475485694,137.55355942859,13.0735512801728));
#77851=CARTESIAN_POINT('Ctrl Pts',(2.73241746689613,137.546972783191,13.1300943074508));
#77852=CARTESIAN_POINT('Ctrl Pts',(2.7292901789353,137.540386137791,13.1866373347289));
#77853=CARTESIAN_POINT('Ctrl Pts',(2.72624093881871,137.537054835619,13.2435969411206));
#77854=CARTESIAN_POINT('Ctrl Pts',(2.72326232145936,137.537016258812,13.3005808617436));
#77855=CARTESIAN_POINT('Ctrl Pts',(2.65409617475124,137.536500110378,13.3005683984462));
#77856=CARTESIAN_POINT('Ctrl Pts',(2.65466310222895,137.53649618178,13.2904531293485));
#77857=CARTESIAN_POINT('Ctrl Pts',(2.65522685214119,137.536597123654,13.2803379125779));
#77858=CARTESIAN_POINT('Ctrl Pts',(2.65629969032862,137.536991033323,13.2609808948677));
#77859=CARTESIAN_POINT('Ctrl Pts',(2.65680928418378,137.537266724753,13.2517392689034));
#77860=CARTESIAN_POINT('Ctrl Pts',(2.65798864352025,137.538111914222,13.230243698703));
#77861=CARTESIAN_POINT('Ctrl Pts',(2.6586562914533,137.538747942181,13.2179929681791));
#77862=CARTESIAN_POINT('Ctrl Pts',(2.66005823903909,137.540418745327,13.1921024513624));
#77863=CARTESIAN_POINT('Ctrl Pts',(2.6607913037575,137.54149087262,13.1784662076472));
#77864=CARTESIAN_POINT('Ctrl Pts',(2.6625813274488,137.544599966471,13.144943433684));
#77865=CARTESIAN_POINT('Ctrl Pts',(2.66363146053399,137.546853526745,13.1250795199141));
#77866=CARTESIAN_POINT('Ctrl Pts',(2.66834263008991,137.558919300866,13.0352063348586));
#77867=CARTESIAN_POINT('Ctrl Pts',(2.67185817974909,137.573389465835,12.9659146751024));
#77868=CARTESIAN_POINT('Ctrl Pts',(2.67760590621929,137.605673846808,12.852922305549));
#77869=CARTESIAN_POINT('Ctrl Pts',(2.67986873855879,137.620687616564,12.8085518927537));
#77870=CARTESIAN_POINT('Ctrl Pts',(2.68446266394564,137.655140256846,12.7208335179032));
#77871=CARTESIAN_POINT('Ctrl Pts',(2.68679168278632,137.674613117955,12.6775606887324));
#77872=CARTESIAN_POINT('Ctrl Pts',(2.69017044385885,137.704876242449,12.6181966807565));
#77873=CARTESIAN_POINT('Ctrl Pts',(2.69115674512985,137.713937278149,12.6012554597535));
#77874=CARTESIAN_POINT('Ctrl Pts',(2.69293514062228,137.730594946282,12.5715331521187));
#77875=CARTESIAN_POINT('Ctrl Pts',(2.69372056735556,137.738057906698,12.5586800566001));
#77876=CARTESIAN_POINT('Ctrl Pts',(2.69496257456362,137.749989265911,12.5388336372937));
#77877=CARTESIAN_POINT('Ctrl Pts',(2.69541111258585,137.754323777508,12.5317605783388));
#77878=CARTESIAN_POINT('Ctrl Pts',(2.69626906594014,137.762655742181,12.5184203879017));
#77879=CARTESIAN_POINT('Ctrl Pts',(2.69667774087347,137.766641181133,12.5121462589585));
#77880=CARTESIAN_POINT('Ctrl Pts',(2.6976003643726,137.775679471678,12.4981542605646));
#77881=CARTESIAN_POINT('Ctrl Pts',(2.69811590052295,137.780757850923,12.4904532633158));
#77882=CARTESIAN_POINT('Ctrl Pts',(2.69996300968592,137.799066420869,12.4632526940456));
#77883=CARTESIAN_POINT('Ctrl Pts',(2.701316989524,137.812693799748,12.4440260628534));
#77884=CARTESIAN_POINT('Ctrl Pts',(2.70962298922062,137.897919974233,12.3297347111804));
#77885=CARTESIAN_POINT('Ctrl Pts',(2.7169600934264,137.980432191215,12.2433642657711));
#77886=CARTESIAN_POINT('Ctrl Pts',(2.72717272619952,138.114418587096,12.1335888538252));
#77887=CARTESIAN_POINT('Ctrl Pts',(2.73030172564423,138.158219121381,12.1015946579821));
#77888=CARTESIAN_POINT('Ctrl Pts',(2.73440065065334,138.219574040901,12.0618054945042));
#77889=CARTESIAN_POINT('Ctrl Pts',(2.73545010890919,138.235648984453,12.0518181689181));
#77890=CARTESIAN_POINT('Ctrl Pts',(2.73722048368912,138.263386625297,12.0353217114875));
#77891=CARTESIAN_POINT('Ctrl Pts',(2.73794702910959,138.274952672293,12.0286555044602));
#77892=CARTESIAN_POINT('Ctrl Pts',(2.73932551419404,138.297240955656,12.016212534551));
#77893=CARTESIAN_POINT('Ctrl Pts',(2.73997834871232,138.307947208204,12.0104095702686));
#77894=CARTESIAN_POINT('Ctrl Pts',(2.7416862026952,138.33634314525,11.9954739917205));
#77895=CARTESIAN_POINT('Ctrl Pts',(2.74273328579147,138.354149177648,11.9865673627086));
#77896=CARTESIAN_POINT('Ctrl Pts',(2.74680045128104,138.424776792109,11.9530229530751));
#77897=CARTESIAN_POINT('Ctrl Pts',(2.74972684311173,138.478870596431,11.9311852117206));
#77898=CARTESIAN_POINT('Ctrl Pts',(2.75658664971136,138.61082545062,11.8868752966019));
#77899=CARTESIAN_POINT('Ctrl Pts',(2.76045455453737,138.689525383751,11.8675254566008));
#77900=CARTESIAN_POINT('Ctrl Pts',(2.76691916346528,138.818955910378,11.8468752272363));
#77901=CARTESIAN_POINT('Ctrl Pts',(2.76943850204505,138.868861896941,11.8415245925354));
#77902=CARTESIAN_POINT('Ctrl Pts',(2.7727361839293,138.931476252696,11.838051162252));
#77903=CARTESIAN_POINT('Ctrl Pts',(2.77340375145205,138.944021190969,11.8375170906944));
#77904=CARTESIAN_POINT('Ctrl Pts',(2.77450047489231,138.964380308864,11.8369126730385));
#77905=CARTESIAN_POINT('Ctrl Pts',(2.77492441769269,138.972191155141,11.8367433746979));
#77906=CARTESIAN_POINT('Ctrl Pts',(2.77578175847501,138.987857464013,11.836529291057));
#77907=CARTESIAN_POINT('Ctrl Pts',(2.77621517565434,138.995712668179,11.8364851999461));
#77908=CARTESIAN_POINT('Ctrl Pts',(2.77736132189666,139.016329295621,11.8365354583956));
#77909=CARTESIAN_POINT('Ctrl Pts',(2.77807936048492,139.029089544468,11.8367334876793));
#77910=CARTESIAN_POINT('Ctrl Pts',(2.78160655630213,139.091117674292,11.83850775197));
#77911=CARTESIAN_POINT('Ctrl Pts',(2.7845143431464,139.140283790947,11.84240551233));
#77912=CARTESIAN_POINT('Ctrl Pts',(2.79305492842287,139.281956325216,11.8608713552696));
#77913=CARTESIAN_POINT('Ctrl Pts',(2.79875424541355,139.373391602539,11.881842220141));
#77914=CARTESIAN_POINT('Ctrl Pts',(2.80715768816329,139.509211580132,11.9270503022962));
#77915=CARTESIAN_POINT('Ctrl Pts',(2.81000767554148,139.555402444196,11.9450770447013));
#77916=CARTESIAN_POINT('Ctrl Pts',(2.81381268079047,139.617388208491,11.9729720312145));
#77917=CARTESIAN_POINT('Ctrl Pts',(2.81483299250233,139.634039122419,11.9808465347684));
#77918=CARTESIAN_POINT('Ctrl Pts',(2.81656942509919,139.662416505644,11.9949281703905));
#77919=CARTESIAN_POINT('Ctrl Pts',(2.81729065503355,139.674215078387,12.000984160351));
#77920=CARTESIAN_POINT('Ctrl Pts',(2.8187593730443,139.698257269211,12.0137403928848));
#77921=CARTESIAN_POINT('Ctrl Pts',(2.81950618456959,139.710490644127,12.0204570918312));
#77922=CARTESIAN_POINT('Ctrl Pts',(2.82141990454456,139.741841969805,12.0382587321009));
#77923=CARTESIAN_POINT('Ctrl Pts',(2.82257742735777,139.760808595488,12.049603709255));
#77924=CARTESIAN_POINT('Ctrl Pts',(2.82975714474677,139.878225878183,12.1234986280291));
#77925=CARTESIAN_POINT('Ctrl Pts',(2.83533651420647,139.969157301158,12.1971981830322));
#77926=CARTESIAN_POINT('Ctrl Pts',(2.84325672149494,140.082172223105,12.3136835617332));
#77927=CARTESIAN_POINT('Ctrl Pts',(2.84550338950116,140.112412532608,12.3479208178204));
#77928=CARTESIAN_POINT('Ctrl Pts',(2.84920294174542,140.158047288461,12.4047348788046));
#77929=CARTESIAN_POINT('Ctrl Pts',(2.85060947145878,140.174496691428,12.426426586926));
#77930=CARTESIAN_POINT('Ctrl Pts',(2.85260507176628,140.196392294626,12.4570371998088));
#77931=CARTESIAN_POINT('Ctrl Pts',(2.8531628421868,140.202363019898,12.4655756709428));
#77932=CARTESIAN_POINT('Ctrl Pts',(2.85412822195039,140.212430002699,12.4803044313401));
#77933=CARTESIAN_POINT('Ctrl Pts',(2.85453288178863,140.2165711873,12.4864633496416));
#77934=CARTESIAN_POINT('Ctrl Pts',(2.85541341923085,140.225409982253,12.4998271485266));
#77935=CARTESIAN_POINT('Ctrl Pts',(2.85589024979634,140.230090984303,12.5070420064163));
#77936=CARTESIAN_POINT('Ctrl Pts',(2.8572580028558,140.243230298316,12.5276900461691));
#77937=CARTESIAN_POINT('Ctrl Pts',(2.85815794375411,140.251533787627,12.5412198102772));
#77938=CARTESIAN_POINT('Ctrl Pts',(2.86345950924891,140.298599510435,12.6207839209644));
#77939=CARTESIAN_POINT('Ctrl Pts',(2.86807804453755,140.332349071655,12.6896398307197));
#77940=CARTESIAN_POINT('Ctrl Pts',(2.8768767107194,140.386155422329,12.8254120832268));
#77941=CARTESIAN_POINT('Ctrl Pts',(2.88104703903556,140.407124255955,12.8917559498268));
#77942=CARTESIAN_POINT('Ctrl Pts',(2.88758115878448,140.433223739487,13.0008021880647));
#77943=CARTESIAN_POINT('Ctrl Pts',(2.89001846051829,140.441331184998,13.0426781319569));
#77944=CARTESIAN_POINT('Ctrl Pts',(2.89337888469893,140.450177806088,13.1022014841772));
#77945=CARTESIAN_POINT('Ctrl Pts',(2.89434870276218,140.452444387427,13.1195969475888));
#77946=CARTESIAN_POINT('Ctrl Pts',(2.89602712253877,140.455859424193,13.1500737646765));
#77947=CARTESIAN_POINT('Ctrl Pts',(2.89673995344613,140.457145557949,13.1631373766263));
#77948=CARTESIAN_POINT('Ctrl Pts',(2.89821668761868,140.459463330673,13.1904424254939));
#77949=CARTESIAN_POINT('Ctrl Pts',(2.89897950928965,140.46046266441,13.2046852522793));
#77950=CARTESIAN_POINT('Ctrl Pts',(2.90099187817338,140.46256615626,13.2426048687142));
#77951=CARTESIAN_POINT('Ctrl Pts',(2.90223001924217,140.463303874755,13.26629814552));
#77952=CARTESIAN_POINT('Ctrl Pts',(2.9094568083219,140.464261335976,13.4064165844386));
#77953=CARTESIAN_POINT('Ctrl Pts',(2.91501336329876,140.45116397503,13.5225085848602));
#77954=CARTESIAN_POINT('Ctrl Pts',(2.92283902460782,140.414411526104,13.6783984440591));
#77955=CARTESIAN_POINT('Ctrl Pts',(2.92499599039625,140.402471864323,13.7204968826564));
#77956=CARTESIAN_POINT('Ctrl Pts',(2.92856583338239,140.380302880672,13.7871324598516));
#77957=CARTESIAN_POINT('Ctrl Pts',(2.9299362479539,140.371259397808,13.8120366964607));
#77958=CARTESIAN_POINT('Ctrl Pts',(2.9318887634983,140.357762059052,13.8462791356142));
#77959=CARTESIAN_POINT('Ctrl Pts',(2.93244131394557,140.353877195534,13.8558374134105));
#77960=CARTESIAN_POINT('Ctrl Pts',(2.93340077535806,140.347029585564,13.8721874161956));
#77961=CARTESIAN_POINT('Ctrl Pts',(2.93380484041928,140.344115787591,13.8789990427618));
#77962=CARTESIAN_POINT('Ctrl Pts',(2.93468801771395,140.337685040656,13.8937220988875));
#77963=CARTESIAN_POINT('Ctrl Pts',(2.93516814755004,140.33414958617,13.9016245280045));
#77964=CARTESIAN_POINT('Ctrl Pts',(2.93655451516751,140.323821717461,13.9241705520232));
#77965=CARTESIAN_POINT('Ctrl Pts',(2.93747013309247,140.316857042938,13.9387333579756));
#77966=CARTESIAN_POINT('Ctrl Pts',(2.94208421657747,140.280971976747,14.0106847079453));
#77967=CARTESIAN_POINT('Ctrl Pts',(2.9459331378894,140.248536099458,14.066236497296));
#77968=CARTESIAN_POINT('Ctrl Pts',(2.9532518798441,140.180466565949,14.1669576837337));
#77969=CARTESIAN_POINT('Ctrl Pts',(2.95671175038683,140.145612332033,14.2125183613962));
#77970=CARTESIAN_POINT('Ctrl Pts',(2.96377187406115,140.067869740671,14.3026436146242));
#77971=CARTESIAN_POINT('Ctrl Pts',(2.96735488027574,140.024646320557,14.3467766592538));
#77972=CARTESIAN_POINT('Ctrl Pts',(2.97192116683008,139.964184379563,14.4011653561232));
#77973=CARTESIAN_POINT('Ctrl Pts',(2.97301007442118,139.949345356427,14.4139838895466));
#77974=CARTESIAN_POINT('Ctrl Pts',(2.97482649388754,139.923884265713,14.4350998019601));
#77975=CARTESIAN_POINT('Ctrl Pts',(2.97556036080566,139.913397368437,14.4435554036328));
#77976=CARTESIAN_POINT('Ctrl Pts',(2.97702583341629,139.892057794421,14.4602806765246));
#77977=CARTESIAN_POINT('Ctrl Pts',(2.97775721775671,139.881203237585,14.4685457749596));
#77978=CARTESIAN_POINT('Ctrl Pts',(2.97957384348168,139.853741406549,14.4888560345353));
#77979=CARTESIAN_POINT('Ctrl Pts',(2.98065155127362,139.836993233847,14.5007062260942));
#77980=CARTESIAN_POINT('Ctrl Pts',(2.98535763085779,139.761944831812,14.5514731919838));
#77981=CARTESIAN_POINT('Ctrl Pts',(2.98884420383262,139.701139044483,14.5865265017309));
#77982=CARTESIAN_POINT('Ctrl Pts',(2.99725695836799,139.54638388673,14.6614961549644));
#77983=CARTESIAN_POINT('Ctrl Pts',(3.00208917402969,139.45034000052,14.6962082373129));
#77984=CARTESIAN_POINT('Ctrl Pts',(3.00845945604121,139.329623909149,14.7260740875111));
#77985=CARTESIAN_POINT('Ctrl Pts',(3.0096316025172,139.307646032047,14.7309762539674));
#77986=CARTESIAN_POINT('Ctrl Pts',(3.01134622464625,139.27603424709,14.737265380843));
#77987=CARTESIAN_POINT('Ctrl Pts',(3.0118678853092,139.266485109035,14.7390664879663));
#77988=CARTESIAN_POINT('Ctrl Pts',(3.01275555679849,139.250369793641,14.7419401764803));
#77989=CARTESIAN_POINT('Ctrl Pts',(3.01311877650576,139.243813073562,14.7430633005873));
#77990=CARTESIAN_POINT('Ctrl Pts',(3.01396417515042,139.228641984634,14.7455556603524));
#77991=CARTESIAN_POINT('Ctrl Pts',(3.01444806219066,139.220023048526,14.7468925926079));
#77992=CARTESIAN_POINT('Ctrl Pts',(3.01585586906362,139.19511408884,14.7505286584277));
#77993=CARTESIAN_POINT('Ctrl Pts',(3.01678959482598,139.178797036445,14.7526301905503));
#77994=CARTESIAN_POINT('Ctrl Pts',(3.02181008430347,139.091915682594,14.762334001119));
#77995=CARTESIAN_POINT('Ctrl Pts',(3.02607930365139,139.020907767063,14.7650702033945));
#77996=CARTESIAN_POINT('Ctrl Pts',(3.03473190503188,138.877368272342,14.7601621163864));
#77997=CARTESIAN_POINT('Ctrl Pts',(3.03910234764817,138.805029774772,14.7522740813092));
#77998=CARTESIAN_POINT('Ctrl Pts',(3.04589242527088,138.690598122333,14.7310879924214));
#77999=CARTESIAN_POINT('Ctrl Pts',(3.04839359277293,138.647998876187,14.7212100903847));
#78000=CARTESIAN_POINT('Ctrl Pts',(3.05182366753431,138.588868195168,14.7046763825307));
#78001=CARTESIAN_POINT('Ctrl Pts',(3.05280195388958,138.571921231778,14.6996048397633));
#78002=CARTESIAN_POINT('Ctrl Pts',(3.05449005322213,138.542544676056,14.6902301005515));
#78003=CARTESIAN_POINT('Ctrl Pts',(3.05520424054462,138.530073686029,14.6860643495454));
#78004=CARTESIAN_POINT('Ctrl Pts',(3.05667926296593,138.504237892961,14.6770454954315));
#78005=CARTESIAN_POINT('Ctrl Pts',(3.05743908946801,138.490884236955,14.6721645391156));
#78006=CARTESIAN_POINT('Ctrl Pts',(3.05943294751541,138.455745629654,14.6587372663541));
#78007=CARTESIAN_POINT('Ctrl Pts',(3.06065596472053,138.434090504514,14.6498615858537));
#78008=CARTESIAN_POINT('Ctrl Pts',(3.06736980104744,138.314932599652,14.5976510984772));
#78009=CARTESIAN_POINT('Ctrl Pts',(3.07250587343878,138.222184622774,14.5442751730275));
#78010=CARTESIAN_POINT('Ctrl Pts',(3.08016700156831,138.095156833528,14.4513726205349));
#78011=CARTESIAN_POINT('Ctrl Pts',(3.08264732581614,138.055838084481,14.4193559852395));
#78012=CARTESIAN_POINT('Ctrl Pts',(3.08668044558145,137.996739474906,14.365899951849));
#78013=CARTESIAN_POINT('Ctrl Pts',(3.08817605995022,137.975802877911,14.3457984691542));
#78014=CARTESIAN_POINT('Ctrl Pts',(3.09027756541743,137.948013910521,14.3174827290039));
#78015=CARTESIAN_POINT('Ctrl Pts',(3.09084761813261,137.940632407218,14.309795091207));
#78016=CARTESIAN_POINT('Ctrl Pts',(3.09182708370348,137.928231132239,14.2965938632666));
#78017=CARTESIAN_POINT('Ctrl Pts',(3.09223331657872,137.923168228597,14.2911211677208));
#78018=CARTESIAN_POINT('Ctrl Pts',(3.09310845939597,137.912437544027,14.2793426545058));
#78019=CARTESIAN_POINT('Ctrl Pts',(3.09357819541395,137.906782492671,14.2730260042519));
#78020=CARTESIAN_POINT('Ctrl Pts',(3.09490608346451,137.891076360544,14.2551726172246));
#78021=CARTESIAN_POINT('Ctrl Pts',(3.09577249751711,137.881151113502,14.2435271583221));
#78022=CARTESIAN_POINT('Ctrl Pts',(3.10165636424834,137.815741043791,14.1642969007287));
#78023=CARTESIAN_POINT('Ctrl Pts',(3.10696111273656,137.766230359656,14.0920158234387));
#78024=CARTESIAN_POINT('Ctrl Pts',(3.11600860073425,137.692707403977,13.9608893736882));
#78025=CARTESIAN_POINT('Ctrl Pts',(3.11976527131541,137.665511789136,13.9040951885532));
#78026=CARTESIAN_POINT('Ctrl Pts',(3.12575861170288,137.627052130992,13.8083944407724));
#78027=CARTESIAN_POINT('Ctrl Pts',(3.12805351381581,137.613595248694,13.7704604725126));
#78028=CARTESIAN_POINT('Ctrl Pts',(3.13125763417118,137.59664053884,13.7155842872592));
#78029=CARTESIAN_POINT('Ctrl Pts',(3.13220780620945,137.591853244956,13.6990624373537));
#78030=CARTESIAN_POINT('Ctrl Pts',(3.13386404533131,137.583939621216,13.6698328969429));
#78031=CARTESIAN_POINT('Ctrl Pts',(3.13457400445591,137.580690452139,13.6571607353527));
#78032=CARTESIAN_POINT('Ctrl Pts',(3.1360559334785,137.574214301904,13.6304175299124));
#78033=CARTESIAN_POINT('Ctrl Pts',(3.13682663955094,137.571024714405,13.6163388283167));
#78034=CARTESIAN_POINT('Ctrl Pts',(3.13888713540599,137.562988404197,13.5782611420473));
#78035=CARTESIAN_POINT('Ctrl Pts',(3.14016448255719,137.558534624514,13.5541834988602));
#78036=CARTESIAN_POINT('Ctrl Pts',(3.14539148405244,137.542581743376,13.4539380260478));
#78037=CARTESIAN_POINT('Ctrl Pts',(3.14917702522996,137.536500000002,13.3770311563965));
#78038=CARTESIAN_POINT('Ctrl Pts',(3.1529262221125,137.5365,13.3000000000405));
#78039=CARTESIAN_POINT('Origin',(4.2,139.,13.3));
#78040=CARTESIAN_POINT('',(3.72552751600545,137.5365,13.2999999999998));
#78041=CARTESIAN_POINT('',(3.65157748137716,137.5365,13.3000000000035));
#78042=CARTESIAN_POINT('',(4.2,137.5365,13.3));
#78043=CARTESIAN_POINT('',(3.22392529813232,137.53661469332,13.2986845264305));
#78044=CARTESIAN_POINT('Ctrl Pts',(3.72552751600545,137.5365,13.2999999999998));
#78045=CARTESIAN_POINT('Ctrl Pts',(3.72552055759137,137.5365,13.3001317195931));
#78046=CARTESIAN_POINT('Ctrl Pts',(3.72551359830482,137.536500017726,13.3002634393025));
#78047=CARTESIAN_POINT('Ctrl Pts',(3.72491065267735,137.536503098796,13.3116741882147));
#78048=CARTESIAN_POINT('Ctrl Pts',(3.72430858380333,137.53663653343,13.3229524639633));
#78049=CARTESIAN_POINT('Ctrl Pts',(3.72329361321726,137.537076133077,13.3417436126553));
#78050=CARTESIAN_POINT('Ctrl Pts',(3.72288457083917,137.537309867579,13.3492579417754));
#78051=CARTESIAN_POINT('Ctrl Pts',(3.7220183172435,137.537922497249,13.3650392762235));
#78052=CARTESIAN_POINT('Ctrl Pts',(3.72156050455177,137.538313626764,13.3733053269853));
#78053=CARTESIAN_POINT('Ctrl Pts',(3.7202852417732,137.539588415186,13.3961423032577));
#78054=CARTESIAN_POINT('Ctrl Pts',(3.71946034626683,137.540619992297,13.4107036565694));
#78055=CARTESIAN_POINT('Ctrl Pts',(3.71432320836805,137.548314434174,13.5002829870594));
#78056=CARTESIAN_POINT('Ctrl Pts',(3.70979067888011,137.560541757334,13.5747044391791));
#78057=CARTESIAN_POINT('Ctrl Pts',(3.69908558943376,137.602774937851,13.7472999962083));
#78058=CARTESIAN_POINT('Ctrl Pts',(3.69295487081315,137.637483031646,13.8439377666827));
#78059=CARTESIAN_POINT('Ctrl Pts',(3.68579717125114,137.692383641285,13.9576793940163));
#78060=CARTESIAN_POINT('Ctrl Pts',(3.68446083742992,137.703291481434,13.9789328679809));
#78061=CARTESIAN_POINT('Ctrl Pts',(3.68234925070244,137.721588767213,14.012533187052));
#78062=CARTESIAN_POINT('Ctrl Pts',(3.68156261378719,137.72864813472,14.0250539829195));
#78063=CARTESIAN_POINT('Ctrl Pts',(3.68006564595427,137.742547286583,14.0488787691578));
#78064=CARTESIAN_POINT('Ctrl Pts',(3.67935436347111,137.749357901011,14.060198061938));
#78065=CARTESIAN_POINT('Ctrl Pts',(3.67770544614854,137.765625069086,14.0864237681303));
#78066=CARTESIAN_POINT('Ctrl Pts',(3.67677225942952,137.775200003886,14.1012545278744));
#78067=CARTESIAN_POINT('Ctrl Pts',(3.67359972327705,137.808992948077,14.151575141327));
#78068=CARTESIAN_POINT('Ctrl Pts',(3.67140842608218,137.83450470886,14.1861710682816));
#78069=CARTESIAN_POINT('Ctrl Pts',(3.66573573895202,137.905699734204,14.2743133111995));
#78070=CARTESIAN_POINT('Ctrl Pts',(3.66233265239016,137.953784496369,14.3257743966884));
#78071=CARTESIAN_POINT('Ctrl Pts',(3.65527363097964,138.060284532009,14.4244412734167));
#78072=CARTESIAN_POINT('Ctrl Pts',(3.65162457188126,138.119000895709,14.4710131626245));
#78073=CARTESIAN_POINT('Ctrl Pts',(3.64689703122542,138.194366934675,14.5219031118683));
#78074=CARTESIAN_POINT('Ctrl Pts',(3.64604841828823,138.207867439716,14.5306981010816));
#78075=CARTESIAN_POINT('Ctrl Pts',(3.64472167167265,138.22886214242,14.5438866679129));
#78076=CARTESIAN_POINT('Ctrl Pts',(3.64425315092351,138.236255219156,14.5484396421401));
#78077=CARTESIAN_POINT('Ctrl Pts',(3.64337380178454,138.250079308209,14.5567843633872));
#78078=CARTESIAN_POINT('Ctrl Pts',(3.64296404575968,138.256499469596,14.560593087611));
#78079=CARTESIAN_POINT('Ctrl Pts',(3.64197312341593,138.271978611614,14.5696166211277));
#78080=CARTESIAN_POINT('Ctrl Pts',(3.64138909004881,138.281064721753,14.5747837303755));
#78081=CARTESIAN_POINT('Ctrl Pts',(3.63926699591292,138.313981095788,14.5930388544123));
#78082=CARTESIAN_POINT('Ctrl Pts',(3.63769915866345,138.338118497709,14.6055589274622));
#78083=CARTESIAN_POINT('Ctrl Pts',(3.6334457770555,138.403541028122,14.637213004489));
#78084=CARTESIAN_POINT('Ctrl Pts',(3.63072142494503,138.445392932358,14.6551061035238));
#78085=CARTESIAN_POINT('Ctrl Pts',(3.6209558427848,138.597428799279,14.7118821814145));
#78086=CARTESIAN_POINT('Ctrl Pts',(3.61391890020323,138.711367617347,14.7395049836129));
#78087=CARTESIAN_POINT('Ctrl Pts',(3.60607251763857,138.849351620248,14.7558936943484));
#78088=CARTESIAN_POINT('Ctrl Pts',(3.60483865118399,138.871370705246,14.7580041026479));
#78089=CARTESIAN_POINT('Ctrl Pts',(3.60284807813009,138.907410190847,14.7606354313836));
#78090=CARTESIAN_POINT('Ctrl Pts',(3.60208220962205,138.92140459749,14.7614552740624));
#78091=CARTESIAN_POINT('Ctrl Pts',(3.60059865088163,138.948755351319,14.7626635667031));
#78092=CARTESIAN_POINT('Ctrl Pts',(3.59988045837982,138.962109463099,14.7630704175964));
#78093=CARTESIAN_POINT('Ctrl Pts',(3.59817440573133,138.99408991786,14.7636065761001));
#78094=CARTESIAN_POINT('Ctrl Pts',(3.59719198722265,139.012717031029,14.7635632741589));
#78095=CARTESIAN_POINT('Ctrl Pts',(3.59356873524607,139.082118683392,14.7620767930083));
#78096=CARTESIAN_POINT('Ctrl Pts',(3.5909978226926,139.132809921046,14.758346388967));
#78097=CARTESIAN_POINT('Ctrl Pts',(3.58355847560734,139.281477528068,14.7395878839013));
#78098=CARTESIAN_POINT('Ctrl Pts',(3.5788611716942,139.378229244989,14.7172453436941));
#78099=CARTESIAN_POINT('Ctrl Pts',(3.57181336461342,139.512631773826,14.6714537184059));
#78100=CARTESIAN_POINT('Ctrl Pts',(3.56964092242108,139.55265109264,14.6558218319845));
#78101=CARTESIAN_POINT('Ctrl Pts',(3.56672857643548,139.603273016283,14.6334346495559));
#78102=CARTESIAN_POINT('Ctrl Pts',(3.56606837805997,139.614559405581,14.6282706852905));
#78103=CARTESIAN_POINT('Ctrl Pts',(3.56502059078414,139.632143664744,14.6199531125627));
#78104=CARTESIAN_POINT('Ctrl Pts',(3.56463864604462,139.638487009202,14.6168964147185));
#78105=CARTESIAN_POINT('Ctrl Pts',(3.56383025074229,139.65176565834,14.6103792764037));
#78106=CARTESIAN_POINT('Ctrl Pts',(3.56340317861143,139.658695919349,14.606909330829));
#78107=CARTESIAN_POINT('Ctrl Pts',(3.56230071818509,139.676380609222,14.5978783087148));
#78108=CARTESIAN_POINT('Ctrl Pts',(3.56162074833845,139.687094055567,14.5922385893897));
#78109=CARTESIAN_POINT('Ctrl Pts',(3.55850035494803,139.735453641193,14.5660099913516));
#78110=CARTESIAN_POINT('Ctrl Pts',(3.5559844134253,139.77225065949,14.5439058246684));
#78111=CARTESIAN_POINT('Ctrl Pts',(3.54660646222448,139.903650575853,14.4568937409475));
#78112=CARTESIAN_POINT('Ctrl Pts',(3.53958601907467,139.991518692225,14.3825355455001));
#78113=CARTESIAN_POINT('Ctrl Pts',(3.53068345530036,140.096149901422,14.270452755276));
#78114=CARTESIAN_POINT('Ctrl Pts',(3.52848126669326,140.121372687485,14.2411943659893));
#78115=CARTESIAN_POINT('Ctrl Pts',(3.52535840073494,140.156190718643,14.1974158556493));
#78116=CARTESIAN_POINT('Ctrl Pts',(3.52440094497153,140.16672992276,14.1836704813028));
#78117=CARTESIAN_POINT('Ctrl Pts',(3.52273025812501,140.184871028997,14.1591200656308));
#78118=CARTESIAN_POINT('Ctrl Pts',(3.52201311119488,140.192575124548,14.1483933231709));
#78119=CARTESIAN_POINT('Ctrl Pts',(3.520526415383,140.208365060775,14.1257681424408));
#78120=CARTESIAN_POINT('Ctrl Pts',(3.51975798039364,140.216422809703,14.1138517759384));
#78121=CARTESIAN_POINT('Ctrl Pts',(3.51772762967691,140.23742019116,14.0817906784012));
#78122=CARTESIAN_POINT('Ctrl Pts',(3.51647738340998,140.25004364801,14.0614436007363));
#78123=CARTESIAN_POINT('Ctrl Pts',(3.51141730825231,140.299727651289,13.9767922718665));
#78124=CARTESIAN_POINT('Ctrl Pts',(3.50775942042999,140.332372005345,13.9100212336995));
#78125=CARTESIAN_POINT('Ctrl Pts',(3.49997472682672,140.391443554923,13.7615600108478));
#78126=CARTESIAN_POINT('Ctrl Pts',(3.49587678859058,140.416040595909,13.6794467112804));
#78127=CARTESIAN_POINT('Ctrl Pts',(3.4902068559564,140.438571477507,13.5702206049436));
#78128=CARTESIAN_POINT('Ctrl Pts',(3.48886331304834,140.443140912839,13.5446451007436));
#78129=CARTESIAN_POINT('Ctrl Pts',(3.48692857706182,140.448601916939,13.5085558129043));
#78130=CARTESIAN_POINT('Ctrl Pts',(3.48636524076321,140.450064366232,13.4981321823053));
#78131=CARTESIAN_POINT('Ctrl Pts',(3.48539139343094,140.45237283916,13.4802810493853));
#78132=CARTESIAN_POINT('Ctrl Pts',(3.48498391022247,140.453274607272,13.4728613175211));
#78133=CARTESIAN_POINT('Ctrl Pts',(3.48409820474165,140.455096506983,13.4568473815084));
#78134=CARTESIAN_POINT('Ctrl Pts',(3.48361903435778,140.455997365785,13.4482518426327));
#78135=CARTESIAN_POINT('Ctrl Pts',(3.48222001330599,140.458386037709,13.4233331643838));
#78136=CARTESIAN_POINT('Ctrl Pts',(3.48129033998743,140.459675783735,13.4069928279238));
#78137=CARTESIAN_POINT('Ctrl Pts',(3.47674120558153,140.464584533842,13.3278824813832));
#78138=CARTESIAN_POINT('Ctrl Pts',(3.47297848363,140.46443010861,13.2649486292002));
#78139=CARTESIAN_POINT('Ctrl Pts',(3.46229997926127,140.452577551596,13.0879354507405));
#78140=CARTESIAN_POINT('Ctrl Pts',(3.45540526651605,140.431531938995,12.9749198354831));
#78141=CARTESIAN_POINT('Ctrl Pts',(3.44766280692175,140.390852670363,12.8440782624796));
#78142=CARTESIAN_POINT('Ctrl Pts',(3.44641023310681,140.383698498533,12.8228057784297));
#78143=CARTESIAN_POINT('Ctrl Pts',(3.44439755376339,140.371262997021,12.7884647162484));
#78144=CARTESIAN_POINT('Ctrl Pts',(3.4436278935083,140.366277360269,12.7752936556342));
#78145=CARTESIAN_POINT('Ctrl Pts',(3.44214219432967,140.356205260591,12.7498026502038));
#78146=CARTESIAN_POINT('Ctrl Pts',(3.44142556662377,140.351139093871,12.7374762247398));
#78147=CARTESIAN_POINT('Ctrl Pts',(3.43973155704996,140.33867011977,12.7082788466883));
#78148=CARTESIAN_POINT('Ctrl Pts',(3.43875940668276,140.331115650545,12.6914749157925));
#78149=CARTESIAN_POINT('Ctrl Pts',(3.43523725161072,140.302305145296,12.630495311347));
#78150=CARTESIAN_POINT('Ctrl Pts',(3.43275185280457,140.279149989483,12.5872510200952));
#78151=CARTESIAN_POINT('Ctrl Pts',(3.42577804639236,140.206835073795,12.467114623918));
#78152=CARTESIAN_POINT('Ctrl Pts',(3.42143141091406,140.152605363204,12.3935511810349));
#78153=CARTESIAN_POINT('Ctrl Pts',(3.41437840618844,140.05720445989,12.2866573226237));
#78154=CARTESIAN_POINT('Ctrl Pts',(3.41176961318957,140.020479385239,12.2496831208837));
#78155=CARTESIAN_POINT('Ctrl Pts',(3.40835685791258,139.97229919986,12.2060928064908));
#78156=CARTESIAN_POINT('Ctrl Pts',(3.40767158892432,139.96261892614,12.1975647581915));
#78157=CARTESIAN_POINT('Ctrl Pts',(3.40655139896407,139.946818981303,12.1840122171201));
#78158=CARTESIAN_POINT('Ctrl Pts',(3.4061220620133,139.940768873303,12.1789073027083));
#78159=CARTESIAN_POINT('Ctrl Pts',(3.4052595336185,139.928634888969,12.1688363669593));
#78160=CARTESIAN_POINT('Ctrl Pts',(3.40482640688436,139.922551871954,12.1638697439615));
#78161=CARTESIAN_POINT('Ctrl Pts',(3.40368955868837,139.906602285339,12.1510598753505));
#78162=CARTESIAN_POINT('Ctrl Pts',(3.40298072234981,139.896674012335,12.1432948485353));
#78163=CARTESIAN_POINT('Ctrl Pts',(3.39941232385398,139.846701104864,12.1052404110541));
#78164=CARTESIAN_POINT('Ctrl Pts',(3.39644951353024,139.805219322734,12.0768997391778));
#78165=CARTESIAN_POINT('Ctrl Pts',(3.38860893858539,139.693293530767,12.0085959591534));
#78166=CARTESIAN_POINT('Ctrl Pts',(3.38368886121182,139.620838593996,11.9722422164872));
#78167=CARTESIAN_POINT('Ctrl Pts',(3.3754248025165,139.491336941169,11.9201959418631));
#78168=CARTESIAN_POINT('Ctrl Pts',(3.37202471328968,139.435654641086,11.9016161047724));
#78169=CARTESIAN_POINT('Ctrl Pts',(3.36762140413896,139.359927220255,11.8813123488158));
#78170=CARTESIAN_POINT('Ctrl Pts',(3.36652439028684,139.340750200544,11.8765845265348));
#78171=CARTESIAN_POINT('Ctrl Pts',(3.36476950223142,139.309576811633,11.8695653164109));
#78172=CARTESIAN_POINT('Ctrl Pts',(3.36410404781468,139.297637639231,11.8670334844503));
#78173=CARTESIAN_POINT('Ctrl Pts',(3.36271362796051,139.272448653474,11.8620202878826));
#78174=CARTESIAN_POINT('Ctrl Pts',(3.36198977215922,139.259193370751,11.8595720307994));
#78175=CARTESIAN_POINT('Ctrl Pts',(3.36024255922599,139.226867303336,11.8540620782963));
#78176=CARTESIAN_POINT('Ctrl Pts',(3.35922536853238,139.20776584591,11.8511940619226));
#78177=CARTESIAN_POINT('Ctrl Pts',(3.35522176623594,139.131561532493,11.8412904294161));
#78178=CARTESIAN_POINT('Ctrl Pts',(3.35232751344371,139.074120199961,11.837246053713));
#78179=CARTESIAN_POINT('Ctrl Pts',(3.3465261985009,138.956572231158,11.8359138209579));
#78180=CARTESIAN_POINT('Ctrl Pts',(3.3436294520061,138.896573086068,11.8389259736535));
#78181=CARTESIAN_POINT('Ctrl Pts',(3.33748065763914,138.771137308895,11.8529903141975));
#78182=CARTESIAN_POINT('Ctrl Pts',(3.33422941245165,138.705927835779,11.8648222421279));
#78183=CARTESIAN_POINT('Ctrl Pts',(3.32994244169614,138.625927337032,11.8850200725186));
#78184=CARTESIAN_POINT('Ctrl Pts',(3.32908333829389,138.6101736009,11.8892789475666));
#78185=CARTESIAN_POINT('Ctrl Pts',(3.32774357454516,138.586110586489,11.8962179841558));
#78186=CARTESIAN_POINT('Ctrl Pts',(3.32727282225491,138.577748154629,11.8987106772942));
#78187=CARTESIAN_POINT('Ctrl Pts',(3.32639180636825,138.562283055776,11.9034715492023));
#78188=CARTESIAN_POINT('Ctrl Pts',(3.32598266537213,138.555174690518,11.9057194426576));
#78189=CARTESIAN_POINT('Ctrl Pts',(3.32499671494542,138.538214984737,11.9112255361837));
#78190=CARTESIAN_POINT('Ctrl Pts',(3.32441711679906,138.528380690997,11.9145343287338));
#78191=CARTESIAN_POINT('Ctrl Pts',(3.32233104883395,138.493428383037,11.926709440084));
#78192=CARTESIAN_POINT('Ctrl Pts',(3.3207960514629,138.468519415094,11.9361561736659));
#78193=CARTESIAN_POINT('Ctrl Pts',(3.31666321124202,138.403146906964,11.9630115280814));
#78194=CARTESIAN_POINT('Ctrl Pts',(3.31402888426484,138.363188093868,11.9815759298846));
#78195=CARTESIAN_POINT('Ctrl Pts',(3.30428824606432,138.219539229737,12.0563691079987));
#78196=CARTESIAN_POINT('Ctrl Pts',(3.29717324240272,138.121895329679,12.1232767923625));
#78197=CARTESIAN_POINT('Ctrl Pts',(3.28922399737098,138.016320789655,12.2161545562617));
#78198=CARTESIAN_POINT('Ctrl Pts',(3.28795864243356,137.99965654557,12.2315156581374));
#78199=CARTESIAN_POINT('Ctrl Pts',(3.28593086056927,137.97319355856,12.2570712706267));
#78200=CARTESIAN_POINT('Ctrl Pts',(3.28515860727105,137.96317442958,12.267031191698));
#78201=CARTESIAN_POINT('Ctrl Pts',(3.28367135472077,137.944001781126,12.2866505870111));
#78202=CARTESIAN_POINT('Ctrl Pts',(3.28295570885517,137.934832735968,12.2962928779888));
#78203=CARTESIAN_POINT('Ctrl Pts',(3.2812694640749,137.913374323431,12.3194841031224));
#78204=CARTESIAN_POINT('Ctrl Pts',(3.28030396148403,137.901204826964,12.3331411725082));
#78205=CARTESIAN_POINT('Ctrl Pts',(3.27684504717546,137.858092776139,12.3833887823832));
#78206=CARTESIAN_POINT('Ctrl Pts',(3.27441303928814,137.828694673803,12.4212664700008));
#78207=CARTESIAN_POINT('Ctrl Pts',(3.26770454816095,137.751409950639,12.5316306916283));
#78208=CARTESIAN_POINT('Ctrl Pts',(3.26355480582356,137.708040678928,12.6070284516602));
#78209=CARTESIAN_POINT('Ctrl Pts',(3.25648070783177,137.64750350872,12.7379635532396));
#78210=CARTESIAN_POINT('Ctrl Pts',(3.25361929884706,137.626490253744,12.7914712264083));
#78211=CARTESIAN_POINT('Ctrl Pts',(3.2499158729755,137.604604409594,12.8585525973906));
#78212=CARTESIAN_POINT('Ctrl Pts',(3.24921884122643,137.600700039935,12.8710894488228));
#78213=CARTESIAN_POINT('Ctrl Pts',(3.24808413696821,137.594699195873,12.8913126600479));
#78214=CARTESIAN_POINT('Ctrl Pts',(3.24765231510458,137.592495801843,12.8989668118558));
#78215=CARTESIAN_POINT('Ctrl Pts',(3.24678981132717,137.588256064853,12.9141602714618));
#78216=CARTESIAN_POINT('Ctrl Pts',(3.24635926947857,137.586217383655,12.9216986110282));
#78217=CARTESIAN_POINT('Ctrl Pts',(3.24523697857455,137.581099390025,12.9412425278066));
#78218=CARTESIAN_POINT('Ctrl Pts',(3.24454034137454,137.578112133274,12.9532713765573));
#78219=CARTESIAN_POINT('Ctrl Pts',(3.24117591250513,137.564560552932,13.0109628221969));
#78220=CARTESIAN_POINT('Ctrl Pts',(3.23841806440327,137.556041782866,13.0570743846208));
#78221=CARTESIAN_POINT('Ctrl Pts',(3.23172620786661,137.540985892648,13.1681991539778));
#78222=CARTESIAN_POINT('Ctrl Pts',(3.22776565882116,137.536559451577,13.2334009106179));
#78223=CARTESIAN_POINT('Ctrl Pts',(3.22385963331144,137.53650059484,13.2986804940338));
#78224=CARTESIAN_POINT('Ctrl Pts',(3.22393332744186,137.536628644961,13.2986850195007));
#78225=CARTESIAN_POINT('Ctrl Pts',(3.22390770808568,137.536629296413,13.2991232392521));
#78226=CARTESIAN_POINT('Ctrl Pts',(3.22388209050693,137.536630143947,13.2995614623613));
#78227=CARTESIAN_POINT('Ctrl Pts',(3.22385647472349,137.536631187551,13.2999996886484));
#78228=CARTESIAN_POINT('',(3.65155456155019,137.536499869567,13.3004052814541));
#78229=CARTESIAN_POINT('Ctrl Pts',(3.1529262221125,137.5365,13.3000000000405));
#78230=CARTESIAN_POINT('Ctrl Pts',(3.15294755840493,137.5365,13.2995616236816));
#78231=CARTESIAN_POINT('Ctrl Pts',(3.15296889379876,137.536500196966,13.2991232433111));
#78232=CARTESIAN_POINT('Ctrl Pts',(3.15751033426512,137.536584055109,13.2058052336659));
#78233=CARTESIAN_POINT('Ctrl Pts',(3.16195982162168,137.545509033665,13.1131535443846));
#78234=CARTESIAN_POINT('Ctrl Pts',(3.16771026279101,137.56663405572,13.0039751141562));
#78235=CARTESIAN_POINT('Ctrl Pts',(3.16867234969529,137.570456420978,12.9860354171264));
#78236=CARTESIAN_POINT('Ctrl Pts',(3.17013174161221,137.576652671786,12.9594189949979));
#78237=CARTESIAN_POINT('Ctrl Pts',(3.1706158604517,137.578771162034,12.9506840693296));
#78238=CARTESIAN_POINT('Ctrl Pts',(3.17150088843002,137.582753232004,12.9349014023963));
#78239=CARTESIAN_POINT('Ctrl Pts',(3.17190027439989,137.584589207954,12.9278472484509));
#78240=CARTESIAN_POINT('Ctrl Pts',(3.1728420867,137.589009672106,12.9113690287514));
#78241=CARTESIAN_POINT('Ctrl Pts',(3.17338677568636,137.591635926829,12.9019568317226));
#78242=CARTESIAN_POINT('Ctrl Pts',(3.17522105621282,137.600718501482,12.8706215717162));
#78243=CARTESIAN_POINT('Ctrl Pts',(3.17653130032495,137.607593797145,12.8488244244251));
#78244=CARTESIAN_POINT('Ctrl Pts',(3.17989083960996,137.626263723224,12.794132787799));
#78245=CARTESIAN_POINT('Ctrl Pts',(3.18196326855966,137.638731205648,12.7614834938888));
#78246=CARTESIAN_POINT('Ctrl Pts',(3.18854188070924,137.681603102232,12.6602438283886));
#78247=CARTESIAN_POINT('Ctrl Pts',(3.19309763093147,137.71611998596,12.5935220360881));
#78248=CARTESIAN_POINT('Ctrl Pts',(3.20125385796455,137.788412655287,12.4767289300527));
#78249=CARTESIAN_POINT('Ctrl Pts',(3.20487897271493,137.824582211789,12.4258640488924));
#78250=CARTESIAN_POINT('Ctrl Pts',(3.20951444539336,137.87656148433,12.3618517018039));
#78251=CARTESIAN_POINT('Ctrl Pts',(3.21063194066752,137.889553518242,12.3465090479064));
#78252=CARTESIAN_POINT('Ctrl Pts',(3.21240752262372,137.910937850465,12.3222858613872));
#78253=CARTESIAN_POINT('Ctrl Pts',(3.21307362791868,137.919132088415,12.3132346414778));
#78254=CARTESIAN_POINT('Ctrl Pts',(3.21445632491872,137.936498631168,12.2945277686582));
#78255=CARTESIAN_POINT('Ctrl Pts',(3.21517195098565,137.94569142272,12.2848926118549));
#78256=CARTESIAN_POINT('Ctrl Pts',(3.21688159878464,137.968138656341,12.2619991267902));
#78257=CARTESIAN_POINT('Ctrl Pts',(3.21787000150962,137.981518981748,12.248867228555));
#78258=CARTESIAN_POINT('Ctrl Pts',(3.22158792416261,138.033328705337,12.1999378372203));
#78259=CARTESIAN_POINT('Ctrl Pts',(3.22424204467757,138.073424029924,12.1659595159793));
#78260=CARTESIAN_POINT('Ctrl Pts',(3.23221073876424,138.201485255124,12.0687718558));
#78261=CARTESIAN_POINT('Ctrl Pts',(3.23731520016404,138.294694732578,12.0131082029346));
#78262=CARTESIAN_POINT('Ctrl Pts',(3.2444334374589,138.423674767298,11.9543387272715));
#78263=CARTESIAN_POINT('Ctrl Pts',(3.24614808605334,138.454632837018,11.9414973703536));
#78264=CARTESIAN_POINT('Ctrl Pts',(3.24852371530324,138.496767966907,11.9256921801478));
#78265=CARTESIAN_POINT('Ctrl Pts',(3.24913699095929,138.507580743555,11.9217809600122));
#78266=CARTESIAN_POINT('Ctrl Pts',(3.25016344770839,138.525542382742,11.9155221858991));
#78267=CARTESIAN_POINT('Ctrl Pts',(3.25057250969724,138.532665520309,11.9131015427845));
#78268=CARTESIAN_POINT('Ctrl Pts',(3.25142967204679,138.547509735395,11.9081844040243));
#78269=CARTESIAN_POINT('Ctrl Pts',(3.25187823324844,138.555233390326,11.9056970382251));
#78270=CARTESIAN_POINT('Ctrl Pts',(3.25310913027287,138.576321240534,11.8990988412559));
#78271=CARTESIAN_POINT('Ctrl Pts',(3.25389818135018,138.589724001539,11.895115192073));
#78272=CARTESIAN_POINT('Ctrl Pts',(3.25881460932111,138.672681873001,11.8717462657293));
#78273=CARTESIAN_POINT('Ctrl Pts',(3.26314868270188,138.743530769368,11.857340036066));
#78274=CARTESIAN_POINT('Ctrl Pts',(3.27398278108366,138.921962374414,11.8346205421573));
#78275=CARTESIAN_POINT('Ctrl Pts',(3.28044530560699,139.029969325974,11.8328479289741));
#78276=CARTESIAN_POINT('Ctrl Pts',(3.28786047488858,139.160385303115,11.845128538219));
#78277=CARTESIAN_POINT('Ctrl Pts',(3.28916206025021,139.183512669676,11.8478644679518));
#78278=CARTESIAN_POINT('Ctrl Pts',(3.2912294450728,139.22061727807,11.8531545619147));
#78279=CARTESIAN_POINT('Ctrl Pts',(3.29200590715503,139.234639116481,11.8553622564576));
#78280=CARTESIAN_POINT('Ctrl Pts',(3.29348968891621,139.261591534641,11.8600086132795));
#78281=CARTESIAN_POINT('Ctrl Pts',(3.29419784328166,139.274525642452,11.8624183459632));
#78282=CARTESIAN_POINT('Ctrl Pts',(3.29584839371893,139.304825110353,11.868487239466));
#78283=CARTESIAN_POINT('Ctrl Pts',(3.29678619325137,139.322160066447,11.8722885237703));
#78284=CARTESIAN_POINT('Ctrl Pts',(3.3000236405971,139.382352909126,11.8866400574855));
#78285=CARTESIAN_POINT('Ctrl Pts',(3.30227214938022,139.424800710582,11.8988130468265));
#78286=CARTESIAN_POINT('Ctrl Pts',(3.30817797019884,139.536752369269,11.9364744913971));
#78287=CARTESIAN_POINT('Ctrl Pts',(3.31174719840716,139.60498112864,11.965345289833));
#78288=CARTESIAN_POINT('Ctrl Pts',(3.31873543755969,139.732592082261,12.0311482059054));
#78289=CARTESIAN_POINT('Ctrl Pts',(3.32214415839357,139.792090269984,12.0674143853622));
#78290=CARTESIAN_POINT('Ctrl Pts',(3.32660042568913,139.861929989689,12.1171349916392));
#78291=CARTESIAN_POINT('Ctrl Pts',(3.32745072213696,139.874926613928,12.1267155871335));
#78292=CARTESIAN_POINT('Ctrl Pts',(3.32877785151568,139.894644718368,12.1417608022986));
#78293=CARTESIAN_POINT('Ctrl Pts',(3.32924499701,139.901480974738,12.1470736121598));
#78294=CARTESIAN_POINT('Ctrl Pts',(3.33011984666183,139.914079307095,12.1570449838738));
#78295=CARTESIAN_POINT('Ctrl Pts',(3.33052645503831,139.919853739121,12.1616871086149));
#78296=CARTESIAN_POINT('Ctrl Pts',(3.33150656011536,139.933584173416,12.1728978383743));
#78297=CARTESIAN_POINT('Ctrl Pts',(3.3320828185508,139.941506309057,12.1795070062589));
#78298=CARTESIAN_POINT('Ctrl Pts',(3.33415677366883,139.969514341964,12.2033798929647));
#78299=CARTESIAN_POINT('Ctrl Pts',(3.33568270399178,139.989199755064,12.2211036216512));
#78300=CARTESIAN_POINT('Ctrl Pts',(3.33978701302044,140.040078104931,12.2694752410841));
#78301=CARTESIAN_POINT('Ctrl Pts',(3.34240146224568,140.070396729978,12.3010033881348));
#78302=CARTESIAN_POINT('Ctrl Pts',(3.35202624990321,140.176056050839,12.4212181711514));
#78303=CARTESIAN_POINT('Ctrl Pts',(3.35904978909633,140.242175864504,12.5174576917622));
#78304=CARTESIAN_POINT('Ctrl Pts',(3.36698869559953,140.307228898286,12.6415557244939));
#78305=CARTESIAN_POINT('Ctrl Pts',(3.36831720314937,140.31774186761,12.6628558093501));
#78306=CARTESIAN_POINT('Ctrl Pts',(3.3704163674997,140.333741851227,12.697364915776));
#78307=CARTESIAN_POINT('Ctrl Pts',(3.37119828437813,140.339561486373,12.7104142004422));
#78308=CARTESIAN_POINT('Ctrl Pts',(3.37268596212271,140.350358499503,12.7356097059127));
#78309=CARTESIAN_POINT('Ctrl Pts',(3.37339266964003,140.355365365852,12.7477417073982));
#78310=CARTESIAN_POINT('Ctrl Pts',(3.37503016978599,140.366673694673,12.7762231282036));
#78311=CARTESIAN_POINT('Ctrl Pts',(3.37595659084267,140.372846157504,12.7926217762155));
#78312=CARTESIAN_POINT('Ctrl Pts',(3.37909766204547,140.392970177589,12.8491445248979));
#78313=CARTESIAN_POINT('Ctrl Pts',(3.38126540331281,140.405469221385,12.8897643997763));
#78314=CARTESIAN_POINT('Ctrl Pts',(3.38685258971738,140.433598868699,12.9976859685849));
#78315=CARTESIAN_POINT('Ctrl Pts',(3.3901968497738,140.44626410632,13.0656495535306));
#78316=CARTESIAN_POINT('Ctrl Pts',(3.3973092414232,140.462834893467,13.2110246708388));
#78317=CARTESIAN_POINT('Ctrl Pts',(3.40107005123646,140.465491309069,13.2883605521666));
#78318=CARTESIAN_POINT('Ctrl Pts',(3.40591345538974,140.461322203631,13.3813685678251));
#78319=CARTESIAN_POINT('Ctrl Pts',(3.40674865438157,140.460355393055,13.3971880281685));
#78320=CARTESIAN_POINT('Ctrl Pts',(3.40805704392904,140.458468331259,13.4215576200612));
#78321=CARTESIAN_POINT('Ctrl Pts',(3.40852096604346,140.457729278714,13.430120985265));
#78322=CARTESIAN_POINT('Ctrl Pts',(3.40939343889964,140.456211406476,13.4460674551689));
#78323=CARTESIAN_POINT('Ctrl Pts',(3.40980096622735,140.455451776379,13.4534518807826));
#78324=CARTESIAN_POINT('Ctrl Pts',(3.4107883893904,140.453489871171,13.4711964359356));
#78325=CARTESIAN_POINT('Ctrl Pts',(3.41137116125793,140.452232979571,13.4815499527864));
#78326=CARTESIAN_POINT('Ctrl Pts',(3.41349816954794,140.44728650236,13.5189501144346));
#78327=CARTESIAN_POINT('Ctrl Pts',(3.41507248036451,140.442951222455,13.5459043723841));
#78328=CARTESIAN_POINT('Ctrl Pts',(3.41935454315111,140.429318300634,13.6177814266914));
#78329=CARTESIAN_POINT('Ctrl Pts',(3.42210180326305,140.418658280452,13.662414327594));
#78330=CARTESIAN_POINT('Ctrl Pts',(3.43185250710553,140.373656736234,13.8180678584859));
#78331=CARTESIAN_POINT('Ctrl Pts',(3.43884921043368,140.328214020917,13.9254461577063));
#78332=CARTESIAN_POINT('Ctrl Pts',(3.44666339893655,140.259544985473,14.0455667357442));
#78333=CARTESIAN_POINT('Ctrl Pts',(3.44789987761416,140.248111009153,14.0645536687447));
#78334=CARTESIAN_POINT('Ctrl Pts',(3.44989032871341,140.228774399358,14.0950728334207));
#78335=CARTESIAN_POINT('Ctrl Pts',(3.45065356862008,140.221130330747,14.1067639489332));
#78336=CARTESIAN_POINT('Ctrl Pts',(3.45212895722999,140.205908614946,14.1293324619642));
#78337=CARTESIAN_POINT('Ctrl Pts',(3.452841654362,140.198348264316,14.1402198363276));
#78338=CARTESIAN_POINT('Ctrl Pts',(3.45452930732891,140.179955506056,14.165953192439));
#78339=CARTESIAN_POINT('Ctrl Pts',(3.45549902623404,140.168989213932,14.180700962625));
#78340=CARTESIAN_POINT('Ctrl Pts',(3.45902820676924,140.127651733932,14.2341597458875));
#78341=CARTESIAN_POINT('Ctrl Pts',(3.46152244505263,140.095610810504,14.2715402235041));
#78342=CARTESIAN_POINT('Ctrl Pts',(3.46854943384063,139.998355457973,14.3740586089793));
#78343=CARTESIAN_POINT('Ctrl Pts',(3.47293690423006,139.928801403468,14.4347436011896));
#78344=CARTESIAN_POINT('Ctrl Pts',(3.47999270329075,139.812495117348,14.5183172232605));
#78345=CARTESIAN_POINT('Ctrl Pts',(3.48255588311855,139.769452979622,14.5459479914702));
#78346=CARTESIAN_POINT('Ctrl Pts',(3.48591455762878,139.713920052445,14.5776207636146));
#78347=CARTESIAN_POINT('Ctrl Pts',(3.48659574462048,139.702699495468,14.5838263331335));
#78348=CARTESIAN_POINT('Ctrl Pts',(3.48770917764604,139.684464793677,14.5936004401251));
#78349=CARTESIAN_POINT('Ctrl Pts',(3.48813590575812,139.677500651613,14.5972613513293));
#78350=CARTESIAN_POINT('Ctrl Pts',(3.48899273800856,139.663576309529,14.6044383986713));
#78351=CARTESIAN_POINT('Ctrl Pts',(3.48942277230695,139.656616865855,14.6079554042241));
#78352=CARTESIAN_POINT('Ctrl Pts',(3.49055016368183,139.638435968646,14.6169615841983));
#78353=CARTESIAN_POINT('Ctrl Pts',(3.49125253775838,139.627171939625,14.62236289914));
#78354=CARTESIAN_POINT('Ctrl Pts',(3.49475168624053,139.571280992994,14.6482889416698));
#78355=CARTESIAN_POINT('Ctrl Pts',(3.49764744150161,139.525712507597,14.6667006298247));
#78356=CARTESIAN_POINT('Ctrl Pts',(3.50412935346481,139.423223342205,14.7022260142005));
#78357=CARTESIAN_POINT('Ctrl Pts',(3.50772643042839,139.366007044435,14.7182364696718));
#78358=CARTESIAN_POINT('Ctrl Pts',(3.51602394684218,139.230628240194,14.747377914374));
#78359=CARTESIAN_POINT('Ctrl Pts',(3.52067440013414,139.152049223164,14.7577297911334));
#78360=CARTESIAN_POINT('Ctrl Pts',(3.52630171018029,139.052234413982,14.7627154535567));
#78361=CARTESIAN_POINT('Ctrl Pts',(3.52745959228154,139.031438842244,14.7633101496295));
#78362=CARTESIAN_POINT('Ctrl Pts',(3.52935718492527,138.996939522364,14.7635609009486));
#78363=CARTESIAN_POINT('Ctrl Pts',(3.53010457018412,138.983241139322,14.7634681533269));
#78364=CARTESIAN_POINT('Ctrl Pts',(3.53157259041123,138.956124311386,14.7629037516989));
#78365=CARTESIAN_POINT('Ctrl Pts',(3.53229339027029,138.942707070637,14.7624397421706));
#78366=CARTESIAN_POINT('Ctrl Pts',(3.53403977574091,138.909963086359,14.76085601952));
#78367=CARTESIAN_POINT('Ctrl Pts',(3.53505909665065,138.89064827656,14.7595373248535));
#78368=CARTESIAN_POINT('Ctrl Pts',(3.53912955012471,138.81280590453,14.7526687337649));
#78369=CARTESIAN_POINT('Ctrl Pts',(3.54208391120584,138.754608863449,14.7439779009135));
#78370=CARTESIAN_POINT('Ctrl Pts',(3.54790020566391,138.639192295387,14.7195604892136));
#78371=CARTESIAN_POINT('Ctrl Pts',(3.55075626980304,138.582092090765,14.703811692831));
#78372=CARTESIAN_POINT('Ctrl Pts',(3.55684165504907,138.463924695934,14.6633687868989));
#78373=CARTESIAN_POINT('Ctrl Pts',(3.56007080357649,138.403256085178,14.6379261480481));
#78374=CARTESIAN_POINT('Ctrl Pts',(3.56432930608584,138.32998821099,14.6012225752537));
#78375=CARTESIAN_POINT('Ctrl Pts',(3.56518438860922,138.315590892404,14.5937078954065));
#78376=CARTESIAN_POINT('Ctrl Pts',(3.56651745580689,138.293697128591,14.5818127040727));
#78377=CARTESIAN_POINT('Ctrl Pts',(3.56698561851442,138.286109253497,14.5776022655315));
#78378=CARTESIAN_POINT('Ctrl Pts',(3.56786123990405,138.272116536529,14.5696742694914));
#78379=CARTESIAN_POINT('Ctrl Pts',(3.56826758017445,138.265701804731,14.5659752126448));
#78380=CARTESIAN_POINT('Ctrl Pts',(3.56924547442094,138.250446800748,14.5570234642089));
#78381=CARTESIAN_POINT('Ctrl Pts',(3.56981975541381,138.241633439664,14.5517260625964));
#78382=CARTESIAN_POINT('Ctrl Pts',(3.57187786619908,138.210527683784,14.5325803935952));
#78383=CARTESIAN_POINT('Ctrl Pts',(3.57338939136101,138.188553802301,14.5182265262404));
#78384=CARTESIAN_POINT('Ctrl Pts',(3.57744159269108,138.131545850945,14.4787607341075));
#78385=CARTESIAN_POINT('Ctrl Pts',(3.58001735579869,138.097215016411,14.4526787954019));
#78386=CARTESIAN_POINT('Ctrl Pts',(3.58944410734881,137.976674460903,14.3524091847949));
#78387=CARTESIAN_POINT('Ctrl Pts',(3.59631549599301,137.898019289369,14.2697453113168));
#78388=CARTESIAN_POINT('Ctrl Pts',(3.60422893629836,137.814465641131,14.1584790690359));
#78389=CARTESIAN_POINT('Ctrl Pts',(3.60565486151238,137.799737438369,14.1377636447471));
#78390=CARTESIAN_POINT('Ctrl Pts',(3.60787672680222,137.77731981009,14.1044272606911));
#78391=CARTESIAN_POINT('Ctrl Pts',(3.60868602987274,137.76926965336,14.0920561222972));
#78392=CARTESIAN_POINT('Ctrl Pts',(3.61019600340686,137.754474604263,14.0685493813113));
#78393=CARTESIAN_POINT('Ctrl Pts',(3.61089814679496,137.747688532325,14.0574415264562));
#78394=CARTESIAN_POINT('Ctrl Pts',(3.61248418145654,137.732581638437,14.0319555007784));
#78395=CARTESIAN_POINT('Ctrl Pts',(3.61336459819105,137.724355546632,14.0175231125313));
#78396=CARTESIAN_POINT('Ctrl Pts',(3.61614751055924,137.698895057913,13.9710311595773));
#78397=CARTESIAN_POINT('Ctrl Pts',(3.61801706801827,137.682609534172,13.9384665353132));
#78398=CARTESIAN_POINT('Ctrl Pts',(3.62255867782303,137.645405641842,13.8565732978988));
#78399=CARTESIAN_POINT('Ctrl Pts',(3.62518925385113,137.625948730523,13.8066391913907));
#78400=CARTESIAN_POINT('Ctrl Pts',(3.63071422561598,137.590639235391,13.6988915293272));
#78401=CARTESIAN_POINT('Ctrl Pts',(3.63359797507643,137.575511475382,13.6409462229351));
#78402=CARTESIAN_POINT('Ctrl Pts',(3.63890633058407,137.554795195006,13.5355422872998));
#78403=CARTESIAN_POINT('Ctrl Pts',(3.64130180439216,137.547901220175,13.4884290088702));
#78404=CARTESIAN_POINT('Ctrl Pts',(3.64446671289217,137.542098559195,13.4285099980814));
#78405=CARTESIAN_POINT('Ctrl Pts',(3.64513737310426,137.541044909464,13.4159372811191));
#78406=CARTESIAN_POINT('Ctrl Pts',(3.64623782630549,137.539601435773,13.3955484146922));
#78407=CARTESIAN_POINT('Ctrl Pts',(3.64666233494489,137.539111505068,13.3877397611939));
#78408=CARTESIAN_POINT('Ctrl Pts',(3.64746287321699,137.538312433838,13.3731303719459));
#78409=CARTESIAN_POINT('Ctrl Pts',(3.64783802623788,137.537988086607,13.3663306384269));
#78410=CARTESIAN_POINT('Ctrl Pts',(3.64870338654884,137.537353593872,13.3507447710495));
#78411=CARTESIAN_POINT('Ctrl Pts',(3.6491952381005,137.537075160363,13.341957681216));
#78412=CARTESIAN_POINT('Ctrl Pts',(3.65030652276399,137.53662836591,13.3222489504325));
#78413=CARTESIAN_POINT('Ctrl Pts',(3.65092794022738,137.53650307742,13.3113269345325));
#78414=CARTESIAN_POINT('Ctrl Pts',(3.65155426291434,137.536500055998,13.3004048542518));
#78415=CARTESIAN_POINT('Ctrl Pts',(3.65155423947869,137.536500056111,13.3004052629325));
#78416=CARTESIAN_POINT('Ctrl Pts',(3.65156198605023,137.536500018704,13.3002701749106));
#78417=CARTESIAN_POINT('Ctrl Pts',(3.65156973335021,137.5365,13.3001350872663));
#78418=CARTESIAN_POINT('Ctrl Pts',(3.65157748137715,137.5365,13.3000000000035));
#78419=CARTESIAN_POINT('Origin',(4.2,139.,13.3));
#78420=CARTESIAN_POINT('',(4.22337996970852,137.5365,13.299999999996));
#78421=CARTESIAN_POINT('',(4.15384019369498,137.5365,13.3000000000084));
#78422=CARTESIAN_POINT('',(4.2,137.5365,13.3));
#78423=CARTESIAN_POINT('',(4.22332920524334,137.536500478426,13.3010219306143));
#78424=CARTESIAN_POINT('Ctrl Pts',(4.22337996970853,137.5365,13.299999999996));
#78425=CARTESIAN_POINT('Ctrl Pts',(4.22336296862726,137.5365,13.3003407816243));
#78426=CARTESIAN_POINT('Ctrl Pts',(4.22334596990515,137.536500119028,13.3006815642919));
#78427=CARTESIAN_POINT('Ctrl Pts',(4.22332897353037,137.536500357088,13.3010223479367));
#78428=CARTESIAN_POINT('Ctrl Pts',(4.22332899486318,137.536500356789,13.301021920206));
#78429=CARTESIAN_POINT('Ctrl Pts',(4.21832396167272,137.536570430274,13.4013746880209));
#78430=CARTESIAN_POINT('Ctrl Pts',(4.21356247497565,137.546961721373,13.501450363291));
#78431=CARTESIAN_POINT('Ctrl Pts',(4.20625949287419,137.577206410225,13.6460245454743));
#78432=CARTESIAN_POINT('Ctrl Pts',(4.2038741173552,137.589145841286,13.6918729294185));
#78433=CARTESIAN_POINT('Ctrl Pts',(4.2007293433516,137.60699605147,13.7489172127474));
#78434=CARTESIAN_POINT('Ctrl Pts',(4.20006838602579,137.610857816477,13.7607283776677));
#78435=CARTESIAN_POINT('Ctrl Pts',(4.19897812123783,137.617392718495,13.7798858643397));
#78436=CARTESIAN_POINT('Ctrl Pts',(4.19855385804683,137.619975227322,13.7872627217991));
#78437=CARTESIAN_POINT('Ctrl Pts',(4.19769045099725,137.625305975751,13.8021074667226));
#78438=CARTESIAN_POINT('Ctrl Pts',(4.19725121228529,137.628056266367,13.8095742870747));
#78439=CARTESIAN_POINT('Ctrl Pts',(4.19608030268081,137.635493099844,13.829268011228));
#78440=CARTESIAN_POINT('Ctrl Pts',(4.19534297447281,137.640282990253,13.8414548339741));
#78441=CARTESIAN_POINT('Ctrl Pts',(4.19138793972816,137.666576951624,13.9058040261453));
#78442=CARTESIAN_POINT('Ctrl Pts',(4.18804105151076,137.69091907293,13.9567507941404));
#78443=CARTESIAN_POINT('Ctrl Pts',(4.17940095242827,137.76041668487,14.0829066702024));
#78444=CARTESIAN_POINT('Ctrl Pts',(4.17408198891199,137.809505506131,14.1557070053943));
#78445=CARTESIAN_POINT('Ctrl Pts',(4.16612309618769,137.895189353068,14.2610108926096));
#78446=CARTESIAN_POINT('Ctrl Pts',(4.16335798259313,137.927389710947,14.2968231491989));
#78447=CARTESIAN_POINT('Ctrl Pts',(4.1596396389996,137.974202017753,14.3439857365848));
#78448=CARTESIAN_POINT('Ctrl Pts',(4.15862527155178,137.987348162386,14.3567421716348));
#78449=CARTESIAN_POINT('Ctrl Pts',(4.15689225499151,138.010454426051,14.3783361887832));
#78450=CARTESIAN_POINT('Ctrl Pts',(4.15616865455337,138.020301830803,14.387290620119));
#78451=CARTESIAN_POINT('Ctrl Pts',(4.15468909695458,138.040843800061,14.4054641286139));
#78452=CARTESIAN_POINT('Ctrl Pts',(4.15393392318336,138.051552393547,14.4146652916057));
#78453=CARTESIAN_POINT('Ctrl Pts',(4.15198504780083,138.079758321728,14.4381999019641));
#78454=CARTESIAN_POINT('Ctrl Pts',(4.15080132032213,138.097458037034,14.4522854856909));
#78455=CARTESIAN_POINT('Ctrl Pts',(4.14377563488128,138.205732327792,14.5344249849649));
#78456=CARTESIAN_POINT('Ctrl Pts',(4.13834519302298,138.303629111033,14.5921824183654));
#78457=CARTESIAN_POINT('Ctrl Pts',(4.1305203277536,138.45036357004,14.6571880495186));
#78458=CARTESIAN_POINT('Ctrl Pts',(4.1282020268816,138.494410984787,14.6742048249214));
#78459=CARTESIAN_POINT('Ctrl Pts',(4.12439821662107,138.565602302351,14.6978213880667));
#78460=CARTESIAN_POINT('Ctrl Pts',(4.12296217820215,138.592246537744,14.7058246416548));
#78461=CARTESIAN_POINT('Ctrl Pts',(4.12092944040672,138.629275923906,14.7158061173772));
#78462=CARTESIAN_POINT('Ctrl Pts',(4.12036546485904,138.639479927177,14.7184387779075));
#78463=CARTESIAN_POINT('Ctrl Pts',(4.11939088860207,138.656970193759,14.72275039893));
#78464=CARTESIAN_POINT('Ctrl Pts',(4.1189833285372,138.664242387833,14.7244841066348));
#78465=CARTESIAN_POINT('Ctrl Pts',(4.11809792430773,138.679943585532,14.7281003894961));
#78466=CARTESIAN_POINT('Ctrl Pts',(4.1176191396927,138.688376058465,14.7299641052484));
#78467=CARTESIAN_POINT('Ctrl Pts',(4.11624842282245,138.712371431767,14.7350451587972));
#78468=CARTESIAN_POINT('Ctrl Pts',(4.11534747507424,138.727970516207,14.7380836969089));
#78469=CARTESIAN_POINT('Ctrl Pts',(4.11000067197004,138.819758727907,14.7544162823216));
#78470=CARTESIAN_POINT('Ctrl Pts',(4.10533361085638,138.896851199879,14.7619070972357));
#78471=CARTESIAN_POINT('Ctrl Pts',(4.0965249698177,139.043044489215,14.7644879103771));
#78472=CARTESIAN_POINT('Ctrl Pts',(4.09239212990641,139.111925392132,14.7608393751406));
#78473=CARTESIAN_POINT('Ctrl Pts',(4.08590382078877,139.22243486444,14.7471205691818));
#78474=CARTESIAN_POINT('Ctrl Pts',(4.08347646765041,139.264327656169,14.7400578479565));
#78475=CARTESIAN_POINT('Ctrl Pts',(4.08012324827709,139.323050790133,14.727508165028));
#78476=CARTESIAN_POINT('Ctrl Pts',(4.0791511836517,139.340177354777,14.7235240705886));
#78477=CARTESIAN_POINT('Ctrl Pts',(4.07746656338379,139.370029072654,14.7160102297428));
#78478=CARTESIAN_POINT('Ctrl Pts',(4.07674979555009,139.382785732073,14.7126151579989));
#78479=CARTESIAN_POINT('Ctrl Pts',(4.07526250813431,139.40936197078,14.7051556741769));
#78480=CARTESIAN_POINT('Ctrl Pts',(4.07449312496803,139.423171032005,14.7010588815359));
#78481=CARTESIAN_POINT('Ctrl Pts',(4.07245696156446,139.459856487304,14.6895833675664));
#78482=CARTESIAN_POINT('Ctrl Pts',(4.07120197561785,139.482615791233,14.6818436988438));
#78483=CARTESIAN_POINT('Ctrl Pts',(4.06375892309784,139.618147055573,14.6319968227625));
#78484=CARTESIAN_POINT('Ctrl Pts',(4.05803570713088,139.725556964742,14.5766711369999));
#78485=CARTESIAN_POINT('Ctrl Pts',(4.0494252812342,139.870779407724,14.4775608976839));
#78486=CARTESIAN_POINT('Ctrl Pts',(4.04667198732655,139.91475926861,14.443731140496));
#78487=CARTESIAN_POINT('Ctrl Pts',(4.04297409797902,139.968474658797,14.3973289233344));
#78488=CARTESIAN_POINT('Ctrl Pts',(4.04215378873461,139.980075894789,14.3869798219101));
#78489=CARTESIAN_POINT('Ctrl Pts',(4.04086684303432,139.997740827494,14.3707087659492));
#78490=CARTESIAN_POINT('Ctrl Pts',(4.04040914065602,140.003921935408,14.3649153772748));
#78491=CARTESIAN_POINT('Ctrl Pts',(4.03953710197643,140.015497933818,14.3538751472433));
#78492=CARTESIAN_POINT('Ctrl Pts',(4.03912358710051,140.020903183948,14.3486398615032));
#78493=CARTESIAN_POINT('Ctrl Pts',(4.03810502958813,140.03401866212,14.3357392816082));
#78494=CARTESIAN_POINT('Ctrl Pts',(4.03749669052269,140.041684220147,14.3280293886896));
#78495=CARTESIAN_POINT('Ctrl Pts',(4.03528762660687,140.068953893885,14.2999838342035));
#78496=CARTESIAN_POINT('Ctrl Pts',(4.03365521910621,140.088053277994,14.2791679953743));
#78497=CARTESIAN_POINT('Ctrl Pts',(4.02533018537058,140.180955193076,14.1718408670755));
#78498=CARTESIAN_POINT('Ctrl Pts',(4.0183368030541,140.245101376927,14.0774874229262));
#78499=CARTESIAN_POINT('Ctrl Pts',(4.00848636368444,140.322393842191,13.9292567472796));
#78500=CARTESIAN_POINT('Ctrl Pts',(4.00540179150499,140.344494810375,13.88053785794));
#78501=CARTESIAN_POINT('Ctrl Pts',(4.0013455241145,140.370740453831,13.8130892129656));
#78502=CARTESIAN_POINT('Ctrl Pts',(4.00029674931193,140.377256677992,13.7953322343927));
#78503=CARTESIAN_POINT('Ctrl Pts',(3.99852387552302,140.387801391026,13.7647787938723));
#78504=CARTESIAN_POINT('Ctrl Pts',(3.99779420961181,140.39200138224,13.752044463254));
#78505=CARTESIAN_POINT('Ctrl Pts',(3.99640730556487,140.399711145863,13.7275414835868));
#78506=CARTESIAN_POINT('Ctrl Pts',(3.99574920202892,140.403248941935,13.7157829139579));
#78507=CARTESIAN_POINT('Ctrl Pts',(3.99402140463634,140.412211674865,13.6845751947648));
#78508=CARTESIAN_POINT('Ctrl Pts',(3.99295993035147,140.417382925553,13.6650555982226));
#78509=CARTESIAN_POINT('Ctrl Pts',(3.98864700581961,140.43696556345,13.5844341850033));
#78510=CARTESIAN_POINT('Ctrl Pts',(3.98550628881357,140.447843135909,13.522540179273));
#78511=CARTESIAN_POINT('Ctrl Pts',(3.97875172484933,140.462886796984,13.3858789997987));
#78512=CARTESIAN_POINT('Ctrl Pts',(3.97517243221057,140.465363170715,13.3111083327715));
#78513=CARTESIAN_POINT('Ctrl Pts',(3.96896817222459,140.45989805607,13.1853170078063));
#78514=CARTESIAN_POINT('Ctrl Pts',(3.96639948695296,140.454991930039,13.1343132177153));
#78515=CARTESIAN_POINT('Ctrl Pts',(3.96304235686779,140.445552480088,13.0711537807292));
#78516=CARTESIAN_POINT('Ctrl Pts',(3.96236934615564,140.443518577131,13.0586565503957));
#78517=CARTESIAN_POINT('Ctrl Pts',(3.96126426766466,140.43995880168,13.0384416675561));
#78518=CARTESIAN_POINT('Ctrl Pts',(3.96083751023105,140.438532357344,13.0307069195181));
#78519=CARTESIAN_POINT('Ctrl Pts',(3.96002705522299,140.435728836242,13.0161634079045));
#78520=CARTESIAN_POINT('Ctrl Pts',(3.9596441642781,140.43436548649,13.009352190306));
#78521=CARTESIAN_POINT('Ctrl Pts',(3.95859865643289,140.430536431775,12.9909058019425));
#78522=CARTESIAN_POINT('Ctrl Pts',(3.95793108622625,140.427977344407,12.9792907998497));
#78523=CARTESIAN_POINT('Ctrl Pts',(3.95515483415933,140.416855888449,12.931588212518));
#78524=CARTESIAN_POINT('Ctrl Pts',(3.9529906206915,140.407065234994,12.8958034128813));
#78525=CARTESIAN_POINT('Ctrl Pts',(3.94459923446142,140.364516640614,12.7606827633394));
#78526=CARTESIAN_POINT('Ctrl Pts',(3.93819516766651,140.322505061653,12.6645855781701));
#78527=CARTESIAN_POINT('Ctrl Pts',(3.92898793419198,140.244856830283,12.528730705472));
#78528=CARTESIAN_POINT('Ctrl Pts',(3.92599731878192,140.216728219209,12.4850778032827));
#78529=CARTESIAN_POINT('Ctrl Pts',(3.92203972465949,140.175360037575,12.4278116871143));
#78530=CARTESIAN_POINT('Ctrl Pts',(3.92100053856733,140.164091379071,12.4128275374667));
#78531=CARTESIAN_POINT('Ctrl Pts',(3.91923880735301,140.144291787919,12.3875266733303));
#78532=CARTESIAN_POINT('Ctrl Pts',(3.91851086829859,140.135901725426,12.3771031722908));
#78533=CARTESIAN_POINT('Ctrl Pts',(3.91703393597284,140.118454840155,12.3560262281017));
#78534=CARTESIAN_POINT('Ctrl Pts',(3.91628554258756,140.109385915296,12.3453845691111));
#78535=CARTESIAN_POINT('Ctrl Pts',(3.91437868821074,140.085701650427,12.318386413845));
#78536=CARTESIAN_POINT('Ctrl Pts',(3.91322936510204,140.070868354315,12.3022253058966));
#78537=CARTESIAN_POINT('Ctrl Pts',(3.90598094691075,139.973904239718,12.2012356758357));
#78538=CARTESIAN_POINT('Ctrl Pts',(3.90033833442323,139.882129184797,12.1262785233545));
#78539=CARTESIAN_POINT('Ctrl Pts',(3.89238120764606,139.744387148381,12.0391523330544));
#78540=CARTESIAN_POINT('Ctrl Pts',(3.89016961381543,139.70535038004,12.016906278948));
#78541=CARTESIAN_POINT('Ctrl Pts',(3.88651932870261,139.641335683084,11.9842310113233));
#78542=CARTESIAN_POINT('Ctrl Pts',(3.88512535964433,139.616983478467,11.9726376876532));
#78543=CARTESIAN_POINT('Ctrl Pts',(3.88314274142508,139.582796035947,11.9575061818194));
#78544=CARTESIAN_POINT('Ctrl Pts',(3.88258473334658,139.573221139347,11.9533900400839));
#78545=CARTESIAN_POINT('Ctrl Pts',(3.88161693500578,139.556717614581,11.9465032627926));
#78546=CARTESIAN_POINT('Ctrl Pts',(3.88121006579688,139.549810401357,11.9436827653763));
#78547=CARTESIAN_POINT('Ctrl Pts',(3.88032172934466,139.534802596547,11.9376879515425));
#78548=CARTESIAN_POINT('Ctrl Pts',(3.87983924859187,139.526695186371,11.9345330075545));
#78549=CARTESIAN_POINT('Ctrl Pts',(3.87844760808565,139.503417803409,11.9257129183067));
#78550=CARTESIAN_POINT('Ctrl Pts',(3.87752902467003,139.488181697183,11.9202271729243));
#78551=CARTESIAN_POINT('Ctrl Pts',(3.87263576209454,139.407494779144,11.8926796183376));
#78552=CARTESIAN_POINT('Ctrl Pts',(3.86848685203145,139.340637921975,11.875020313664));
#78553=CARTESIAN_POINT('Ctrl Pts',(3.86014374127758,139.204560953943,11.8492037326183));
#78554=CARTESIAN_POINT('Ctrl Pts',(3.85596079064354,139.135492925998,11.841131326362));
#78555=CARTESIAN_POINT('Ctrl Pts',(3.84908373439546,139.018277317928,11.8358310225527));
#78556=CARTESIAN_POINT('Ctrl Pts',(3.84633334790217,138.970364498649,11.8360166315343));
#78557=CARTESIAN_POINT('Ctrl Pts',(3.84263075183139,138.904282574278,11.8395189814417));
#78558=CARTESIAN_POINT('Ctrl Pts',(3.84161809719459,138.886041308312,11.8408289714711));
#78559=CARTESIAN_POINT('Ctrl Pts',(3.83988705475158,138.854578887924,11.8436820562074));
#78560=CARTESIAN_POINT('Ctrl Pts',(3.83916374590359,138.841345707555,11.8450642333475));
#78561=CARTESIAN_POINT('Ctrl Pts',(3.83768396061898,138.814102905639,11.8482858016616));
#78562=CARTESIAN_POINT('Ctrl Pts',(3.83692828080843,138.800097354914,11.8501480093337));
#78563=CARTESIAN_POINT('Ctrl Pts',(3.83497628356272,138.763696575985,11.855525440397));
#78564=CARTESIAN_POINT('Ctrl Pts',(3.83379000339494,138.74135179744,11.8593587394846));
#78565=CARTESIAN_POINT('Ctrl Pts',(3.82678163231227,138.60828751533,11.8853821633067));
#78566=CARTESIAN_POINT('Ctrl Pts',(3.82136769962694,138.500353465382,11.9198053462218));
#78567=CARTESIAN_POINT('Ctrl Pts',(3.81355275051088,138.354269567926,11.9858047700099));
#78568=CARTESIAN_POINT('Ctrl Pts',(3.81122592844991,138.312068630723,12.0073953166884));
#78569=CARTESIAN_POINT('Ctrl Pts',(3.80740991363426,138.246814161613,12.0448821599283));
#78570=CARTESIAN_POINT('Ctrl Pts',(3.80597057988463,138.223040152559,12.0594586220882));
#78571=CARTESIAN_POINT('Ctrl Pts',(3.80393392049375,138.190868025508,12.080471837516));
#78572=CARTESIAN_POINT('Ctrl Pts',(3.8033694847094,138.1821004754,12.0863345412152));
#78573=CARTESIAN_POINT('Ctrl Pts',(3.8023943832412,138.167226701139,12.0965147294686));
#78574=CARTESIAN_POINT('Ctrl Pts',(3.80198676743256,138.161088912129,12.1007851114584));
#78575=CARTESIAN_POINT('Ctrl Pts',(3.80110157825485,138.147936699133,12.1100861879634));
#78576=CARTESIAN_POINT('Ctrl Pts',(3.80062306992748,138.140933972358,12.1151319477517));
#78577=CARTESIAN_POINT('Ctrl Pts',(3.79925391112954,138.121183754555,12.1296299321361));
#78578=CARTESIAN_POINT('Ctrl Pts',(3.79835427523849,138.108545144009,12.139227719482));
#78579=CARTESIAN_POINT('Ctrl Pts',(3.79271121648546,138.031157533831,12.200005360638));
#78580=CARTESIAN_POINT('Ctrl Pts',(3.78771596629495,137.970682110082,12.2563779836028));
#78581=CARTESIAN_POINT('Ctrl Pts',(3.77880622281925,137.871357519453,12.3660406535302));
#78582=CARTESIAN_POINT('Ctrl Pts',(3.77489039654456,137.830730073361,12.4174338972059));
#78583=CARTESIAN_POINT('Ctrl Pts',(3.76868459473099,137.770337398581,12.5053545947858));
#78584=CARTESIAN_POINT('Ctrl Pts',(3.76633086988188,137.748442817897,12.540304984396));
#78585=CARTESIAN_POINT('Ctrl Pts',(3.76305838130558,137.719442002921,12.5912641816702));
#78586=CARTESIAN_POINT('Ctrl Pts',(3.7620964147948,137.711102775709,12.6065454404336));
#78587=CARTESIAN_POINT('Ctrl Pts',(3.76042321510648,137.696933329037,12.6336494008941));
#78588=CARTESIAN_POINT('Ctrl Pts',(3.75970794376827,137.690986613755,12.6454086462637));
#78589=CARTESIAN_POINT('Ctrl Pts',(3.75821806247147,137.678838684959,12.6702581626843));
#78590=CARTESIAN_POINT('Ctrl Pts',(3.75744468255218,137.672671334046,12.6833634498767));
#78591=CARTESIAN_POINT('Ctrl Pts',(3.75538401435701,137.656624989219,12.7188177564366));
#78592=CARTESIAN_POINT('Ctrl Pts',(3.75410905246291,137.647109260933,12.7413266091364));
#78593=CARTESIAN_POINT('Ctrl Pts',(3.74860499163086,137.607972059841,12.8407761050442));
#78594=CARTESIAN_POINT('Ctrl Pts',(3.74456837703722,137.58431694611,12.91990606702));
#78595=CARTESIAN_POINT('Ctrl Pts',(3.73731512557805,137.553800044451,13.0659263820307));
#78596=CARTESIAN_POINT('Ctrl Pts',(3.73409385448265,137.544633281552,13.1320963501165));
#78597=CARTESIAN_POINT('Ctrl Pts',(3.72904437780249,137.537671566675,13.2323895721751));
#78598=CARTESIAN_POINT('Ctrl Pts',(3.72731356542675,137.5365,13.2661909020476));
#78599=CARTESIAN_POINT('Ctrl Pts',(3.72552751600545,137.5365,13.2999999999998));
#78600=CARTESIAN_POINT('Ctrl Pts',(3.65157748137715,137.5365,13.3000000000035));
#78601=CARTESIAN_POINT('Ctrl Pts',(3.6559595390121,137.5365,13.2235985914167));
#78602=CARTESIAN_POINT('Ctrl Pts',(3.66056768225208,137.542482743807,13.1473188192194));
#78603=CARTESIAN_POINT('Ctrl Pts',(3.66936004533574,137.565232991498,13.0031619070513));
#78604=CARTESIAN_POINT('Ctrl Pts',(3.67353428369732,137.580958599639,12.9353192368978));
#78605=CARTESIAN_POINT('Ctrl Pts',(3.68007346966338,137.614016173195,12.8280886455043));
#78606=CARTESIAN_POINT('Ctrl Pts',(3.68251207469555,137.628358372174,12.787895273671));
#78607=CARTESIAN_POINT('Ctrl Pts',(3.68587396188387,137.651049815535,12.7321325411057));
#78608=CARTESIAN_POINT('Ctrl Pts',(3.68684399021867,137.657954399548,12.7160019733571));
#78609=CARTESIAN_POINT('Ctrl Pts',(3.68852268610921,137.6705293786,12.6880257872626));
#78610=CARTESIAN_POINT('Ctrl Pts',(3.6892355856517,137.676072141994,12.676125322923));
#78611=CARTESIAN_POINT('Ctrl Pts',(3.69071238411208,137.687975716195,12.651441328679));
#78612=CARTESIAN_POINT('Ctrl Pts',(3.69147520262237,137.694365008948,12.6386730300857));
#78613=CARTESIAN_POINT('Ctrl Pts',(3.69348738642181,137.711853620816,12.6049656862361));
#78614=CARTESIAN_POINT('Ctrl Pts',(3.69472535154334,137.723276600438,12.5841988859888));
#78615=CARTESIAN_POINT('Ctrl Pts',(3.70130413365152,137.787449489421,12.4739613712733));
#78616=CARTESIAN_POINT('Ctrl Pts',(3.70631289035946,137.849104639831,12.3900218699495));
#78617=CARTESIAN_POINT('Ctrl Pts',(3.71503692647108,137.969992526518,12.2575950189444));
#78618=CARTESIAN_POINT('Ctrl Pts',(3.7187272117014,138.025081508897,12.2058998390586));
#78619=CARTESIAN_POINT('Ctrl Pts',(3.72340276834783,138.094727030487,12.1499974887333));
#78620=CARTESIAN_POINT('Ctrl Pts',(3.72413811930958,138.105674644592,12.1414633988737));
#78621=CARTESIAN_POINT('Ctrl Pts',(3.72531844024373,138.123194436607,12.1282023427525));
#78622=CARTESIAN_POINT('Ctrl Pts',(3.72575663245445,138.129687535584,12.123371786218));
#78623=CARTESIAN_POINT('Ctrl Pts',(3.72661015792459,138.142303347593,12.1141477795188));
#78624=CARTESIAN_POINT('Ctrl Pts',(3.72702501439003,138.148420498184,12.1097473462109));
#78625=CARTESIAN_POINT('Ctrl Pts',(3.72808430974567,138.164010835324,12.0987139792721));
#78626=CARTESIAN_POINT('Ctrl Pts',(3.72873284863476,138.173529074821,12.0921457953897));
#78627=CARTESIAN_POINT('Ctrl Pts',(3.73131953313215,138.211435226257,12.0666459929452));
#78628=CARTESIAN_POINT('Ctrl Pts',(3.73330454516756,138.240402152435,12.0485978674107));
#78629=CARTESIAN_POINT('Ctrl Pts',(3.74099668692803,138.353285264456,11.9836289133351));
#78630=CARTESIAN_POINT('Ctrl Pts',(3.74687556360808,138.441121135358,11.9440028837653));
#78631=CARTESIAN_POINT('Ctrl Pts',(3.75624718454596,138.590809290217,11.8935080021171));
#78632=CARTESIAN_POINT('Ctrl Pts',(3.75983843349468,138.650606629817,11.8774731937288));
#78633=CARTESIAN_POINT('Ctrl Pts',(3.76441307319211,138.730476774297,11.8613984877837));
#78634=CARTESIAN_POINT('Ctrl Pts',(3.7655026005123,138.749784726641,11.857914895081));
#78635=CARTESIAN_POINT('Ctrl Pts',(3.76731973342343,138.782460885137,11.8526954442103));
#78636=CARTESIAN_POINT('Ctrl Pts',(3.76805370594936,138.795793203704,11.8507542150959));
#78637=CARTESIAN_POINT('Ctrl Pts',(3.76951914198925,138.822673593312,11.8472186584254));
#78638=CARTESIAN_POINT('Ctrl Pts',(3.77025038808297,138.836220938847,11.8456290991434));
#78639=CARTESIAN_POINT('Ctrl Pts',(3.77206619432492,138.870181056187,11.8421249843269));
#78640=CARTESIAN_POINT('Ctrl Pts',(3.77314323531011,138.890615834623,11.84044949435));
#78641=CARTESIAN_POINT('Ctrl Pts',(3.77782905041354,138.980662903238,11.8349682324521));
#78642=CARTESIAN_POINT('Ctrl Pts',(3.78129774082775,139.050463875804,11.8357094864554));
#78643=CARTESIAN_POINT('Ctrl Pts',(3.78970860472904,139.221773486801,11.8497976731603));
#78644=CARTESIAN_POINT('Ctrl Pts',(3.79455420759934,139.322429880264,11.8688097087033));
#78645=CARTESIAN_POINT('Ctrl Pts',(3.80094312821479,139.441914740646,11.9046312610839));
#78646=CARTESIAN_POINT('Ctrl Pts',(3.80211897084394,139.463398976648,11.9116182661255));
#78647=CARTESIAN_POINT('Ctrl Pts',(3.80383804376152,139.493891934969,11.922321639245));
#78648=CARTESIAN_POINT('Ctrl Pts',(3.80436030882322,139.503039495858,11.9256353597822));
#78649=CARTESIAN_POINT('Ctrl Pts',(3.80528296155999,139.518978881099,11.9315898770309));
#78650=CARTESIAN_POINT('Ctrl Pts',(3.80568104985409,139.52578509335,11.9341905784235));
#78651=CARTESIAN_POINT('Ctrl Pts',(3.80657888458789,139.540974485965,11.9401249186257));
#78652=CARTESIAN_POINT('Ctrl Pts',(3.80708011039229,139.549346377047,11.9434852817703));
#78653=CARTESIAN_POINT('Ctrl Pts',(3.80862275282325,139.574806919939,11.9539791389318));
#78654=CARTESIAN_POINT('Ctrl Pts',(3.8096771898035,139.591791154296,11.9613595256413));
#78655=CARTESIAN_POINT('Ctrl Pts',(3.81675792220808,139.703461500401,12.0124256210612));
#78656=CARTESIAN_POINT('Ctrl Pts',(3.82314857806906,139.793383380652,12.0658006937683));
#78657=CARTESIAN_POINT('Ctrl Pts',(3.83233156481164,139.916404085803,12.1578641275573));
#78658=CARTESIAN_POINT('Ctrl Pts',(3.83524590337054,139.954420029233,12.1894353538638));
#78659=CARTESIAN_POINT('Ctrl Pts',(3.84008511997826,140.01617245682,12.2462367012198));
#78660=CARTESIAN_POINT('Ctrl Pts',(3.84204256879515,140.040742288077,12.2704955953336));
#78661=CARTESIAN_POINT('Ctrl Pts',(3.84486968343108,140.075620493591,12.3074585437684));
#78662=CARTESIAN_POINT('Ctrl Pts',(3.84576810047058,140.08660960416,12.3195013579638));
#78663=CARTESIAN_POINT('Ctrl Pts',(3.8473672055468,140.10598985916,12.3414660053249));
#78664=CARTESIAN_POINT('Ctrl Pts',(3.84807090950391,140.114454300091,12.3513205938423));
#78665=CARTESIAN_POINT('Ctrl Pts',(3.84957368263292,140.132383976573,12.3727661223391));
#78666=CARTESIAN_POINT('Ctrl Pts',(3.85037091508543,140.141804957003,12.3843922254662));
#78667=CARTESIAN_POINT('Ctrl Pts',(3.85255550461618,140.167347713134,12.4169211328737));
#78668=CARTESIAN_POINT('Ctrl Pts',(3.85392787961937,140.18308515989,12.4381191588654));
#78669=CARTESIAN_POINT('Ctrl Pts',(3.86152059563325,140.268103248291,12.5593569099986));
#78670=CARTESIAN_POINT('Ctrl Pts',(3.86728023822072,140.325265167053,12.6672992339697));
#78671=CARTESIAN_POINT('Ctrl Pts',(3.87593215114509,140.38767303944,12.831868490789));
#78672=CARTESIAN_POINT('Ctrl Pts',(3.87864837312771,140.404091023392,12.8836937053413));
#78673=CARTESIAN_POINT('Ctrl Pts',(3.88217383030035,140.420764698408,12.9486836125298));
#78674=CARTESIAN_POINT('Ctrl Pts',(3.88285276687226,140.423777854834,12.961101592924));
#78675=CARTESIAN_POINT('Ctrl Pts',(3.88396342406861,140.428380797936,12.9812174701327));
#78676=CARTESIAN_POINT('Ctrl Pts',(3.88438967694581,140.43007190478,12.9888917446427));
#78677=CARTESIAN_POINT('Ctrl Pts',(3.885195338534,140.433125524312,13.0033003438746));
#78678=CARTESIAN_POINT('Ctrl Pts',(3.88557389634429,140.43450258235,13.0100313961806));
#78679=CARTESIAN_POINT('Ctrl Pts',(3.88660031175646,140.43808361763,13.0281855364697));
#78680=CARTESIAN_POINT('Ctrl Pts',(3.88725286792019,140.440198823085,13.0396254115975));
#78681=CARTESIAN_POINT('Ctrl Pts',(3.8898819530568,140.448094364926,13.0853717521105));
#78682=CARTESIAN_POINT('Ctrl Pts',(3.89190725257507,140.452786659995,13.1198524018986));
#78683=CARTESIAN_POINT('Ctrl Pts',(3.90028349260316,140.466880633635,13.2608787353366));
#78684=CARTESIAN_POINT('Ctrl Pts',(3.90683979102233,140.465820146062,13.3681395152964));
#78685=CARTESIAN_POINT('Ctrl Pts',(3.91621259908423,140.446851056471,13.5262481215619));
#78686=CARTESIAN_POINT('Ctrl Pts',(3.91922685476312,140.437844468185,13.5777955916369));
#78687=CARTESIAN_POINT('Ctrl Pts',(3.92320544304582,140.421891484899,13.6469976041969));
#78688=CARTESIAN_POINT('Ctrl Pts',(3.92424329842703,140.417336252384,13.6651584939201));
#78689=CARTESIAN_POINT('Ctrl Pts',(3.92600006245297,140.408947843428,13.6960750332449));
#78690=CARTESIAN_POINT('Ctrl Pts',(3.92672439351498,140.405286819029,13.7088745897112));
#78691=CARTESIAN_POINT('Ctrl Pts',(3.92819150907265,140.397457887946,13.734897541871));
#78692=CARTESIAN_POINT('Ctrl Pts',(3.92893374248915,140.3932756959,13.7481152460229));
#78693=CARTESIAN_POINT('Ctrl Pts',(3.93081911675292,140.382086819839,13.7818053565549));
#78694=CARTESIAN_POINT('Ctrl Pts',(3.93195342471692,140.374812684126,13.8021857489357));
#78695=CARTESIAN_POINT('Ctrl Pts',(3.93927729960581,140.324348613182,13.9342476408025));
#78696=CARTESIAN_POINT('Ctrl Pts',(3.9449938094545,140.268045884759,14.040425815554));
#78697=CARTESIAN_POINT('Ctrl Pts',(3.95300197059865,140.174105246651,14.1747932881044));
#78698=CARTESIAN_POINT('Ctrl Pts',(3.95518081178516,140.147148540434,14.2098550739459));
#78699=CARTESIAN_POINT('Ctrl Pts',(3.95878237032418,140.101450845468,14.2640278231389));
#78700=CARTESIAN_POINT('Ctrl Pts',(3.96016169376737,140.083700500262,14.2839393631438));
#78701=CARTESIAN_POINT('Ctrl Pts',(3.96212485849522,140.058326064124,14.3108833624017));
#78702=CARTESIAN_POINT('Ctrl Pts',(3.96267872459099,140.051155548001,14.3183374843031));
#78703=CARTESIAN_POINT('Ctrl Pts',(3.96363968540931,140.038711716985,14.3310020190881));
#78704=CARTESIAN_POINT('Ctrl Pts',(3.96404390844426,140.03347682495,14.3362494125651));
#78705=CARTESIAN_POINT('Ctrl Pts',(3.96492643957711,140.022051407912,14.3475294141827));
#78706=CARTESIAN_POINT('Ctrl Pts',(3.96540574897659,140.0158472488,14.3535470152796));
#78707=CARTESIAN_POINT('Ctrl Pts',(3.966787466933,139.997952635452,14.3705985228441));
#78708=CARTESIAN_POINT('Ctrl Pts',(3.96769916455442,139.986133510134,14.381494945388));
#78709=CARTESIAN_POINT('Ctrl Pts',(3.97223139678058,139.927184240608,14.4340723373437));
#78710=CARTESIAN_POINT('Ctrl Pts',(3.97599627123935,139.877582270678,14.4728763297018));
#78711=CARTESIAN_POINT('Ctrl Pts',(3.98304077816822,139.780947300625,14.5389042712005));
#78712=CARTESIAN_POINT('Ctrl Pts',(3.98630986891245,139.73459128679,14.5669405815518));
#78713=CARTESIAN_POINT('Ctrl Pts',(3.9921503458027,139.647883558447,14.613019469843));
#78714=CARTESIAN_POINT('Ctrl Pts',(3.99473585633516,139.608063501114,14.6319281078316));
#78715=CARTESIAN_POINT('Ctrl Pts',(3.99910354093672,139.537999086306,14.6613999964778));
#78716=CARTESIAN_POINT('Ctrl Pts',(4.00091024156335,139.508150550561,14.6728205297644));
#78717=CARTESIAN_POINT('Ctrl Pts',(4.00356584191722,139.462962008761,14.6884343340623));
#78718=CARTESIAN_POINT('Ctrl Pts',(4.00443867784491,139.447890073429,14.6933693808845));
#78719=CARTESIAN_POINT('Ctrl Pts',(4.00594189783183,139.421557837628,14.7015199862459));
#78720=CARTESIAN_POINT('Ctrl Pts',(4.00657586982329,139.410333859412,14.7048471152453));
#78721=CARTESIAN_POINT('Ctrl Pts',(4.00800246387277,139.38481504522,14.7120797380649));
#78722=CARTESIAN_POINT('Ctrl Pts',(4.00879238663683,139.370498280608,14.7159035459655));
#78723=CARTESIAN_POINT('Ctrl Pts',(4.01093361213583,139.331203440597,14.7257618087751));
#78724=CARTESIAN_POINT('Ctrl Pts',(4.01227093681568,139.306120124011,14.7313570578386));
#78725=CARTESIAN_POINT('Ctrl Pts',(4.01940991845956,139.169661360009,14.7580449039939));
#78726=CARTESIAN_POINT('Ctrl Pts',(4.02481732361069,139.056274180173,14.7668040410783));
#78727=CARTESIAN_POINT('Ctrl Pts',(4.03246117195231,138.900033933597,14.7607151134656));
#78728=CARTESIAN_POINT('Ctrl Pts',(4.03458388500347,138.857156287189,14.7571469230109));
#78729=CARTESIAN_POINT('Ctrl Pts',(4.03810396074534,138.788503002239,14.7483743202933));
#78730=CARTESIAN_POINT('Ctrl Pts',(4.03946031416457,138.762600955802,14.7443547656003));
#78731=CARTESIAN_POINT('Ctrl Pts',(4.04139606006478,138.726711888992,14.7377939684263));
#78732=CARTESIAN_POINT('Ctrl Pts',(4.04194657371947,138.71662148115,14.7358392981711));
#78733=CARTESIAN_POINT('Ctrl Pts',(4.04290375600285,138.699298700405,14.7322938959975));
#78734=CARTESIAN_POINT('Ctrl Pts',(4.04330761959031,138.692056429221,14.7307542876261));
#78735=CARTESIAN_POINT('Ctrl Pts',(4.0441919269265,138.676348822641,14.7272902717135));
#78736=CARTESIAN_POINT('Ctrl Pts',(4.04467341440647,138.667888840573,14.7253454929711));
#78737=CARTESIAN_POINT('Ctrl Pts',(4.04606752076343,138.643639357422,14.719543421416));
#78738=CARTESIAN_POINT('Ctrl Pts',(4.04698967263832,138.62789658688,14.7154983004126));
#78739=CARTESIAN_POINT('Ctrl Pts',(4.05222164705189,138.540007805663,14.6913477525239));
#78740=CARTESIAN_POINT('Ctrl Pts',(4.05673629204259,138.469425139258,14.6659905546303));
#78741=CARTESIAN_POINT('Ctrl Pts',(4.06547668218033,138.337053820994,14.6066221283293));
#78742=CARTESIAN_POINT('Ctrl Pts',(4.06969138821679,138.275154199536,14.5733259382087));
#78743=CARTESIAN_POINT('Ctrl Pts',(4.07628260744218,138.179679065078,14.512742344237));
#78744=CARTESIAN_POINT('Ctrl Pts',(4.07873436937187,138.144502860815,14.4881900494096));
#78745=CARTESIAN_POINT('Ctrl Pts',(4.08211062087354,138.096497320693,14.4514443232666));
#78746=CARTESIAN_POINT('Ctrl Pts',(4.08308240477574,138.082734844035,14.4405111979827));
#78747=CARTESIAN_POINT('Ctrl Pts',(4.08476309656061,138.05903918876,14.4209805680931));
#78748=CARTESIAN_POINT('Ctrl Pts',(4.08547626664903,138.049018825852,14.4124924738826));
#78749=CARTESIAN_POINT('Ctrl Pts',(4.08695267026238,138.028355264155,14.3945054624182));
#78750=CARTESIAN_POINT('Ctrl Pts',(4.08771483885581,138.017733943762,14.3849834626508));
#78751=CARTESIAN_POINT('Ctrl Pts',(4.08972304396049,137.989889434926,14.3592768196595));
#78752=CARTESIAN_POINT('Ctrl Pts',(4.09095776450311,137.972915866849,14.3428274063508));
#78753=CARTESIAN_POINT('Ctrl Pts',(4.09756780077649,137.883081158669,14.2514447140352));
#78754=CARTESIAN_POINT('Ctrl Pts',(4.10260592464691,137.818008848913,14.169283283989));
#78755=CARTESIAN_POINT('Ctrl Pts',(4.11021619046105,137.734559770707,14.0370105296152));
#78756=CARTESIAN_POINT('Ctrl Pts',(4.11275240513295,137.709233261231,13.9916965908737));
#78757=CARTESIAN_POINT('Ctrl Pts',(4.11686444382543,137.673393637549,13.9187196249728));
#78758=CARTESIAN_POINT('Ctrl Pts',(4.11838035725497,137.661220664982,13.8919189927172));
#78759=CARTESIAN_POINT('Ctrl Pts',(4.12050593524552,137.645731550318,13.8548909103951));
#78760=CARTESIAN_POINT('Ctrl Pts',(4.12107868444872,137.641707180174,13.8449656486929));
#78761=CARTESIAN_POINT('Ctrl Pts',(4.12206127345906,137.635063919493,13.8280506110251));
#78762=CARTESIAN_POINT('Ctrl Pts',(4.12246787956441,137.632388848541,13.821083188101));
#78763=CARTESIAN_POINT('Ctrl Pts',(4.12334197325096,137.626797716945,13.8061809927464));
#78764=CARTESIAN_POINT('Ctrl Pts',(4.12381025777677,137.623896974158,13.7982410687968));
#78765=CARTESIAN_POINT('Ctrl Pts',(4.12513005722918,137.615978320578,13.775969344801));
#78766=CARTESIAN_POINT('Ctrl Pts',(4.12598968430334,137.61111456798,13.7615842786274));
#78767=CARTESIAN_POINT('Ctrl Pts',(4.13198503240694,137.579120818063,13.6618719060824));
#78768=CARTESIAN_POINT('Ctrl Pts',(4.13742270801435,137.559649003968,13.5742919889431));
#78769=CARTESIAN_POINT('Ctrl Pts',(4.1465190212976,137.540485762504,13.4243136421574));
#78770=CARTESIAN_POINT('Ctrl Pts',(4.15019876702927,137.536543412072,13.3627020648448));
#78771=CARTESIAN_POINT('Ctrl Pts',(4.15380065009266,137.536500118786,13.3006810578158));
#78772=CARTESIAN_POINT('Ctrl Pts',(4.15382042339436,137.5365,13.3003405284137));
#78773=CARTESIAN_POINT('Ctrl Pts',(4.15384019369498,137.5365,13.3000000000084));
#78774=CARTESIAN_POINT('Origin',(4.2,139.,13.3));
#78775=CARTESIAN_POINT('',(4.72326784382708,137.5365,13.299999999986));
#78776=CARTESIAN_POINT('',(4.65349091708139,137.5365,13.3000000000138));
#78777=CARTESIAN_POINT('',(4.2,137.5365,13.3));
#78778=CARTESIAN_POINT('Ctrl Pts',(4.72326784382709,137.5365,13.299999999986));
#78779=CARTESIAN_POINT('Ctrl Pts',(4.72061524380913,137.5365,13.3453339538471));
#78780=CARTESIAN_POINT('Ctrl Pts',(4.71801361931224,137.53860639665,13.3906465426194));
#78781=CARTESIAN_POINT('Ctrl Pts',(4.71444138633859,137.544527309669,13.4541839839692));
#78782=CARTESIAN_POINT('Ctrl Pts',(4.7134180312487,137.546589320802,13.4725424436615));
#78783=CARTESIAN_POINT('Ctrl Pts',(4.71167463899143,137.550737327058,13.5040778128034));
#78784=CARTESIAN_POINT('Ctrl Pts',(4.71094949104831,137.552656886909,13.5172739706296));
#78785=CARTESIAN_POINT('Ctrl Pts',(4.7094710256624,137.556971359962,13.5443326401013));
#78786=CARTESIAN_POINT('Ctrl Pts',(4.70871842341543,137.559386331807,13.5581905745248));
#78787=CARTESIAN_POINT('Ctrl Pts',(4.70678543932857,137.566156359927,13.5939805379733));
#78788=CARTESIAN_POINT('Ctrl Pts',(4.70561471242539,137.570814966113,13.6158517843623));
#78789=CARTESIAN_POINT('Ctrl Pts',(4.70306634081857,137.582180418672,13.6637910703942));
#78790=CARTESIAN_POINT('Ctrl Pts',(4.70169559515881,137.589108896027,13.6897982854271));
#78791=CARTESIAN_POINT('Ctrl Pts',(4.69734817772567,137.613644266652,13.7726404065773));
#78792=CARTESIAN_POINT('Ctrl Pts',(4.69444289289453,137.634000460912,13.8285990321994));
#78793=CARTESIAN_POINT('Ctrl Pts',(4.68700466870989,137.69495885825,13.9689093254457));
#78794=CARTESIAN_POINT('Ctrl Pts',(4.68251287172916,137.740337030202,14.0508778103034));
#78795=CARTESIAN_POINT('Ctrl Pts',(4.67685289757051,137.801705914959,14.1403266265909));
#78796=CARTESIAN_POINT('Ctrl Pts',(4.67605988082319,137.810387216702,14.1525719588196));
#78797=CARTESIAN_POINT('Ctrl Pts',(4.67480661410092,137.824195091883,14.1714269787448));
#78798=CARTESIAN_POINT('Ctrl Pts',(4.67435456923428,137.829192801036,14.1781302051289));
#78799=CARTESIAN_POINT('Ctrl Pts',(4.67348574573492,137.838822564522,14.1908178705304));
#78800=CARTESIAN_POINT('Ctrl Pts',(4.67306965128551,137.843444025805,14.1968097814536));
#78801=CARTESIAN_POINT('Ctrl Pts',(4.67203382195927,137.854977300894,14.211525726363));
#78802=CARTESIAN_POINT('Ctrl Pts',(4.67141052552929,137.861942504336,14.2202071790097));
#78803=CARTESIAN_POINT('Ctrl Pts',(4.66893853649453,137.889696386245,14.2540026206678));
#78804=CARTESIAN_POINT('Ctrl Pts',(4.66704650263296,137.911221698844,14.278497131732));
#78805=CARTESIAN_POINT('Ctrl Pts',(4.66147800265538,137.975936429219,14.3473574751078));
#78806=CARTESIAN_POINT('Ctrl Pts',(4.65773413139017,138.02114533015,14.3897279393647));
#78807=CARTESIAN_POINT('Ctrl Pts',(4.64865261700329,138.137540046658,14.4857110019324));
#78808=CARTESIAN_POINT('Ctrl Pts',(4.64336233459033,138.211207212264,14.5359439597559));
#78809=CARTESIAN_POINT('Ctrl Pts',(4.63692862724951,138.310329913068,14.5910397088626));
#78810=CARTESIAN_POINT('Ctrl Pts',(4.63556149513708,138.33196454868,14.6023659605611));
#78811=CARTESIAN_POINT('Ctrl Pts',(4.63341360162938,138.366865154074,14.619538618867));
#78812=CARTESIAN_POINT('Ctrl Pts',(4.63262075420044,138.379951364202,14.625738137889));
#78813=CARTESIAN_POINT('Ctrl Pts',(4.6311191113978,138.40511887321,14.6372069176151));
#78814=CARTESIAN_POINT('Ctrl Pts',(4.63040923946097,138.417183494506,14.6425091553187));
#78815=CARTESIAN_POINT('Ctrl Pts',(4.62877395032389,138.445354060618,14.6544384028692));
#78816=CARTESIAN_POINT('Ctrl Pts',(4.62785274418139,138.461510106765,14.660942384727));
#78817=CARTESIAN_POINT('Ctrl Pts',(4.62477881320439,138.516335551381,14.6818843929356));
#78818=CARTESIAN_POINT('Ctrl Pts',(4.62266996606128,138.555499756284,14.6949751549734));
#78819=CARTESIAN_POINT('Ctrl Pts',(4.61730915445143,138.658186686741,14.7245337516346));
#78820=CARTESIAN_POINT('Ctrl Pts',(4.61412380821832,138.722356023647,14.7384182611133));
#78821=CARTESIAN_POINT('Ctrl Pts',(4.60693935348308,138.868633644632,14.7599119310595));
#78822=CARTESIAN_POINT('Ctrl Pts',(4.60295292946381,138.950881513117,14.7649862391874));
#78823=CARTESIAN_POINT('Ctrl Pts',(4.59784738573456,139.049008834441,14.7627656247637));
#78824=CARTESIAN_POINT('Ctrl Pts',(4.59700942133953,139.064899696617,14.7621467532466));
#78825=CARTESIAN_POINT('Ctrl Pts',(4.5956958951159,139.089401785117,14.7607923160744));
#78826=CARTESIAN_POINT('Ctrl Pts',(4.59522965068714,139.098022288642,14.760239190423));
#78827=CARTESIAN_POINT('Ctrl Pts',(4.59435195000735,139.114093233815,14.7590650683276));
#78828=CARTESIAN_POINT('Ctrl Pts',(4.59394151438726,139.121544565854,14.7584632491666));
#78829=CARTESIAN_POINT('Ctrl Pts',(4.59294528427974,139.139483738102,14.7568759385589));
#78830=CARTESIAN_POINT('Ctrl Pts',(4.59235653955841,139.149966024748,14.7558342596704));
#78831=CARTESIAN_POINT('Ctrl Pts',(4.59019548031936,139.188053226898,14.7516336424636));
#78832=CARTESIAN_POINT('Ctrl Pts',(4.58859200771951,139.215576642738,14.7478020474996));
#78833=CARTESIAN_POINT('Ctrl Pts',(4.58420553275568,139.289427177466,14.7353687199519));
#78834=CARTESIAN_POINT('Ctrl Pts',(4.58138109121222,139.335475147444,14.7253096112762));
#78835=CARTESIAN_POINT('Ctrl Pts',(4.57171610680341,139.49049036792,14.683517750077));
#78836=CARTESIAN_POINT('Ctrl Pts',(4.56489066287521,139.596238515597,14.6413461354945));
#78837=CARTESIAN_POINT('Ctrl Pts',(4.55719925712931,139.715934922768,14.5766283203304));
#78838=CARTESIAN_POINT('Ctrl Pts',(4.55593780948091,139.735557950647,14.5654237485081));
#78839=CARTESIAN_POINT('Ctrl Pts',(4.55391464452965,139.767004786916,14.5464891002431));
#78840=CARTESIAN_POINT('Ctrl Pts',(4.55314318417796,139.778989432255,14.5390346662714));
#78841=CARTESIAN_POINT('Ctrl Pts',(4.55165641420507,139.802064920249,14.5242145655376));
#78842=CARTESIAN_POINT('Ctrl Pts',(4.55094047554314,139.813166740185,14.5168686484249));
#78843=CARTESIAN_POINT('Ctrl Pts',(4.54925189567034,139.839314072328,14.4990496749514));
#78844=CARTESIAN_POINT('Ctrl Pts',(4.54828439141823,139.854266244477,14.4884432920331));
#78845=CARTESIAN_POINT('Ctrl Pts',(4.54480660739406,139.907834774698,14.4489107395221));
#78846=CARTESIAN_POINT('Ctrl Pts',(4.54235867710823,139.945215399676,14.4183596358661));
#78847=CARTESIAN_POINT('Ctrl Pts',(4.53557279854838,140.046384972724,14.3269710087976));
#78848=CARTESIAN_POINT('Ctrl Pts',(4.53136585453615,140.106283400253,14.2621475302998));
#78849=CARTESIAN_POINT('Ctrl Pts',(4.5242997567057,140.194046433971,14.1480597011772));
#78850=CARTESIAN_POINT('Ctrl Pts',(4.52151282410431,140.22553785362,14.1018777984787));
#78851=CARTESIAN_POINT('Ctrl Pts',(4.51789491042624,140.261045618056,14.0428102653399));
#78852=CARTESIAN_POINT('Ctrl Pts',(4.51720085158219,140.267630106552,14.0315169379568));
#78853=CARTESIAN_POINT('Ctrl Pts',(4.51606981659935,140.277975434385,14.013214052116));
#78854=CARTESIAN_POINT('Ctrl Pts',(4.5156386232797,140.281832077576,14.0062591690428));
#78855=CARTESIAN_POINT('Ctrl Pts',(4.51477613502987,140.289368207323,13.9924038041014));
#78856=CARTESIAN_POINT('Ctrl Pts',(4.51434496133859,140.29304943079,13.9855046056288));
#78857=CARTESIAN_POINT('Ctrl Pts',(4.51321909779949,140.302445750852,13.9675494080406));
#78858=CARTESIAN_POINT('Ctrl Pts',(4.51251946431231,140.308075329569,13.9564495845292));
#78859=CARTESIAN_POINT('Ctrl Pts',(4.50910723641913,140.334571586698,13.9025125266296));
#78860=CARTESIAN_POINT('Ctrl Pts',(4.50630157970903,140.353477921117,13.8587481052505));
#78861=CARTESIAN_POINT('Ctrl Pts',(4.4998458088929,140.391464907886,13.7575111675326));
#78862=CARTESIAN_POINT('Ctrl Pts',(4.49617951182463,140.409183511943,13.6996159626668));
#78863=CARTESIAN_POINT('Ctrl Pts',(4.48779353900733,140.441767722605,13.5635320661247));
#78864=CARTESIAN_POINT('Ctrl Pts',(4.48312263413881,140.453947311259,13.4848876952869));
#78865=CARTESIAN_POINT('Ctrl Pts',(4.47747031874333,140.461191682427,13.3847830675418));
#78866=CARTESIAN_POINT('Ctrl Pts',(4.47630646862535,140.462253741338,13.3639011811713));
#78867=CARTESIAN_POINT('Ctrl Pts',(4.4743985819566,140.463272922123,13.329230808299));
#78868=CARTESIAN_POINT('Ctrl Pts',(4.47364680406799,140.463483275162,13.3154533593042));
#78869=CARTESIAN_POINT('Ctrl Pts',(4.47216953385779,140.463514507769,13.2881588164907));
#78870=CARTESIAN_POINT('Ctrl Pts',(4.4714438862747,140.463342739576,13.2746431194095));
#78871=CARTESIAN_POINT('Ctrl Pts',(4.46968422028167,140.462465340623,13.2416184899986));
#78872=CARTESIAN_POINT('Ctrl Pts',(4.4686565901549,140.461556570574,13.2221173199478));
#78873=CARTESIAN_POINT('Ctrl Pts',(4.46452411382651,140.456277016541,13.1429320972543));
#78874=CARTESIAN_POINT('Ctrl Pts',(4.4615197971198,140.448637769159,13.0835222071212));
#78875=CARTESIAN_POINT('Ctrl Pts',(4.45566792211834,140.426294644332,12.9668475265027));
#78876=CARTESIAN_POINT('Ctrl Pts',(4.45282367913398,140.41171996263,12.9096747290141));
#78877=CARTESIAN_POINT('Ctrl Pts',(4.44679792735274,140.374005493121,12.7919403061043));
#78878=CARTESIAN_POINT('Ctrl Pts',(4.44361672799574,140.350213753348,12.7317244313659));
#78879=CARTESIAN_POINT('Ctrl Pts',(4.4394133888414,140.315580022539,12.6586388360612));
#78880=CARTESIAN_POINT('Ctrl Pts',(4.4385599254505,140.308396865528,12.6441093549624));
#78881=CARTESIAN_POINT('Ctrl Pts',(4.4372271592523,140.296988252589,12.6219664753817));
#78882=CARTESIAN_POINT('Ctrl Pts',(4.43675760533899,140.292933482964,12.6142660947776));
#78883=CARTESIAN_POINT('Ctrl Pts',(4.43587749063871,140.285275541539,12.6000323617701));
#78884=CARTESIAN_POINT('Ctrl Pts',(4.43546802553276,140.281690730425,12.5934897204696));
#78885=CARTESIAN_POINT('Ctrl Pts',(4.43447943289447,140.272981014828,12.5778780610627));
#78886=CARTESIAN_POINT('Ctrl Pts',(4.43389747496432,140.267809086137,12.5688359507009));
#78887=CARTESIAN_POINT('Ctrl Pts',(4.43179231625153,140.248922432107,12.5366192614772));
#78888=CARTESIAN_POINT('Ctrl Pts',(4.43023992948614,140.234665841876,12.5137700864426));
#78889=CARTESIAN_POINT('Ctrl Pts',(4.42604350681794,140.19503015121,12.4539841918559));
#78890=CARTESIAN_POINT('Ctrl Pts',(4.42336176831437,140.16857141976,12.4177980494649));
#78891=CARTESIAN_POINT('Ctrl Pts',(4.41355124002165,140.066380135663,12.2907162004508));
#78892=CARTESIAN_POINT('Ctrl Pts',(4.40642153497016,139.981350967856,12.2078556047324));
#78893=CARTESIAN_POINT('Ctrl Pts',(4.39850797964479,139.869847984118,12.1228524484857));
#78894=CARTESIAN_POINT('Ctrl Pts',(4.39728661682781,139.852134989961,12.1099672670553));
#78895=CARTESIAN_POINT('Ctrl Pts',(4.39531081857828,139.822656524541,12.0895191979166));
#78896=CARTESIAN_POINT('Ctrl Pts',(4.39454748063528,139.811060532055,12.0817190956297));
#78897=CARTESIAN_POINT('Ctrl Pts',(4.39306525688809,139.788143506692,12.0667761027732));
#78898=CARTESIAN_POINT('Ctrl Pts',(4.39234592795921,139.776832717028,12.0596200929069));
#78899=CARTESIAN_POINT('Ctrl Pts',(4.39063134363075,139.749428355323,12.0428040566279));
#78900=CARTESIAN_POINT('Ctrl Pts',(4.38964167918662,139.733243825585,12.0332963903809));
#78901=CARTESIAN_POINT('Ctrl Pts',(4.38594435343274,139.671463446012,11.9985842466251));
#78902=CARTESIAN_POINT('Ctrl Pts',(4.38331066303194,139.624714240454,11.9755080521171));
#78903=CARTESIAN_POINT('Ctrl Pts',(4.37548701779975,139.479703507052,11.9133185222476));
#78904=CARTESIAN_POINT('Ctrl Pts',(4.37049556356813,139.378357345495,11.8823101177945));
#78905=CARTESIAN_POINT('Ctrl Pts',(4.363406849765,139.239242829361,11.8557396286439));
#78906=CARTESIAN_POINT('Ctrl Pts',(4.36157267617855,139.203690079903,11.8502982564802));
#78907=CARTESIAN_POINT('Ctrl Pts',(4.35905495496564,139.156263194633,11.8448185410939));
#78908=CARTESIAN_POINT('Ctrl Pts',(4.35842662066347,139.144535125688,11.8436069060677));
#78909=CARTESIAN_POINT('Ctrl Pts',(4.35741707671776,139.125894563764,11.8419085051731));
#78910=CARTESIAN_POINT('Ctrl Pts',(4.3570408182921,139.118990814221,11.8413288819334));
#78911=CARTESIAN_POINT('Ctrl Pts',(4.35622997632615,139.104214740743,11.8401939107736));
#78912=CARTESIAN_POINT('Ctrl Pts',(4.35579457795852,139.096341558384,11.8396531821344));
#78913=CARTESIAN_POINT('Ctrl Pts',(4.35464505300111,139.075701386944,11.8384032544777));
#78914=CARTESIAN_POINT('Ctrl Pts',(4.35392561240461,139.062929051513,11.8377976685513));
#78915=CARTESIAN_POINT('Ctrl Pts',(4.35015562016846,138.996644400834,11.8355249066066));
#78916=CARTESIAN_POINT('Ctrl Pts',(4.34698783984977,138.943081776475,11.8366278953048));
#78917=CARTESIAN_POINT('Ctrl Pts',(4.33672789560924,138.772288474592,11.8495362427571));
#78918=CARTESIAN_POINT('Ctrl Pts',(4.32956424276089,138.656351667912,11.8725509790387));
#78919=CARTESIAN_POINT('Ctrl Pts',(4.32129741046464,138.519115914299,11.9175052109642));
#78920=CARTESIAN_POINT('Ctrl Pts',(4.31979359506577,138.494040061178,11.9264840682957));
#78921=CARTESIAN_POINT('Ctrl Pts',(4.31739925764554,138.453935876973,11.9420915793491));
#78922=CARTESIAN_POINT('Ctrl Pts',(4.31649515605332,138.438750446375,11.9482972683423));
#78923=CARTESIAN_POINT('Ctrl Pts',(4.31488594808555,138.411656240579,11.9599049467496));
#78924=CARTESIAN_POINT('Ctrl Pts',(4.31417778983348,138.39970963308,11.9652136418841));
#78925=CARTESIAN_POINT('Ctrl Pts',(4.31266524806803,138.374152975368,11.9769827422231));
#78926=CARTESIAN_POINT('Ctrl Pts',(4.31186273103771,138.360568246003,11.9834946952689));
#78927=CARTESIAN_POINT('Ctrl Pts',(4.30962179824281,138.322592345118,12.0024252831896));
#78928=CARTESIAN_POINT('Ctrl Pts',(4.3081999258387,138.298444985847,12.0153202882339));
#78929=CARTESIAN_POINT('Ctrl Pts',(4.302493013396,138.201662661238,12.0705465396761));
#78930=CARTESIAN_POINT('Ctrl Pts',(4.29839919908082,138.13237429301,12.1184225302951));
#78931=CARTESIAN_POINT('Ctrl Pts',(4.29015156213149,138.001555283847,12.2265580233159));
#78932=CARTESIAN_POINT('Ctrl Pts',(4.28601050084204,137.940458406364,12.2868178083429));
#78933=CARTESIAN_POINT('Ctrl Pts',(4.28074611099032,137.874993355294,12.3638213943632));
#78934=CARTESIAN_POINT('Ctrl Pts',(4.27993216898166,137.865186055896,12.3757340168827));
#78935=CARTESIAN_POINT('Ctrl Pts',(4.2786484915229,137.850247940468,12.3944751029844));
#78936=CARTESIAN_POINT('Ctrl Pts',(4.27818742170565,137.844985212898,12.401197478999));
#78937=CARTESIAN_POINT('Ctrl Pts',(4.27731325681139,137.835207917254,12.4139142461282));
#78938=CARTESIAN_POINT('Ctrl Pts',(4.27690106272641,137.830680183305,12.4198978944214));
#78939=CARTESIAN_POINT('Ctrl Pts',(4.27589179586616,137.819788962989,12.4345236362853));
#78940=CARTESIAN_POINT('Ctrl Pts',(4.27529157010167,137.813474220414,12.4432013139837));
#78941=CARTESIAN_POINT('Ctrl Pts',(4.27303235851283,137.790279705423,12.4758232592277));
#78942=CARTESIAN_POINT('Ctrl Pts',(4.27133859180853,137.774025505082,12.5002020192344));
#78943=CARTESIAN_POINT('Ctrl Pts',(4.26660342064742,137.731303958476,12.5686428125337));
#78944=CARTESIAN_POINT('Ctrl Pts',(4.26351337388326,137.706409026388,12.6136364328211));
#78945=CARTESIAN_POINT('Ctrl Pts',(4.25380586780446,137.635921784948,12.7585478612234));
#78946=CARTESIAN_POINT('Ctrl Pts',(4.24723054336891,137.599159407215,12.8623556247961));
#78947=CARTESIAN_POINT('Ctrl Pts',(4.23984036412408,137.569535098134,12.9900700359249));
#78948=CARTESIAN_POINT('Ctrl Pts',(4.23865307596634,137.565173513987,13.0109335015103));
#78949=CARTESIAN_POINT('Ctrl Pts',(4.23671752771,137.558730285462,13.0455085653541));
#78950=CARTESIAN_POINT('Ctrl Pts',(4.23596105933893,137.556385137852,13.0591672184189));
#78951=CARTESIAN_POINT('Ctrl Pts',(4.23454010988995,137.552312125227,13.085092005668));
#78952=CARTESIAN_POINT('Ctrl Pts',(4.23387445778955,137.550545307902,13.0973507036926));
#78953=CARTESIAN_POINT('Ctrl Pts',(4.23251030404093,137.547219753015,13.1226993111181));
#78954=CARTESIAN_POINT('Ctrl Pts',(4.23181250406407,137.545681827711,13.1357908375227));
#78955=CARTESIAN_POINT('Ctrl Pts',(4.2300265921284,137.542172459393,13.1696000340503));
#78956=CARTESIAN_POINT('Ctrl Pts',(4.22894654802664,137.540465631519,13.1903424854856));
#78957=CARTESIAN_POINT('Ctrl Pts',(4.22635640040071,137.537401034063,13.2407082029399));
#78958=CARTESIAN_POINT('Ctrl Pts',(4.22485915534941,137.5365,13.2703501628265));
#78959=CARTESIAN_POINT('Ctrl Pts',(4.22337996970853,137.5365,13.299999999996));
#78960=CARTESIAN_POINT('Ctrl Pts',(4.15384019369498,137.5365,13.3000000000084));
#78961=CARTESIAN_POINT('Ctrl Pts',(4.15607472658841,137.5365,13.2615118688951));
#78962=CARTESIAN_POINT('Ctrl Pts',(4.15826981926394,137.538018265763,13.2230364088225));
#78963=CARTESIAN_POINT('Ctrl Pts',(4.16138452616685,137.542414759486,13.1674233280491));
#78964=CARTESIAN_POINT('Ctrl Pts',(4.16234063728151,137.544083120963,13.1502088626569));
#78965=CARTESIAN_POINT('Ctrl Pts',(4.16400620404721,137.547554843945,13.1199782017664));
#78966=CARTESIAN_POINT('Ctrl Pts',(4.16471960742066,137.549229078288,13.1069494169621));
#78967=CARTESIAN_POINT('Ctrl Pts',(4.16619567982448,137.553085232305,13.0798340624415));
#78968=CARTESIAN_POINT('Ctrl Pts',(4.16695729710165,137.555298003072,13.0657532400044));
#78969=CARTESIAN_POINT('Ctrl Pts',(4.16896212673931,137.561716254987,13.0284709664775));
#78970=CARTESIAN_POINT('Ctrl Pts',(4.17019409437374,137.566277391314,13.0053345800878));
#78971=CARTESIAN_POINT('Ctrl Pts',(4.17512285334786,137.587016298755,12.9120725908745));
#78972=CARTESIAN_POINT('Ctrl Pts',(4.17867733745783,137.607797370253,12.843071436529));
#78973=CARTESIAN_POINT('Ctrl Pts',(4.18724347397128,137.670706117532,12.6790640776115));
#78974=CARTESIAN_POINT('Ctrl Pts',(4.19217589461417,137.7180194162,12.5864842493955));
#78975=CARTESIAN_POINT('Ctrl Pts',(4.19839563671274,137.783410891301,12.4863683765902));
#78976=CARTESIAN_POINT('Ctrl Pts',(4.19923411764975,137.792329299431,12.4731887054791));
#78977=CARTESIAN_POINT('Ctrl Pts',(4.20054658233332,137.80640078228,12.4531072847093));
#78978=CARTESIAN_POINT('Ctrl Pts',(4.20101120726351,137.811403084096,12.4461008679168));
#78979=CARTESIAN_POINT('Ctrl Pts',(4.20188418953157,137.820831637893,12.4331382539465));
#78980=CARTESIAN_POINT('Ctrl Pts',(4.20229150759562,137.825241806847,12.4271709835776));
#78981=CARTESIAN_POINT('Ctrl Pts',(4.20327729496526,137.835944467099,12.4129175803851));
#78982=CARTESIAN_POINT('Ctrl Pts',(4.20385861482471,137.842280217851,12.4046646460619));
#78983=CARTESIAN_POINT('Ctrl Pts',(4.20597367810308,137.865442541586,12.375150396395));
#78984=CARTESIAN_POINT('Ctrl Pts',(4.20753707628258,137.882770402185,12.3542911320474));
#78985=CARTESIAN_POINT('Ctrl Pts',(4.21177866697193,137.930619061791,12.2998422352468));
#78986=CARTESIAN_POINT('Ctrl Pts',(4.214495573892,137.962139311721,12.2671708928763));
#78987=CARTESIAN_POINT('Ctrl Pts',(4.22427759497091,138.080331219417,12.1555447967853));
#78988=CARTESIAN_POINT('Ctrl Pts',(4.23133951014079,138.174911759852,12.085583986997));
#78989=CARTESIAN_POINT('Ctrl Pts',(4.23920112383857,138.295971676181,12.0167771759081));
#78990=CARTESIAN_POINT('Ctrl Pts',(4.24042891555272,138.31535059719,12.0063339045895));
#78991=CARTESIAN_POINT('Ctrl Pts',(4.24240909776419,138.347373588144,11.9899979915115));
#78992=CARTESIAN_POINT('Ctrl Pts',(4.24317057485579,138.359878810792,11.9838421911854));
#78993=CARTESIAN_POINT('Ctrl Pts',(4.24464497763192,138.384458341932,11.9721759139507));
#78994=CARTESIAN_POINT('Ctrl Pts',(4.24535841163774,138.396523400525,11.9666492036496));
#78995=CARTESIAN_POINT('Ctrl Pts',(4.24705171010445,138.425558422576,11.9538238200286));
#78996=CARTESIAN_POINT('Ctrl Pts',(4.24802623978598,138.442594855711,11.9466807548848));
#78997=CARTESIAN_POINT('Ctrl Pts',(4.25160258310699,138.506254909727,11.9213954182307));
#78998=CARTESIAN_POINT('Ctrl Pts',(4.25413671055688,138.553665804301,11.9053239774023));
#78999=CARTESIAN_POINT('Ctrl Pts',(4.26137678335802,138.693884513256,11.8656775026844));
#79000=CARTESIAN_POINT('Ctrl Pts',(4.26592427193415,138.788286129175,11.8487370356814));
#79001=CARTESIAN_POINT('Ctrl Pts',(4.27297104799777,138.930352013112,11.837408095101));
#79002=CARTESIAN_POINT('Ctrl Pts',(4.27533008182458,138.977188667297,11.8359286707962));
#79003=CARTESIAN_POINT('Ctrl Pts',(4.27845650512993,139.03665357107,11.8369044351704));
#79004=CARTESIAN_POINT('Ctrl Pts',(4.27912855590273,139.049292043918,11.8372756961673));
#79005=CARTESIAN_POINT('Ctrl Pts',(4.28023072289703,139.069746510032,11.8381419423788));
#79006=CARTESIAN_POINT('Ctrl Pts',(4.28065552394442,139.077566363101,11.8385360046013));
#79007=CARTESIAN_POINT('Ctrl Pts',(4.28151252844178,139.093203606233,11.8394498582668));
#79008=CARTESIAN_POINT('Ctrl Pts',(4.28194472159916,139.10102073758,11.8399697148931));
#79009=CARTESIAN_POINT('Ctrl Pts',(4.28308416592121,139.121463599015,11.8414941686687));
#79010=CARTESIAN_POINT('Ctrl Pts',(4.28379662180679,139.13408087908,11.8425999308707));
#79011=CARTESIAN_POINT('Ctrl Pts',(4.28747903731392,139.198557637978,11.8490949280712));
#79012=CARTESIAN_POINT('Ctrl Pts',(4.29056038634395,139.250113118417,11.8570886422134));
#79013=CARTESIAN_POINT('Ctrl Pts',(4.30030688216188,139.409456753762,11.8905918066465));
#79014=CARTESIAN_POINT('Ctrl Pts',(4.30704757444879,139.514867928042,11.9255900863472));
#79015=CARTESIAN_POINT('Ctrl Pts',(4.31546563218395,139.647184363066,11.9869054016359));
#79016=CARTESIAN_POINT('Ctrl Pts',(4.31745813701234,139.678501142851,12.0028101469375));
#79017=CARTESIAN_POINT('Ctrl Pts',(4.32032485832862,139.723563824557,12.0277749297356));
#79018=CARTESIAN_POINT('Ctrl Pts',(4.32122900209576,139.73777596668,12.035963651045));
#79019=CARTESIAN_POINT('Ctrl Pts',(4.32283430509653,139.762999104231,12.051067034467));
#79020=CARTESIAN_POINT('Ctrl Pts',(4.32353857684145,139.774061119087,12.0578926839658));
#79021=CARTESIAN_POINT('Ctrl Pts',(4.3250383922315,139.797601019457,12.0728542473699));
#79022=CARTESIAN_POINT('Ctrl Pts',(4.3258321710095,139.810048647682,12.0810351543719));
#79023=CARTESIAN_POINT('Ctrl Pts',(4.32803501370844,139.844536163861,12.104462873564));
#79024=CARTESIAN_POINT('Ctrl Pts',(4.32942834291698,139.86628582693,12.1201274073436));
#79025=CARTESIAN_POINT('Ctrl Pts',(4.33536940140819,139.958424254276,12.1904094482468));
#79026=CARTESIAN_POINT('Ctrl Pts',(4.33969559168371,140.024177114373,12.2507950853459));
#79027=CARTESIAN_POINT('Ctrl Pts',(4.34796129116489,140.138448072097,12.3767833530805));
#79028=CARTESIAN_POINT('Ctrl Pts',(4.35189127976683,140.187784750827,12.4411881430152));
#79029=CARTESIAN_POINT('Ctrl Pts',(4.35692571791642,140.240055642322,12.5226050352027));
#79030=CARTESIAN_POINT('Ctrl Pts',(4.35775689949884,140.248359845524,12.5360113978862));
#79031=CARTESIAN_POINT('Ctrl Pts',(4.35906030018459,140.260844324583,12.5569135788284));
#79032=CARTESIAN_POINT('Ctrl Pts',(4.35952336097061,140.265178229208,12.56431672502));
#79033=CARTESIAN_POINT('Ctrl Pts',(4.36039521688847,140.273142837004,12.5782003462117));
#79034=CARTESIAN_POINT('Ctrl Pts',(4.36080300811647,140.27678965871,12.5846709972));
#79035=CARTESIAN_POINT('Ctrl Pts',(4.36179247004454,140.285453544043,12.6003208856314));
#79036=CARTESIAN_POINT('Ctrl Pts',(4.36237704847317,140.290421674015,12.6095265630458));
#79037=CARTESIAN_POINT('Ctrl Pts',(4.3645190165567,140.308103218136,12.6431469583352));
#79038=CARTESIAN_POINT('Ctrl Pts',(4.36610701042705,140.32022524925,12.6678646877221));
#79039=CARTESIAN_POINT('Ctrl Pts',(4.37044014009899,140.350925110714,12.7352041152564));
#79040=CARTESIAN_POINT('Ctrl Pts',(4.37322579466914,140.368180924087,12.7783932322061));
#79041=CARTESIAN_POINT('Ctrl Pts',(4.38293779713587,140.420846521304,12.9309142816477));
#79042=CARTESIAN_POINT('Ctrl Pts',(4.38985318374172,140.445432061495,13.0435565857797));
#79043=CARTESIAN_POINT('Ctrl Pts',(4.39760789358402,140.458756688159,13.1801649168837));
#79044=CARTESIAN_POINT('Ctrl Pts',(4.39885502942365,140.460416330658,13.20245133984));
#79045=CARTESIAN_POINT('Ctrl Pts',(4.40085807773653,140.462284942251,13.2387536449457));
#79046=CARTESIAN_POINT('Ctrl Pts',(4.40162348130133,140.462804073718,13.2527492918936));
#79047=CARTESIAN_POINT('Ctrl Pts',(4.40310012625846,140.463422956029,13.2799828698539));
#79048=CARTESIAN_POINT('Ctrl Pts',(4.40381196462155,140.463544145673,13.2932189071393));
#79049=CARTESIAN_POINT('Ctrl Pts',(4.40549293358754,140.463405210924,13.3247180023036));
#79050=CARTESIAN_POINT('Ctrl Pts',(4.40645694290561,140.462982807187,13.3429783231926));
#79051=CARTESIAN_POINT('Ctrl Pts',(4.40993133599375,140.460200443284,13.4094270583793));
#79052=CARTESIAN_POINT('Ctrl Pts',(4.41237929135753,140.455800031882,13.4575006173614));
#79053=CARTESIAN_POINT('Ctrl Pts',(4.41917243735557,140.436658022981,13.5926255284767));
#79054=CARTESIAN_POINT('Ctrl Pts',(4.42338589466456,140.416410351921,13.678678694971));
#79055=CARTESIAN_POINT('Ctrl Pts',(4.43045813602883,140.370896496535,13.8153564368705));
#79056=CARTESIAN_POINT('Ctrl Pts',(4.43324411987877,140.350241329141,13.8672712804011));
#79057=CARTESIAN_POINT('Ctrl Pts',(4.43685858259673,140.321175226722,13.9296807888178));
#79058=CARTESIAN_POINT('Ctrl Pts',(4.43755011055743,140.315519445971,13.9414128463607));
#79059=CARTESIAN_POINT('Ctrl Pts',(4.43867630317367,140.306177936797,13.9601469751066));
#79060=CARTESIAN_POINT('Ctrl Pts',(4.43910521712508,140.302590571982,13.967197592269));
#79061=CARTESIAN_POINT('Ctrl Pts',(4.43996203409697,140.295371713058,13.9811054109097));
#79062=CARTESIAN_POINT('Ctrl Pts',(4.44038980146203,140.291742511708,13.9879634670568));
#79063=CARTESIAN_POINT('Ctrl Pts',(4.44150442629145,140.282215954222,14.0056245314454));
#79064=CARTESIAN_POINT('Ctrl Pts',(4.4421961032529,140.276236629808,14.0163824235733));
#79065=CARTESIAN_POINT('Ctrl Pts',(4.44552117242477,140.247133961319,14.0672225057958));
#79066=CARTESIAN_POINT('Ctrl Pts',(4.44824247441362,140.22225538904,14.1062658160743));
#79067=CARTESIAN_POINT('Ctrl Pts',(4.45764078123967,140.131383440153,14.2349814341667));
#79068=CARTESIAN_POINT('Ctrl Pts',(4.46443966126184,140.05702367351,14.3182948759328));
#79069=CARTESIAN_POINT('Ctrl Pts',(4.4731259126145,139.945314792796,14.41789200921));
#79070=CARTESIAN_POINT('Ctrl Pts',(4.47531218732434,139.915700060866,14.4422768381431));
#79071=CARTESIAN_POINT('Ctrl Pts',(4.47841368021054,139.871451882207,14.4758827133057));
#79072=CARTESIAN_POINT('Ctrl Pts',(4.47936516660053,139.857561132568,14.4860512122345));
#79073=CARTESIAN_POINT('Ctrl Pts',(4.48102544600319,139.832769383045,14.5035363006908));
#79074=CARTESIAN_POINT('Ctrl Pts',(4.48173810907615,139.821943491134,14.5109555670904));
#79075=CARTESIAN_POINT('Ctrl Pts',(4.48321526204958,139.799125441095,14.5261463742231));
#79076=CARTESIAN_POINT('Ctrl Pts',(4.4839786578458,139.787116279016,14.5338899402026));
#79077=CARTESIAN_POINT('Ctrl Pts',(4.48599437570639,139.754845114647,14.5540356322645));
#79078=CARTESIAN_POINT('Ctrl Pts',(4.48723522260499,139.734390943077,14.5661226400624));
#79079=CARTESIAN_POINT('Ctrl Pts',(4.49223878229768,139.649683184851,14.6134353397257));
#79080=CARTESIAN_POINT('Ctrl Pts',(4.49585354788017,139.583119267484,14.6443116633613));
#79081=CARTESIAN_POINT('Ctrl Pts',(4.50349064738112,139.436430045322,14.6993994975616));
#79082=CARTESIAN_POINT('Ctrl Pts',(4.50748617562391,139.355982038661,14.7219933863773));
#79083=CARTESIAN_POINT('Ctrl Pts',(4.51315067967486,139.246042824063,14.7429512498732));
#79084=CARTESIAN_POINT('Ctrl Pts',(4.51461990057514,139.217883352072,14.7474709086357));
#79085=CARTESIAN_POINT('Ctrl Pts',(4.51670410694126,139.178832909682,14.7525733043793));
#79086=CARTESIAN_POINT('Ctrl Pts',(4.51728509833133,139.168039160471,14.7538614929084));
#79087=CARTESIAN_POINT('Ctrl Pts',(4.5182772899113,139.149787369549,14.7558338055957));
#79088=CARTESIAN_POINT('Ctrl Pts',(4.51868509143302,139.142336416472,14.7565811577237));
#79089=CARTESIAN_POINT('Ctrl Pts',(4.51955623090263,139.126535283995,14.7580436559551));
#79090=CARTESIAN_POINT('Ctrl Pts',(4.52002027989087,139.11818429914,14.7587443042348));
#79091=CARTESIAN_POINT('Ctrl Pts',(4.52133938144975,139.094614844516,14.7605180694513));
#79092=CARTESIAN_POINT('Ctrl Pts',(4.52220274678679,139.079385344195,14.7614249654902));
#79093=CARTESIAN_POINT('Ctrl Pts',(4.52421434770709,139.044273616558,14.7629653899106));
#79094=CARTESIAN_POINT('Ctrl Pts',(4.5253692183087,139.024387228937,14.7634319538735));
#79095=CARTESIAN_POINT('Ctrl Pts',(4.52948969943811,138.954143630889,14.763647862995));
#79096=CARTESIAN_POINT('Ctrl Pts',(4.53251549486401,138.903816500256,14.7612036772121));
#79097=CARTESIAN_POINT('Ctrl Pts',(4.54200948280427,138.746987118872,14.7454491140233));
#79098=CARTESIAN_POINT('Ctrl Pts',(4.54844624827276,138.641742350195,14.723023743515));
#79099=CARTESIAN_POINT('Ctrl Pts',(4.55584159818675,138.517736029587,14.681954450664));
#79100=CARTESIAN_POINT('Ctrl Pts',(4.55714595008593,138.495764719356,14.6740900664668));
#79101=CARTESIAN_POINT('Ctrl Pts',(4.55921660185348,138.460735912598,14.6605984794889));
#79102=CARTESIAN_POINT('Ctrl Pts',(4.55999362517918,138.447556612074,14.6553008158658));
#79103=CARTESIAN_POINT('Ctrl Pts',(4.56147779752238,138.422325593943,14.6447295316362));
#79104=CARTESIAN_POINT('Ctrl Pts',(4.56218579288799,138.410263810942,14.6394836600474));
#79105=CARTESIAN_POINT('Ctrl Pts',(4.56383494720659,138.382120329102,14.6267897321185));
#79106=CARTESIAN_POINT('Ctrl Pts',(4.56477153368218,138.366099789032,14.6192106881229));
#79107=CARTESIAN_POINT('Ctrl Pts',(4.56799853473739,138.310836042586,14.5918271010185));
#79108=CARTESIAN_POINT('Ctrl Pts',(4.57023827876785,138.27234903339,14.5705466274166));
#79109=CARTESIAN_POINT('Ctrl Pts',(4.57610858690483,138.172286305583,14.5091787369855));
#79110=CARTESIAN_POINT('Ctrl Pts',(4.5796525711301,138.112672446209,14.4661361168609));
#79111=CARTESIAN_POINT('Ctrl Pts',(4.58665240335781,138.002708581535,14.3734061090697));
#79112=CARTESIAN_POINT('Ctrl Pts',(4.59009890308002,137.95222787324,14.3241887643335));
#79113=CARTESIAN_POINT('Ctrl Pts',(4.59459720308539,137.894781716608,14.259471212818));
#79114=CARTESIAN_POINT('Ctrl Pts',(4.59544675541706,137.884273809671,14.247231486277));
#79115=CARTESIAN_POINT('Ctrl Pts',(4.59677296166917,137.868442384981,14.228161904938));
#79116=CARTESIAN_POINT('Ctrl Pts',(4.5972399490073,137.862973304891,14.2214539841473));
#79117=CARTESIAN_POINT('Ctrl Pts',(4.59811468002497,137.852932862765,14.2089137149107));
#79118=CARTESIAN_POINT('Ctrl Pts',(4.59852133145856,137.848345824272,14.203094573959));
#79119=CARTESIAN_POINT('Ctrl Pts',(4.59950178623109,137.837474772798,14.1890859907664));
#79120=CARTESIAN_POINT('Ctrl Pts',(4.6000783567779,137.831232940549,14.1808645474776));
#79121=CARTESIAN_POINT('Ctrl Pts',(4.60215482182166,137.809264712078,14.1512844557708));
#79122=CARTESIAN_POINT('Ctrl Pts',(4.60368303567754,137.794033341633,14.1295661522787));
#79123=CARTESIAN_POINT('Ctrl Pts',(4.60779563820658,137.755224738493,14.0709001319609));
#79124=CARTESIAN_POINT('Ctrl Pts',(4.61041625493469,137.732702791868,14.0332870496166));
#79125=CARTESIAN_POINT('Ctrl Pts',(4.61961011309098,137.660132224584,13.8987326932972));
#79126=CARTESIAN_POINT('Ctrl Pts',(4.6261989894649,137.619245512181,13.7972420806901));
#79127=CARTESIAN_POINT('Ctrl Pts',(4.63385416431974,137.583308717479,13.6680279026232));
#79128=CARTESIAN_POINT('Ctrl Pts',(4.63526437986805,137.577221561168,13.6437445978089));
#79129=CARTESIAN_POINT('Ctrl Pts',(4.63753889101354,137.568288659596,13.6037894219891));
#79130=CARTESIAN_POINT('Ctrl Pts',(4.63841472944284,137.565070658528,13.5882068498785));
#79131=CARTESIAN_POINT('Ctrl Pts',(4.63998979705221,137.559692067439,13.5598335493491));
#79132=CARTESIAN_POINT('Ctrl Pts',(4.64069166069231,137.557446232436,13.547060836032));
#79133=CARTESIAN_POINT('Ctrl Pts',(4.64204800344924,137.553404150259,13.5221341739343));
#79134=CARTESIAN_POINT('Ctrl Pts',(4.64270297354198,137.551590594976,13.5099841697536));
#79135=CARTESIAN_POINT('Ctrl Pts',(4.64415000269553,137.547896026201,13.4829010368947));
#79136=CARTESIAN_POINT('Ctrl Pts',(4.64493963952388,137.546091947451,13.4679587339457));
#79137=CARTESIAN_POINT('Ctrl Pts',(4.64838128406959,137.539176794057,13.4021713089129));
#79138=CARTESIAN_POINT('Ctrl Pts',(4.65095968919661,137.5365,13.3511048930752));
#79139=CARTESIAN_POINT('Ctrl Pts',(4.65349091708139,137.5365,13.3000000000138));
#79140=CARTESIAN_POINT('Origin',(4.2,139.,13.3));
#79141=CARTESIAN_POINT('',(5.22549387428705,137.5365,13.2999999999999));
#79142=CARTESIAN_POINT('',(5.15144231116594,137.5365,13.3));
#79143=CARTESIAN_POINT('',(4.2,137.5365,13.3));
#79144=CARTESIAN_POINT('Ctrl Pts',(5.22549387428705,137.5365,13.2999999999999));
#79145=CARTESIAN_POINT('Ctrl Pts',(5.22431648033678,137.5365,13.3208217959711));
#79146=CARTESIAN_POINT('Ctrl Pts',(5.22311897584145,137.536944360793,13.3416403099394));
#79147=CARTESIAN_POINT('Ctrl Pts',(5.21846390751971,137.540355485263,13.4215175314062));
#79148=CARTESIAN_POINT('Ctrl Pts',(5.21490846015814,137.546456176573,13.4803836302408));
#79149=CARTESIAN_POINT('Ctrl Pts',(5.20729369344285,137.567074131322,13.6050936794817));
#79150=CARTESIAN_POINT('Ctrl Pts',(5.2032430825151,137.582612999915,13.6706397550122));
#79151=CARTESIAN_POINT('Ctrl Pts',(5.19644604084043,137.617049107716,13.7812909378183));
#79152=CARTESIAN_POINT('Ctrl Pts',(5.19365270477895,137.633794068136,13.8269499321652));
#79153=CARTESIAN_POINT('Ctrl Pts',(5.18990422377233,137.65995846791,13.8886072377813));
#79154=CARTESIAN_POINT('Ctrl Pts',(5.18888660424214,137.667453348639,13.9053835589099));
#79155=CARTESIAN_POINT('Ctrl Pts',(5.18714983477347,137.680922800274,13.934070154979));
#79156=CARTESIAN_POINT('Ctrl Pts',(5.18642567596165,137.686747635177,13.9460478797736));
#79157=CARTESIAN_POINT('Ctrl Pts',(5.18494652791685,137.699073575902,13.9705381857021));
#79158=CARTESIAN_POINT('Ctrl Pts',(5.18419229718666,137.705593645546,13.9830396971194));
#79159=CARTESIAN_POINT('Ctrl Pts',(5.18224925247977,137.722995725423,14.0152618858895));
#79160=CARTESIAN_POINT('Ctrl Pts',(5.18107029499875,137.734154297162,14.0348293751879));
#79161=CARTESIAN_POINT('Ctrl Pts',(5.17401263216525,137.804489654537,14.1518080432635));
#79162=CARTESIAN_POINT('Ctrl Pts',(5.16855169606009,137.874425432198,14.2422873462168));
#79163=CARTESIAN_POINT('Ctrl Pts',(5.16070838078417,137.986934110349,14.3572253827301));
#79164=CARTESIAN_POINT('Ctrl Pts',(5.15840574566655,138.021300340968,14.3891164018531));
#79165=CARTESIAN_POINT('Ctrl Pts',(5.15462439430924,138.078315182926,14.4371439100982));
#79166=CARTESIAN_POINT('Ctrl Pts',(5.15319443863056,138.099996351133,14.4543796710292));
#79167=CARTESIAN_POINT('Ctrl Pts',(5.15116894004427,138.130570668894,14.4773001284452));
#79168=CARTESIAN_POINT('Ctrl Pts',(5.150605815392,138.139056882537,14.4835201264684));
#79169=CARTESIAN_POINT('Ctrl Pts',(5.14963220817474,138.153684740911,14.4940010866857));
#79170=CARTESIAN_POINT('Ctrl Pts',(5.1492247491626,138.159793199931,14.4983074081484));
#79171=CARTESIAN_POINT('Ctrl Pts',(5.14833893985886,138.173038248708,14.5074937873587));
#79172=CARTESIAN_POINT('Ctrl Pts',(5.14785963888882,138.180185164641,14.5123574607467));
#79173=CARTESIAN_POINT('Ctrl Pts',(5.14648600893945,138.200626294917,14.5260048184096));
#79174=CARTESIAN_POINT('Ctrl Pts',(5.14558260813531,138.21402109619,14.5346348674491));
#79175=CARTESIAN_POINT('Ctrl Pts',(5.13996987247755,138.297137283842,14.5862845249898));
#79176=CARTESIAN_POINT('Ctrl Pts',(5.13501289323092,138.370224414343,14.6236030014981));
#79177=CARTESIAN_POINT('Ctrl Pts',(5.12611934787148,138.50691583713,14.6795018385329));
#79178=CARTESIAN_POINT('Ctrl Pts',(5.12218275058585,138.56940059672,14.7002652097761));
#79179=CARTESIAN_POINT('Ctrl Pts',(5.11594971739297,138.673096359438,14.7271213988878));
#79180=CARTESIAN_POINT('Ctrl Pts',(5.11358877472775,138.713542318993,14.7357868719834));
#79181=CARTESIAN_POINT('Ctrl Pts',(5.11030835350008,138.771480765783,14.7456537658146));
#79182=CARTESIAN_POINT('Ctrl Pts',(5.10934538263123,138.788708976814,14.7482720709701));
#79183=CARTESIAN_POINT('Ctrl Pts',(5.10767104980481,138.819042813287,14.752329310508));
#79184=CARTESIAN_POINT('Ctrl Pts',(5.10695563241221,138.832128530929,14.7538999674374));
#79185=CARTESIAN_POINT('Ctrl Pts',(5.10546602418558,138.859627448787,14.7568243928691));
#79186=CARTESIAN_POINT('Ctrl Pts',(5.10469305388997,138.874043158052,14.7581415086025));
#79187=CARTESIAN_POINT('Ctrl Pts',(5.10263489763599,138.912797624306,14.7611033408969));
#79188=CARTESIAN_POINT('Ctrl Pts',(5.10136198308602,138.937162345626,14.7623538373338));
#79189=CARTESIAN_POINT('Ctrl Pts',(5.0953846989902,139.053174861332,14.765403010299));
#79190=CARTESIAN_POINT('Ctrl Pts',(5.09092659283357,139.144830604221,14.7591981909216));
#79191=CARTESIAN_POINT('Ctrl Pts',(5.083557811952,139.294499947794,14.7348166941196));
#79192=CARTESIAN_POINT('Ctrl Pts',(5.0806472093606,139.353042359927,14.7215447744809));
#79193=CARTESIAN_POINT('Ctrl Pts',(5.07601317639603,139.441351221602,14.6957319367232));
#79194=CARTESIAN_POINT('Ctrl Pts',(5.07436908577361,139.471794943004,14.6857372784024));
#79195=CARTESIAN_POINT('Ctrl Pts',(5.07208987477992,139.512278453656,14.6709578686598));
#79196=CARTESIAN_POINT('Ctrl Pts',(5.07149878865746,139.522629098198,14.6670455378476));
#79197=CARTESIAN_POINT('Ctrl Pts',(5.07049276547103,139.539971451507,14.6602647454083));
#79198=CARTESIAN_POINT('Ctrl Pts',(5.07008140083164,139.546987307034,14.6574587400175));
#79199=CARTESIAN_POINT('Ctrl Pts',(5.06920633791023,139.561744841373,14.6514234491596));
#79200=CARTESIAN_POINT('Ctrl Pts',(5.06874197743711,139.569480888435,14.6481817816459));
#79201=CARTESIAN_POINT('Ctrl Pts',(5.06742929754634,139.59109969396,14.6389034954454));
#79202=CARTESIAN_POINT('Ctrl Pts',(5.06657284404308,139.604916925543,14.6327178602115));
#79203=CARTESIAN_POINT('Ctrl Pts',(5.06042488099548,139.702294296705,14.5872981288399));
#79204=CARTESIAN_POINT('Ctrl Pts',(5.05481085427807,139.782068756456,14.5404516704972));
#79205=CARTESIAN_POINT('Ctrl Pts',(5.04450560618098,139.921001405237,14.4401062183733));
#79206=CARTESIAN_POINT('Ctrl Pts',(5.03981278437006,139.981256226024,14.3886802167703));
#79207=CARTESIAN_POINT('Ctrl Pts',(5.03377431621596,140.056020141462,14.3135952660986));
#79208=CARTESIAN_POINT('Ctrl Pts',(5.03226481078145,140.074447906305,14.2940401062208));
#79209=CARTESIAN_POINT('Ctrl Pts',(5.02994978801104,140.102287472923,14.262818018029));
#79210=CARTESIAN_POINT('Ctrl Pts',(5.02912873020647,140.112075474131,14.2514958602498));
#79211=CARTESIAN_POINT('Ctrl Pts',(5.02760325243495,140.130091922281,14.2299976718177));
#79212=CARTESIAN_POINT('Ctrl Pts',(5.0268972212633,140.138360825223,14.21985763538));
#79213=CARTESIAN_POINT('Ctrl Pts',(5.02531051656691,140.156776801803,14.1966456706902));
#79214=CARTESIAN_POINT('Ctrl Pts',(5.02443319537824,140.16684046828,14.1835096939502));
#79215=CARTESIAN_POINT('Ctrl Pts',(5.02169319657924,140.197860823561,14.1415644114764));
#79216=CARTESIAN_POINT('Ctrl Pts',(5.01986179067266,140.217990296151,14.1121582994356));
#79217=CARTESIAN_POINT('Ctrl Pts',(5.01249800742321,140.295840750304,13.9890156029986));
#79218=CARTESIAN_POINT('Ctrl Pts',(5.00728157368047,140.343969674476,13.8896531849894));
#79219=CARTESIAN_POINT('Ctrl Pts',(4.99930229820903,140.397759585905,13.7368085105194));
#79220=CARTESIAN_POINT('Ctrl Pts',(4.99669734801785,140.412387922633,13.6869017447962));
#79221=CARTESIAN_POINT('Ctrl Pts',(4.99329824343388,140.427249520676,13.6239636512686));
#79222=CARTESIAN_POINT('Ctrl Pts',(4.99262305764535,140.430007821726,13.6115625934559));
#79223=CARTESIAN_POINT('Ctrl Pts',(4.99151530026912,140.434213669998,13.5914196324865));
#79224=CARTESIAN_POINT('Ctrl Pts',(4.9910880874694,140.435760826695,13.5836989535385));
#79225=CARTESIAN_POINT('Ctrl Pts',(4.99027754234871,140.438554228036,13.5691507892851));
#79226=CARTESIAN_POINT('Ctrl Pts',(4.98989502755304,140.439814362344,13.5623261562576));
#79227=CARTESIAN_POINT('Ctrl Pts',(4.98885191915191,140.443096014263,13.5438170543221));
#79228=CARTESIAN_POINT('Ctrl Pts',(4.98818641009163,140.445024096006,13.532116793384));
#79229=CARTESIAN_POINT('Ctrl Pts',(4.98543512099859,140.452335038783,13.4841231767654));
#79230=CARTESIAN_POINT('Ctrl Pts',(4.98329502740733,140.456494015416,13.4476590858289));
#79231=CARTESIAN_POINT('Ctrl Pts',(4.97490769957814,140.467245002696,13.3064215570208));
#79232=CARTESIAN_POINT('Ctrl Pts',(4.96847894171036,140.463930188275,13.2012076657758));
#79233=CARTESIAN_POINT('Ctrl Pts',(4.95924429192299,140.442188488971,13.0457861633595));
#79234=CARTESIAN_POINT('Ctrl Pts',(4.956249362654,140.432253592853,12.994741330572));
#79235=CARTESIAN_POINT('Ctrl Pts',(4.95228722505338,140.415065497773,12.9261369225789));
#79236=CARTESIAN_POINT('Ctrl Pts',(4.95124758902434,140.410158350388,12.9080338833798));
#79237=CARTESIAN_POINT('Ctrl Pts',(4.94948533529721,140.401155994288,12.8771842211054));
#79238=CARTESIAN_POINT('Ctrl Pts',(4.94875731558008,140.397231474106,12.86439062496));
#79239=CARTESIAN_POINT('Ctrl Pts',(4.9472804193623,140.388849607488,12.838346000716));
#79240=CARTESIAN_POINT('Ctrl Pts',(4.94653213955791,140.384376747959,12.825101394582));
#79241=CARTESIAN_POINT('Ctrl Pts',(4.9446259938738,140.372403904487,12.7912561322809));
#79242=CARTESIAN_POINT('Ctrl Pts',(4.94347725197428,140.364629455367,12.7707559016435));
#79243=CARTESIAN_POINT('Ctrl Pts',(4.9362252062303,140.312031472422,12.6409367650834));
#79244=CARTESIAN_POINT('Ctrl Pts',(4.93057914401306,140.25457188878,12.5372144466056));
#79245=CARTESIAN_POINT('Ctrl Pts',(4.9226197969618,140.158942398364,12.405182519189));
#79246=CARTESIAN_POINT('Ctrl Pts',(4.92040989973246,140.130964277353,12.3700724757106));
#79247=CARTESIAN_POINT('Ctrl Pts',(4.91676206613021,140.083670618105,12.3160199488406));
#79248=CARTESIAN_POINT('Ctrl Pts',(4.91536877810655,140.06536600081,12.2962301732213));
#79249=CARTESIAN_POINT('Ctrl Pts',(4.91338697196033,140.039242414412,12.269506896768));
#79250=CARTESIAN_POINT('Ctrl Pts',(4.91282906174203,140.031879099899,12.2621337551059));
#79251=CARTESIAN_POINT('Ctrl Pts',(4.9118613739175,140.019109618759,12.249617449956));
#79252=CARTESIAN_POINT('Ctrl Pts',(4.91145451540155,140.013741810766,12.2444359536495));
#79253=CARTESIAN_POINT('Ctrl Pts',(4.91056612817975,140.002028284513,12.2333007591275));
#79254=CARTESIAN_POINT('Ctrl Pts',(4.91008358473448,139.995669031698,12.2273625379867));
#79255=CARTESIAN_POINT('Ctrl Pts',(4.90869158810821,139.977320149219,12.2105322584695));
#79256=CARTESIAN_POINT('Ctrl Pts',(4.90777270424951,139.96520245095,12.1997823766872));
#79257=CARTESIAN_POINT('Ctrl Pts',(4.90313870872369,139.903921509832,12.147210275159));
#79258=CARTESIAN_POINT('Ctrl Pts',(4.8992720420793,139.852210516469,12.1084739714692));
#79259=CARTESIAN_POINT('Ctrl Pts',(4.89183240199377,139.7486353442,12.0410869216755));
#79260=CARTESIAN_POINT('Ctrl Pts',(4.88826911363359,139.697249759838,12.0119160375971));
#79261=CARTESIAN_POINT('Ctrl Pts',(4.88122387674749,139.590465039665,11.959563403886));
#79262=CARTESIAN_POINT('Ctrl Pts',(4.87775068112213,139.535116749234,11.9365225949072));
#79263=CARTESIAN_POINT('Ctrl Pts',(4.87329227671756,139.460055272962,11.9105531330193));
#79264=CARTESIAN_POINT('Ctrl Pts',(4.87220820256922,139.441477533651,11.9045391121224));
#79265=CARTESIAN_POINT('Ctrl Pts',(4.8703941252912,139.409843985337,11.8949936448065));
#79266=CARTESIAN_POINT('Ctrl Pts',(4.86965790811844,139.396849851136,11.8912682429645));
#79267=CARTESIAN_POINT('Ctrl Pts',(4.86818303625158,139.370510858223,11.8841102586444));
#79268=CARTESIAN_POINT('Ctrl Pts',(4.86744468255715,139.357165410997,11.8806850445975));
#79269=CARTESIAN_POINT('Ctrl Pts',(4.86560110869692,139.323457670658,11.8725392434399));
#79270=CARTESIAN_POINT('Ctrl Pts',(4.86450381242269,139.303038620099,11.8680653895067));
#79271=CARTESIAN_POINT('Ctrl Pts',(4.85930034877243,139.204657337507,11.8487086668416));
#79272=CARTESIAN_POINT('Ctrl Pts',(4.85538129394282,139.125662589388,11.8397459995933));
#79273=CARTESIAN_POINT('Ctrl Pts',(4.84856790425203,138.985923751041,11.8353204378668));
#79274=CARTESIAN_POINT('Ctrl Pts',(4.84565586842749,138.925462449639,11.8371506670341));
#79275=CARTESIAN_POINT('Ctrl Pts',(4.84030771838227,138.817711515504,11.8471111082985));
#79276=CARTESIAN_POINT('Ctrl Pts',(4.83790196758462,138.770381561137,11.8538361629626));
#79277=CARTESIAN_POINT('Ctrl Pts',(4.83473357131472,138.711239614577,11.8652161144749));
#79278=CARTESIAN_POINT('Ctrl Pts',(4.83407118444928,138.699040651448,11.8677253027943));
#79279=CARTESIAN_POINT('Ctrl Pts',(4.83297916583313,138.67923506587,11.8720632767878));
#79280=CARTESIAN_POINT('Ctrl Pts',(4.83255460970626,138.671608205385,11.873797962008));
#79281=CARTESIAN_POINT('Ctrl Pts',(4.83174446885236,138.657203079681,11.8771959975687));
#79282=CARTESIAN_POINT('Ctrl Pts',(4.83135963611221,138.650422095979,11.8788468616057));
#79283=CARTESIAN_POINT('Ctrl Pts',(4.83030185495524,138.631941871041,11.8834862280648));
#79284=CARTESIAN_POINT('Ctrl Pts',(4.829623758664,138.620267637226,11.886571061028));
#79285=CARTESIAN_POINT('Ctrl Pts',(4.82671483766814,138.570844130305,11.900287351417));
#79286=CARTESIAN_POINT('Ctrl Pts',(4.8244217778305,138.533494433918,11.9122888055571));
#79287=CARTESIAN_POINT('Ctrl Pts',(4.81600791076604,138.400372776943,11.9610460801033));
#79288=CARTESIAN_POINT('Ctrl Pts',(4.8097337224059,138.308042899344,12.0063431193744));
#79289=CARTESIAN_POINT('Ctrl Pts',(4.80067139355871,138.177597192873,12.0883323779925));
#79290=CARTESIAN_POINT('Ctrl Pts',(4.79770403475069,138.135466159805,12.1180241468914));
#79291=CARTESIAN_POINT('Ctrl Pts',(4.79377095516974,138.080285980148,12.1614446838187));
#79292=CARTESIAN_POINT('Ctrl Pts',(4.79273420937021,138.065809758149,12.173292085729));
#79293=CARTESIAN_POINT('Ctrl Pts',(4.7909753099417,138.041379689634,12.1940803928994));
#79294=CARTESIAN_POINT('Ctrl Pts',(4.79024780622353,138.031314284487,12.202886023247));
#79295=CARTESIAN_POINT('Ctrl Pts',(4.7887706684013,138.010966116866,12.2211858167205));
#79296=CARTESIAN_POINT('Ctrl Pts',(4.78802165158011,138.000695997261,12.2306920029107));
#79297=CARTESIAN_POINT('Ctrl Pts',(4.78611091541732,137.97463706906,12.2555159442617));
#79298=CARTESIAN_POINT('Ctrl Pts',(4.78495841017063,137.959054154115,12.2710452412685));
#79299=CARTESIAN_POINT('Ctrl Pts',(4.7777299298348,137.862392491039,12.3718186444322));
#79300=CARTESIAN_POINT('Ctrl Pts',(4.77210627988811,137.791493457466,12.4662224993563));
#79301=CARTESIAN_POINT('Ctrl Pts',(4.76416132558251,137.710099106485,12.6071632660803));
#79302=CARTESIAN_POINT('Ctrl Pts',(4.76194039249237,137.68935927512,12.647246194033));
#79303=CARTESIAN_POINT('Ctrl Pts',(4.75827661865235,137.65920000554,12.7127871428391));
#79304=CARTESIAN_POINT('Ctrl Pts',(4.75687890750066,137.648579165048,12.737661026311));
#79305=CARTESIAN_POINT('Ctrl Pts',(4.7548918269284,137.634824729027,12.7725177075315));
#79306=CARTESIAN_POINT('Ctrl Pts',(4.75433328109003,137.631099363174,12.7822624958746));
#79307=CARTESIAN_POINT('Ctrl Pts',(4.75336487447504,137.624888491528,12.799044633777));
#79308=CARTESIAN_POINT('Ctrl Pts',(4.7529579455227,137.622352099886,12.8060625531796));
#79309=CARTESIAN_POINT('Ctrl Pts',(4.75206988458404,137.616976987586,12.8212984444337));
#79310=CARTESIAN_POINT('Ctrl Pts',(4.75158774581658,137.61415778368,12.8295223960637));
#79311=CARTESIAN_POINT('Ctrl Pts',(4.75019804766149,137.606306518591,12.8531084672919));
#79312=CARTESIAN_POINT('Ctrl Pts',(4.74928110284224,137.601455625317,12.8685290850124));
#79313=CARTESIAN_POINT('Ctrl Pts',(4.74468326752112,137.578683589876,12.9453423946502));
#79314=CARTESIAN_POINT('Ctrl Pts',(4.74085350185027,137.564545861888,13.0077799023517));
#79315=CARTESIAN_POINT('Ctrl Pts',(4.73240862021616,137.542590011186,13.1463281796392));
#79316=CARTESIAN_POINT('Ctrl Pts',(4.72780130089799,137.536558490182,13.2225444839638));
#79317=CARTESIAN_POINT('Ctrl Pts',(4.72331126934335,137.53650014106,13.2992578962685));
#79318=CARTESIAN_POINT('Ctrl Pts',(4.7232895549327,137.5365,13.2996289488461));
#79319=CARTESIAN_POINT('Ctrl Pts',(4.72326784382709,137.5365,13.299999999986));
#79320=CARTESIAN_POINT('',(4.65354584395168,137.536500526148,13.298887278614));
#79321=CARTESIAN_POINT('Ctrl Pts',(4.65349091708139,137.5365,13.3000000000138));
#79322=CARTESIAN_POINT('Ctrl Pts',(4.65350929441382,137.5365,13.2996289660132));
#79323=CARTESIAN_POINT('Ctrl Pts',(4.65352766935275,137.5365001411,13.2992579299891));
#79324=CARTESIAN_POINT('Ctrl Pts',(4.65354604191487,137.536500423304,13.2988868920213));
#79325=CARTESIAN_POINT('Ctrl Pts',(4.65354602233856,137.536500423003,13.2988872873692));
#79326=CARTESIAN_POINT('Ctrl Pts',(4.6577293092493,137.536564655774,13.2144048882518));
#79327=CARTESIAN_POINT('Ctrl Pts',(4.66176523213553,137.543943858772,13.1300884198745));
#79328=CARTESIAN_POINT('Ctrl Pts',(4.66770202050596,137.564816053257,13.0112274796867));
#79329=CARTESIAN_POINT('Ctrl Pts',(4.66950433321345,137.572396927557,12.975821440743));
#79330=CARTESIAN_POINT('Ctrl Pts',(4.67255190081265,137.587027913655,12.9180445111731));
#79331=CARTESIAN_POINT('Ctrl Pts',(4.67376859434626,137.593317034569,12.8954965619373));
#79332=CARTESIAN_POINT('Ctrl Pts',(4.67553689863044,137.603019658087,12.8636797256772));
#79333=CARTESIAN_POINT('Ctrl Pts',(4.67606586182223,137.605990696879,12.8542786638995));
#79334=CARTESIAN_POINT('Ctrl Pts',(4.67699931657034,137.611345985791,12.8379107324697));
#79335=CARTESIAN_POINT('Ctrl Pts',(4.67740143162642,137.613688184537,12.8309306983713));
#79336=CARTESIAN_POINT('Ctrl Pts',(4.6782996574533,137.618996209603,12.8154992325445));
#79337=CARTESIAN_POINT('Ctrl Pts',(4.67879711645867,137.621986977745,12.8070572398695));
#79338=CARTESIAN_POINT('Ctrl Pts',(4.68031617372947,137.631279886708,12.7815719056368));
#79339=CARTESIAN_POINT('Ctrl Pts',(4.6813502497828,137.637821941617,12.7646185338567));
#79340=CARTESIAN_POINT('Ctrl Pts',(4.6884303602977,137.684183619342,12.6508298199644));
#79341=CARTESIAN_POINT('Ctrl Pts',(4.69484769726215,137.733979064281,12.5583903501883));
#79342=CARTESIAN_POINT('Ctrl Pts',(4.70406066107294,137.821184918616,12.4312810680816));
#79343=CARTESIAN_POINT('Ctrl Pts',(4.70697924740942,137.851210623,12.3919464916551));
#79344=CARTESIAN_POINT('Ctrl Pts',(4.71182447440425,137.905498477526,12.3278414899117));
#79345=CARTESIAN_POINT('Ctrl Pts',(4.71378379700898,137.928752374379,12.3022753113496));
#79346=CARTESIAN_POINT('Ctrl Pts',(4.71661303131404,137.964283281533,12.2658873165816));
#79347=CARTESIAN_POINT('Ctrl Pts',(4.71751175655903,137.97587024234,12.2544109637432));
#79348=CARTESIAN_POINT('Ctrl Pts',(4.71910470302774,137.996942031261,12.2342267436489));
#79349=CARTESIAN_POINT('Ctrl Pts',(4.71980204478394,138.00635438291,12.225445987874));
#79350=CARTESIAN_POINT('Ctrl Pts',(4.72129605731582,138.02692023061,12.2067614887341));
#79351=CARTESIAN_POINT('Ctrl Pts',(4.72209084117459,138.038111812014,12.1969017196732));
#79352=CARTESIAN_POINT('Ctrl Pts',(4.72426087409004,138.069343435545,12.1702234934595));
#79353=CARTESIAN_POINT('Ctrl Pts',(4.72562148158929,138.089687127381,12.1537682704418));
#79354=CARTESIAN_POINT('Ctrl Pts',(4.73274708444683,138.199989058206,12.0693392616625));
#79355=CARTESIAN_POINT('Ctrl Pts',(4.73812522945409,138.297131622474,12.0113882208182));
#79356=CARTESIAN_POINT('Ctrl Pts',(4.74573324193404,138.439060493645,11.9475887371679));
#79357=CARTESIAN_POINT('Ctrl Pts',(4.74784913313509,138.478905060962,11.9317423323137));
#79358=CARTESIAN_POINT('Ctrl Pts',(4.75135928007426,138.544086838964,11.9090796684693));
#79359=CARTESIAN_POINT('Ctrl Pts',(4.75271281234012,138.569012832597,11.9011554464974));
#79360=CARTESIAN_POINT('Ctrl Pts',(4.75464518845147,138.604003338899,11.8910555845466));
#79361=CARTESIAN_POINT('Ctrl Pts',(4.75519528672644,138.613899867883,11.8883115084047));
#79362=CARTESIAN_POINT('Ctrl Pts',(4.75615200229201,138.630978920424,11.8837689084596));
#79363=CARTESIAN_POINT('Ctrl Pts',(4.75655582279702,138.638147564674,11.8819203565725));
#79364=CARTESIAN_POINT('Ctrl Pts',(4.75744035672023,138.653756774579,11.878021337886));
#79365=CARTESIAN_POINT('Ctrl Pts',(4.75792211920961,138.662201649147,11.8759915895538));
#79366=CARTESIAN_POINT('Ctrl Pts',(4.75931779363978,138.68652271521,11.8703744684641));
#79367=CARTESIAN_POINT('Ctrl Pts',(4.76024126965751,138.702440909593,11.8669767232499));
#79368=CARTESIAN_POINT('Ctrl Pts',(4.7654736357832,138.791886269775,11.8494390852533));
#79369=CARTESIAN_POINT('Ctrl Pts',(4.76998707633885,138.86635306689,11.8406935610312));
#79370=CARTESIAN_POINT('Ctrl Pts',(4.78067379438162,139.043590360665,11.8335614827661));
#79371=CARTESIAN_POINT('Ctrl Pts',(4.78679874052828,139.146189003452,11.8402134983184));
#79372=CARTESIAN_POINT('Ctrl Pts',(4.79385500135757,139.269286943371,11.8613144146805));
#79373=CARTESIAN_POINT('Ctrl Pts',(4.79510233003266,139.291224833312,11.8655942535914));
#79374=CARTESIAN_POINT('Ctrl Pts',(4.7971056062786,139.326737720072,11.873370808738));
#79375=CARTESIAN_POINT('Ctrl Pts',(4.79787104900426,139.340375059701,11.8765628833789));
#79376=CARTESIAN_POINT('Ctrl Pts',(4.79934771716192,139.366807249459,11.883151431197));
#79377=CARTESIAN_POINT('Ctrl Pts',(4.80005954043639,139.379605936125,11.8865266984298));
#79378=CARTESIAN_POINT('Ctrl Pts',(4.8017403908532,139.409949977277,11.8949709135095));
#79379=CARTESIAN_POINT('Ctrl Pts',(4.80270429876016,139.427449893669,11.9001956045442));
#79380=CARTESIAN_POINT('Ctrl Pts',(4.80599205970899,139.487406210783,11.9193251593732));
#79381=CARTESIAN_POINT('Ctrl Pts',(4.80826406382799,139.529322388639,11.9348457612707));
#79382=CARTESIAN_POINT('Ctrl Pts',(4.8158739985949,139.669699711035,11.994264093138));
#79383=CARTESIAN_POINT('Ctrl Pts',(4.82096425383808,139.763985276689,12.0470958002338));
#79384=CARTESIAN_POINT('Ctrl Pts',(4.82840832789733,139.885746281297,12.134218201754));
#79385=CARTESIAN_POINT('Ctrl Pts',(4.83053567654524,139.918809352761,12.1600953947755));
#79386=CARTESIAN_POINT('Ctrl Pts',(4.83337846541901,139.959826218681,12.1951427279094));
#79387=CARTESIAN_POINT('Ctrl Pts',(4.83401688123966,139.968843916272,12.2030417468687));
#79388=CARTESIAN_POINT('Ctrl Pts',(4.83507781751693,139.983487947561,12.216190560888));
#79389=CARTESIAN_POINT('Ctrl Pts',(4.83549575378303,139.989171925473,12.2213757177941));
#79390=CARTESIAN_POINT('Ctrl Pts',(4.83635494859805,140.000677108576,12.2320386418503));
#79391=CARTESIAN_POINT('Ctrl Pts',(4.83679642533085,140.006494775698,12.2375196950466));
#79392=CARTESIAN_POINT('Ctrl Pts',(4.8379875998989,140.021951854619,12.2523232930375));
#79393=CARTESIAN_POINT('Ctrl Pts',(4.83874333923753,140.031508312428,12.2617309352858));
#79394=CARTESIAN_POINT('Ctrl Pts',(4.84367714058061,140.092403765029,12.3233486817743));
#79395=CARTESIAN_POINT('Ctrl Pts',(4.84807196708989,140.139888540211,12.3792143788359));
#79396=CARTESIAN_POINT('Ctrl Pts',(4.85700107141657,140.227165073143,12.4990453624152));
#79397=CARTESIAN_POINT('Ctrl Pts',(4.8615213544411,140.266613495803,12.5630100150866));
#79398=CARTESIAN_POINT('Ctrl Pts',(4.86850072466635,140.321352486862,12.669256205408));
#79399=CARTESIAN_POINT('Ctrl Pts',(4.87104763310839,140.339909781994,12.7097013625851));
#79400=CARTESIAN_POINT('Ctrl Pts',(4.87452737305845,140.363271775711,12.7674224993983));
#79401=CARTESIAN_POINT('Ctrl Pts',(4.8755115517479,140.36964503468,12.7840336765302));
#79402=CARTESIAN_POINT('Ctrl Pts',(4.87720637966401,140.380204129535,12.8131303461209));
#79403=CARTESIAN_POINT('Ctrl Pts',(4.87792150524246,140.384527186493,12.8255635082221));
#79404=CARTESIAN_POINT('Ctrl Pts',(4.87939537261687,140.393156505919,12.8515045709968));
#79405=CARTESIAN_POINT('Ctrl Pts',(4.88015315563447,140.397435419971,12.8650201544894));
#79406=CARTESIAN_POINT('Ctrl Pts',(4.88213449702556,140.40819654698,12.900809825447));
#79407=CARTESIAN_POINT('Ctrl Pts',(4.88334730157221,140.414346852789,12.9231799263664));
#79408=CARTESIAN_POINT('Ctrl Pts',(4.89014334604605,140.446214748924,13.0508955733023));
#79409=CARTESIAN_POINT('Ctrl Pts',(4.89535738076678,140.460693104425,13.1586935896334));
#79410=CARTESIAN_POINT('Ctrl Pts',(4.90306074918849,140.464248291956,13.3168378993344));
#79411=CARTESIAN_POINT('Ctrl Pts',(4.90549779740134,140.462830072721,13.3665901598664));
#79412=CARTESIAN_POINT('Ctrl Pts',(4.90946957942771,140.456604106806,13.4447763686312));
#79413=CARTESIAN_POINT('Ctrl Pts',(4.91094920990118,140.453485521771,13.4733071243042));
#79414=CARTESIAN_POINT('Ctrl Pts',(4.91303174597363,140.448067297232,13.5122405489863));
#79415=CARTESIAN_POINT('Ctrl Pts',(4.91359965026627,140.446489698711,13.5227386050876));
#79416=CARTESIAN_POINT('Ctrl Pts',(4.91457663704094,140.443610973675,13.5405724422096));
#79417=CARTESIAN_POINT('Ctrl Pts',(4.91498258233514,140.442367761664,13.5479172889239));
#79418=CARTESIAN_POINT('Ctrl Pts',(4.91585860534388,140.439586224405,13.5636209047145));
#79419=CARTESIAN_POINT('Ctrl Pts',(4.91632953283807,140.438031106115,13.5719761191759));
#79420=CARTESIAN_POINT('Ctrl Pts',(4.91766406165464,140.433454369699,13.5954282721577));
#79421=CARTESIAN_POINT('Ctrl Pts',(4.91853604874715,140.430267235034,13.6104913721952));
#79422=CARTESIAN_POINT('Ctrl Pts',(4.92432476240232,140.407791051954,13.7090164531306));
#79423=CARTESIAN_POINT('Ctrl Pts',(4.92951661196094,140.381444500495,13.7906927793563));
#79424=CARTESIAN_POINT('Ctrl Pts',(4.93852291305073,140.323217398582,13.9285049773874));
#79425=CARTESIAN_POINT('Ctrl Pts',(4.94234584116324,140.294488520076,13.9857283621063));
#79426=CARTESIAN_POINT('Ctrl Pts',(4.94842690466793,140.241535982016,14.075932747213));
#79427=CARTESIAN_POINT('Ctrl Pts',(4.95074559909251,140.219514517456,14.1101037028003));
#79428=CARTESIAN_POINT('Ctrl Pts',(4.95397595522907,140.186153025661,14.1574211898993));
#79429=CARTESIAN_POINT('Ctrl Pts',(4.95492950487781,140.175959261039,14.1713494990618));
#79430=CARTESIAN_POINT('Ctrl Pts',(4.95658955039651,140.157605403645,14.1955184499758));
#79431=CARTESIAN_POINT('Ctrl Pts',(4.95729999584974,140.149549959481,14.2058357858829));
#79432=CARTESIAN_POINT('Ctrl Pts',(4.9587809694609,140.132339777438,14.2272790394083));
#79433=CARTESIAN_POINT('Ctrl Pts',(4.95955026609241,140.123156946185,14.238380670513));
#79434=CARTESIAN_POINT('Ctrl Pts',(4.961602110347,140.098022015188,14.267870022555));
#79435=CARTESIAN_POINT('Ctrl Pts',(4.9628724049213,140.081772335783,14.2859986960734));
#79436=CARTESIAN_POINT('Ctrl Pts',(4.96880755549505,140.002746320679,14.3698560435872));
#79437=CARTESIAN_POINT('Ctrl Pts',(4.97323077851787,139.934386113374,14.430051520221));
#79438=CARTESIAN_POINT('Ctrl Pts',(4.98059408309831,139.811844899949,14.519187012722));
#79439=CARTESIAN_POINT('Ctrl Pts',(4.98353536043907,139.760641217656,14.5517720739616));
#79440=CARTESIAN_POINT('Ctrl Pts',(4.98821003081118,139.679381464709,14.5966533321517));
#79441=CARTESIAN_POINT('Ctrl Pts',(4.98986222412942,139.650691353748,14.6112854493932));
#79442=CARTESIAN_POINT('Ctrl Pts',(4.99214888547682,139.611545870546,14.6296487733508));
#79443=CARTESIAN_POINT('Ctrl Pts',(4.99273878963075,139.601495193339,14.6342255168632));
#79444=CARTESIAN_POINT('Ctrl Pts',(4.99374145690061,139.584518091223,14.6417255143741));
#79445=CARTESIAN_POINT('Ctrl Pts',(4.99415064172394,139.577618995616,14.6447100243752));
#79446=CARTESIAN_POINT('Ctrl Pts',(4.99501900857966,139.563047429241,14.6508807702581));
#79447=CARTESIAN_POINT('Ctrl Pts',(4.99547881388643,139.555370426522,14.6540550009044));
#79448=CARTESIAN_POINT('Ctrl Pts',(4.99677352348183,139.5338466528,14.6627406601994));
#79449=CARTESIAN_POINT('Ctrl Pts',(4.99761628450161,139.51994244611,14.6681060534114));
#79450=CARTESIAN_POINT('Ctrl Pts',(5.0038526295739,139.41761102848,14.705808752729));
#79451=CARTESIAN_POINT('Ctrl Pts',(5.0095836642536,139.326333119556,14.7297559339527));
#79452=CARTESIAN_POINT('Ctrl Pts',(5.01880232494781,139.174930702076,14.7542141032738));
#79453=CARTESIAN_POINT('Ctrl Pts',(5.02232880022041,139.11594429806,14.7601018052138));
#79454=CARTESIAN_POINT('Ctrl Pts',(5.02801402233816,139.018005018681,14.7639030859506));
#79455=CARTESIAN_POINT('Ctrl Pts',(5.03022326647168,138.979203811503,14.7638662279143));
#79456=CARTESIAN_POINT('Ctrl Pts',(5.03333257655306,138.923477506688,14.7615967319414));
#79457=CARTESIAN_POINT('Ctrl Pts',(5.03427031242056,138.90652063568,14.7606102633936));
#79458=CARTESIAN_POINT('Ctrl Pts',(5.03591262208634,138.876566243085,14.7583438539825));
#79459=CARTESIAN_POINT('Ctrl Pts',(5.03662087629769,138.863561713782,14.7571847165865));
#79460=CARTESIAN_POINT('Ctrl Pts',(5.03810674242522,138.83610562449,14.7543666754639));
#79461=CARTESIAN_POINT('Ctrl Pts',(5.03888296666831,138.821659724293,14.752666017947));
#79462=CARTESIAN_POINT('Ctrl Pts',(5.04097729194917,138.782428296083,14.747453402945));
#79463=CARTESIAN_POINT('Ctrl Pts',(5.04228219856684,138.757703187908,14.743520401952));
#79464=CARTESIAN_POINT('Ctrl Pts',(5.04946532204629,138.620400192299,14.718052248975));
#79465=CARTESIAN_POINT('Ctrl Pts',(5.05493407459768,138.510559260962,14.6839859156849));
#79466=CARTESIAN_POINT('Ctrl Pts',(5.06265286310582,138.366234640612,14.6198672128381));
#79467=CARTESIAN_POINT('Ctrl Pts',(5.06478975637915,138.327457004694,14.6005358620952));
#79468=CARTESIAN_POINT('Ctrl Pts',(5.06833045295634,138.266578987038,14.5667355480619));
#79469=CARTESIAN_POINT('Ctrl Pts',(5.06969265011079,138.243912509433,14.5533382939366));
#79470=CARTESIAN_POINT('Ctrl Pts',(5.07163537463751,138.212903160918,14.5338625515269));
#79471=CARTESIAN_POINT('Ctrl Pts',(5.07218674618762,138.204243578797,14.528295541012));
#79472=CARTESIAN_POINT('Ctrl Pts',(5.07314489350277,138.18945617945,14.5185671179001));
#79473=CARTESIAN_POINT('Ctrl Pts',(5.07354884717647,138.183300029537,14.5144497776335));
#79474=CARTESIAN_POINT('Ctrl Pts',(5.07443269150977,138.170004399232,14.5054106098516));
#79475=CARTESIAN_POINT('Ctrl Pts',(5.07491361493358,138.16287733258,14.5004720186524));
#79476=CARTESIAN_POINT('Ctrl Pts',(5.07630450722704,138.142555661318,14.486121467005));
#79477=CARTESIAN_POINT('Ctrl Pts',(5.07722394552476,138.129473323293,14.4765535217626));
#79478=CARTESIAN_POINT('Ctrl Pts',(5.08190186572212,138.064495102423,14.4273537908969));
#79479=CARTESIAN_POINT('Ctrl Pts',(5.08581549023863,138.01513705013,14.3844997577729));
#79480=CARTESIAN_POINT('Ctrl Pts',(5.0942867185469,137.915306700359,14.2853717699152));
#79481=CARTESIAN_POINT('Ctrl Pts',(5.09883474597897,137.865986216653,14.2281871016063));
#79482=CARTESIAN_POINT('Ctrl Pts',(5.10595098669164,137.793892199592,14.1302245870076));
#79483=CARTESIAN_POINT('Ctrl Pts',(5.10860223332788,137.768271521638,14.0917161676484));
#79484=CARTESIAN_POINT('Ctrl Pts',(5.11219468617073,137.735256992552,14.036601609092));
#79485=CARTESIAN_POINT('Ctrl Pts',(5.11319186334254,137.726285197964,14.0209767328904));
#79486=CARTESIAN_POINT('Ctrl Pts',(5.11490159218869,137.711245108907,13.9936261456993));
#79487=CARTESIAN_POINT('Ctrl Pts',(5.11561884639264,137.705042881322,13.9819768882044));
#79488=CARTESIAN_POINT('Ctrl Pts',(5.11709049190248,137.692545861232,13.9577191389076));
#79489=CARTESIAN_POINT('Ctrl Pts',(5.11784403035187,137.686273891123,13.94510039557));
#79490=CARTESIAN_POINT('Ctrl Pts',(5.11979932245047,137.670344496966,13.9118554631895));
#79491=CARTESIAN_POINT('Ctrl Pts',(5.12099085694664,137.660984394251,13.8910906408747));
#79492=CARTESIAN_POINT('Ctrl Pts',(5.12794340021902,137.608572669799,13.7671768538486));
#79493=CARTESIAN_POINT('Ctrl Pts',(5.13330636907962,137.57696824617,13.6595921755099));
#79494=CARTESIAN_POINT('Ctrl Pts',(5.14218297669775,137.54592361668,13.4801235496561));
#79495=CARTESIAN_POINT('Ctrl Pts',(5.14564447161847,137.538947345914,13.410026280976));
#79496=CARTESIAN_POINT('Ctrl Pts',(5.15002837370352,137.536679592768,13.3264741820039));
#79497=CARTESIAN_POINT('Ctrl Pts',(5.15073066744659,137.5365,13.3132371636019));
#79498=CARTESIAN_POINT('Ctrl Pts',(5.15144231116594,137.5365,13.3));
#79499=CARTESIAN_POINT('Origin',(4.2,139.,13.3));
#79500=CARTESIAN_POINT('',(5.72391728548022,137.5365,13.299999999962));
#79501=CARTESIAN_POINT('',(5.65336626804119,137.5365,13.3000000000336));
#79502=CARTESIAN_POINT('',(4.2,137.5365,13.3));
#79503=CARTESIAN_POINT('',(5.2255072336721,137.536499824611,13.2997577413145));
#79504=CARTESIAN_POINT('Ctrl Pts',(5.72391728548022,137.5365,13.299999999962));
#79505=CARTESIAN_POINT('Ctrl Pts',(5.72389637822813,137.5365,13.3004283951292));
#79506=CARTESIAN_POINT('Ctrl Pts',(5.72387547249502,137.536500188098,13.3008567940772));
#79507=CARTESIAN_POINT('Ctrl Pts',(5.71865265859192,137.536594181926,13.4078908979809));
#79508=CARTESIAN_POINT('Ctrl Pts',(5.7135925703568,137.548335533245,13.5141545643487));
#79509=CARTESIAN_POINT('Ctrl Pts',(5.70723738865168,137.574864658269,13.6332564662892));
#79510=CARTESIAN_POINT('Ctrl Pts',(5.70642300759539,137.57845946586,13.648271571164));
#79511=CARTESIAN_POINT('Ctrl Pts',(5.70513895596488,137.584409563309,13.671495397304));
#79512=CARTESIAN_POINT('Ctrl Pts',(5.70467797229086,137.586600386487,13.6797454935331));
#79513=CARTESIAN_POINT('Ctrl Pts',(5.70380404553555,137.590851812169,13.6952086850735));
#79514=CARTESIAN_POINT('Ctrl Pts',(5.70339200516247,137.592895891053,13.7024258159171));
#79515=CARTESIAN_POINT('Ctrl Pts',(5.70238346454748,137.597996370207,13.7199202726893));
#79516=CARTESIAN_POINT('Ctrl Pts',(5.70178381971873,137.601110374666,13.7301802128068));
#79517=CARTESIAN_POINT('Ctrl Pts',(5.69952978702925,137.613128469687,13.7682661235052));
#79518=CARTESIAN_POINT('Ctrl Pts',(5.69784081637494,137.622751992439,13.7958563424438));
#79519=CARTESIAN_POINT('Ctrl Pts',(5.69312465437233,137.651478924373,13.8709113489526));
#79520=CARTESIAN_POINT('Ctrl Pts',(5.6900492266378,137.672255226099,13.9176910625191));
#79521=CARTESIAN_POINT('Ctrl Pts',(5.68060372021012,137.743319690697,14.0574622007059));
#79522=CARTESIAN_POINT('Ctrl Pts',(5.67426820867668,137.801267145866,14.1461915252801));
#79523=CARTESIAN_POINT('Ctrl Pts',(5.66694802020969,137.883214985727,14.2461389450492));
#79524=CARTESIAN_POINT('Ctrl Pts',(5.66563009526459,137.898596194119,14.2640007357975));
#79525=CARTESIAN_POINT('Ctrl Pts',(5.66354012923289,137.924000012934,14.2920993247205));
#79526=CARTESIAN_POINT('Ctrl Pts',(5.66275711945597,137.933752684019,14.302573550367));
#79527=CARTESIAN_POINT('Ctrl Pts',(5.6612625736126,137.952816984269,14.3224554355365));
#79528=CARTESIAN_POINT('Ctrl Pts',(5.66055016371869,137.962105641241,14.3318830854263));
#79529=CARTESIAN_POINT('Ctrl Pts',(5.65889193409669,137.984191531386,14.3536994780832));
#79530=CARTESIAN_POINT('Ctrl Pts',(5.6579507193345,137.997089696933,14.36598329992));
#79531=CARTESIAN_POINT('Ctrl Pts',(5.65471068725743,138.042709486387,14.4078690426697));
#79532=CARTESIAN_POINT('Ctrl Pts',(5.65246288138475,138.076544003566,14.4362255112131));
#79533=CARTESIAN_POINT('Ctrl Pts',(5.64656531863272,138.170277436183,14.5078256707518));
#79534=CARTESIAN_POINT('Ctrl Pts',(5.64300302555776,138.232253012377,14.5481375679306));
#79535=CARTESIAN_POINT('Ctrl Pts',(5.63602132383873,138.358058514244,14.617037904631));
#79536=CARTESIAN_POINT('Ctrl Pts',(5.632612065005,138.42141378614,14.646073537052));
#79537=CARTESIAN_POINT('Ctrl Pts',(5.62815343091723,138.501743713544,14.6761667309332));
#79538=CARTESIAN_POINT('Ctrl Pts',(5.62730111691074,138.51699246217,14.681592513932));
#79539=CARTESIAN_POINT('Ctrl Pts',(5.62596970057426,138.540570722669,14.6895440508814));
#79540=CARTESIAN_POINT('Ctrl Pts',(5.62550031015406,138.548838434775,14.6922503957847));
#79541=CARTESIAN_POINT('Ctrl Pts',(5.62462020890355,138.564242986697,14.6971412873433));
#79542=CARTESIAN_POINT('Ctrl Pts',(5.62421058799822,138.571373137075,14.6993451879723));
#79543=CARTESIAN_POINT('Ctrl Pts',(5.62322113619387,138.588507002627,14.7044979638206));
#79544=CARTESIAN_POINT('Ctrl Pts',(5.62263846368407,138.598525820858,14.7073945743019));
#79545=CARTESIAN_POINT('Ctrl Pts',(5.62052769670455,138.634604237196,14.7174088821815));
#79546=CARTESIAN_POINT('Ctrl Pts',(5.61897022514301,138.660827578822,14.7239114771334));
#79547=CARTESIAN_POINT('Ctrl Pts',(5.6147551592352,138.731204470769,14.7393085104492));
#79548=CARTESIAN_POINT('Ctrl Pts',(5.61205950614645,138.775613650252,14.7468968252568));
#79549=CARTESIAN_POINT('Ctrl Pts',(5.60226436306562,138.937188858354,14.7668876046108));
#79550=CARTESIAN_POINT('Ctrl Pts',(5.59516570191898,139.055417762657,14.7671884546904));
#79551=CARTESIAN_POINT('Ctrl Pts',(5.5872746105708,139.194233374073,14.7507199658923));
#79552=CARTESIAN_POINT('Ctrl Pts',(5.58604909393427,139.215992171165,14.7476403140392));
#79553=CARTESIAN_POINT('Ctrl Pts',(5.58406836846119,139.251477418635,14.7417999329865));
#79554=CARTESIAN_POINT('Ctrl Pts',(5.58330417193893,139.265247633504,14.7393302785854));
#79555=CARTESIAN_POINT('Ctrl Pts',(5.58182146426441,139.292111278597,14.7341137211655));
#79556=CARTESIAN_POINT('Ctrl Pts',(5.58110249043369,139.305206599046,14.7313839850039));
#79557=CARTESIAN_POINT('Ctrl Pts',(5.57939068850764,139.336536138022,14.7244037916816));
#79558=CARTESIAN_POINT('Ctrl Pts',(5.57840340179084,139.354730022388,14.7199821785688));
#79559=CARTESIAN_POINT('Ctrl Pts',(5.57473089708195,139.422787296265,14.7020526395447));
#79560=CARTESIAN_POINT('Ctrl Pts',(5.57211827514126,139.472010574343,14.6862566088054));
#79561=CARTESIAN_POINT('Ctrl Pts',(5.56442898639115,139.616893465292,14.6311480523088));
#79562=CARTESIAN_POINT('Ctrl Pts',(5.55954090568322,139.709318528831,14.5842811928146));
#79563=CARTESIAN_POINT('Ctrl Pts',(5.55246840493619,139.828257901125,14.5071851007473));
#79564=CARTESIAN_POINT('Ctrl Pts',(5.55051524489856,139.859646042782,14.4850380898172));
#79565=CARTESIAN_POINT('Ctrl Pts',(5.54785935113477,139.899654459646,14.4543821905583));
#79566=CARTESIAN_POINT('Ctrl Pts',(5.54721996416373,139.90909377802,14.4469633266888));
#79567=CARTESIAN_POINT('Ctrl Pts',(5.54619721030052,139.923864333395,14.435057476911));
#79568=CARTESIAN_POINT('Ctrl Pts',(5.54581903187127,139.929256819687,14.4306469569978));
#79569=CARTESIAN_POINT('Ctrl Pts',(5.54500939844907,139.940648532755,14.4211931198686));
#79570=CARTESIAN_POINT('Ctrl Pts',(5.54457719797828,139.946639097534,14.4161398148752));
#79571=CARTESIAN_POINT('Ctrl Pts',(5.54344548138047,139.962101216796,14.4028828169579));
#79572=CARTESIAN_POINT('Ctrl Pts',(5.54274092982271,139.971508354934,14.3946052959675));
#79573=CARTESIAN_POINT('Ctrl Pts',(5.53924676317011,140.017168473478,14.3533758222069));
#79574=CARTESIAN_POINT('Ctrl Pts',(5.53635880439322,140.051854881851,14.3187408150879));
#79575=CARTESIAN_POINT('Ctrl Pts',(5.52987984334206,140.124641088656,14.2383753653396));
#79576=CARTESIAN_POINT('Ctrl Pts',(5.52627752556616,140.161824111303,14.1919252695472));
#79577=CARTESIAN_POINT('Ctrl Pts',(5.51797867341239,140.241635265008,14.078732269978));
#79578=CARTESIAN_POINT('Ctrl Pts',(5.51333182801939,140.281885954351,14.010530343963));
#79579=CARTESIAN_POINT('Ctrl Pts',(5.50770395810861,140.325550132345,13.9206323577577));
#79580=CARTESIAN_POINT('Ctrl Pts',(5.50654235398232,140.334264689012,13.9016689121472));
#79581=CARTESIAN_POINT('Ctrl Pts',(5.50463715044389,140.348051952222,13.8698927913858));
#79582=CARTESIAN_POINT('Ctrl Pts',(5.5038858529879,140.353354423861,13.8571837050474));
#79583=CARTESIAN_POINT('Ctrl Pts',(5.50240882193819,140.363506394877,13.8318508922021));
#79584=CARTESIAN_POINT('Ctrl Pts',(5.50168294448817,140.36836186416,13.8192310525399));
#79585=CARTESIAN_POINT('Ctrl Pts',(5.49992148939154,140.379808536156,13.7882037079661));
#79586=CARTESIAN_POINT('Ctrl Pts',(5.49889233365343,140.386207197057,13.7697276993828));
#79587=CARTESIAN_POINT('Ctrl Pts',(5.4947398886582,140.410790720533,13.6938601324959));
#79588=CARTESIAN_POINT('Ctrl Pts',(5.49171847632477,140.42579725201,13.6354987578867));
#79589=CARTESIAN_POINT('Ctrl Pts',(5.48582101902314,140.448412099927,13.5178998681133));
#79590=CARTESIAN_POINT('Ctrl Pts',(5.48294889062536,140.456077893386,13.458792970542));
#79591=CARTESIAN_POINT('Ctrl Pts',(5.47693737706805,140.464450500837,13.3357848690572));
#79592=CARTESIAN_POINT('Ctrl Pts',(5.47379931191519,140.464619094939,13.2719761437451));
#79593=CARTESIAN_POINT('Ctrl Pts',(5.46964664275004,140.459616931282,13.1922426392474));
#79594=CARTESIAN_POINT('Ctrl Pts',(5.4687958546543,140.458338558129,13.1761378072726));
#79595=CARTESIAN_POINT('Ctrl Pts',(5.46746642633736,140.455962839974,13.151406602761));
#79596=CARTESIAN_POINT('Ctrl Pts',(5.46699746099894,140.455054733,13.1427629007822));
#79597=CARTESIAN_POINT('Ctrl Pts',(5.46611779991708,140.453223864314,13.1267131090235));
#79598=CARTESIAN_POINT('Ctrl Pts',(5.46570818692665,140.452321361576,13.1193052287706));
#79599=CARTESIAN_POINT('Ctrl Pts',(5.46471835710986,140.450020992145,13.101555346394));
#79600=CARTESIAN_POINT('Ctrl Pts',(5.46413529008978,140.448569103508,13.0912209359819));
#79601=CARTESIAN_POINT('Ctrl Pts',(5.46202111818797,140.442954835541,13.0541419545273));
#79602=CARTESIAN_POINT('Ctrl Pts',(5.46046051416501,140.438161426173,13.0274997788727));
#79603=CARTESIAN_POINT('Ctrl Pts',(5.45623386065201,140.423404113051,12.9567896154052));
#79604=CARTESIAN_POINT('Ctrl Pts',(5.45352952400148,140.412133945916,12.913024566162));
#79605=CARTESIAN_POINT('Ctrl Pts',(5.44374294222581,140.364326547212,12.7575526153661));
#79606=CARTESIAN_POINT('Ctrl Pts',(5.4366625875207,140.31639024624,12.6497989908346));
#79607=CARTESIAN_POINT('Ctrl Pts',(5.42878468025893,140.244777001058,12.5300343004235));
#79608=CARTESIAN_POINT('Ctrl Pts',(5.42755661454506,140.233052939967,12.511395230575));
#79609=CARTESIAN_POINT('Ctrl Pts',(5.42557288282212,140.21319406304,12.4813496792768));
#79610=CARTESIAN_POINT('Ctrl Pts',(5.42480817596103,140.205308494417,12.4697833809009));
#79611=CARTESIAN_POINT('Ctrl Pts',(5.42332521182643,140.189568372943,12.4473933414201));
#79612=CARTESIAN_POINT('Ctrl Pts',(5.42260647974065,140.181729035038,12.436560637797));
#79613=CARTESIAN_POINT('Ctrl Pts',(5.42089644896204,140.162577485868,12.4108457868462));
#79614=CARTESIAN_POINT('Ctrl Pts',(5.41991066083533,140.151126334015,12.3960697866276));
#79615=CARTESIAN_POINT('Ctrl Pts',(5.4162533701934,140.1071431454,12.3415078546338));
#79616=CARTESIAN_POINT('Ctrl Pts',(5.41365362948447,140.072804949657,12.3032235283665));
#79617=CARTESIAN_POINT('Ctrl Pts',(5.40604299584359,139.964521200469,12.1945893362171));
#79618=CARTESIAN_POINT('Ctrl Pts',(5.40121505470921,139.885172302452,12.1300844713586));
#79619=CARTESIAN_POINT('Ctrl Pts',(5.39415212338304,139.766427698706,12.0526005056986));
#79620=CARTESIAN_POINT('Ctrl Pts',(5.39213093264031,139.732218250109,12.0322173358668));
#79621=CARTESIAN_POINT('Ctrl Pts',(5.38939545877631,139.686553104341,12.0074736492702));
#79622=CARTESIAN_POINT('Ctrl Pts',(5.38874939080079,139.67581168462,12.001825096474));
#79623=CARTESIAN_POINT('Ctrl Pts',(5.38771861103018,139.658774511172,11.9931345670738));
#79624=CARTESIAN_POINT('Ctrl Pts',(5.38733923226514,139.652524859342,11.9900028930779));
#79625=CARTESIAN_POINT('Ctrl Pts',(5.38653008246416,139.639247501558,11.9834682499054));
#79626=CARTESIAN_POINT('Ctrl Pts',(5.38609960638404,139.632214590793,11.980076547275));
#79627=CARTESIAN_POINT('Ctrl Pts',(5.38497770191796,139.61395370643,11.9714494469709));
#79628=CARTESIAN_POINT('Ctrl Pts',(5.38428139150684,139.602685956641,11.9663001303511));
#79629=CARTESIAN_POINT('Ctrl Pts',(5.38092214719258,139.54856011565,11.9423907878854));
#79630=CARTESIAN_POINT('Ctrl Pts',(5.37816948083471,139.504887055656,11.9255512638113));
#79631=CARTESIAN_POINT('Ctrl Pts',(5.36859128213735,139.352522387501,11.875044805052));
#79632=CARTESIAN_POINT('Ctrl Pts',(5.36164375114044,139.240737436001,11.851959883935));
#79633=CARTESIAN_POINT('Ctrl Pts',(5.35291289419451,139.090464055092,11.8388280316334));
#79634=CARTESIAN_POINT('Ctrl Pts',(5.35080417091939,139.053412249684,11.8370048736925));
#79635=CARTESIAN_POINT('Ctrl Pts',(5.34780341457363,138.99954809044,11.8364038565968));
#79636=CARTESIAN_POINT('Ctrl Pts',(5.34687747424622,138.982765000258,11.8365052569061));
#79637=CARTESIAN_POINT('Ctrl Pts',(5.34524445508551,138.952885706068,11.8371998679991));
#79638=CARTESIAN_POINT('Ctrl Pts',(5.34453395360437,138.939788955931,11.8376803945055));
#79639=CARTESIAN_POINT('Ctrl Pts',(5.3430317626913,138.911902479224,11.8390788530151));
#79640=CARTESIAN_POINT('Ctrl Pts',(5.34224167617368,138.897116613836,11.8400456166482));
#79641=CARTESIAN_POINT('Ctrl Pts',(5.34007816415281,138.856326418779,11.8433354338352));
#79642=CARTESIAN_POINT('Ctrl Pts',(5.33871940407466,138.830365124708,11.8461300356354));
#79643=CARTESIAN_POINT('Ctrl Pts',(5.3356780056225,138.771648982735,11.8540448533916));
#79644=CARTESIAN_POINT('Ctrl Pts',(5.33400772487917,138.738965258159,11.8595863411916));
#79645=CARTESIAN_POINT('Ctrl Pts',(5.32787996588602,138.618292921139,11.8842889232365));
#79646=CARTESIAN_POINT('Ctrl Pts',(5.32358549382512,138.531946212759,11.9104448448433));
#79647=CARTESIAN_POINT('Ctrl Pts',(5.31652840601565,138.399012477598,11.9645201713861));
#79648=CARTESIAN_POINT('Ctrl Pts',(5.31385344278118,138.350620067362,11.9873701649532));
#79649=CARTESIAN_POINT('Ctrl Pts',(5.31036447819183,138.292185530774,12.0189851317788));
#79650=CARTESIAN_POINT('Ctrl Pts',(5.30967577803063,138.280862874708,12.0253070222855));
#79651=CARTESIAN_POINT('Ctrl Pts',(5.30855135615362,138.262753915427,12.0357360435736));
#79652=CARTESIAN_POINT('Ctrl Pts',(5.30812129578216,138.255914162491,12.0397494689021));
#79653=CARTESIAN_POINT('Ctrl Pts',(5.30725880344192,138.242378267333,12.0478406557384));
#79654=CARTESIAN_POINT('Ctrl Pts',(5.30682645844377,138.235681622389,12.0519170203705));
#79655=CARTESIAN_POINT('Ctrl Pts',(5.30569398860872,138.218358540849,12.0626535824364));
#79656=CARTESIAN_POINT('Ctrl Pts',(5.30498881718051,138.207784566565,12.069396809259));
#79657=CARTESIAN_POINT('Ctrl Pts',(5.30148438581034,138.156194204514,12.1032374464806));
#79658=CARTESIAN_POINT('Ctrl Pts',(5.29858611670499,138.116477271433,12.1322518993748));
#79659=CARTESIAN_POINT('Ctrl Pts',(5.29210541126258,138.032240467435,12.2005502924573));
#79660=CARTESIAN_POINT('Ctrl Pts',(5.28851227052994,137.988494315543,12.2406584725215));
#79661=CARTESIAN_POINT('Ctrl Pts',(5.28022459515594,137.892405800322,12.3401501579366));
#79662=CARTESIAN_POINT('Ctrl Pts',(5.27557990580273,137.842197838869,12.4013489706316));
#79663=CARTESIAN_POINT('Ctrl Pts',(5.26995414774073,137.785286932719,12.4834586694853));
#79664=CARTESIAN_POINT('Ctrl Pts',(5.2687926787047,137.773769005332,12.5008597173924));
#79665=CARTESIAN_POINT('Ctrl Pts',(5.26688760417105,137.755273607153,12.5301441245525));
#79666=CARTESIAN_POINT('Ctrl Pts',(5.26613630418817,137.748085057403,12.5418899442028));
#79667=CARTESIAN_POINT('Ctrl Pts',(5.26465920006158,137.734168031286,12.5653677631145));
#79668=CARTESIAN_POINT('Ctrl Pts',(5.26393325316231,137.727434281331,12.5770950235596));
#79669=CARTESIAN_POINT('Ctrl Pts',(5.26217150526856,137.711362780758,12.606005229778));
#79670=CARTESIAN_POINT('Ctrl Pts',(5.26114212995328,137.702204909271,12.6232854558685));
#79671=CARTESIAN_POINT('Ctrl Pts',(5.25698723001979,137.666258370454,12.6945293134945));
#79672=CARTESIAN_POINT('Ctrl Pts',(5.2539637372614,137.64246644401,12.7499408288739));
#79673=CARTESIAN_POINT('Ctrl Pts',(5.24709262408483,137.595432626154,12.8813025273928));
#79674=CARTESIAN_POINT('Ctrl Pts',(5.24330052769944,137.574818391967,12.9579853109963));
#79675=CARTESIAN_POINT('Ctrl Pts',(5.23802369550025,137.555506771268,13.0632672224454));
#79676=CARTESIAN_POINT('Ctrl Pts',(5.23664098441709,137.551275932362,13.090711779619));
#79677=CARTESIAN_POINT('Ctrl Pts',(5.23386176523994,137.544474589783,13.1450567819482));
#79678=CARTESIAN_POINT('Ctrl Pts',(5.23246718569157,137.541863418749,13.1719407837177));
#79679=CARTESIAN_POINT('Ctrl Pts',(5.23047084162199,137.539259359563,13.2095390088446));
#79680=CARTESIAN_POINT('Ctrl Pts',(5.22989933575708,137.53863788567,13.2202054712121));
#79681=CARTESIAN_POINT('Ctrl Pts',(5.22892328871679,137.537785449126,13.2382335798347));
#79682=CARTESIAN_POINT('Ctrl Pts',(5.22852203532409,137.537493159396,13.2455920639323));
#79683=CARTESIAN_POINT('Ctrl Pts',(5.22771005788807,137.537017846487,13.2603699195707));
#79684=CARTESIAN_POINT('Ctrl Pts',(5.2272993791108,137.536835702114,13.2677888646555));
#79685=CARTESIAN_POINT('Ctrl Pts',(5.22642976870488,137.536571363474,13.2833912809813));
#79686=CARTESIAN_POINT('Ctrl Pts',(5.22597023111713,137.53650137286,13.2915746869978));
#79687=CARTESIAN_POINT('Ctrl Pts',(5.22550755435867,137.536500019999,13.2997580565886));
#79688=CARTESIAN_POINT('Ctrl Pts',(5.22550757110334,137.536500020048,13.2997577604254));
#79689=CARTESIAN_POINT('Ctrl Pts',(5.22550300580094,137.536500006683,13.2998385069991));
#79690=CARTESIAN_POINT('Ctrl Pts',(5.22549844019539,137.5365,13.2999192535242));
#79691=CARTESIAN_POINT('Ctrl Pts',(5.22549387428705,137.5365,13.2999999999999));
#79692=CARTESIAN_POINT('',(5.65328936190197,137.536500632965,13.3012892780789));
#79693=CARTESIAN_POINT('Ctrl Pts',(5.15144231116594,137.5365,13.3));
#79694=CARTESIAN_POINT('Ctrl Pts',(5.15144646621951,137.5365,13.2999227125564));
#79695=CARTESIAN_POINT('Ctrl Pts',(5.15145062163286,137.536500006051,13.29984542511));
#79696=CARTESIAN_POINT('Ctrl Pts',(5.15188347220723,137.536501281478,13.2917952796205));
#79697=CARTESIAN_POINT('Ctrl Pts',(5.15231554190402,137.536567696437,13.2838227555621));
#79698=CARTESIAN_POINT('Ctrl Pts',(5.15317263650352,137.536826449736,13.26814344612));
#79699=CARTESIAN_POINT('Ctrl Pts',(5.15359743401917,137.537014548003,13.2604369174702));
#79700=CARTESIAN_POINT('Ctrl Pts',(5.1546951210923,137.537653110221,13.2406760253341));
#79701=CARTESIAN_POINT('Ctrl Pts',(5.15537256982121,137.538191741659,13.2286252396572));
#79702=CARTESIAN_POINT('Ctrl Pts',(5.15849059953924,137.541325323637,13.1737379114092));
#79703=CARTESIAN_POINT('Ctrl Pts',(5.16100682102238,137.545654579616,13.1310244124952));
#79704=CARTESIAN_POINT('Ctrl Pts',(5.17040674743905,137.568476826116,12.9747106951274));
#79705=CARTESIAN_POINT('Ctrl Pts',(5.17745000925033,137.598472760067,12.8631954233111));
#79706=CARTESIAN_POINT('Ctrl Pts',(5.18635965703472,137.655493181044,12.7206821770838));
#79707=CARTESIAN_POINT('Ctrl Pts',(5.18854988645136,137.671161592884,12.6855924882341));
#79708=CARTESIAN_POINT('Ctrl Pts',(5.19165583146573,137.69583001922,12.6357187467277));
#79709=CARTESIAN_POINT('Ctrl Pts',(5.19260796013722,137.703738527365,12.620415455939));
#79710=CARTESIAN_POINT('Ctrl Pts',(5.19426897269919,137.718146201342,12.5937030700346));
#79711=CARTESIAN_POINT('Ctrl Pts',(5.19498173743427,137.724532062223,12.5822353660219));
#79712=CARTESIAN_POINT('Ctrl Pts',(5.1964587349886,137.738187621774,12.5584706478231));
#79713=CARTESIAN_POINT('Ctrl Pts',(5.19722187964384,137.745484844507,12.5461910041623));
#79714=CARTESIAN_POINT('Ctrl Pts',(5.19923606196109,137.765380514118,12.5138002443835));
#79715=CARTESIAN_POINT('Ctrl Pts',(5.20047565704583,137.778290522975,12.4938850162607));
#79716=CARTESIAN_POINT('Ctrl Pts',(5.20546860748793,137.832913404767,12.4139512832592));
#79717=CARTESIAN_POINT('Ctrl Pts',(5.20907482337719,137.878611397436,12.3567808620436));
#79718=CARTESIAN_POINT('Ctrl Pts',(5.21668441351769,137.984936661586,12.2424690942639));
#79719=CARTESIAN_POINT('Ctrl Pts',(5.22066134704973,138.046548021553,12.1866030186736));
#79720=CARTESIAN_POINT('Ctrl Pts',(5.2263257844008,138.135612605281,12.1186840919646));
#79721=CARTESIAN_POINT('Ctrl Pts',(5.22781859081503,138.159183010634,12.1017932440421));
#79722=CARTESIAN_POINT('Ctrl Pts',(5.2299308936223,138.192311079561,12.0795122212282));
#79723=CARTESIAN_POINT('Ctrl Pts',(5.23051517800192,138.201452046782,12.0735119395835));
#79724=CARTESIAN_POINT('Ctrl Pts',(5.23151122929005,138.21697366425,12.0635703664218));
#79725=CARTESIAN_POINT('Ctrl Pts',(5.23191953131606,138.223319102512,12.0595745634491));
#79726=CARTESIAN_POINT('Ctrl Pts',(5.23278959702834,138.236797106945,12.0512312615137));
#79727=CARTESIAN_POINT('Ctrl Pts',(5.23325203873197,138.243936530905,12.0468958375753));
#79728=CARTESIAN_POINT('Ctrl Pts',(5.23456188055164,138.264104774722,12.0348837422996));
#79729=CARTESIAN_POINT('Ctrl Pts',(5.23541741902444,138.277215704362,12.0273477483613));
#79730=CARTESIAN_POINT('Ctrl Pts',(5.23740732974182,138.307633005543,12.0104859013627));
#79731=CARTESIAN_POINT('Ctrl Pts',(5.23854815078499,138.325015101979,12.0013029643975));
#79732=CARTESIAN_POINT('Ctrl Pts',(5.242593073207,138.386651087998,11.9703124169934));
#79733=CARTESIAN_POINT('Ctrl Pts',(5.24555540226669,138.431816565312,11.9503951956846));
#79734=CARTESIAN_POINT('Ctrl Pts',(5.25510285665952,138.579914644636,11.893840210316));
#79735=CARTESIAN_POINT('Ctrl Pts',(5.26166103881786,138.685985989613,11.8664173976163));
#79736=CARTESIAN_POINT('Ctrl Pts',(5.2691492785385,138.817003073326,11.8478023457227));
#79737=CARTESIAN_POINT('Ctrl Pts',(5.27044022770045,138.839948867676,11.8450946343882));
#79738=CARTESIAN_POINT('Ctrl Pts',(5.27249505040638,138.8770443951,11.8416054801674));
#79739=CARTESIAN_POINT('Ctrl Pts',(5.27326935387441,138.891157501101,11.8404843315371));
#79740=CARTESIAN_POINT('Ctrl Pts',(5.27475165734572,138.918427133229,11.8387157842537));
#79741=CARTESIAN_POINT('Ctrl Pts',(5.27546044684804,138.93158044096,11.8380408790497));
#79742=CARTESIAN_POINT('Ctrl Pts',(5.27711649088458,138.962567728502,11.8368700304699));
#79743=CARTESIAN_POINT('Ctrl Pts',(5.2780590542116,138.980405391547,11.8365224392377));
#79744=CARTESIAN_POINT('Ctrl Pts',(5.28133794221558,139.043094612097,11.8364472844683));
#79745=CARTESIAN_POINT('Ctrl Pts',(5.28362124549377,139.087924597964,11.8384551228243));
#79746=CARTESIAN_POINT('Ctrl Pts',(5.28967052909967,139.208511052563,11.8494254871192));
#79747=CARTESIAN_POINT('Ctrl Pts',(5.29334217554952,139.283773927069,11.8622531415987));
#79748=CARTESIAN_POINT('Ctrl Pts',(5.30027948630146,139.421859560158,11.897058279467));
#79749=CARTESIAN_POINT('Ctrl Pts',(5.30352943641082,139.484848413172,11.9175632208407));
#79750=CARTESIAN_POINT('Ctrl Pts',(5.30781295347927,139.56132804225,11.9483314008382));
#79751=CARTESIAN_POINT('Ctrl Pts',(5.30866988649024,139.576325316098,11.9546575676899));
#79752=CARTESIAN_POINT('Ctrl Pts',(5.31000524925259,139.599158556797,11.9647409573135));
#79753=CARTESIAN_POINT('Ctrl Pts',(5.31047380481253,139.607072174531,11.9683202132259));
#79754=CARTESIAN_POINT('Ctrl Pts',(5.31134972829718,139.621671607149,11.975080577099));
#79755=CARTESIAN_POINT('Ctrl Pts',(5.31175596911822,139.62836583279,11.9782422929549));
#79756=CARTESIAN_POINT('Ctrl Pts',(5.31273302653917,139.644288424333,11.9859109056203));
#79757=CARTESIAN_POINT('Ctrl Pts',(5.3133065569548,139.653493730939,11.9904643369108));
#79758=CARTESIAN_POINT('Ctrl Pts',(5.31535867608064,139.685967685746,12.0069553337115));
#79759=CARTESIAN_POINT('Ctrl Pts',(5.31686475778166,139.708962377867,12.0194187415709));
#79760=CARTESIAN_POINT('Ctrl Pts',(5.32089736269073,139.768730419634,12.0539169971704));
#79761=CARTESIAN_POINT('Ctrl Pts',(5.32345860558771,139.804890608806,12.0769627669271));
#79762=CARTESIAN_POINT('Ctrl Pts',(5.33281180597075,139.932296393498,12.1662614260395));
#79763=CARTESIAN_POINT('Ctrl Pts',(5.33962666596036,140.016837633374,12.2414217710385));
#79764=CARTESIAN_POINT('Ctrl Pts',(5.34753799592571,140.109333988725,12.3450682312167));
#79765=CARTESIAN_POINT('Ctrl Pts',(5.34900743183869,140.126226327528,12.365050287922));
#79766=CARTESIAN_POINT('Ctrl Pts',(5.35128076508101,140.151894358731,12.3971190189345));
#79767=CARTESIAN_POINT('Ctrl Pts',(5.35209907743536,140.161035696619,12.408904711036));
#79768=CARTESIAN_POINT('Ctrl Pts',(5.35361041140312,140.177727815262,12.4311184677967));
#79769=CARTESIAN_POINT('Ctrl Pts',(5.35430517345941,140.185324176356,12.4415103172189));
#79770=CARTESIAN_POINT('Ctrl Pts',(5.35586828005345,140.202231417226,12.4652917951563));
#79771=CARTESIAN_POINT('Ctrl Pts',(5.3567333503536,140.211457651472,12.4787396545397));
#79772=CARTESIAN_POINT('Ctrl Pts',(5.3594060230579,140.239523420335,12.5211498845817));
#79773=CARTESIAN_POINT('Ctrl Pts',(5.36118445407896,140.257564041181,12.5506277776409));
#79774=CARTESIAN_POINT('Ctrl Pts',(5.36543710875225,140.29885030092,12.6237857619784));
#79775=CARTESIAN_POINT('Ctrl Pts',(5.36787707630344,140.320957619038,12.6680592058672));
#79776=CARTESIAN_POINT('Ctrl Pts',(5.37540776842262,140.382756508672,12.8093043572145));
#79777=CARTESIAN_POINT('Ctrl Pts',(5.38037692756727,140.414308946801,12.9094574267174));
#79778=CARTESIAN_POINT('Ctrl Pts',(5.38673295043903,140.438477576492,13.0299175922779));
#79779=CARTESIAN_POINT('Ctrl Pts',(5.38768614720088,140.441718983239,13.0477926243908));
#79780=CARTESIAN_POINT('Ctrl Pts',(5.38913466340411,140.446060253086,13.0745622270729));
#79781=CARTESIAN_POINT('Ctrl Pts',(5.38961708346854,140.447412596039,13.0834146507383));
#79782=CARTESIAN_POINT('Ctrl Pts',(5.39050443496787,140.449728652993,13.0995672244277));
#79783=CARTESIAN_POINT('Ctrl Pts',(5.39090793898311,140.450718642334,13.1068630575315));
#79784=CARTESIAN_POINT('Ctrl Pts',(5.39185898253675,140.452905636494,13.1239468995723));
#79785=CARTESIAN_POINT('Ctrl Pts',(5.39240881864613,140.454058816827,13.1337398759583));
#79786=CARTESIAN_POINT('Ctrl Pts',(5.39428038542812,140.457616102224,13.1668241583656));
#79787=CARTESIAN_POINT('Ctrl Pts',(5.3956238698896,140.459560081497,13.1901603255108));
#79788=CARTESIAN_POINT('Ctrl Pts',(5.39909354875647,140.463083174909,13.2496855062319));
#79789=CARTESIAN_POINT('Ctrl Pts',(5.40124463207642,140.463880114815,13.2859045974367));
#79790=CARTESIAN_POINT('Ctrl Pts',(5.41039807306712,140.461570852026,13.438713625626));
#79791=CARTESIAN_POINT('Ctrl Pts',(5.41749376015007,140.445878051767,13.55470449641));
#79792=CARTESIAN_POINT('Ctrl Pts',(5.42590183501994,140.40903585322,13.6966763473822));
#79793=CARTESIAN_POINT('Ctrl Pts',(5.42759736254931,140.40059902728,13.7255075908075));
#79794=CARTESIAN_POINT('Ctrl Pts',(5.43013576229703,140.386411919014,13.7689781273738));
#79795=CARTESIAN_POINT('Ctrl Pts',(5.43099903710802,140.381303591431,13.78381701962));
#79796=CARTESIAN_POINT('Ctrl Pts',(5.43256105048977,140.371541719345,13.8107578412828));
#79797=CARTESIAN_POINT('Ctrl Pts',(5.43326221014194,140.366964190116,13.8228854351483));
#79798=CARTESIAN_POINT('Ctrl Pts',(5.43478797649018,140.356575142137,13.8493406329289));
#79799=CARTESIAN_POINT('Ctrl Pts',(5.43561024045213,140.350696453762,13.8636402767373));
#79800=CARTESIAN_POINT('Ctrl Pts',(5.43799394653683,140.332842243807,13.9051854183788));
#79801=CARTESIAN_POINT('Ctrl Pts',(5.43953496512592,140.320260708261,13.9321626807603));
#79802=CARTESIAN_POINT('Ctrl Pts',(5.44308278099412,140.288950723886,13.9942782170509));
#79803=CARTESIAN_POINT('Ctrl Pts',(5.44506958116845,140.269593805768,14.0290734125879));
#79804=CARTESIAN_POINT('Ctrl Pts',(5.44993688475439,140.218108598054,14.1133377608396));
#79805=CARTESIAN_POINT('Ctrl Pts',(5.452781759856,140.184364210054,14.1617356846067));
#79806=CARTESIAN_POINT('Ctrl Pts',(5.45884913286976,140.107110750787,14.2593945744269));
#79807=CARTESIAN_POINT('Ctrl Pts',(5.46207162515903,140.063021218632,14.3080260697235));
#79808=CARTESIAN_POINT('Ctrl Pts',(5.46632215634683,140.004141926804,14.3647979244937));
#79809=CARTESIAN_POINT('Ctrl Pts',(5.46717667803751,139.992273047967,14.3758669922274));
#79810=CARTESIAN_POINT('Ctrl Pts',(5.46850904790812,139.973780999331,14.3925466026891));
#79811=CARTESIAN_POINT('Ctrl Pts',(5.46897708982476,139.967287572472,14.3982997123756));
#79812=CARTESIAN_POINT('Ctrl Pts',(5.46985261650331,139.95515708649,14.4088561825648));
#79813=CARTESIAN_POINT('Ctrl Pts',(5.47025898548705,139.949534151391,14.4136749886845));
#79814=CARTESIAN_POINT('Ctrl Pts',(5.47123712863113,139.936013512736,14.4250852285997));
#79815=CARTESIAN_POINT('Ctrl Pts',(5.47181163378226,139.928082551652,14.4316363516975));
#79816=CARTESIAN_POINT('Ctrl Pts',(5.47387153977532,139.899653743742,14.4546192206599));
#79817=CARTESIAN_POINT('Ctrl Pts',(5.47538469689689,139.878784219547,14.470581280652));
#79818=CARTESIAN_POINT('Ctrl Pts',(5.47944277972557,139.822517498149,14.5112640164428));
#79819=CARTESIAN_POINT('Ctrl Pts',(5.48202290309546,139.786436904842,14.5349948181222));
#79820=CARTESIAN_POINT('Ctrl Pts',(5.49147178306497,139.651445039794,14.6154643078039));
#79821=CARTESIAN_POINT('Ctrl Pts',(5.49836017198872,139.547026788292,14.6622026166579));
#79822=CARTESIAN_POINT('Ctrl Pts',(5.50627447615158,139.414197161587,14.7038901524748));
#79823=CARTESIAN_POINT('Ctrl Pts',(5.50768755231191,139.389970111386,14.7108119192568));
#79824=CARTESIAN_POINT('Ctrl Pts',(5.50989419562295,139.351329389669,14.7207801952475));
#79825=CARTESIAN_POINT('Ctrl Pts',(5.51070082119714,139.337028486189,14.7242403326006));
#79826=CARTESIAN_POINT('Ctrl Pts',(5.51220845294001,139.309974703634,14.7303557382969));
#79827=CARTESIAN_POINT('Ctrl Pts',(5.51291088256839,139.297233917155,14.733057524532));
#79828=CARTESIAN_POINT('Ctrl Pts',(5.51450111961948,139.268090259283,14.738832269715));
#79829=CARTESIAN_POINT('Ctrl Pts',(5.51538537814265,139.251667355918,14.741795498651));
#79830=CARTESIAN_POINT('Ctrl Pts',(5.51819652395127,139.198805570433,14.7504027146267));
#79831=CARTESIAN_POINT('Ctrl Pts',(5.52008946916763,139.162201739746,14.7549510518571));
#79832=CARTESIAN_POINT('Ctrl Pts',(5.52470719752459,139.071023163151,14.762796504619));
#79833=CARTESIAN_POINT('Ctrl Pts',(5.5273884606941,139.016361605603,14.7644284427876));
#79834=CARTESIAN_POINT('Ctrl Pts',(5.53432614235396,138.873959285715,14.7607038785996));
#79835=CARTESIAN_POINT('Ctrl Pts',(5.5385315852486,138.786575426571,14.7505135816117));
#79836=CARTESIAN_POINT('Ctrl Pts',(5.54420187072996,138.677942678452,14.7278126554631));
#79837=CARTESIAN_POINT('Ctrl Pts',(5.54540589547608,138.655362804147,14.7225311910118));
#79838=CARTESIAN_POINT('Ctrl Pts',(5.54712332221838,138.624044309751,14.7144163528826));
#79839=CARTESIAN_POINT('Ctrl Pts',(5.54761413656486,138.615191515355,14.7120335413478));
#79840=CARTESIAN_POINT('Ctrl Pts',(5.54851459195195,138.599143147112,14.7075518491842));
#79841=CARTESIAN_POINT('Ctrl Pts',(5.54892271245598,138.591940090674,14.7054805348877));
#79842=CARTESIAN_POINT('Ctrl Pts',(5.5497931973991,138.576733620486,14.700981001567));
#79843=CARTESIAN_POINT('Ctrl Pts',(5.55025625224375,138.568734718494,14.6985393969137));
#79844=CARTESIAN_POINT('Ctrl Pts',(5.55156957570382,138.546284493274,14.6914757237726));
#79845=CARTESIAN_POINT('Ctrl Pts',(5.55242804740352,138.531883856106,14.6866974038771));
#79846=CARTESIAN_POINT('Ctrl Pts',(5.5544260721784,138.498919713078,14.6751874950941));
#79847=CARTESIAN_POINT('Ctrl Pts',(5.55557214298547,138.480413086165,14.6683024066775));
#79848=CARTESIAN_POINT('Ctrl Pts',(5.55964517484957,138.415819653272,14.642772107222));
#79849=CARTESIAN_POINT('Ctrl Pts',(5.56263108570559,138.370550094219,14.6221558188611));
#79850=CARTESIAN_POINT('Ctrl Pts',(5.57215968650534,138.23009500097,14.5493400900722));
#79851=CARTESIAN_POINT('Ctrl Pts',(5.57867365104861,138.139607601796,14.4888380779715));
#79852=CARTESIAN_POINT('Ctrl Pts',(5.58612738079609,138.038916969706,14.4039423329906));
#79853=CARTESIAN_POINT('Ctrl Pts',(5.58742254039263,138.02155684579,14.3885854794396));
#79854=CARTESIAN_POINT('Ctrl Pts',(5.58948234907378,137.994179661264,14.363183203355));
#79855=CARTESIAN_POINT('Ctrl Pts',(5.59025751949347,137.983931613357,14.3533936259726));
#79856=CARTESIAN_POINT('Ctrl Pts',(5.59174043650857,137.96444098823,14.3342258396538));
#79857=CARTESIAN_POINT('Ctrl Pts',(5.59244899041773,137.955179639167,14.3248687640099));
#79858=CARTESIAN_POINT('Ctrl Pts',(5.59410289900716,137.933694258032,14.3025673215696));
#79859=CARTESIAN_POINT('Ctrl Pts',(5.59504359985574,137.921577546443,14.289522216996));
#79860=CARTESIAN_POINT('Ctrl Pts',(5.59830609660957,137.879972863463,14.2430575713872));
#79861=CARTESIAN_POINT('Ctrl Pts',(5.60057562209633,137.851774883274,14.2085141217825));
#79862=CARTESIAN_POINT('Ctrl Pts',(5.60656756534489,137.780275511439,14.1122675611804));
#79863=CARTESIAN_POINT('Ctrl Pts',(5.6101981834469,137.74008974083,14.0484203184192));
#79864=CARTESIAN_POINT('Ctrl Pts',(5.61741422150682,137.671059893276,13.9172988771268));
#79865=CARTESIAN_POINT('Ctrl Pts',(5.62098958648454,137.641986236878,13.8503963785111));
#79866=CARTESIAN_POINT('Ctrl Pts',(5.62551107200565,137.613610244128,13.7689722501961));
#79867=CARTESIAN_POINT('Ctrl Pts',(5.62622130129798,137.609377860415,13.7562691819363));
#79868=CARTESIAN_POINT('Ctrl Pts',(5.62737058769988,137.602899557178,13.7358972606584));
#79869=CARTESIAN_POINT('Ctrl Pts',(5.62780346399546,137.600541036462,13.7282647223738));
#79870=CARTESIAN_POINT('Ctrl Pts',(5.628660657519,137.596033157479,13.7132415669794));
#79871=CARTESIAN_POINT('Ctrl Pts',(5.62908472411609,137.59387940404,13.7058526198756));
#79872=CARTESIAN_POINT('Ctrl Pts',(5.63017827883031,137.588516195094,13.686897649915));
#79873=CARTESIAN_POINT('Ctrl Pts',(5.63085226363257,137.585390608779,13.6753086384701));
#79874=CARTESIAN_POINT('Ctrl Pts',(5.6339236577602,137.571930507609,13.622842789949));
#79875=CARTESIAN_POINT('Ctrl Pts',(5.63639408510215,137.563223535799,13.5815719847109));
#79876=CARTESIAN_POINT('Ctrl Pts',(5.64365701630666,137.543196703086,13.4610963525993));
#79877=CARTESIAN_POINT('Ctrl Pts',(5.64852536850634,137.536571038055,13.381264277037));
#79878=CARTESIAN_POINT('Ctrl Pts',(5.65328945758633,137.536500568152,13.3012895659352));
#79879=CARTESIAN_POINT('Ctrl Pts',(5.65328947433155,137.536500567904,13.3012892848334));
#79880=CARTESIAN_POINT('Ctrl Pts',(5.6533150753595,137.536500189299,13.3008595206364));
#79881=CARTESIAN_POINT('Ctrl Pts',(5.65334067327062,137.5365,13.3004297589952));
#79882=CARTESIAN_POINT('Ctrl Pts',(5.6533662680412,137.5365,13.3000000000336));
#79883=CARTESIAN_POINT('Origin',(4.2,139.,13.3));
#79884=CARTESIAN_POINT('',(6.22415553577981,137.536500247676,13.2991485609046));
#79885=CARTESIAN_POINT('',(6.1539436045687,137.5365,13.30000001305));
#79886=CARTESIAN_POINT('',(4.2,137.5365,13.3));
#79887=CARTESIAN_POINT('Ctrl Pts',(6.22273965880574,137.536500296291,13.2990687414511));
#79888=CARTESIAN_POINT('Ctrl Pts',(6.222044214228,137.536492446524,13.3114048768242));
#79889=CARTESIAN_POINT('Ctrl Pts',(6.2213535867996,137.53664057234,13.323740935255));
#79890=CARTESIAN_POINT('Ctrl Pts',(6.22001613084792,137.537233710625,13.3477968911271));
#79891=CARTESIAN_POINT('Ctrl Pts',(6.21936887733289,137.537663649918,13.3595161414469));
#79892=CARTESIAN_POINT('Ctrl Pts',(6.21807604716484,137.538811751986,13.383077486202));
#79893=CARTESIAN_POINT('Ctrl Pts',(6.2174306252796,137.539533140684,13.3949185428767));
#79894=CARTESIAN_POINT('Ctrl Pts',(6.21607770235265,137.541360165099,13.4198996497014));
#79895=CARTESIAN_POINT('Ctrl Pts',(6.21537136504241,137.542499579291,13.4330362125317));
#79896=CARTESIAN_POINT('Ctrl Pts',(6.21362057472982,137.5457900118,13.4658195203661));
#79897=CARTESIAN_POINT('Ctrl Pts',(6.21258341250646,137.548161781306,13.4854417471171));
#79898=CARTESIAN_POINT('Ctrl Pts',(6.20826591339485,137.559821838086,13.5678581426207));
#79899=CARTESIAN_POINT('Ctrl Pts',(6.20510621794372,137.572792873788,13.6300637899079));
#79900=CARTESIAN_POINT('Ctrl Pts',(6.19722307775851,137.616026451684,13.7859021479421));
#79901=CARTESIAN_POINT('Ctrl Pts',(6.19262035113756,137.651752558102,13.8776767969723));
#79902=CARTESIAN_POINT('Ctrl Pts',(6.18588796045833,137.713321831012,13.9983392664641));
#79903=CARTESIAN_POINT('Ctrl Pts',(6.18399774454713,137.731502086943,14.0308427064663));
#79904=CARTESIAN_POINT('Ctrl Pts',(6.18144287536967,137.756771656705,14.0722321539532));
#79905=CARTESIAN_POINT('Ctrl Pts',(6.18084280882312,137.762753870045,14.0817807944641));
#79906=CARTESIAN_POINT('Ctrl Pts',(6.17983686065803,137.772843056661,14.0974789989223));
#79907=CARTESIAN_POINT('Ctrl Pts',(6.17943512195257,137.77688736565,14.103668089127));
#79908=CARTESIAN_POINT('Ctrl Pts',(6.1785912915681,137.785411422791,14.1164992431133));
#79909=CARTESIAN_POINT('Ctrl Pts',(6.17814875790932,137.789898901364,14.123135317369));
#79910=CARTESIAN_POINT('Ctrl Pts',(6.17695534727235,137.802053652023,14.1407955240577));
#79911=CARTESIAN_POINT('Ctrl Pts',(6.17619840006465,137.80981838798,14.1517512958659));
#79912=CARTESIAN_POINT('Ctrl Pts',(6.17122124626072,137.861314030513,14.2223306466869));
#79913=CARTESIAN_POINT('Ctrl Pts',(6.16677943139859,137.909356331349,14.2786695943109));
#79914=CARTESIAN_POINT('Ctrl Pts',(6.15779942961889,138.014340880967,14.3844099122492));
#79915=CARTESIAN_POINT('Ctrl Pts',(6.15327552512922,138.071262475373,14.4335417597504));
#79916=CARTESIAN_POINT('Ctrl Pts',(6.14627893816397,138.167690663832,14.5046126808137));
#79917=CARTESIAN_POINT('Ctrl Pts',(6.14371871499775,138.204873696299,14.5294735811563));
#79918=CARTESIAN_POINT('Ctrl Pts',(6.14021488458455,138.258534348764,14.561897170226));
#79919=CARTESIAN_POINT('Ctrl Pts',(6.13921978228206,138.274099826181,14.5709149295976));
#79920=CARTESIAN_POINT('Ctrl Pts',(6.13750349103926,138.30150762835,14.5861256092759));
#79921=CARTESIAN_POINT('Ctrl Pts',(6.13677780642107,138.313275611648,14.5924474097258));
#79922=CARTESIAN_POINT('Ctrl Pts',(6.13527897273767,138.337947308381,14.6052690051632));
#79923=CARTESIAN_POINT('Ctrl Pts',(6.13450685801153,138.350864065961,14.6117406380377));
#79924=CARTESIAN_POINT('Ctrl Pts',(6.13247775877977,138.385339650733,14.6283798275873));
#79925=CARTESIAN_POINT('Ctrl Pts',(6.13123207788039,138.407055026696,14.6382139784917));
#79926=CARTESIAN_POINT('Ctrl Pts',(6.12491170941017,138.5198148705,14.6859950683551));
#79927=CARTESIAN_POINT('Ctrl Pts',(6.12012611455855,138.614285280199,14.7151981792919));
#79928=CARTESIAN_POINT('Ctrl Pts',(6.11273338811958,138.762712527666,14.745099194244));
#79929=CARTESIAN_POINT('Ctrl Pts',(6.11014859626989,138.814967612255,14.7527145284675));
#79930=CARTESIAN_POINT('Ctrl Pts',(6.10597138077205,138.897130728009,14.7601829995804));
#79931=CARTESIAN_POINT('Ctrl Pts',(6.10443893358022,138.926818050694,14.7619715003115));
#79932=CARTESIAN_POINT('Ctrl Pts',(6.10228719388142,138.967424482485,14.763177952371));
#79933=CARTESIAN_POINT('Ctrl Pts',(6.10170465908702,138.978314583121,14.7633798595471));
#79934=CARTESIAN_POINT('Ctrl Pts',(6.10070364707831,138.996826051883,14.7635163991386));
#79935=CARTESIAN_POINT('Ctrl Pts',(6.10028843238366,139.004446705273,14.7635130850595));
#79936=CARTESIAN_POINT('Ctrl Pts',(6.09939381986166,139.020733633276,14.7633787894919));
#79937=CARTESIAN_POINT('Ctrl Pts',(6.09891355985767,139.029399208304,14.7632303454761));
#79938=CARTESIAN_POINT('Ctrl Pts',(6.09751943514681,139.054349834836,14.7625812096661));
#79939=CARTESIAN_POINT('Ctrl Pts',(6.09659599328652,139.070628062481,14.7618855398829));
#79940=CARTESIAN_POINT('Ctrl Pts',(6.09213875034915,139.148217445811,14.7572707806052));
#79941=CARTESIAN_POINT('Ctrl Pts',(6.08846890548091,139.209249526039,14.749765524995));
#79942=CARTESIAN_POINT('Ctrl Pts',(6.07999781812186,139.347738764418,14.7238069538988));
#79943=CARTESIAN_POINT('Ctrl Pts',(6.07519974503492,139.424536506281,14.7028253306703));
#79944=CARTESIAN_POINT('Ctrl Pts',(6.06787074379707,139.542373624631,14.6600615069225));
#79945=CARTESIAN_POINT('Ctrl Pts',(6.06524085514309,139.58473675776,14.6423933847799));
#79946=CARTESIAN_POINT('Ctrl Pts',(6.0616640244784,139.642556275291,14.6150213066711));
#79947=CARTESIAN_POINT('Ctrl Pts',(6.06066260232415,139.658764811965,14.6069768810432));
#79948=CARTESIAN_POINT('Ctrl Pts',(6.05894116113815,139.686652140228,14.5924855414837));
#79949=CARTESIAN_POINT('Ctrl Pts',(6.05821649783322,139.698399424661,14.5861758420241));
#79950=CARTESIAN_POINT('Ctrl Pts',(6.05672524454002,139.72258029141,14.5727588224701));
#79951=CARTESIAN_POINT('Ctrl Pts',(6.05595959704273,139.734999109348,14.5656277598967));
#79952=CARTESIAN_POINT('Ctrl Pts',(6.05396171736826,139.7673938598,14.5463885676313));
#79953=CARTESIAN_POINT('Ctrl Pts',(6.0527402946741,139.787188403661,14.5339822905692));
#79954=CARTESIAN_POINT('Ctrl Pts',(6.04547812510897,139.904533117828,14.4564629364915));
#79955=CARTESIAN_POINT('Ctrl Pts',(6.03987724374481,139.994260212743,14.3802937459376));
#79956=CARTESIAN_POINT('Ctrl Pts',(6.03200053668788,140.103737340647,14.2620396483392));
#79957=CARTESIAN_POINT('Ctrl Pts',(6.02983677567864,140.132073434613,14.2285288100749));
#79958=CARTESIAN_POINT('Ctrl Pts',(6.02625469943177,140.175102436962,14.1727392465524));
#79959=CARTESIAN_POINT('Ctrl Pts',(6.02487879924249,140.190766589596,14.1512427953628));
#79960=CARTESIAN_POINT('Ctrl Pts',(6.02291658663522,140.21172554076,14.1207688460803));
#79961=CARTESIAN_POINT('Ctrl Pts',(6.02235987760694,140.21752400669,14.1121425770545));
#79962=CARTESIAN_POINT('Ctrl Pts',(6.02139311240099,140.227328075581,14.097216261855));
#79963=CARTESIAN_POINT('Ctrl Pts',(6.02098592347601,140.23137832815,14.0909458799062));
#79964=CARTESIAN_POINT('Ctrl Pts',(6.02009687029709,140.240047345375,14.0772969830976));
#79965=CARTESIAN_POINT('Ctrl Pts',(6.0196139719613,140.244648443965,14.0699079566835));
#79966=CARTESIAN_POINT('Ctrl Pts',(6.01821519839237,140.257679458185,14.0485589953317));
#79967=CARTESIAN_POINT('Ctrl Pts',(6.01728969379064,140.265942081212,14.0344990069006));
#79968=CARTESIAN_POINT('Ctrl Pts',(6.01255006059004,140.306565857409,13.9626497021191));
#79969=CARTESIAN_POINT('Ctrl Pts',(6.00857620792415,140.335210320654,13.9028524787359));
#79970=CARTESIAN_POINT('Ctrl Pts',(6.00000225040313,140.387852260403,13.7706262959092));
#79971=CARTESIAN_POINT('Ctrl Pts',(5.99541303730799,140.410444327656,13.6978333688117));
#79972=CARTESIAN_POINT('Ctrl Pts',(5.98834762946852,140.437181098722,13.5799115068666));
#79973=CARTESIAN_POINT('Ctrl Pts',(5.98578032340018,140.445077543099,13.5357783877591));
#79974=CARTESIAN_POINT('Ctrl Pts',(5.98227807868768,140.453270160398,13.4736564454145));
#79975=CARTESIAN_POINT('Ctrl Pts',(5.98129068485707,140.455279708766,13.4559221900238));
#79976=CARTESIAN_POINT('Ctrl Pts',(5.9795916161321,140.458208913983,13.425031185483));
#79977=CARTESIAN_POINT('Ctrl Pts',(5.97887539529392,140.459276016412,13.4118908310042));
#79978=CARTESIAN_POINT('Ctrl Pts',(5.97740040596324,140.461121995369,13.3845918454692));
#79979=CARTESIAN_POINT('Ctrl Pts',(5.97664258622784,140.461872950412,13.3704326757375));
#79980=CARTESIAN_POINT('Ctrl Pts',(5.97466377355011,140.463308148105,13.3331292281276));
#79981=CARTESIAN_POINT('Ctrl Pts',(5.97345353028372,140.463649156035,13.3099753526027));
#79982=CARTESIAN_POINT('Ctrl Pts',(5.96618680777581,140.4623814455,13.1691911392114));
#79983=CARTESIAN_POINT('Ctrl Pts',(5.96057870747964,140.447144646371,13.0521207858882));
#79984=CARTESIAN_POINT('Ctrl Pts',(5.95268614726718,140.407153658407,12.8954074642292));
#79985=CARTESIAN_POINT('Ctrl Pts',(5.95051439063421,140.394326073208,12.8531992158087));
#79986=CARTESIAN_POINT('Ctrl Pts',(5.94692175253812,140.370722674627,12.7865202126219));
#79987=CARTESIAN_POINT('Ctrl Pts',(5.94554434879728,140.361148027467,12.7616525051066));
#79988=CARTESIAN_POINT('Ctrl Pts',(5.94358314219853,140.346922785979,12.7275157622443));
#79989=CARTESIAN_POINT('Ctrl Pts',(5.94302944851173,140.342844005569,12.7180127508745));
#79990=CARTESIAN_POINT('Ctrl Pts',(5.94206783464265,140.335663267261,12.7017600353641));
#79991=CARTESIAN_POINT('Ctrl Pts',(5.94166278428657,140.332610072855,12.6949894130177));
#79992=CARTESIAN_POINT('Ctrl Pts',(5.94077624273421,140.325868394609,12.6803380352376));
#79993=CARTESIAN_POINT('Ctrl Pts',(5.94029370723431,140.32216113687,12.6724668369694));
#79994=CARTESIAN_POINT('Ctrl Pts',(5.93890173164414,140.31135175035,12.6500375308205));
#79995=CARTESIAN_POINT('Ctrl Pts',(5.9379828610423,140.304078004894,12.6355640454456));
#79996=CARTESIAN_POINT('Ctrl Pts',(5.93334773284171,140.26662035635,12.5640151742937));
#79997=CARTESIAN_POINT('Ctrl Pts',(5.92947981772648,140.232924584106,12.5088637569139));
#79998=CARTESIAN_POINT('Ctrl Pts',(5.92203714569948,140.161646071081,12.4078684184591));
#79999=CARTESIAN_POINT('Ctrl Pts',(5.91847208025445,140.124699950273,12.3617191890794));
#80000=CARTESIAN_POINT('Ctrl Pts',(5.91258293853601,140.057991392317,12.2880147026651));
#80001=CARTESIAN_POINT('Ctrl Pts',(5.91022534492137,140.029690866555,12.2592324348137));
#80002=CARTESIAN_POINT('Ctrl Pts',(5.90618938801653,139.978268926778,12.2110887822059));
#80003=CARTESIAN_POINT('Ctrl Pts',(5.90449151586008,139.95567243821,12.1912042071751));
#80004=CARTESIAN_POINT('Ctrl Pts',(5.90195692376185,139.920459404514,12.1620940792194));
#80005=CARTESIAN_POINT('Ctrl Pts',(5.90109959087046,139.908282801352,12.1523511951962));
#80006=CARTESIAN_POINT('Ctrl Pts',(5.89953829921091,139.885623926212,12.1348076814118));
#80007=CARTESIAN_POINT('Ctrl Pts',(5.89883210526393,139.875188560566,12.1269493289893));
#80008=CARTESIAN_POINT('Ctrl Pts',(5.89728328217412,139.851896388601,12.1098930156426));
#80009=CARTESIAN_POINT('Ctrl Pts',(5.89644325606804,139.838992869227,12.1007614571737));
#80010=CARTESIAN_POINT('Ctrl Pts',(5.89401723797274,139.800963415186,12.0747630821864));
#80011=CARTESIAN_POINT('Ctrl Pts',(5.8924521932004,139.775458630695,12.0584638664878));
#80012=CARTESIAN_POINT('Ctrl Pts',(5.88500388482994,139.649864501263,11.9835824309555));
#80013=CARTESIAN_POINT('Ctrl Pts',(5.87950877405515,139.543564051749,11.9362489200195));
#80014=CARTESIAN_POINT('Ctrl Pts',(5.87118770458335,139.382060112064,11.8862522972906));
#80015=CARTESIAN_POINT('Ctrl Pts',(5.86852864505822,139.330516332581,11.8733218755028));
#80016=CARTESIAN_POINT('Ctrl Pts',(5.86506664663542,139.265844331865,11.8607910787119));
#80017=CARTESIAN_POINT('Ctrl Pts',(5.86438761144379,139.253268745226,11.8585249053419));
#80018=CARTESIAN_POINT('Ctrl Pts',(5.86327447989685,139.232871245547,11.8551243401695));
#80019=CARTESIAN_POINT('Ctrl Pts',(5.86284580432276,139.225066750608,11.8538880952062));
#80020=CARTESIAN_POINT('Ctrl Pts',(5.86203363893271,139.210386569871,11.8516844443037));
#80021=CARTESIAN_POINT('Ctrl Pts',(5.86165098199122,139.203513232919,11.8507026470455));
#80022=CARTESIAN_POINT('Ctrl Pts',(5.86060846822576,139.184895108791,11.848178259011));
#80023=CARTESIAN_POINT('Ctrl Pts',(5.85994371603298,139.173138379242,11.8467293259645));
#80024=CARTESIAN_POINT('Ctrl Pts',(5.85720491314605,139.125101023145,11.8414002262686));
#80025=CARTESIAN_POINT('Ctrl Pts',(5.85507721592598,139.08870099091,11.8387350276837));
#80026=CARTESIAN_POINT('Ctrl Pts',(5.84669517950804,138.947196026553,11.8336805326472));
#80027=CARTESIAN_POINT('Ctrl Pts',(5.84025725618538,138.842049281319,11.8412556799315));
#80028=CARTESIAN_POINT('Ctrl Pts',(5.83101251125895,138.68746545757,11.8693159357432));
#80029=CARTESIAN_POINT('Ctrl Pts',(5.82801624564579,138.636843277737,11.8813200415955));
#80030=CARTESIAN_POINT('Ctrl Pts',(5.82405237315119,138.568964275335,11.9012890073804));
#80031=CARTESIAN_POINT('Ctrl Pts',(5.82301232399686,138.551068577809,11.9069296998691));
#80032=CARTESIAN_POINT('Ctrl Pts',(5.82124931482719,138.52059744695,11.917182347678));
#80033=CARTESIAN_POINT('Ctrl Pts',(5.82052095254888,138.50796811122,11.9216255572136));
#80034=CARTESIAN_POINT('Ctrl Pts',(5.81904329849012,138.48227281332,11.9310637637119));
#80035=CARTESIAN_POINT('Ctrl Pts',(5.81829460477804,138.469213916878,11.9360740447966));
#80036=CARTESIAN_POINT('Ctrl Pts',(5.81638724512933,138.435862584686,11.9494214461254));
#80037=CARTESIAN_POINT('Ctrl Pts',(5.81523771369553,138.415681825091,11.9580291395752));
#80038=CARTESIAN_POINT('Ctrl Pts',(5.80798446849508,138.288089788978,12.015875160176));
#80039=CARTESIAN_POINT('Ctrl Pts',(5.80233787926683,138.186785184517,12.0775124080618));
#80040=CARTESIAN_POINT('Ctrl Pts',(5.79437664164933,138.058724127397,12.1784615884725));
#80041=CARTESIAN_POINT('Ctrl Pts',(5.79216520176852,138.024758791509,12.2078677498098));
#80042=CARTESIAN_POINT('Ctrl Pts',(5.78851500752631,137.972645537959,12.2573579937815));
#80043=CARTESIAN_POINT('Ctrl Pts',(5.78712095805331,137.953608394412,12.2764649578319));
#80044=CARTESIAN_POINT('Ctrl Pts',(5.78513817249175,137.927960755744,12.3036703544242));
#80045=CARTESIAN_POINT('Ctrl Pts',(5.78458007238846,137.920891861777,12.3113309364265));
#80046=CARTESIAN_POINT('Ctrl Pts',(5.78361218002465,137.908904649935,12.3246032315321));
#80047=CARTESIAN_POINT('Ctrl Pts',(5.78320531060899,137.903946411247,12.330178136015));
#80048=CARTESIAN_POINT('Ctrl Pts',(5.78231719941338,137.893301895956,12.3423324337592));
#80049=CARTESIAN_POINT('Ctrl Pts',(5.7818349476132,137.887631562945,12.348924654229));
#80050=CARTESIAN_POINT('Ctrl Pts',(5.78044402150243,137.871576333891,12.3679301469697));
#80051=CARTESIAN_POINT('Ctrl Pts',(5.77952592971365,137.86133843644,12.3804653454155));
#80052=CARTESIAN_POINT('Ctrl Pts',(5.77490422749186,137.811441086024,12.4436705353262));
#80053=CARTESIAN_POINT('Ctrl Pts',(5.77104989921061,137.774948046035,12.4967447758345));
#80054=CARTESIAN_POINT('Ctrl Pts',(5.76372100027898,137.712736949158,12.6013728939457));
#80055=CARTESIAN_POINT('Ctrl Pts',(5.76025635280797,137.686331842526,12.6523871454748));
#80056=CARTESIAN_POINT('Ctrl Pts',(5.75320684658108,137.637995404598,12.760970174725));
#80057=CARTESIAN_POINT('Ctrl Pts',(5.74963844029193,137.616560165947,12.8186421958136));
#80058=CARTESIAN_POINT('Ctrl Pts',(5.74508335810925,137.593140617498,12.8963106942074));
#80059=CARTESIAN_POINT('Ctrl Pts',(5.74399201146777,137.587847054098,12.9152371014115));
#80060=CARTESIAN_POINT('Ctrl Pts',(5.74216973223066,137.579553863482,12.9473696099917));
#80061=CARTESIAN_POINT('Ctrl Pts',(5.74143244174944,137.576353529733,12.9605207463537));
#80062=CARTESIAN_POINT('Ctrl Pts',(5.73995852077226,137.570273212558,12.9871065891242));
#80063=CARTESIAN_POINT('Ctrl Pts',(5.73922214162866,137.567399065723,13.0005412315861));
#80064=CARTESIAN_POINT('Ctrl Pts',(5.73738955708814,137.560664290573,13.034341306802));
#80065=CARTESIAN_POINT('Ctrl Pts',(5.73630108586578,137.557046276954,13.0547522980622));
#80066=CARTESIAN_POINT('Ctrl Pts',(5.73131828483472,137.542305501869,13.1495939443217));
#80067=CARTESIAN_POINT('Ctrl Pts',(5.72759032558515,137.536500000002,13.2247384293328));
#80068=CARTESIAN_POINT('Ctrl Pts',(5.72391728548022,137.5365,13.299999999962));
#80069=CARTESIAN_POINT('Ctrl Pts',(5.6533662680412,137.5365,13.3000000000336));
#80070=CARTESIAN_POINT('Ctrl Pts',(5.65697576249153,137.536499999999,13.2393933779925));
#80071=CARTESIAN_POINT('Ctrl Pts',(5.66051905483574,137.540264715002,13.1788398257535));
#80072=CARTESIAN_POINT('Ctrl Pts',(5.66493101344803,137.549915832198,13.1015388318754));
#80073=CARTESIAN_POINT('Ctrl Pts',(5.66590078546337,137.552360588956,13.0844284336989));
#80074=CARTESIAN_POINT('Ctrl Pts',(5.66757947452231,137.557162490758,13.0546039247781));
#80075=CARTESIAN_POINT('Ctrl Pts',(5.6682924378738,137.559386067369,13.0418705285407));
#80076=CARTESIAN_POINT('Ctrl Pts',(5.66972008679681,137.564211833059,13.0162438632421));
#80077=CARTESIAN_POINT('Ctrl Pts',(5.67043451871115,137.566819723821,13.0033528742392));
#80078=CARTESIAN_POINT('Ctrl Pts',(5.67190907110246,137.57260468111,12.9766169900121));
#80079=CARTESIAN_POINT('Ctrl Pts',(5.67266819879496,137.575810260272,12.9627796387201));
#80080=CARTESIAN_POINT('Ctrl Pts',(5.67465794725342,137.584813131011,12.9263386360229));
#80081=CARTESIAN_POINT('Ctrl Pts',(5.67587763759821,137.590950535077,12.9038228006479));
#80082=CARTESIAN_POINT('Ctrl Pts',(5.68297053624817,137.630250783349,12.7721411094394));
#80083=CARTESIAN_POINT('Ctrl Pts',(5.68842942902264,137.675546905034,12.6670123508193));
#80084=CARTESIAN_POINT('Ctrl Pts',(5.69622892650164,137.7554690448,12.5285939362078));
#80085=CARTESIAN_POINT('Ctrl Pts',(5.69847955861117,137.780185076684,12.4900767073825));
#80086=CARTESIAN_POINT('Ctrl Pts',(5.70218479769977,137.822438041925,12.43056185106));
#80087=CARTESIAN_POINT('Ctrl Pts',(5.70359287116361,137.838830172965,12.4087877251487));
#80088=CARTESIAN_POINT('Ctrl Pts',(5.70559029422991,137.862318361711,12.3793364475598));
#80089=CARTESIAN_POINT('Ctrl Pts',(5.70614826520265,137.868903880071,12.3712576020478));
#80090=CARTESIAN_POINT('Ctrl Pts',(5.70711386780697,137.88032586865,12.3575472518085));
#80091=CARTESIAN_POINT('Ctrl Pts',(5.70751854574648,137.885119830445,12.3518810469976));
#80092=CARTESIAN_POINT('Ctrl Pts',(5.70839898750365,137.895560418243,12.3397295209064));
#80093=CARTESIAN_POINT('Ctrl Pts',(5.7088757020187,137.901221147062,12.3332574243764));
#80094=CARTESIAN_POINT('Ctrl Pts',(5.71024272975254,137.917486988537,12.314987572934));
#80095=CARTESIAN_POINT('Ctrl Pts',(5.71114204658586,137.928227066828,12.3033121653655));
#80096=CARTESIAN_POINT('Ctrl Pts',(5.71673256266189,137.995382236531,12.2326493314217));
#80097=CARTESIAN_POINT('Ctrl Pts',(5.72167012102453,138.056457438729,12.1782959172463));
#80098=CARTESIAN_POINT('Ctrl Pts',(5.73056645239369,138.174619641106,12.0896489629321));
#80099=CARTESIAN_POINT('Ctrl Pts',(5.73452429668179,138.230130455645,12.0536034102975));
#80100=CARTESIAN_POINT('Ctrl Pts',(5.74078273043686,138.324086738216,12.0012737112748));
#80101=CARTESIAN_POINT('Ctrl Pts',(5.74314875636077,138.361123529924,11.9826594833613));
#80102=CARTESIAN_POINT('Ctrl Pts',(5.7464311898699,138.414743363113,11.9585050307912));
#80103=CARTESIAN_POINT('Ctrl Pts',(5.74739137224624,138.430709932742,11.9516517736723));
#80104=CARTESIAN_POINT('Ctrl Pts',(5.74905892724868,138.458927140236,11.940130841145));
#80105=CARTESIAN_POINT('Ctrl Pts',(5.74977036242739,138.47112527388,11.9353405155711));
#80106=CARTESIAN_POINT('Ctrl Pts',(5.75124961530128,138.496815553994,11.925647906543));
#80107=CARTESIAN_POINT('Ctrl Pts',(5.75201626322393,138.510318837146,11.9207789727201));
#80108=CARTESIAN_POINT('Ctrl Pts',(5.75405179314551,138.546657799159,11.9082770642428));
#80109=CARTESIAN_POINT('Ctrl Pts',(5.75530877724265,138.569614267595,11.9010074738027));
#80110=CARTESIAN_POINT('Ctrl Pts',(5.76165962002447,138.687977340127,11.866715142009));
#80111=CARTESIAN_POINT('Ctrl Pts',(5.76645666101301,138.785771727214,11.84887228459));
#80112=CARTESIAN_POINT('Ctrl Pts',(5.77395428176452,138.939499799882,11.8367153341214));
#80113=CARTESIAN_POINT('Ctrl Pts',(5.77663737081935,138.994572709531,11.8354754283577));
#80114=CARTESIAN_POINT('Ctrl Pts',(5.78095528113385,139.080040614718,11.8383726249417));
#80115=CARTESIAN_POINT('Ctrl Pts',(5.7825227818539,139.110458335318,11.8403562744335));
#80116=CARTESIAN_POINT('Ctrl Pts',(5.78470946486359,139.151580241848,11.8443306698612));
#80117=CARTESIAN_POINT('Ctrl Pts',(5.78528892739312,139.162358312024,11.8454933713165));
#80118=CARTESIAN_POINT('Ctrl Pts',(5.78627937891608,139.180554097086,11.8476610292999));
#80119=CARTESIAN_POINT('Ctrl Pts',(5.78668700117038,139.187979010471,11.8486033766396));
#80120=CARTESIAN_POINT('Ctrl Pts',(5.787558896572,139.203718181919,11.8507237458842));
#80121=CARTESIAN_POINT('Ctrl Pts',(5.78802389826536,139.212029921588,11.8519164169021));
#80122=CARTESIAN_POINT('Ctrl Pts',(5.78934811970957,139.235485320512,11.8554883518329));
#80123=CARTESIAN_POINT('Ctrl Pts',(5.79021574391387,139.250602122528,11.8580340585846));
#80124=CARTESIAN_POINT('Ctrl Pts',(5.79727733072901,139.371908243837,11.8804273599112));
#80125=CARTESIAN_POINT('Ctrl Pts',(5.80390257703309,139.475638444459,11.9117388218285));
#80126=CARTESIAN_POINT('Ctrl Pts',(5.8133645079529,139.621144096273,11.9739031131033));
#80127=CARTESIAN_POINT('Ctrl Pts',(5.81632986685041,139.666270649019,11.9959919421423));
#80128=CARTESIAN_POINT('Ctrl Pts',(5.82124112551004,139.740687077363,12.0372915602315));
#80129=CARTESIAN_POINT('Ctrl Pts',(5.82322093362158,139.770584946117,12.055311654391));
#80130=CARTESIAN_POINT('Ctrl Pts',(5.82607342195843,139.813518275877,12.0833290766765));
#80131=CARTESIAN_POINT('Ctrl Pts',(5.82697559271159,139.827074062998,12.0925031487259));
#80132=CARTESIAN_POINT('Ctrl Pts',(5.82857240202151,139.851016516525,12.1092989483834));
#80133=CARTESIAN_POINT('Ctrl Pts',(5.82927021660863,139.86146166295,12.1168339407565));
#80134=CARTESIAN_POINT('Ctrl Pts',(5.83076286949335,139.883756579928,12.1333689868138));
#80135=CARTESIAN_POINT('Ctrl Pts',(5.83155586106612,139.895571362298,12.1424139036313));
#80136=CARTESIAN_POINT('Ctrl Pts',(5.83371479382208,139.927631320412,12.1677423930271));
#80137=CARTESIAN_POINT('Ctrl Pts',(5.83506635647265,139.947584462736,12.1843876357522));
#80138=CARTESIAN_POINT('Ctrl Pts',(5.84219773149226,140.051889601134,12.2762192644865));
#80139=CARTESIAN_POINT('Ctrl Pts',(5.84758776100299,140.127760627587,12.3604492426307));
#80140=CARTESIAN_POINT('Ctrl Pts',(5.85521029515537,140.218040440163,12.4875642707814));
#80141=CARTESIAN_POINT('Ctrl Pts',(5.8573289085875,140.241340057753,12.523631005899));
#80142=CARTESIAN_POINT('Ctrl Pts',(5.86084302808322,140.276243026866,12.5832565921059));
#80143=CARTESIAN_POINT('Ctrl Pts',(5.86219769897589,140.288856966002,12.6061953146103));
#80144=CARTESIAN_POINT('Ctrl Pts',(5.86413144545184,140.3055553693,12.6385901644603));
#80145=CARTESIAN_POINT('Ctrl Pts',(5.86468172313351,140.310165985271,12.6477708441284));
#80146=CARTESIAN_POINT('Ctrl Pts',(5.8656385614609,140.31793176553,12.6636487543553));
#80147=CARTESIAN_POINT('Ctrl Pts',(5.86604232001495,140.321133403085,12.6703226413633));
#80148=CARTESIAN_POINT('Ctrl Pts',(5.86692632877688,140.327978043523,12.684872487048));
#80149=CARTESIAN_POINT('Ctrl Pts',(5.86740762163779,140.331601675158,12.6927566285216));
#80150=CARTESIAN_POINT('Ctrl Pts',(5.86880146119969,140.341810418521,12.7154992016563));
#80151=CARTESIAN_POINT('Ctrl Pts',(5.86972354831471,140.348218232883,12.7304353112508));
#80152=CARTESIAN_POINT('Ctrl Pts',(5.87444010108554,140.379350713558,12.8064734133424));
#80153=CARTESIAN_POINT('Ctrl Pts',(5.87839261959991,140.40017448443,12.8690857994544));
#80154=CARTESIAN_POINT('Ctrl Pts',(5.88593417453586,140.43158689687,12.9903064563344));
#80155=CARTESIAN_POINT('Ctrl Pts',(5.88951340184243,140.442962802065,13.0485839523468));
#80156=CARTESIAN_POINT('Ctrl Pts',(5.89535748610721,140.455959657195,13.1464797876939));
#80157=CARTESIAN_POINT('Ctrl Pts',(5.89765902870917,140.459567455845,13.1857626298503));
#80158=CARTESIAN_POINT('Ctrl Pts',(5.90160904877756,140.463096435683,13.254668406482));
#80159=CARTESIAN_POINT('Ctrl Pts',(5.90327601833361,140.463713656544,13.2842316146644));
#80160=CARTESIAN_POINT('Ctrl Pts',(5.90577059080835,140.463289659303,13.3292117398176));
#80161=CARTESIAN_POINT('Ctrl Pts',(5.90661803458687,140.462900719914,13.3446258007389));
#80162=CARTESIAN_POINT('Ctrl Pts',(5.90816360619895,140.461736870412,13.3729753634333));
#80163=CARTESIAN_POINT('Ctrl Pts',(5.90886389101222,140.461033609066,13.3859121071203));
#80164=CARTESIAN_POINT('Ctrl Pts',(5.91040205680386,140.459097131236,13.4145201511361));
#80165=CARTESIAN_POINT('Ctrl Pts',(5.91123733109681,140.457783020476,13.430184462665));
#80166=CARTESIAN_POINT('Ctrl Pts',(5.91365503742473,140.45320842033,13.4758666851387));
#80167=CARTESIAN_POINT('Ctrl Pts',(5.91521651274233,140.449271028005,13.5058092617556));
#80168=CARTESIAN_POINT('Ctrl Pts',(5.92320795417005,140.424011930144,13.6606604578252));
#80169=CARTESIAN_POINT('Ctrl Pts',(5.92915707016481,140.387463903187,13.782522653517));
#80170=CARTESIAN_POINT('Ctrl Pts',(5.93763254924681,140.317623140847,13.9384775904453));
#80171=CARTESIAN_POINT('Ctrl Pts',(5.93986629223164,140.297749527945,13.9779601173162));
#80172=CARTESIAN_POINT('Ctrl Pts',(5.94283266149028,140.270171550407,14.0270792535848));
#80173=CARTESIAN_POINT('Ctrl Pts',(5.94347967245631,140.264088954362,14.0376036229821));
#80174=CARTESIAN_POINT('Ctrl Pts',(5.94455098484331,140.253927321835,14.0546908019192));
#80175=CARTESIAN_POINT('Ctrl Pts',(5.94497051413286,140.2499260164,14.0612994712912));
#80176=CARTESIAN_POINT('Ctrl Pts',(5.94582876313332,140.241702163078,14.0746426060735));
#80177=CARTESIAN_POINT('Ctrl Pts',(5.94626763921887,140.237476741196,14.0813749022207));
#80178=CARTESIAN_POINT('Ctrl Pts',(5.94744401771789,140.226090987063,14.0991916378737));
#80179=CARTESIAN_POINT('Ctrl Pts',(5.94818731514329,140.218835366291,14.1102139887132));
#80180=CARTESIAN_POINT('Ctrl Pts',(5.95261557662548,140.175181980069,14.1746163373711));
#80181=CARTESIAN_POINT('Ctrl Pts',(5.95647032850294,140.135433269071,14.2256329228595));
#80182=CARTESIAN_POINT('Ctrl Pts',(5.96660487842762,140.023307145018,14.3514138633291));
#80183=CARTESIAN_POINT('Ctrl Pts',(5.97288412030695,139.946092433288,14.4214021463712));
#80184=CARTESIAN_POINT('Ctrl Pts',(5.98061089440359,139.837237049878,14.5007554754419));
#80185=CARTESIAN_POINT('Ctrl Pts',(5.9823490665748,139.811798316072,14.5180982235904));
#80186=CARTESIAN_POINT('Ctrl Pts',(5.98492633364281,139.772625888458,14.5430311633009));
#80187=CARTESIAN_POINT('Ctrl Pts',(5.98578729338112,139.759287312848,14.5512234172284));
#80188=CARTESIAN_POINT('Ctrl Pts',(5.98734728210769,139.734662029811,14.5658088773062));
#80189=CARTESIAN_POINT('Ctrl Pts',(5.98804868636133,139.723416975461,14.5722689599892));
#80190=CARTESIAN_POINT('Ctrl Pts',(5.9895774872314,139.698534343617,14.5861270066639));
#80191=CARTESIAN_POINT('Ctrl Pts',(5.99040249398316,139.684861915198,14.5934593493193));
#80192=CARTESIAN_POINT('Ctrl Pts',(5.99275371047503,139.645218577311,14.6139146836974));
#80193=CARTESIAN_POINT('Ctrl Pts',(5.99426080569329,139.618968931615,14.6264827237329));
#80194=CARTESIAN_POINT('Ctrl Pts',(5.99774695640422,139.55650277023,14.6541324303148));
#80195=CARTESIAN_POINT('Ctrl Pts',(5.99970622901512,139.52001994584,14.6685574454841));
#80196=CARTESIAN_POINT('Ctrl Pts',(6.0045889324306,139.426584480367,14.701224360436));
#80197=CARTESIAN_POINT('Ctrl Pts',(6.00747351366385,139.36901276103,14.717474417418));
#80198=CARTESIAN_POINT('Ctrl Pts',(6.01359016967776,139.246345875599,14.7441158223409));
#80199=CARTESIAN_POINT('Ctrl Pts',(6.01682155523195,139.181220397575,14.753724342107));
#80200=CARTESIAN_POINT('Ctrl Pts',(6.02108275488072,139.09947871777,14.7602055484217));
#80201=CARTESIAN_POINT('Ctrl Pts',(6.02193827720658,139.083261583861,14.7612199440886));
#80202=CARTESIAN_POINT('Ctrl Pts',(6.02327211548137,139.058356607022,14.7623618464705));
#80203=CARTESIAN_POINT('Ctrl Pts',(6.02374061167786,139.049678472142,14.7626823665254));
#80204=CARTESIAN_POINT('Ctrl Pts',(6.02461742149734,139.033580154739,14.7631335189008));
#80205=CARTESIAN_POINT('Ctrl Pts',(6.02502462531589,139.026161067507,14.7632849725592));
#80206=CARTESIAN_POINT('Ctrl Pts',(6.02600531581143,139.008424122384,14.7635121267794));
#80207=CARTESIAN_POINT('Ctrl Pts',(6.02658155015462,138.99810616258,14.7635351420108));
#80208=CARTESIAN_POINT('Ctrl Pts',(6.02865032523758,138.96139198578,14.7632288027181));
#80209=CARTESIAN_POINT('Ctrl Pts',(6.03017080556315,138.935007142182,14.762294385749));
#80210=CARTESIAN_POINT('Ctrl Pts',(6.03425517211736,138.865257064081,14.7579328145923));
#80211=CARTESIAN_POINT('Ctrl Pts',(6.03685460391053,138.821994932134,14.7532851057885));
#80212=CARTESIAN_POINT('Ctrl Pts',(6.04641928212429,138.664694571314,14.729256652979));
#80213=CARTESIAN_POINT('Ctrl Pts',(6.05339910789472,138.552835589036,14.6983047196228));
#80214=CARTESIAN_POINT('Ctrl Pts',(6.06131903926754,138.423527407056,14.6453957206966));
#80215=CARTESIAN_POINT('Ctrl Pts',(6.06266448652038,138.401502376958,14.635743608258));
#80216=CARTESIAN_POINT('Ctrl Pts',(6.06478431823162,138.366719099659,14.619467209964));
#80217=CARTESIAN_POINT('Ctrl Pts',(6.06557031596723,138.353803951958,14.613190429847));
#80218=CARTESIAN_POINT('Ctrl Pts',(6.06706229219365,138.329262805641,14.6008136549379));
#80219=CARTESIAN_POINT('Ctrl Pts',(6.06776927869749,138.317622478903,14.5947453351638));
#80220=CARTESIAN_POINT('Ctrl Pts',(6.06940245757921,138.290718831501,14.5802563368812));
#80221=CARTESIAN_POINT('Ctrl Pts',(6.0703243842096,138.275521031118,14.5717178626686));
#80222=CARTESIAN_POINT('Ctrl Pts',(6.0734228321803,138.224465170957,14.5418211215038));
#80223=CARTESIAN_POINT('Ctrl Pts',(6.07555433134893,138.189368282953,14.5192007934152));
#80224=CARTESIAN_POINT('Ctrl Pts',(6.08100162206062,138.100656327443,14.4564982730705));
#80225=CARTESIAN_POINT('Ctrl Pts',(6.08424755849882,138.048738442852,14.4141854724613));
#80226=CARTESIAN_POINT('Ctrl Pts',(6.09141875441242,137.941001027503,14.3133415492535));
#80227=CARTESIAN_POINT('Ctrl Pts',(6.09533386832001,137.886770008277,14.2534444714429));
#80228=CARTESIAN_POINT('Ctrl Pts',(6.10035156963313,137.828166169026,14.1768618397456));
#80229=CARTESIAN_POINT('Ctrl Pts',(6.1011832123673,137.81878092496,14.1641774533306));
#80230=CARTESIAN_POINT('Ctrl Pts',(6.10248718083329,137.804611665318,14.1443652056503));
#80231=CARTESIAN_POINT('Ctrl Pts',(6.10295033497054,137.799681960186,14.137342502853));
#80232=CARTESIAN_POINT('Ctrl Pts',(6.10382039045731,137.79062011418,14.1241888135682));
#80233=CARTESIAN_POINT('Ctrl Pts',(6.10422625624439,137.786472267466,14.1180692774802));
#80234=CARTESIAN_POINT('Ctrl Pts',(6.10520919734878,137.776613695097,14.1032844423948));
#80235=CARTESIAN_POINT('Ctrl Pts',(6.10578912543287,137.770948544979,14.0945894880172));
#80236=CARTESIAN_POINT('Ctrl Pts',(6.10790681526746,137.750782483832,14.0629066492488));
#80237=CARTESIAN_POINT('Ctrl Pts',(6.10947463367642,137.736830872648,14.0395772661838));
#80238=CARTESIAN_POINT('Ctrl Pts',(6.1137346422948,137.701240172514,13.9761161658724));
#80239=CARTESIAN_POINT('Ctrl Pts',(6.11646629783227,137.680813312742,13.9353394864149));
#80240=CARTESIAN_POINT('Ctrl Pts',(6.12629454618935,137.614609778026,13.7861696165259));
#80241=CARTESIAN_POINT('Ctrl Pts',(6.13338760801281,137.580022259446,13.6732811597668));
#80242=CARTESIAN_POINT('Ctrl Pts',(6.14127450084188,137.555452133638,13.5357925116783));
#80243=CARTESIAN_POINT('Ctrl Pts',(6.14250239594808,137.552069405187,13.5140413837613));
#80244=CARTESIAN_POINT('Ctrl Pts',(6.14448003346254,137.547354132912,13.4784521085903));
#80245=CARTESIAN_POINT('Ctrl Pts',(6.14523895209424,137.54572589518,13.4646572715126));
#80246=CARTESIAN_POINT('Ctrl Pts',(6.1467063820322,137.542935031073,13.4377237655496));
#80247=CARTESIAN_POINT('Ctrl Pts',(6.14741543291234,137.541753146379,13.4245884781647));
#80248=CARTESIAN_POINT('Ctrl Pts',(6.1490947416746,137.539356311365,13.3932027575419));
#80249=CARTESIAN_POINT('Ctrl Pts',(6.15005978637313,137.538305604865,13.3749418047271));
#80250=CARTESIAN_POINT('Ctrl Pts',(6.15200166140935,137.536865783236,13.337783340469));
#80251=CARTESIAN_POINT('Ctrl Pts',(6.15297747730672,137.536500000168,13.3188913700656));
#80252=CARTESIAN_POINT('Ctrl Pts',(6.1539436045687,137.5365,13.30000001305));
#80253=CARTESIAN_POINT('Origin',(1.13913288526384,139.,13.3));
#80254=CARTESIAN_POINT('',(2.4607468847319,137.88614821265,13.6826607614027));
#80255=CARTESIAN_POINT('',(2.36281348338426,137.886148197203,13.6826607164382));
#80256=CARTESIAN_POINT('',(1.13913288526384,137.88614821265,13.6826607614027));
#80257=CARTESIAN_POINT('',(2.06349999999998,138.327116518419,12.3333962121348));
#80258=CARTESIAN_POINT('Ctrl Pts',(2.46074688473191,137.88614821265,13.6826607614027));
#80259=CARTESIAN_POINT('Ctrl Pts',(2.45928397525449,137.89272897163,13.701816083534));
#80260=CARTESIAN_POINT('Ctrl Pts',(2.45783385173158,137.899805886111,13.7208075478205));
#80261=CARTESIAN_POINT('Ctrl Pts',(2.45549200100449,137.91219985181,13.7516116641803));
#80262=CARTESIAN_POINT('Ctrl Pts',(2.45458867175444,137.917223828975,13.7635278372366));
#80263=CARTESIAN_POINT('Ctrl Pts',(2.45315465607098,137.92560881407,13.7825351313431));
#80264=CARTESIAN_POINT('Ctrl Pts',(2.45261724523232,137.92884607051,13.7896793272959));
#80265=CARTESIAN_POINT('Ctrl Pts',(2.45154083877098,137.935527919108,13.8040418697068));
#80266=CARTESIAN_POINT('Ctrl Pts',(2.45100202155896,137.938975128628,13.8112584954435));
#80267=CARTESIAN_POINT('Ctrl Pts',(2.44955373087507,137.948511270729,13.8307101520025));
#80268=CARTESIAN_POINT('Ctrl Pts',(2.44865230826454,137.954740264935,13.8428756203764));
#80269=CARTESIAN_POINT('Ctrl Pts',(2.44661626077223,137.969445941233,13.870404383881));
#80270=CARTESIAN_POINT('Ctrl Pts',(2.44548826582058,137.978057098827,13.8856924102223));
#80271=CARTESIAN_POINT('Ctrl Pts',(2.44158744149147,138.009328372448,13.9384195598443));
#80272=CARTESIAN_POINT('Ctrl Pts',(2.4388772983383,138.033731260977,13.9747851473174));
#80273=CARTESIAN_POINT('Ctrl Pts',(2.43142808267214,138.106345354465,14.0709508714327));
#80274=CARTESIAN_POINT('Ctrl Pts',(2.42670574502547,138.158457623931,14.1275197170264));
#80275=CARTESIAN_POINT('Ctrl Pts',(2.42038367873486,138.23155745979,14.1927726647626));
#80276=CARTESIAN_POINT('Ctrl Pts',(2.41899696075887,138.247795763608,14.2064963677247));
#80277=CARTESIAN_POINT('Ctrl Pts',(2.41668526924672,138.275120239638,14.2283495983067));
#80278=CARTESIAN_POINT('Ctrl Pts',(2.41577079766173,138.285993514856,14.2367381469551));
#80279=CARTESIAN_POINT('Ctrl Pts',(2.41394526472066,138.307806678174,14.2529661761489));
#80280=CARTESIAN_POINT('Ctrl Pts',(2.41303464185118,138.318739201053,14.26081206558));
#80281=CARTESIAN_POINT('Ctrl Pts',(2.41077065550203,138.3460298843,14.2796976784835));
#80282=CARTESIAN_POINT('Ctrl Pts',(2.40940928043307,138.362535135864,14.2905164907587));
#80283=CARTESIAN_POINT('Ctrl Pts',(2.40291109855419,138.441712771649,14.3396168407627));
#80284=CARTESIAN_POINT('Ctrl Pts',(2.39758344690424,138.507595105554,14.3723907901521));
#80285=CARTESIAN_POINT('Ctrl Pts',(2.38723026835388,138.639206968591,14.4231653422949));
#80286=CARTESIAN_POINT('Ctrl Pts',(2.38223621736652,138.704310978394,14.4420338633483));
#80287=CARTESIAN_POINT('Ctrl Pts',(2.37648601230282,138.784121255699,14.4578770429948));
#80288=CARTESIAN_POINT('Ctrl Pts',(2.37552695144948,138.797609866748,14.4603108004324));
#80289=CARTESIAN_POINT('Ctrl Pts',(2.37402629816139,138.819043497177,14.4637929125631));
#80290=CARTESIAN_POINT('Ctrl Pts',(2.37347693170749,138.826961589692,14.4649965310344));
#80291=CARTESIAN_POINT('Ctrl Pts',(2.37239730849052,138.842676950449,14.4672216356913));
#80292=CARTESIAN_POINT('Ctrl Pts',(2.37186693858509,138.850473348529,14.4682459830209));
#80293=CARTESIAN_POINT('Ctrl Pts',(2.37047294911137,138.871147787263,14.4707519768697));
#80294=CARTESIAN_POINT('Ctrl Pts',(2.36961633097778,138.884041448505,14.4720992845166));
#80295=CARTESIAN_POINT('Ctrl Pts',(2.36481160582904,138.957245402524,14.478528758298));
#80296=CARTESIAN_POINT('Ctrl Pts',(2.36105569286795,139.017861469534,14.4791694998175));
#80297=CARTESIAN_POINT('Ctrl Pts',(2.35243766820181,139.156865156438,14.4699119157188));
#80298=CARTESIAN_POINT('Ctrl Pts',(2.34759513308405,139.234734817817,14.4568053851832));
#80299=CARTESIAN_POINT('Ctrl Pts',(2.34115013904538,139.331043419698,14.4304643649378));
#80300=CARTESIAN_POINT('Ctrl Pts',(2.33977452344838,139.351222484418,14.4243585300967));
#80301=CARTESIAN_POINT('Ctrl Pts',(2.33747566698884,139.384234683821,14.4133942098578));
#80302=CARTESIAN_POINT('Ctrl Pts',(2.3365626471314,139.397166569647,14.408846990365));
#80303=CARTESIAN_POINT('Ctrl Pts',(2.33473554987574,139.422669961128,14.3993759050918));
#80304=CARTESIAN_POINT('Ctrl Pts',(2.3338218382357,139.435242012673,14.3944595199405));
#80305=CARTESIAN_POINT('Ctrl Pts',(2.33154125650734,139.466155997043,14.3817535201762));
#80306=CARTESIAN_POINT('Ctrl Pts',(2.33016612931047,139.484389400856,14.3737126785111));
#80307=CARTESIAN_POINT('Ctrl Pts',(2.32376092596492,139.567412600211,14.3345546976335));
#80308=CARTESIAN_POINT('Ctrl Pts',(2.31854969547642,139.629463176611,14.2980148119132));
#80309=CARTESIAN_POINT('Ctrl Pts',(2.30820956986678,139.743847341394,14.2157266188255));
#80310=CARTESIAN_POINT('Ctrl Pts',(2.30310767114884,139.796254528154,14.1705424760453));
#80311=CARTESIAN_POINT('Ctrl Pts',(2.29726318606867,139.853912515423,14.1112426106492));
#80312=CARTESIAN_POINT('Ctrl Pts',(2.29630860946709,139.863252149824,14.1012970256901));
#80313=CARTESIAN_POINT('Ctrl Pts',(2.29481358382522,139.877785594431,14.0852715259833));
#80314=CARTESIAN_POINT('Ctrl Pts',(2.29426543952778,139.883093650073,14.0792974618079));
#80315=CARTESIAN_POINT('Ctrl Pts',(2.29319136909778,139.893461453587,14.0673868145198));
#80316=CARTESIAN_POINT('Ctrl Pts',(2.29266530742886,139.8985237803,14.0614531596122));
#80317=CARTESIAN_POINT('Ctrl Pts',(2.29128354858555,139.91176582025,14.0456159358502));
#80318=CARTESIAN_POINT('Ctrl Pts',(2.29043477776658,139.919843404728,14.0356277450894));
#80319=CARTESIAN_POINT('Ctrl Pts',(2.28853886649562,139.937707459874,14.0127837924098));
#80320=CARTESIAN_POINT('Ctrl Pts',(2.28749714922217,139.947396187672,13.9998546496914));
#80321=CARTESIAN_POINT('Ctrl Pts',(2.28405353974228,139.978854665698,13.9560237398922));
#80322=CARTESIAN_POINT('Ctrl Pts',(2.28170046311129,139.999403565874,13.9242727565533));
#80323=CARTESIAN_POINT('Ctrl Pts',(2.27388012267663,140.062867599536,13.81502216255));
#80324=CARTESIAN_POINT('Ctrl Pts',(2.26847548926846,140.098564180645,13.7336941031766));
#80325=CARTESIAN_POINT('Ctrl Pts',(2.26145351050725,140.130757100884,13.6299785591863));
#80326=CARTESIAN_POINT('Ctrl Pts',(2.26014254050079,140.13621304909,13.6106723356718));
#80327=CARTESIAN_POINT('Ctrl Pts',(2.25801419572744,140.144169297777,13.5794968534091));
#80328=CARTESIAN_POINT('Ctrl Pts',(2.25720705160607,140.146984056923,13.5677114633326));
#80329=CARTESIAN_POINT('Ctrl Pts',(2.25550066819096,140.152508754552,13.5428906244995));
#80330=CARTESIAN_POINT('Ctrl Pts',(2.25460033050362,140.155180468557,13.5298485249686));
#80331=CARTESIAN_POINT('Ctrl Pts',(2.25238244960284,140.161168304665,13.4978704807504));
#80332=CARTESIAN_POINT('Ctrl Pts',(2.2510574696775,140.164242878733,13.4788938286223));
#80333=CARTESIAN_POINT('Ctrl Pts',(2.24453588561216,140.176946797534,13.3861602685533));
#80334=CARTESIAN_POINT('Ctrl Pts',(2.2391399945279,140.180036989101,13.3116904380777));
#80335=CARTESIAN_POINT('Ctrl Pts',(2.22870469908476,140.172486848981,13.1697553418608));
#80336=CARTESIAN_POINT('Ctrl Pts',(2.22369890502352,140.163050232008,13.1025042048074));
#80337=CARTESIAN_POINT('Ctrl Pts',(2.21794038478802,140.144819201995,13.0231045165625));
#80338=CARTESIAN_POINT('Ctrl Pts',(2.21698306898224,140.141526405918,13.0098282935504));
#80339=CARTESIAN_POINT('Ctrl Pts',(2.21548604850883,140.135947360223,12.9889014113496));
#80340=CARTESIAN_POINT('Ctrl Pts',(2.21493855734802,140.133813423178,12.9812118760396));
#80341=CARTESIAN_POINT('Ctrl Pts',(2.21386072339937,140.129422060607,12.9659899860858));
#80342=CARTESIAN_POINT('Ctrl Pts',(2.2133302739426,140.127167033051,12.9584573687298));
#80343=CARTESIAN_POINT('Ctrl Pts',(2.21193853135526,140.121006181999,12.9386037546601));
#80344=CARTESIAN_POINT('Ctrl Pts',(2.21108417134733,140.116972579735,12.9263231390681));
#80345=CARTESIAN_POINT('Ctrl Pts',(2.20917584803252,140.107412486386,12.898755967871));
#80346=CARTESIAN_POINT('Ctrl Pts',(2.20812730575607,140.101770020611,12.8835122302565));
#80347=CARTESIAN_POINT('Ctrl Pts',(2.20465874539275,140.08186684179,12.8329801642291));
#80348=CARTESIAN_POINT('Ctrl Pts',(2.20228749641355,140.066211124872,12.7982654231828));
#80349=CARTESIAN_POINT('Ctrl Pts',(2.19450105713038,140.009062155612,12.68635352426));
#80350=CARTESIAN_POINT('Ctrl Pts',(2.18914401530618,139.960648532175,12.6130347060686));
#80351=CARTESIAN_POINT('Ctrl Pts',(2.18216845580539,139.891592326052,12.5302156380824));
#80352=CARTESIAN_POINT('Ctrl Pts',(2.1808450237708,139.878230628679,12.5150059084846));
#80353=CARTESIAN_POINT('Ctrl Pts',(2.17869562473881,139.85617144352,12.4911642030252));
#80354=CARTESIAN_POINT('Ctrl Pts',(2.17787995294451,139.847719351996,12.4823101025167));
#80355=CARTESIAN_POINT('Ctrl Pts',(2.17615414929313,139.829679767511,12.4639928404264));
#80356=CARTESIAN_POINT('Ctrl Pts',(2.17524288943651,139.820064896154,12.4545592702435));
#80357=CARTESIAN_POINT('Ctrl Pts',(2.1729936275348,139.796128752399,12.4318670091998));
#80358=CARTESIAN_POINT('Ctrl Pts',(2.17164800729215,139.781636098753,12.4187958179911));
#80359=CARTESIAN_POINT('Ctrl Pts',(2.16497177872032,139.708936910061,12.3564319094249));
#80360=CARTESIAN_POINT('Ctrl Pts',(2.15943391124451,139.646369881718,12.3125210332979));
#80361=CARTESIAN_POINT('Ctrl Pts',(2.14910595607752,139.523863190429,12.2432009689591));
#80362=CARTESIAN_POINT('Ctrl Pts',(2.14435391962411,139.465197206728,12.2160951855371));
#80363=CARTESIAN_POINT('Ctrl Pts',(2.13879798874671,139.391393542256,12.1890976716974));
#80364=CARTESIAN_POINT('Ctrl Pts',(2.13781337941443,139.378098282155,12.1845025233635));
#80365=CARTESIAN_POINT('Ctrl Pts',(2.13627988467631,139.357002187677,12.1776317726565));
#80366=CARTESIAN_POINT('Ctrl Pts',(2.1357227967925,139.349255097007,12.1751969564406));
#80367=CARTESIAN_POINT('Ctrl Pts',(2.13462845607441,139.333858820776,12.1705325076397));
#80368=CARTESIAN_POINT('Ctrl Pts',(2.13409105683266,139.326210966168,12.1682999764697));
#80369=CARTESIAN_POINT('Ctrl Pts',(2.13268129110015,139.305936539197,12.1626041578633));
#80370=CARTESIAN_POINT('Ctrl Pts',(2.13181592933848,139.293273497132,12.1592734077159));
#80371=CARTESIAN_POINT('Ctrl Pts',(2.12728516373587,139.225994317005,12.1427714965815));
#80372=CARTESIAN_POINT('Ctrl Pts',(2.12378034255749,139.170537653335,12.1333082816886));
#80373=CARTESIAN_POINT('Ctrl Pts',(2.11525682551867,139.033868034591,12.1199449508485));
#80374=CARTESIAN_POINT('Ctrl Pts',(2.11026701857196,138.952532233442,12.1204143121773));
#80375=CARTESIAN_POINT('Ctrl Pts',(2.10368943184909,138.851417175468,12.1314785018599));
#80376=CARTESIAN_POINT('Ctrl Pts',(2.10234335522298,138.831004583655,12.1342556820317));
#80377=CARTESIAN_POINT('Ctrl Pts',(2.10007501371621,138.797160654769,12.1397677908201));
#80378=CARTESIAN_POINT('Ctrl Pts',(2.09916210251997,138.78368498598,12.1422045226007));
#80379=CARTESIAN_POINT('Ctrl Pts',(2.0973191559252,138.756792773886,12.1475531606829));
#80380=CARTESIAN_POINT('Ctrl Pts',(2.09638922911049,138.743378577313,12.150465794256));
#80381=CARTESIAN_POINT('Ctrl Pts',(2.09403383361451,138.709809894335,12.1583714189739));
#80382=CARTESIAN_POINT('Ctrl Pts',(2.09259909307004,138.689731540893,12.1636640008672));
#80383=CARTESIAN_POINT('Ctrl Pts',(2.08941622219356,138.646019822059,12.1764311005241));
#80384=CARTESIAN_POINT('Ctrl Pts',(2.08766193247673,138.622461733889,12.1841264637165));
#80385=CARTESIAN_POINT('Ctrl Pts',(2.07854696123358,138.502726554575,12.2274642197546));
#80386=CARTESIAN_POINT('Ctrl Pts',(2.07086395863705,138.41127481782,12.2748109570225));
#80387=CARTESIAN_POINT('Ctrl Pts',(2.06349999999998,138.327116518419,12.3333962121349));
#80388=CARTESIAN_POINT('',(2.0635,139.684664424539,12.3417048010816));
#80389=CARTESIAN_POINT('Origin',(2.0635,139.,13.3));
#80390=CARTESIAN_POINT('Ctrl Pts',(2.06349999999976,139.684664424539,12.3417048010814));
#80391=CARTESIAN_POINT('Ctrl Pts',(2.06413207243538,139.692276025771,12.3471429923432));
#80392=CARTESIAN_POINT('Ctrl Pts',(2.06475846007851,139.699814794663,12.3526659312376));
#80393=CARTESIAN_POINT('Ctrl Pts',(2.06626808273718,139.717950082849,12.3662868168646));
#80394=CARTESIAN_POINT('Ctrl Pts',(2.06714603508711,139.728468797957,12.374469952678));
#80395=CARTESIAN_POINT('Ctrl Pts',(2.0715132138531,139.780513105435,12.4163954144151));
#80396=CARTESIAN_POINT('Ctrl Pts',(2.07489099690678,139.819847070126,12.4527636475568));
#80397=CARTESIAN_POINT('Ctrl Pts',(2.08230577647004,139.900562164323,12.5382974931292));
#80398=CARTESIAN_POINT('Ctrl Pts',(2.08633185582837,139.940669195938,12.588421714189));
#80399=CARTESIAN_POINT('Ctrl Pts',(2.09201028102551,139.989650974106,12.6610637734024));
#80400=CARTESIAN_POINT('Ctrl Pts',(2.09355018068357,140.002215711147,12.6809587124619));
#80401=CARTESIAN_POINT('Ctrl Pts',(2.09611575615856,140.021896338493,12.7142922723833));
#80402=CARTESIAN_POINT('Ctrl Pts',(2.09712994397898,140.029363050064,12.7275165091744));
#80403=CARTESIAN_POINT('Ctrl Pts',(2.09916946998459,140.043740119151,12.754170696032));
#80404=CARTESIAN_POINT('Ctrl Pts',(2.10019451974577,140.050651981217,12.767596538696));
#80405=CARTESIAN_POINT('Ctrl Pts',(2.10279087435359,140.067360811613,12.8016455744444));
#80406=CARTESIAN_POINT('Ctrl Pts',(2.10437266492368,140.076819414721,12.8224269023685));
#80407=CARTESIAN_POINT('Ctrl Pts',(2.11222247014196,140.120210322204,12.9256139468685));
#80408=CARTESIAN_POINT('Ctrl Pts',(2.11876461733174,140.145312735583,13.011400775157));
#80409=CARTESIAN_POINT('Ctrl Pts',(2.13001082082233,140.171256861151,13.1613263014646));
#80410=CARTESIAN_POINT('Ctrl Pts',(2.13466710424179,140.177002791467,13.2242435825927));
#80411=CARTESIAN_POINT('Ctrl Pts',(2.14005074624944,140.177822454712,13.300392861075));
#80412=CARTESIAN_POINT('Ctrl Pts',(2.1409657211342,140.177745574321,13.3134643170549));
#80413=CARTESIAN_POINT('Ctrl Pts',(2.14241951757392,140.177271994475,13.3344807262676));
#80414=CARTESIAN_POINT('Ctrl Pts',(2.14296523071435,140.177012406725,13.3424272709685));
#80415=CARTESIAN_POINT('Ctrl Pts',(2.14403999052804,140.176337051815,13.3582036799551));
#80416=CARTESIAN_POINT('Ctrl Pts',(2.14456903170626,140.175923540063,13.3660330204332));
#80417=CARTESIAN_POINT('Ctrl Pts',(2.14598272575006,140.174599359911,13.3871070701734));
#80418=CARTESIAN_POINT('Ctrl Pts',(2.1468596103102,140.17354284871,13.4003420054723));
#80419=CARTESIAN_POINT('Ctrl Pts',(2.15231803634139,140.165485612026,13.4835178808387));
#80420=CARTESIAN_POINT('Ctrl Pts',(2.15663328603,140.152458270382,13.5527409858127));
#80421=CARTESIAN_POINT('Ctrl Pts',(2.16529624695658,140.114293047057,13.68774228311));
#80422=CARTESIAN_POINT('Ctrl Pts',(2.16962937644036,140.089291502112,13.7532500846333));
#80423=CARTESIAN_POINT('Ctrl Pts',(2.17539110814622,140.050281864033,13.8332592998947));
#80424=CARTESIAN_POINT('Ctrl Pts',(2.17663621255472,140.041525625264,13.8501652284155));
#80425=CARTESIAN_POINT('Ctrl Pts',(2.1787566843611,140.026104282296,13.8782509944093));
#80426=CARTESIAN_POINT('Ctrl Pts',(2.17962407072749,140.019656467382,13.889546330235));
#80427=CARTESIAN_POINT('Ctrl Pts',(2.18138981032915,140.006261303003,13.9121347843412));
#80428=CARTESIAN_POINT('Ctrl Pts',(2.18228830853187,139.999307683292,13.9234219536115));
#80429=CARTESIAN_POINT('Ctrl Pts',(2.18458701174971,139.981182154403,13.951760802839));
#80430=CARTESIAN_POINT('Ctrl Pts',(2.18599685241096,139.969755755006,13.9686435862105));
#80431=CARTESIAN_POINT('Ctrl Pts',(2.19368597685254,139.905832308907,14.0580047812989));
#80432=CARTESIAN_POINT('Ctrl Pts',(2.20027555257896,139.845649928336,14.1246052346611));
#80433=CARTESIAN_POINT('Ctrl Pts',(2.21122798441851,139.7344934079,14.2225279832514));
#80434=CARTESIAN_POINT('Ctrl Pts',(2.21555282743687,139.687619651618,14.2579765791127));
#80435=CARTESIAN_POINT('Ctrl Pts',(2.22053519540554,139.628252999963,14.2962609999035));
#80436=CARTESIAN_POINT('Ctrl Pts',(2.22136977755323,139.618113556419,14.3025833995454));
#80437=CARTESIAN_POINT('Ctrl Pts',(2.22271079299268,139.601473834201,14.3126105943606));
#80438=CARTESIAN_POINT('Ctrl Pts',(2.22322308167965,139.595031759257,14.3164094682078));
#80439=CARTESIAN_POINT('Ctrl Pts',(2.22427832534028,139.581579256063,14.3241706199419));
#80440=CARTESIAN_POINT('Ctrl Pts',(2.22482070539569,139.574563810906,14.3281227196552));
#80441=CARTESIAN_POINT('Ctrl Pts',(2.22628572417675,139.555356986974,14.3386847352448));
#80442=CARTESIAN_POINT('Ctrl Pts',(2.22719998283471,139.543088118983,14.3451519979256));
#80443=CARTESIAN_POINT('Ctrl Pts',(2.23238903180733,139.472031978979,14.3810184213317));
#80444=CARTESIAN_POINT('Ctrl Pts',(2.23644148188335,139.410973121126,14.4056754410378));
#80445=CARTESIAN_POINT('Ctrl Pts',(2.24510756763881,139.276929959089,14.4471555727982));
#80446=CARTESIAN_POINT('Ctrl Pts',(2.24971002566705,139.203765534783,14.4623829840665));
#80447=CARTESIAN_POINT('Ctrl Pts',(2.25585498591522,139.109273320645,14.4728490839006));
#80448=CARTESIAN_POINT('Ctrl Pts',(2.25719482552104,139.088835756897,14.4745738625621));
#80449=CARTESIAN_POINT('Ctrl Pts',(2.25945995909053,139.054645455405,14.476561849671));
#80450=CARTESIAN_POINT('Ctrl Pts',(2.2603760186917,139.040913980292,14.4771193360399));
#80451=CARTESIAN_POINT('Ctrl Pts',(2.26223090317901,139.013323248518,14.4777561567112));
#80452=CARTESIAN_POINT('Ctrl Pts',(2.26316970638875,138.999466102471,14.4778313802513));
#80453=CARTESIAN_POINT('Ctrl Pts',(2.26556139801454,138.96445252382,14.4774035850751));
#80454=CARTESIAN_POINT('Ctrl Pts',(2.26702400649114,138.943305768658,14.4765748978057));
#80455=CARTESIAN_POINT('Ctrl Pts',(2.2737518499631,138.847279805774,14.4702172154917));
#80456=CARTESIAN_POINT('Ctrl Pts',(2.27920927473163,138.773022258433,14.4581060911347));
#80457=CARTESIAN_POINT('Ctrl Pts',(2.28784152407662,138.65902399702,14.428124024552));
#80458=CARTESIAN_POINT('Ctrl Pts',(2.29097993590114,138.618237303402,14.4149825016667));
#80459=CARTESIAN_POINT('Ctrl Pts',(2.29531233963049,138.562037334715,14.3934283182496));
#80460=CARTESIAN_POINT('Ctrl Pts',(2.2965526426546,138.54595786279,14.3868498430392));
#80461=CARTESIAN_POINT('Ctrl Pts',(2.29873849430818,138.51755119602,14.3744875049502));
#80462=CARTESIAN_POINT('Ctrl Pts',(2.29968952716099,138.505167731833,14.3688411070798));
#80463=CARTESIAN_POINT('Ctrl Pts',(2.3011885533406,138.485569742248,14.3594915062799));
#80464=CARTESIAN_POINT('Ctrl Pts',(2.30174392208495,138.478291139038,14.3559264254956));
#80465=CARTESIAN_POINT('Ctrl Pts',(2.30284396359321,138.463827158832,14.3486558501001));
#80466=CARTESIAN_POINT('Ctrl Pts',(2.30338859513916,138.456642025645,14.3449509686713));
#80467=CARTESIAN_POINT('Ctrl Pts',(2.30484681387049,138.437359100049,14.3347554041012));
#80468=CARTESIAN_POINT('Ctrl Pts',(2.3057524089987,138.4253352836,14.3281264670286));
#80469=CARTESIAN_POINT('Ctrl Pts',(2.31113667315481,138.35377327029,14.2870252821611));
#80470=CARTESIAN_POINT('Ctrl Pts',(2.31537294259488,138.297226435663,14.2475966902402));
#80471=CARTESIAN_POINT('Ctrl Pts',(2.32266531069903,138.206778066183,14.1719544603465));
#80472=CARTESIAN_POINT('Ctrl Pts',(2.32570361507321,138.171123362906,14.1381340913705));
#80473=CARTESIAN_POINT('Ctrl Pts',(2.33027701625526,138.121939579175,14.0852638658834));
#80474=CARTESIAN_POINT('Ctrl Pts',(2.33175537515584,138.106696874624,14.0678794635745));
#80475=CARTESIAN_POINT('Ctrl Pts',(2.33453026448093,138.079415915783,14.0348530302698));
#80476=CARTESIAN_POINT('Ctrl Pts',(2.3358211561055,138.067240177319,14.0193351597679));
#80477=CARTESIAN_POINT('Ctrl Pts',(2.33802583763286,138.047355667512,13.9926383796948));
#80478=CARTESIAN_POINT('Ctrl Pts',(2.3389314363825,138.039439950873,13.9816183061784));
#80479=CARTESIAN_POINT('Ctrl Pts',(2.3406725046085,138.0247108208,13.9603465233313));
#80480=CARTESIAN_POINT('Ctrl Pts',(2.34150656079126,138.017864251657,13.9501198857444));
#80481=CARTESIAN_POINT('Ctrl Pts',(2.34373310838499,138.000146681057,13.9227366056069));
#80482=CARTESIAN_POINT('Ctrl Pts',(2.34513565670164,137.989557499316,13.9054035044915));
#80483=CARTESIAN_POINT('Ctrl Pts',(2.35181427384127,137.941826054495,13.8225298473835));
#80484=CARTESIAN_POINT('Ctrl Pts',(2.35728795971268,137.910598130773,13.7538297741315));
#80485=CARTESIAN_POINT('Ctrl Pts',(2.36281347991194,137.88614819712,13.6826607161973));
#80486=CARTESIAN_POINT('Origin',(1.13913288526384,139.,13.3));
#80487=CARTESIAN_POINT('',(2.96251705962155,137.886148212658,13.6826607614251));
#80488=CARTESIAN_POINT('',(2.86376176824067,137.886148209742,13.6826607529367));
#80489=CARTESIAN_POINT('',(1.13913288526384,137.88614821265,13.6826607614027));
#80490=CARTESIAN_POINT('Ctrl Pts',(2.96251705962155,137.886148212665,13.6826607614475));
#80491=CARTESIAN_POINT('Ctrl Pts',(2.95646427638088,137.914303066403,13.7646141188798));
#80492=CARTESIAN_POINT('Ctrl Pts',(2.95012116491658,137.951412599125,13.8431978452712));
#80493=CARTESIAN_POINT('Ctrl Pts',(2.94094865633092,138.016846374047,13.9495915135337));
#80494=CARTESIAN_POINT('Ctrl Pts',(2.93814404898771,138.038477049007,13.9812004767065));
#80495=CARTESIAN_POINT('Ctrl Pts',(2.93421783410981,138.071450872807,14.0246770331796));
#80496=CARTESIAN_POINT('Ctrl Pts',(2.93305563758885,138.081560683279,14.0374480041505));
#80497=CARTESIAN_POINT('Ctrl Pts',(2.93099474864767,138.10016896321,14.059977926502));
#80498=CARTESIAN_POINT('Ctrl Pts',(2.93009120527257,138.108569459425,14.0698142436267));
#80499=CARTESIAN_POINT('Ctrl Pts',(2.92865679132281,138.122323516098,14.0853920087352));
#80500=CARTESIAN_POINT('Ctrl Pts',(2.92811919652302,138.127575181228,14.0912215644773));
#80501=CARTESIAN_POINT('Ctrl Pts',(2.92704265943291,138.138296328096,14.1028859131977));
#80502=CARTESIAN_POINT('Ctrl Pts',(2.92650389367022,138.143767735551,14.1087183233468));
#80503=CARTESIAN_POINT('Ctrl Pts',(2.9250555123353,138.158750749254,14.1243673801587));
#80504=CARTESIAN_POINT('Ctrl Pts',(2.92415395412031,138.168374824719,14.1340752285838));
#80505=CARTESIAN_POINT('Ctrl Pts',(2.91879091357252,138.227262727787,14.1914427888018));
#80506=CARTESIAN_POINT('Ctrl Pts',(2.91457257147433,138.280447035369,14.2349005065517));
#80507=CARTESIAN_POINT('Ctrl Pts',(2.90727758395957,138.378028587346,14.3013473983221));
#80508=CARTESIAN_POINT('Ctrl Pts',(2.90421788048289,138.420655381496,14.3265984975157));
#80509=CARTESIAN_POINT('Ctrl Pts',(2.89961986449765,138.485371650327,14.3596174241781));
#80510=CARTESIAN_POINT('Ctrl Pts',(2.89813975559793,138.506306109645,14.3695315181162));
#80511=CARTESIAN_POINT('Ctrl Pts',(2.89536475165503,138.545568622493,14.3867269639389));
#80512=CARTESIAN_POINT('Ctrl Pts',(2.89407561786099,138.563813584067,14.3941776400951));
#80513=CARTESIAN_POINT('Ctrl Pts',(2.89188108521518,138.594808206175,14.4059364728599));
#80514=CARTESIAN_POINT('Ctrl Pts',(2.89098401695126,138.607460677712,14.410490309218));
#80515=CARTESIAN_POINT('Ctrl Pts',(2.88915629679668,138.633183899496,14.4192539973092));
#80516=CARTESIAN_POINT('Ctrl Pts',(2.88822547886479,138.6462558124,14.4234538637689));
#80517=CARTESIAN_POINT('Ctrl Pts',(2.88583351993616,138.679756063075,14.4335745119744));
#80518=CARTESIAN_POINT('Ctrl Pts',(2.88436222385205,138.700276055443,14.4391719835894));
#80519=CARTESIAN_POINT('Ctrl Pts',(2.87752814097923,138.795141304597,14.4623089394183));
#80520=CARTESIAN_POINT('Ctrl Pts',(2.87196243263017,138.870920950121,14.4731429258473));
#80521=CARTESIAN_POINT('Ctrl Pts',(2.86312578182455,138.991108701895,14.478536211947));
#80522=CARTESIAN_POINT('Ctrl Pts',(2.85989427780272,139.035092070729,14.4780473327829));
#80523=CARTESIAN_POINT('Ctrl Pts',(2.85545500363692,139.096489825624,14.4739224532959));
#80524=CARTESIAN_POINT('Ctrl Pts',(2.85419700888376,139.114005294646,14.4723510863785));
#80525=CARTESIAN_POINT('Ctrl Pts',(2.85198700728598,139.14508170287,14.4688600030221));
#80526=CARTESIAN_POINT('Ctrl Pts',(2.85102913643867,139.158656616601,14.4670949086401));
#80527=CARTESIAN_POINT('Ctrl Pts',(2.8495301914702,139.180113010494,14.4639236983597));
#80528=CARTESIAN_POINT('Ctrl Pts',(2.84898135787315,139.188015807698,14.4626732721216));
#80529=CARTESIAN_POINT('Ctrl Pts',(2.84790362175273,139.203639071181,14.4600378013745));
#80530=CARTESIAN_POINT('Ctrl Pts',(2.84737459876056,139.211359604073,14.458655987293));
#80531=CARTESIAN_POINT('Ctrl Pts',(2.84598491146719,139.231758263538,14.4547943699576));
#80532=CARTESIAN_POINT('Ctrl Pts',(2.84513121119135,139.244410804899,14.4521828510139));
#80533=CARTESIAN_POINT('Ctrl Pts',(2.83930804671342,139.331323913121,14.4327475100138));
#80534=CARTESIAN_POINT('Ctrl Pts',(2.83464826567873,139.403852941535,14.4089627125076));
#80535=CARTESIAN_POINT('Ctrl Pts',(2.82711638647817,139.515392998031,14.3599764965389));
#80536=CARTESIAN_POINT('Ctrl Pts',(2.82428398209048,139.556095966834,14.3392001837738));
#80537=CARTESIAN_POINT('Ctrl Pts',(2.81998207717441,139.614619769986,14.3049026469251));
#80538=CARTESIAN_POINT('Ctrl Pts',(2.81856210774795,139.633430018696,14.2931531174113));
#80539=CARTESIAN_POINT('Ctrl Pts',(2.8158869145189,139.667792776651,14.270315500188));
#80540=CARTESIAN_POINT('Ctrl Pts',(2.81463670508925,139.683428989856,14.259366515478));
#80541=CARTESIAN_POINT('Ctrl Pts',(2.8124882130804,139.709530642263,14.240127286651));
#80542=CARTESIAN_POINT('Ctrl Pts',(2.81159743286672,139.720134041103,14.2320300346127));
#80543=CARTESIAN_POINT('Ctrl Pts',(2.80976504738042,139.741486455576,14.215142417727));
#80544=CARTESIAN_POINT('Ctrl Pts',(2.80882299533033,139.752222102584,14.2063386167127));
#80545=CARTESIAN_POINT('Ctrl Pts',(2.80636219022813,139.779627715741,14.1830421986584));
#80546=CARTESIAN_POINT('Ctrl Pts',(2.80483207943284,139.796049399458,14.1682673201443));
#80547=CARTESIAN_POINT('Ctrl Pts',(2.79596435802696,139.887663566981,14.0810559285882));
#80548=CARTESIAN_POINT('Ctrl Pts',(2.78821814302433,139.953365569953,13.9993436884224));
#80549=CARTESIAN_POINT('Ctrl Pts',(2.77876875349182,140.020489283649,13.8885002619602));
#80550=CARTESIAN_POINT('Ctrl Pts',(2.77694338091867,140.032856017517,13.8665152494277));
#80551=CARTESIAN_POINT('Ctrl Pts',(2.77388139473684,140.052696169122,13.8284315674735));
#80552=CARTESIAN_POINT('Ctrl Pts',(2.77263146660674,140.060529080949,13.8125302875807));
#80553=CARTESIAN_POINT('Ctrl Pts',(2.77079016566074,140.071704948047,13.7884882744695));
#80554=CARTESIAN_POINT('Ctrl Pts',(2.77018456005063,140.07532015996,13.7804777369926));
#80555=CARTESIAN_POINT('Ctrl Pts',(2.76907479188195,140.081838118129,13.7655931784909));
#80556=CARTESIAN_POINT('Ctrl Pts',(2.76856931279198,140.084765579221,13.7587312538943));
#80557=CARTESIAN_POINT('Ctrl Pts',(2.76734605272378,140.091744339827,13.7419326728629));
#80558=CARTESIAN_POINT('Ctrl Pts',(2.76663230603118,140.095725385821,13.7319676960192));
#80559=CARTESIAN_POINT('Ctrl Pts',(2.763837912919,140.110918673227,13.6923750661017));
#80560=CARTESIAN_POINT('Ctrl Pts',(2.76180972217653,140.121070782741,13.6623522576163));
#80561=CARTESIAN_POINT('Ctrl Pts',(2.7555091423141,140.149233394899,13.5664842484062));
#80562=CARTESIAN_POINT('Ctrl Pts',(2.75135332240071,140.162740684014,13.4994646764901));
#80563=CARTESIAN_POINT('Ctrl Pts',(2.74606215449591,140.172244708905,13.4149739945561));
#80564=CARTESIAN_POINT('Ctrl Pts',(2.74501340583822,140.173763873846,13.3982599705989));
#80565=CARTESIAN_POINT('Ctrl Pts',(2.74161964085247,140.1774976719,13.3444454654854));
#80566=CARTESIAN_POINT('Ctrl Pts',(2.73924862467719,140.178313569384,13.3072735012378));
#80567=CARTESIAN_POINT('Ctrl Pts',(2.73573465045298,140.176947063702,13.2534150163207));
#80568=CARTESIAN_POINT('Ctrl Pts',(2.73463417971304,140.176167251754,13.2367141328168));
#80569=CARTESIAN_POINT('Ctrl Pts',(2.73265520278804,140.174146518575,13.207020373354));
#80570=CARTESIAN_POINT('Ctrl Pts',(2.73178116875128,140.173044591831,13.1940206614416));
#80571=CARTESIAN_POINT('Ctrl Pts',(2.72990781827039,140.170242429182,13.166419492816));
#80572=CARTESIAN_POINT('Ctrl Pts',(2.72890682441286,140.168484323683,13.151826297632));
#80573=CARTESIAN_POINT('Ctrl Pts',(2.7260808992278,140.162800178642,13.11108207491));
#80574=CARTESIAN_POINT('Ctrl Pts',(2.72423742540446,140.158266078932,13.0850261977428));
#80575=CARTESIAN_POINT('Ctrl Pts',(2.71554413255922,140.133109548212,12.9646129095003));
#80576=CARTESIAN_POINT('Ctrl Pts',(2.70837759843094,140.101808294031,12.8728758460773));
#80577=CARTESIAN_POINT('Ctrl Pts',(2.69870720917318,140.043930321278,12.7535516889008));
#80578=CARTESIAN_POINT('Ctrl Pts',(2.69610461206466,140.026703374677,12.7218331269415));
#80579=CARTESIAN_POINT('Ctrl Pts',(2.69276029577135,140.00207914963,12.681077085518));
#80580=CARTESIAN_POINT('Ctrl Pts',(2.6919571582432,139.995967247938,12.6712890467248));
#80581=CARTESIAN_POINT('Ctrl Pts',(2.6906458910845,139.985642919904,12.6552834317038));
#80582=CARTESIAN_POINT('Ctrl Pts',(2.69013278603232,139.9815132273,12.6490136586495));
#80583=CARTESIAN_POINT('Ctrl Pts',(2.68905528701246,139.972644951077,12.6358259588382));
#80584=CARTESIAN_POINT('Ctrl Pts',(2.68849183153208,139.967891984953,12.6289184297513));
#80585=CARTESIAN_POINT('Ctrl Pts',(2.68689328005565,139.95408979238,12.6093113049842));
#80586=CARTESIAN_POINT('Ctrl Pts',(2.68586930428567,139.944861241485,12.5967393823012));
#80587=CARTESIAN_POINT('Ctrl Pts',(2.68349261644428,139.92260433705,12.5676485030669));
#80588=CARTESIAN_POINT('Ctrl Pts',(2.68215023481727,139.909377519702,12.5512877034403));
#80589=CARTESIAN_POINT('Ctrl Pts',(2.67684015034007,139.854776040291,12.4873320624687));
#80590=CARTESIAN_POINT('Ctrl Pts',(2.67298891306041,139.810046183845,12.4427385488402));
#80591=CARTESIAN_POINT('Ctrl Pts',(2.66557615801517,139.718945518702,12.3654442474519));
#80592=CARTESIAN_POINT('Ctrl Pts',(2.66203676676584,139.673370213679,12.3320905920249));
#80593=CARTESIAN_POINT('Ctrl Pts',(2.65717130904673,139.609879379389,12.2922868569744));
#80594=CARTESIAN_POINT('Ctrl Pts',(2.65595576476691,139.593945200348,12.2828138454466));
#80595=CARTESIAN_POINT('Ctrl Pts',(2.65384787932054,139.566246960718,12.267219740887));
#80596=CARTESIAN_POINT('Ctrl Pts',(2.65296232148721,139.554590618507,12.2609139084754));
#80597=CARTESIAN_POINT('Ctrl Pts',(2.65112351693161,139.530364629532,12.2483319230294));
#80598=CARTESIAN_POINT('Ctrl Pts',(2.65016954817143,139.517784172462,12.2420813333175));
#80599=CARTESIAN_POINT('Ctrl Pts',(2.6476358947917,139.484359447224,12.2262133007545));
#80600=CARTESIAN_POINT('Ctrl Pts',(2.64604353078672,139.463341503351,12.2169780827989));
#80601=CARTESIAN_POINT('Ctrl Pts',(2.63904814699702,139.371015738573,12.1795899085017));
#80602=CARTESIAN_POINT('Ctrl Pts',(2.63344720661547,139.297333456835,12.1578262082442));
#80603=CARTESIAN_POINT('Ctrl Pts',(2.6233513268985,139.162357044138,12.131910712448));
#80604=CARTESIAN_POINT('Ctrl Pts',(2.61888690131824,139.101838166796,12.1250860651044));
#80605=CARTESIAN_POINT('Ctrl Pts',(2.61374785087651,139.028862343082,12.1225404692164));
#80606=CARTESIAN_POINT('Ctrl Pts',(2.61289690439158,139.016660029395,12.1223046002309));
#80607=CARTESIAN_POINT('Ctrl Pts',(2.6115768950797,138.997511803851,12.1222321581758));
#80608=CARTESIAN_POINT('Ctrl Pts',(2.61110134948665,138.990567612995,12.122267298177));
#80609=CARTESIAN_POINT('Ctrl Pts',(2.61009009270014,138.975693367215,12.1224741379759));
#80610=CARTESIAN_POINT('Ctrl Pts',(2.60955545845676,138.967763852686,12.1226645303241));
#80611=CARTESIAN_POINT('Ctrl Pts',(2.60813233657684,138.946500278861,12.1233900789607));
#80612=CARTESIAN_POINT('Ctrl Pts',(2.60725142571311,138.933171975335,12.1240717799075));
#80613=CARTESIAN_POINT('Ctrl Pts',(2.60527078173857,138.902910402694,12.1261357782268));
#80614=CARTESIAN_POINT('Ctrl Pts',(2.60417715766075,138.885989467951,12.1276582161223));
#80615=CARTESIAN_POINT('Ctrl Pts',(2.60046542407353,138.828100590766,12.13413200809));
#80616=CARTESIAN_POINT('Ctrl Pts',(2.59790383431498,138.787361331258,12.140869810963));
#80617=CARTESIAN_POINT('Ctrl Pts',(2.59034158179797,138.667967260764,12.1671244168521));
#80618=CARTESIAN_POINT('Ctrl Pts',(2.58537165666007,138.590889263896,12.1926248313139));
#80619=CARTESIAN_POINT('Ctrl Pts',(2.5787934169404,138.497965454653,12.2344045145641));
#80620=CARTESIAN_POINT('Ctrl Pts',(2.57742838146803,138.47912434219,12.2434864478856));
#80621=CARTESIAN_POINT('Ctrl Pts',(2.57514297570203,138.448388001399,12.2593242492612));
#80622=CARTESIAN_POINT('Ctrl Pts',(2.57423261405881,138.436350451406,12.2657945199197));
#80623=CARTESIAN_POINT('Ctrl Pts',(2.57240777441562,138.412647480277,12.2790717825479));
#80624=CARTESIAN_POINT('Ctrl Pts',(2.57149361126972,138.400981153039,12.2858728865739));
#80625=CARTESIAN_POINT('Ctrl Pts',(2.56920604004584,138.372316469135,12.3032506919806));
#80626=CARTESIAN_POINT('Ctrl Pts',(2.56782422807919,138.355466542002,12.3140627129904));
#80627=CARTESIAN_POINT('Ctrl Pts',(2.56104135236056,138.275038526765,12.3686136249284));
#80628=CARTESIAN_POINT('Ctrl Pts',(2.5554277968484,138.215597506304,12.4180936589112));
#80629=CARTESIAN_POINT('Ctrl Pts',(2.54516716506433,138.117493759442,12.517572295702));
#80630=CARTESIAN_POINT('Ctrl Pts',(2.54055902904284,138.077174286213,12.5655585181767));
#80631=CARTESIAN_POINT('Ctrl Pts',(2.53513126941458,138.032653893176,12.6280354518401));
#80632=CARTESIAN_POINT('Ctrl Pts',(2.53414114286161,138.024658780827,12.6396937113549));
#80633=CARTESIAN_POINT('Ctrl Pts',(2.53260395005526,138.012419215598,12.6582486921008));
#80634=CARTESIAN_POINT('Ctrl Pts',(2.53204848415557,138.008032940814,12.665049678961));
#80635=CARTESIAN_POINT('Ctrl Pts',(2.53096927703127,137.999576441104,12.6784631610406));
#80636=CARTESIAN_POINT('Ctrl Pts',(2.53044525326067,137.995500885975,12.6850716507389));
#80637=CARTESIAN_POINT('Ctrl Pts',(2.52908539718374,137.985015539958,12.7024560283014));
#80638=CARTESIAN_POINT('Ctrl Pts',(2.5282559990971,137.978711719937,12.7132951911438));
#80639=CARTESIAN_POINT('Ctrl Pts',(2.52641263751658,137.964945637128,12.7378598759104));
#80640=CARTESIAN_POINT('Ctrl Pts',(2.52540359728806,137.957580854063,12.7516375058554));
#80641=CARTESIAN_POINT('Ctrl Pts',(2.5221279857152,137.934337645941,12.7972812673542));
#80642=CARTESIAN_POINT('Ctrl Pts',(2.51990488982002,137.919628879312,12.8297224923258));
#80643=CARTESIAN_POINT('Ctrl Pts',(2.51194043115319,137.871957632597,12.9489598685272));
#80644=CARTESIAN_POINT('Ctrl Pts',(2.50628575698445,137.847813491294,13.0388994043874));
#80645=CARTESIAN_POINT('Ctrl Pts',(2.49901509361655,137.831683349772,13.1499701873584));
#80646=CARTESIAN_POINT('Ctrl Pts',(2.4977430908007,137.829366964721,13.169267579232));
#80647=CARTESIAN_POINT('Ctrl Pts',(2.49557808838465,137.826275003925,13.2018137492617));
#80648=CARTESIAN_POINT('Ctrl Pts',(2.49469319961711,137.825243950473,13.2150346778205));
#80649=CARTESIAN_POINT('Ctrl Pts',(2.49287625974316,137.823598863839,13.241995465887));
#80650=CARTESIAN_POINT('Ctrl Pts',(2.4919438184932,137.823001837056,13.255734261437));
#80651=CARTESIAN_POINT('Ctrl Pts',(2.489539971741,137.822090615859,13.2908858258664));
#80652=CARTESIAN_POINT('Ctrl Pts',(2.48805818800391,137.822119636331,13.3123016249424));
#80653=CARTESIAN_POINT('Ctrl Pts',(2.48214734766849,137.824535676554,13.3966940542107));
#80654=CARTESIAN_POINT('Ctrl Pts',(2.47758840895213,137.831391287714,13.459429453727));
#80655=CARTESIAN_POINT('Ctrl Pts',(2.46888627835354,137.853704825262,13.5760620385627));
#80656=CARTESIAN_POINT('Ctrl Pts',(2.46477007283849,137.868050284058,13.6299811763935));
#80657=CARTESIAN_POINT('Ctrl Pts',(2.46074688473191,137.88614821265,13.6826607614027));
#80658=CARTESIAN_POINT('Ctrl Pts',(2.36281347991194,137.88614819712,13.6826607161973));
#80659=CARTESIAN_POINT('Ctrl Pts',(2.36370494271238,137.882203553803,13.6711786176069));
#80660=CARTESIAN_POINT('Ctrl Pts',(2.36459733014602,137.878435320883,13.6596322255798));
#80661=CARTESIAN_POINT('Ctrl Pts',(2.36828519000139,137.863595032016,13.6116540706226));
#80662=CARTESIAN_POINT('Ctrl Pts',(2.37107428274278,137.854114502947,13.5747566644989));
#80663=CARTESIAN_POINT('Ctrl Pts',(2.37498502668362,137.843155181419,13.521517850011));
#80664=CARTESIAN_POINT('Ctrl Pts',(2.37614673066806,137.840203586683,13.5055052918271));
#80665=CARTESIAN_POINT('Ctrl Pts',(2.37820869752349,137.83550089769,13.4766486884019));
#80666=CARTESIAN_POINT('Ctrl Pts',(2.37911376202389,137.833628026566,13.4638272654617));
#80667=CARTESIAN_POINT('Ctrl Pts',(2.3805534315095,137.830954285057,13.443141860933));
#80668=CARTESIAN_POINT('Ctrl Pts',(2.38109472504524,137.83002036977,13.4352965275862));
#80669=CARTESIAN_POINT('Ctrl Pts',(2.38217850131203,137.828294316822,13.4194389535477));
#80670=CARTESIAN_POINT('Ctrl Pts',(2.38272078806668,137.827505244843,13.4114267938098));
#80671=CARTESIAN_POINT('Ctrl Pts',(2.38418591104725,137.825580522056,13.3895898716165));
#80672=CARTESIAN_POINT('Ctrl Pts',(2.38510036017024,137.824606797752,13.3757516794376));
#80673=CARTESIAN_POINT('Ctrl Pts',(2.39026989169334,137.820439133956,13.2965630087617));
#80674=CARTESIAN_POINT('Ctrl Pts',(2.39430478192049,137.822450397756,13.2310462106728));
#80675=CARTESIAN_POINT('Ctrl Pts',(2.40151098035598,137.83572054376,13.1151443196098));
#80676=CARTESIAN_POINT('Ctrl Pts',(2.40467113387298,137.844859456328,13.0646954947855));
#80677=CARTESIAN_POINT('Ctrl Pts',(2.40939932616093,137.862959193525,12.9921210168449));
#80678=CARTESIAN_POINT('Ctrl Pts',(2.41090490556354,137.86935186253,12.9694157444935));
#80679=CARTESIAN_POINT('Ctrl Pts',(2.41372229769881,137.882409200919,12.9278645682477));
#80680=CARTESIAN_POINT('Ctrl Pts',(2.41502799622043,137.888880306906,12.908966849498));
#80681=CARTESIAN_POINT('Ctrl Pts',(2.41724298798655,137.900526983021,12.8775825192685));
#80682=CARTESIAN_POINT('Ctrl Pts',(2.41814356103877,137.905442759992,12.8650036027267));
#80683=CARTESIAN_POINT('Ctrl Pts',(2.41997204211476,137.915775907125,12.839847142172));
#80684=CARTESIAN_POINT('Ctrl Pts',(2.42090001345591,137.921198502948,12.8272740345724));
#80685=CARTESIAN_POINT('Ctrl Pts',(2.42327065143957,137.93549166057,12.7956606332028));
#80686=CARTESIAN_POINT('Ctrl Pts',(2.42472313582341,137.94465433273,12.7767585403582));
#80687=CARTESIAN_POINT('Ctrl Pts',(2.43184752135921,137.991510012431,12.6863408938383));
#80688=CARTESIAN_POINT('Ctrl Pts',(2.43775288960991,138.035987712953,12.6186001107558));
#80689=CARTESIAN_POINT('Ctrl Pts',(2.44807394619868,138.124690481633,12.5097594508452));
#80690=CARTESIAN_POINT('Ctrl Pts',(2.45245277928582,138.1657966472,12.466481603452));
#80691=CARTESIAN_POINT('Ctrl Pts',(2.45757202356835,138.21961343685,12.4178097268812));
#80692=CARTESIAN_POINT('Ctrl Pts',(2.45847719720754,138.22936416045,12.4092793344997));
#80693=CARTESIAN_POINT('Ctrl Pts',(2.4599137108304,138.245248935978,12.3958387531089));
#80694=CARTESIAN_POINT('Ctrl Pts',(2.46045184443412,138.251294597947,12.3908262201031));
#80695=CARTESIAN_POINT('Ctrl Pts',(2.46153208348657,138.263633059035,12.3808028049711));
#80696=CARTESIAN_POINT('Ctrl Pts',(2.46207398446655,138.269927887874,12.3757952197848));
#80697=CARTESIAN_POINT('Ctrl Pts',(2.4635304760307,138.287116566024,12.3624067155546));
#80698=CARTESIAN_POINT('Ctrl Pts',(2.46443692383154,138.298106963837,12.3541510883681));
#80699=CARTESIAN_POINT('Ctrl Pts',(2.46974089713571,138.363971711688,12.306456122906));
#80700=CARTESIAN_POINT('Ctrl Pts',(2.47390281228041,138.422019827442,12.2716019509782));
#80701=CARTESIAN_POINT('Ctrl Pts',(2.48255144186157,138.547765708745,12.2101295802508));
#80702=CARTESIAN_POINT('Ctrl Pts',(2.48702651210484,138.615572691124,12.1844070781383));
#80703=CARTESIAN_POINT('Ctrl Pts',(2.49302055325611,138.704911492484,12.1596352822596));
#80704=CARTESIAN_POINT('Ctrl Pts',(2.49434993994169,138.724651767359,12.1547086889104));
#80705=CARTESIAN_POINT('Ctrl Pts',(2.49659746925259,138.757818684663,12.14733822211));
#80706=CARTESIAN_POINT('Ctrl Pts',(2.49750648697719,138.771178423432,12.1446119165284));
#80707=CARTESIAN_POINT('Ctrl Pts',(2.49934647970019,138.798089224461,12.1396052996263));
#80708=CARTESIAN_POINT('Ctrl Pts',(2.5002774253177,138.811638842421,12.1373289938924));
#80709=CARTESIAN_POINT('Ctrl Pts',(2.50264515492876,138.84591527995,12.1321855020265));
#80710=CARTESIAN_POINT('Ctrl Pts',(2.5040915052838,138.866683689059,12.1296327642032));
#80711=CARTESIAN_POINT('Ctrl Pts',(2.51122721403268,138.968265985038,12.1198856326596));
#80712=CARTESIAN_POINT('Ctrl Pts',(2.51715038312931,139.049596363856,12.1205030222231));
#80713=CARTESIAN_POINT('Ctrl Pts',(2.52738559354353,139.188131821146,12.1359129221112));
#80714=CARTESIAN_POINT('Ctrl Pts',(2.53166186741653,139.245507379856,12.1466485243347));
#80715=CARTESIAN_POINT('Ctrl Pts',(2.53670134925441,139.314551830955,12.1649560724034));
#80716=CARTESIAN_POINT('Ctrl Pts',(2.53761915624092,139.327190877144,12.1685346942726));
#80717=CARTESIAN_POINT('Ctrl Pts',(2.53907341540822,139.347360371918,12.1746117511051));
#80718=CARTESIAN_POINT('Ctrl Pts',(2.5396168056144,139.354929709527,12.176976024111));
#80719=CARTESIAN_POINT('Ctrl Pts',(2.54070249699927,139.370131193591,12.1818932455645));
#80720=CARTESIAN_POINT('Ctrl Pts',(2.54124465009739,139.377762188072,12.1844483187086));
#80721=CARTESIAN_POINT('Ctrl Pts',(2.54270111718668,139.398349993115,12.1915771911104));
#80722=CARTESIAN_POINT('Ctrl Pts',(2.54360730825848,139.41125434383,12.1962999749666));
#80723=CARTESIAN_POINT('Ctrl Pts',(2.54892245681042,139.487276639879,12.2256414952513));
#80724=CARTESIAN_POINT('Ctrl Pts',(2.55309476832289,139.548264799519,12.2554461967351));
#80725=CARTESIAN_POINT('Ctrl Pts',(2.56177207600366,139.668640266625,12.3277379455101));
#80726=CARTESIAN_POINT('Ctrl Pts',(2.56626547947886,139.727322110554,12.3708205972148));
#80727=CARTESIAN_POINT('Ctrl Pts',(2.57226350223519,139.79667163363,12.4323524860332));
#80728=CARTESIAN_POINT('Ctrl Pts',(2.57357577401968,139.811341058487,12.4460541528802));
#80729=CARTESIAN_POINT('Ctrl Pts',(2.57580232370098,139.835334820325,12.4696415572273));
#80730=CARTESIAN_POINT('Ctrl Pts',(2.57670784220026,139.844851383168,12.4793261794082));
#80731=CARTESIAN_POINT('Ctrl Pts',(2.5785471687522,139.863683246502,12.4991653532434));
#80732=CARTESIAN_POINT('Ctrl Pts',(2.57948105188919,139.87299198058,12.5093231662068));
#80733=CARTESIAN_POINT('Ctrl Pts',(2.58186968724454,139.896151278757,12.5355025224336));
#80734=CARTESIAN_POINT('Ctrl Pts',(2.58333439004339,139.909751326121,12.5517380596833));
#80735=CARTESIAN_POINT('Ctrl Pts',(2.59032458202646,139.971814861545,12.6300231117368));
#80736=CARTESIAN_POINT('Ctrl Pts',(2.59606788310749,140.014407679925,12.6964550673818));
#80737=CARTESIAN_POINT('Ctrl Pts',(2.60641231920528,140.078182210739,12.8220076299135));
#80738=CARTESIAN_POINT('Ctrl Pts',(2.61097741341454,140.101890564828,12.8795333896135));
#80739=CARTESIAN_POINT('Ctrl Pts',(2.61622089572783,140.124739890963,12.9504178079355));
#80740=CARTESIAN_POINT('Ctrl Pts',(2.61708219075277,140.128343351051,12.9622295983991));
#80741=CARTESIAN_POINT('Ctrl Pts',(2.61846891045585,140.133908733837,12.9815564231586));
#80742=CARTESIAN_POINT('Ctrl Pts',(2.61900025170515,140.135983215132,12.9890378220453));
#80743=CARTESIAN_POINT('Ctrl Pts',(2.62008566264482,140.140103423939,13.0044887030572));
#80744=CARTESIAN_POINT('Ctrl Pts',(2.62063923220957,140.142139900528,13.0124600867968));
#80745=CARTESIAN_POINT('Ctrl Pts',(2.62216691417989,140.147571698341,13.034690582458));
#80746=CARTESIAN_POINT('Ctrl Pts',(2.62313146678731,140.150784746255,13.0489932158116));
#80747=CARTESIAN_POINT('Ctrl Pts',(2.62780971386251,140.165234984486,13.119442734379));
#80748=CARTESIAN_POINT('Ctrl Pts',(2.63136248784062,140.172635508967,13.1763032675171));
#80749=CARTESIAN_POINT('Ctrl Pts',(2.63834502554683,140.179012900032,13.2890392135396));
#80750=CARTESIAN_POINT('Ctrl Pts',(2.64176753553828,140.178214243876,13.344748063664));
#80751=CARTESIAN_POINT('Ctrl Pts',(2.64683311795144,140.171385549814,13.4247301074581));
#80752=CARTESIAN_POINT('Ctrl Pts',(2.64840284579948,140.168521104795,13.4491979201679));
#80753=CARTESIAN_POINT('Ctrl Pts',(2.65132723971652,140.161850757156,13.4939684569883));
#80754=CARTESIAN_POINT('Ctrl Pts',(2.65267497205706,140.158273842006,13.5142955145468));
#80755=CARTESIAN_POINT('Ctrl Pts',(2.65494318086267,140.151443266099,13.5479118654387));
#80756=CARTESIAN_POINT('Ctrl Pts',(2.65585408809344,140.148488699442,13.5612576673292));
#80757=CARTESIAN_POINT('Ctrl Pts',(2.65768956496284,140.142121125143,13.5878205437596));
#80758=CARTESIAN_POINT('Ctrl Pts',(2.65861397038254,140.138709272596,13.6010357040442));
#80759=CARTESIAN_POINT('Ctrl Pts',(2.66094726208514,140.129593504645,13.6339682748677));
#80760=CARTESIAN_POINT('Ctrl Pts',(2.66236519682339,140.123602553707,13.6536007685401));
#80761=CARTESIAN_POINT('Ctrl Pts',(2.669743135192,140.090154788374,13.7537562324198));
#80762=CARTESIAN_POINT('Ctrl Pts',(2.6759660382059,140.054548305496,13.8312771278612));
#80763=CARTESIAN_POINT('Ctrl Pts',(2.68508805045857,139.990827878354,13.9378776161496));
#80764=CARTESIAN_POINT('Ctrl Pts',(2.68795849905837,139.969077288269,13.9704604696807));
#80765=CARTESIAN_POINT('Ctrl Pts',(2.69196624158601,139.935899495469,14.0151643297314));
#80766=CARTESIAN_POINT('Ctrl Pts',(2.69314556178104,139.925777267946,14.0282200144966));
#80767=CARTESIAN_POINT('Ctrl Pts',(2.69523417996089,139.907150796955,14.0512281124043));
#80768=CARTESIAN_POINT('Ctrl Pts',(2.69614849047403,139.898749012578,14.061259806929));
#80769=CARTESIAN_POINT('Ctrl Pts',(2.6975976009109,139.885005722024,14.0771244539462));
#80770=CARTESIAN_POINT('Ctrl Pts',(2.69813930780114,139.87976983265,14.0830469956334));
#80771=CARTESIAN_POINT('Ctrl Pts',(2.69922270416607,139.869090664656,14.0948843173224));
#80772=CARTESIAN_POINT('Ctrl Pts',(2.69976423547238,139.863645701496,14.1007969612631));
#80773=CARTESIAN_POINT('Ctrl Pts',(2.70121841231904,139.848747508035,14.116646071639));
#80774=CARTESIAN_POINT('Ctrl Pts',(2.70212296075423,139.839180261047,14.1264742393575));
#80775=CARTESIAN_POINT('Ctrl Pts',(2.70747480747601,139.780931870744,14.1842565399776));
#80776=CARTESIAN_POINT('Ctrl Pts',(2.7116807756843,139.728318596275,14.2280724683605));
#80777=CARTESIAN_POINT('Ctrl Pts',(2.71896711854889,139.631494000551,14.2953730326502));
#80778=CARTESIAN_POINT('Ctrl Pts',(2.72203098029131,139.589047695657,14.321065410084));
#80779=CARTESIAN_POINT('Ctrl Pts',(2.72663659360722,139.524533514388,14.3547504607225));
#80780=CARTESIAN_POINT('Ctrl Pts',(2.72812006565005,139.503643737149,14.3648834815391));
#80781=CARTESIAN_POINT('Ctrl Pts',(2.7309023439459,139.464438134442,14.3824892423539));
#80782=CARTESIAN_POINT('Ctrl Pts',(2.73219538132343,139.446207106281,14.3901306732219));
#80783=CARTESIAN_POINT('Ctrl Pts',(2.734398854613,139.415195769642,14.4022206459882));
#80784=CARTESIAN_POINT('Ctrl Pts',(2.73530094314328,139.402515097274,14.4069143825244));
#80785=CARTESIAN_POINT('Ctrl Pts',(2.73703174222824,139.37823355822,14.4154297626416));
#80786=CARTESIAN_POINT('Ctrl Pts',(2.73785899297669,139.366648494687,14.4192913122783));
#80787=CARTESIAN_POINT('Ctrl Pts',(2.74005812356436,139.335919381437,14.4290057271924));
#80788=CARTESIAN_POINT('Ctrl Pts',(2.74143974328702,139.316683275063,14.4345516209504));
#80789=CARTESIAN_POINT('Ctrl Pts',(2.74904499861801,139.211237336399,14.4620618552608));
#80790=CARTESIAN_POINT('Ctrl Pts',(2.75556162124577,139.122904598153,14.4746906426126));
#80791=CARTESIAN_POINT('Ctrl Pts',(2.76482496490398,138.996786747674,14.4783342369882));
#80792=CARTESIAN_POINT('Ctrl Pts',(2.76755157684444,138.959530033395,14.4776435622599));
#80793=CARTESIAN_POINT('Ctrl Pts',(2.77138473949638,138.906344529368,14.4741301275034));
#80794=CARTESIAN_POINT('Ctrl Pts',(2.77253005615581,138.890344523968,14.4727440605465));
#80795=CARTESIAN_POINT('Ctrl Pts',(2.77456557616334,138.861635890586,14.4696643289929));
#80796=CARTESIAN_POINT('Ctrl Pts',(2.77546043949872,138.848917158788,14.468089584899));
#80797=CARTESIAN_POINT('Ctrl Pts',(2.77688682533256,138.828447362137,14.4652151971332));
#80798=CARTESIAN_POINT('Ctrl Pts',(2.7774248808188,138.820679458299,14.4640450670873));
#80799=CARTESIAN_POINT('Ctrl Pts',(2.77850912859651,138.804920066812,14.4615096188324));
#80800=CARTESIAN_POINT('Ctrl Pts',(2.77905504088709,138.796929871471,14.4601393483755));
#80801=CARTESIAN_POINT('Ctrl Pts',(2.78053546697373,138.775132086452,14.4561690499583));
#80802=CARTESIAN_POINT('Ctrl Pts',(2.78146137786792,138.761355407105,14.453404201376));
#80803=CARTESIAN_POINT('Ctrl Pts',(2.78657798172832,138.684661493557,14.4365793613153));
#80804=CARTESIAN_POINT('Ctrl Pts',(2.7905574157926,138.62292506064,14.4176168633181));
#80805=CARTESIAN_POINT('Ctrl Pts',(2.79773282293255,138.515097844997,14.3745375203155));
#80806=CARTESIAN_POINT('Ctrl Pts',(2.8009187210109,138.468463586943,14.3522497975832));
#80807=CARTESIAN_POINT('Ctrl Pts',(2.80568176338657,138.402766683406,14.3153668060605));
#80808=CARTESIAN_POINT('Ctrl Pts',(2.80719570560732,138.382445466318,14.3031369193902));
#80809=CARTESIAN_POINT('Ctrl Pts',(2.81002831548545,138.345627946676,14.2794362133505));
#80810=CARTESIAN_POINT('Ctrl Pts',(2.81134081580199,138.329029241261,14.268140611536));
#80811=CARTESIAN_POINT('Ctrl Pts',(2.81356733303682,138.301705141275,14.2485059820357));
#80812=CARTESIAN_POINT('Ctrl Pts',(2.81447257598025,138.290820386679,14.2403954262185));
#80813=CARTESIAN_POINT('Ctrl Pts',(2.81631096095968,138.269182197627,14.2236828261546));
#80814=CARTESIAN_POINT('Ctrl Pts',(2.81724417199555,138.258434625036,14.2150767127517));
#80815=CARTESIAN_POINT('Ctrl Pts',(2.81963021074647,138.23156623608,14.1927776365519));
#80816=CARTESIAN_POINT('Ctrl Pts',(2.82109295833759,138.215659456017,14.178835689056));
#80817=CARTESIAN_POINT('Ctrl Pts',(2.82809624855325,138.142188946103,14.1108564104354));
#80818=CARTESIAN_POINT('Ctrl Pts',(2.83385615181188,138.089787170954,14.0515562314469));
#80819=CARTESIAN_POINT('Ctrl Pts',(2.84410799879032,138.008321553379,13.9382366290328));
#80820=CARTESIAN_POINT('Ctrl Pts',(2.8485637062218,137.976777856709,13.8863359681887));
#80821=CARTESIAN_POINT('Ctrl Pts',(2.85375788054518,137.943499476499,13.8206442738174));
#80822=CARTESIAN_POINT('Ctrl Pts',(2.85466545471157,137.937820798617,13.8089589329466));
#80823=CARTESIAN_POINT('Ctrl Pts',(2.85610679578974,137.929006096192,13.7900299528661));
#80824=CARTESIAN_POINT('Ctrl Pts',(2.85664733617375,137.925747639733,13.7828448759772));
#80825=CARTESIAN_POINT('Ctrl Pts',(2.85773109774786,137.919306156813,13.7682529841614));
#80826=CARTESIAN_POINT('Ctrl Pts',(2.85827411959659,137.91612650171,13.7608451900794));
#80827=CARTESIAN_POINT('Ctrl Pts',(2.85973740429669,137.907698472623,13.7406401366959));
#80828=CARTESIAN_POINT('Ctrl Pts',(2.86064939361364,137.902598889426,13.7277817204549));
#80829=CARTESIAN_POINT('Ctrl Pts',(2.86229480890035,137.893710802472,13.7041649034555));
#80830=CARTESIAN_POINT('Ctrl Pts',(2.86303115989592,137.889850956811,13.6934387371489));
#80831=CARTESIAN_POINT('Ctrl Pts',(2.86376176824068,137.886148206833,13.6826607444707));
#80832=CARTESIAN_POINT('Origin',(1.13913288526384,139.,13.3));
#80833=CARTESIAN_POINT('',(3.46173780540502,137.886148220981,13.6826607856522));
#80834=CARTESIAN_POINT('',(3.36195598355709,137.886148212417,13.6826607607244));
#80835=CARTESIAN_POINT('',(1.13913288526384,137.88614821265,13.6826607614027));
#80836=CARTESIAN_POINT('Ctrl Pts',(3.46173780698925,137.886148221013,13.6826607857451));
#80837=CARTESIAN_POINT('Ctrl Pts',(3.45836838296447,137.903798630072,13.7340377239194));
#80838=CARTESIAN_POINT('Ctrl Pts',(3.4549629707539,137.924986636544,13.7841441124887));
#80839=CARTESIAN_POINT('Ctrl Pts',(3.45016111005712,137.958539568967,13.8503170867777));
#80840=CARTESIAN_POINT('Ctrl Pts',(3.44886346368914,137.967957637348,13.867782715661));
#80841=CARTESIAN_POINT('Ctrl Pts',(3.44665880860375,137.984502739928,13.8966924042346));
#80842=CARTESIAN_POINT('Ctrl Pts',(3.44576031457575,137.991393398323,13.9082673820296));
#80843=CARTESIAN_POINT('Ctrl Pts',(3.44393330418159,138.005689426144,13.9313709083526));
#80844=CARTESIAN_POINT('Ctrl Pts',(3.44300467975767,138.013100458757,13.9428934663466));
#80845=CARTESIAN_POINT('Ctrl Pts',(3.44062623712217,138.03243567786,13.9718331692168));
#80846=CARTESIAN_POINT('Ctrl Pts',(3.43916649497018,138.044629745427,13.9890632057143));
#80847=CARTESIAN_POINT('Ctrl Pts',(3.43375299313194,138.091009244744,14.0509975789069));
#80848=CARTESIAN_POINT('Ctrl Pts',(3.42969913269336,138.127919275501,14.0935586035251));
#80849=CARTESIAN_POINT('Ctrl Pts',(3.41950168214345,138.226636605513,14.1921528536077));
#80850=CARTESIAN_POINT('Ctrl Pts',(3.41330701396937,138.291623602701,14.2445802319252));
#80851=CARTESIAN_POINT('Ctrl Pts',(3.40651566562879,138.372527379974,14.2967659164351));
#80852=CARTESIAN_POINT('Ctrl Pts',(3.40560701895227,138.383572286705,14.3036339425661));
#80853=CARTESIAN_POINT('Ctrl Pts',(3.40416654812882,138.401471968,14.3143574513776));
#80854=CARTESIAN_POINT('Ctrl Pts',(3.40362790460698,138.408255242592,14.3183295128722));
#80855=CARTESIAN_POINT('Ctrl Pts',(3.40255137636818,138.422004684899,14.3261969425864));
#80856=CARTESIAN_POINT('Ctrl Pts',(3.4020136377026,138.428971667734,14.3300899972183));
#80857=CARTESIAN_POINT('Ctrl Pts',(3.40057142001163,138.447907618626,14.3404199801074));
#80858=CARTESIAN_POINT('Ctrl Pts',(3.39967488138512,138.459949676213,14.3467212711553));
#80859=CARTESIAN_POINT('Ctrl Pts',(3.39423534859957,138.53447122782,14.3840878500927));
#80860=CARTESIAN_POINT('Ctrl Pts',(3.38994529973612,138.599507540974,14.4097619971875));
#80861=CARTESIAN_POINT('Ctrl Pts',(3.38121794782789,138.734956449527,14.4497611357717));
#80862=CARTESIAN_POINT('Ctrl Pts',(3.37679391651474,138.805162748747,14.463716334325));
#80863=CARTESIAN_POINT('Ctrl Pts',(3.37088986772326,138.895867876636,14.4733042413624));
#80864=CARTESIAN_POINT('Ctrl Pts',(3.36959600343743,138.915587325411,14.4748875554781));
#80865=CARTESIAN_POINT('Ctrl Pts',(3.3673958482543,138.948775783991,14.4767124990439));
#80866=CARTESIAN_POINT('Ctrl Pts',(3.36649799012021,138.962226354736,14.4772210293705));
#80867=CARTESIAN_POINT('Ctrl Pts',(3.36467067810907,138.989392028937,14.4777820563403));
#80868=CARTESIAN_POINT('Ctrl Pts',(3.36374109055478,139.003105197759,14.4778257219704));
#80869=CARTESIAN_POINT('Ctrl Pts',(3.36135670714543,139.037990177743,14.4773275953248));
#80870=CARTESIAN_POINT('Ctrl Pts',(3.35989188592125,139.059151554218,14.4764542120358));
#80871=CARTESIAN_POINT('Ctrl Pts',(3.3529626225683,139.1579462292,14.4697045597161));
#80872=CARTESIAN_POINT('Ctrl Pts',(3.34728588692791,139.234886570133,14.4567110490137));
#80873=CARTESIAN_POINT('Ctrl Pts',(3.33840595325053,139.351515204987,14.4248940301977));
#80874=CARTESIAN_POINT('Ctrl Pts',(3.33524118673407,139.392409245801,14.4112897078416));
#80875=CARTESIAN_POINT('Ctrl Pts',(3.33088142890843,139.448642233739,14.3890902605491));
#80876=CARTESIAN_POINT('Ctrl Pts',(3.32963773032751,139.464674203836,14.3823471699356));
#80877=CARTESIAN_POINT('Ctrl Pts',(3.32744987806223,139.492946540754,14.3697116842225));
#80878=CARTESIAN_POINT('Ctrl Pts',(3.32650001641606,139.50524530785,14.3639579869557));
#80879=CARTESIAN_POINT('Ctrl Pts',(3.32501058194549,139.524608995583,14.3544876046362));
#80880=CARTESIAN_POINT('Ctrl Pts',(3.32446340574519,139.531739989095,14.3509097487427));
#80881=CARTESIAN_POINT('Ctrl Pts',(3.32338603398,139.545825820355,14.3436623291972));
#80882=CARTESIAN_POINT('Ctrl Pts',(3.32285575840621,139.55278132278,14.339995048269));
#80883=CARTESIAN_POINT('Ctrl Pts',(3.32145837865224,139.571152442221,14.3300725105765));
#80884=CARTESIAN_POINT('Ctrl Pts',(3.32059838025901,139.582502349165,14.3236969948901));
#80885=CARTESIAN_POINT('Ctrl Pts',(3.31482710664153,139.658755003209,14.2791850590484));
#80886=CARTESIAN_POINT('Ctrl Pts',(3.31021736387331,139.719985865332,14.2350854680397));
#80887=CARTESIAN_POINT('Ctrl Pts',(3.30163879361943,139.824311371667,14.1435842883494));
#80888=CARTESIAN_POINT('Ctrl Pts',(3.29769709531925,139.868563508873,14.0979473592663));
#80889=CARTESIAN_POINT('Ctrl Pts',(3.29221966239704,139.922578631638,14.0323967098507));
#80890=CARTESIAN_POINT('Ctrl Pts',(3.29081932656742,139.935779178061,14.0154533589605));
#80891=CARTESIAN_POINT('Ctrl Pts',(3.28849154127559,139.956670325095,13.9870709718419));
#80892=CARTESIAN_POINT('Ctrl Pts',(3.28757492063597,139.964636728147,13.9758406520039));
#80893=CARTESIAN_POINT('Ctrl Pts',(3.28576043245001,139.979886476013,13.953523863034));
#80894=CARTESIAN_POINT('Ctrl Pts',(3.28486324619194,139.987183036697,13.9424488870522));
#80895=CARTESIAN_POINT('Ctrl Pts',(3.28263558342335,140.004693778336,13.9148676214361));
#80896=CARTESIAN_POINT('Ctrl Pts',(3.28129737408778,140.014689558669,13.8982280514226));
#80897=CARTESIAN_POINT('Ctrl Pts',(3.27346485324006,140.070162278796,13.8004917436436));
#80898=CARTESIAN_POINT('Ctrl Pts',(3.26664388542069,140.10631187933,13.7144963522789));
#80899=CARTESIAN_POINT('Ctrl Pts',(3.25721729603795,140.14177476633,13.5910429590802));
#80900=CARTESIAN_POINT('Ctrl Pts',(3.25462110955812,140.150029680615,13.5564909711158));
#80901=CARTESIAN_POINT('Ctrl Pts',(3.2509494330637,140.159646245647,13.5062981698378));
#80902=CARTESIAN_POINT('Ctrl Pts',(3.24983796188384,140.162276798773,13.49092155693));
#80903=CARTESIAN_POINT('Ctrl Pts',(3.24785670157042,140.166467640818,13.4631109749276));
#80904=CARTESIAN_POINT('Ctrl Pts',(3.24698256610957,140.16813644254,13.4506958219219));
#80905=CARTESIAN_POINT('Ctrl Pts',(3.24558296370976,140.170518381318,13.4305452587776));
#80906=CARTESIAN_POINT('Ctrl Pts',(3.24505131614193,140.171353596489,13.4228255251882));
#80907=CARTESIAN_POINT('Ctrl Pts',(3.24397408217778,140.172903856802,13.4070382469128));
#80908=CARTESIAN_POINT('Ctrl Pts',(3.24342885740922,140.173612152311,13.3989705475416));
#80909=CARTESIAN_POINT('Ctrl Pts',(3.24194163928365,140.175330390584,13.3767735112108));
#80910=CARTESIAN_POINT('Ctrl Pts',(3.24100845544324,140.176168781239,13.3626317880328));
#80911=CARTESIAN_POINT('Ctrl Pts',(3.23593604413233,140.179373999623,13.2848279198774));
#80912=CARTESIAN_POINT('Ctrl Pts',(3.23200192620154,140.176827942798,13.221062715401));
#80913=CARTESIAN_POINT('Ctrl Pts',(3.22485021694789,140.16285605262,13.1061807304899));
#80914=CARTESIAN_POINT('Ctrl Pts',(3.22164194641489,140.153164000722,13.0550254956201));
#80915=CARTESIAN_POINT('Ctrl Pts',(3.21685223766466,140.1341637527,12.9816722612954));
#80916=CARTESIAN_POINT('Ctrl Pts',(3.21533502313076,140.127509213828,12.9588507142722));
#80917=CARTESIAN_POINT('Ctrl Pts',(3.2124986664702,140.113966252323,12.9171454586621));
#80918=CARTESIAN_POINT('Ctrl Pts',(3.21118576990382,140.10727611206,12.8982065887315));
#80919=CARTESIAN_POINT('Ctrl Pts',(3.20896293948137,140.095280046206,12.8668264881014));
#80920=CARTESIAN_POINT('Ctrl Pts',(3.20806185296122,140.090238021495,12.8542885442418));
#80921=CARTESIAN_POINT('Ctrl Pts',(3.20623587025286,140.079671968242,12.8292667465182));
#80922=CARTESIAN_POINT('Ctrl Pts',(3.20531096720339,140.074144406381,12.8167866704284));
#80923=CARTESIAN_POINT('Ctrl Pts',(3.20295553797155,140.059635614489,12.7855086262486));
#80924=CARTESIAN_POINT('Ctrl Pts',(3.20151547786178,140.050370522561,12.7668483533693));
#80925=CARTESIAN_POINT('Ctrl Pts',(3.19433579516952,140.002284031912,12.6761238902412));
#80926=CARTESIAN_POINT('Ctrl Pts',(3.18835678133591,139.956523142738,12.6080072330928));
#80927=CARTESIAN_POINT('Ctrl Pts',(3.17808917411832,139.866939104729,12.5007062524346));
#80928=CARTESIAN_POINT('Ctrl Pts',(3.17383654351491,139.826559592481,12.4590158547615));
#80929=CARTESIAN_POINT('Ctrl Pts',(3.16881717108323,139.773444214679,12.4117138599098));
#80930=CARTESIAN_POINT('Ctrl Pts',(3.16789740098424,139.763470720846,12.4031272583048));
#80931=CARTESIAN_POINT('Ctrl Pts',(3.16644372228409,139.747288857042,12.3896612139027));
#80932=CARTESIAN_POINT('Ctrl Pts',(3.16590278581643,139.741171992806,12.384674140957));
#80933=CARTESIAN_POINT('Ctrl Pts',(3.16482619341234,139.728796278721,12.3747896508646));
#80934=CARTESIAN_POINT('Ctrl Pts',(3.1642906185319,139.722537077851,12.3698933467504));
#80935=CARTESIAN_POINT('Ctrl Pts',(3.16286136406658,139.705572319966,12.3568971630647));
#80936=CARTESIAN_POINT('Ctrl Pts',(3.1619753812029,139.694776717644,12.3489160866601));
#80937=CARTESIAN_POINT('Ctrl Pts',(3.156425623832,139.625563384154,12.2995550209397));
#80938=CARTESIAN_POINT('Ctrl Pts',(3.15203005996752,139.563604428024,12.2633841995888));
#80939=CARTESIAN_POINT('Ctrl Pts',(3.14333910096303,139.436206454115,12.2038323834162));
#80940=CARTESIAN_POINT('Ctrl Pts',(3.13906025550019,139.371234114205,12.1801592256757));
#80941=CARTESIAN_POINT('Ctrl Pts',(3.13329083730982,139.285051533183,12.1570875697915));
#80942=CARTESIAN_POINT('Ctrl Pts',(3.13197047012983,139.265406149983,12.1523664798762));
#80943=CARTESIAN_POINT('Ctrl Pts',(3.1297387185587,139.232413100441,12.1453301782094));
#80944=CARTESIAN_POINT('Ctrl Pts',(3.12883634579817,139.219129036005,12.142735688635));
#80945=CARTESIAN_POINT('Ctrl Pts',(3.127010759545,139.192387944015,12.1379898486125));
#80946=CARTESIAN_POINT('Ctrl Pts',(3.12608758758131,139.178932431487,12.1358419906512));
#80947=CARTESIAN_POINT('Ctrl Pts',(3.12374290479611,139.144945382887,12.1310198824146));
#80948=CARTESIAN_POINT('Ctrl Pts',(3.12231204065755,139.124375696271,12.1286527965437));
#80949=CARTESIAN_POINT('Ctrl Pts',(3.11505855702339,139.021014221465,12.1195114928741));
#80950=CARTESIAN_POINT('Ctrl Pts',(3.1089878774016,138.937743712085,12.1209688224316));
#80951=CARTESIAN_POINT('Ctrl Pts',(3.09869023911081,138.798610077406,12.138189292158));
#80952=CARTESIAN_POINT('Ctrl Pts',(3.09449856238143,138.742466710349,12.1493307189832));
#80953=CARTESIAN_POINT('Ctrl Pts',(3.08954210526601,138.67473893858,12.1679790599948));
#80954=CARTESIAN_POINT('Ctrl Pts',(3.08862797395389,138.662185632882,12.1716615507934));
#80955=CARTESIAN_POINT('Ctrl Pts',(3.08718099203487,138.642176414888,12.1778951160327));
#80956=CARTESIAN_POINT('Ctrl Pts',(3.08664121942925,138.634680558193,12.180313077565));
#80957=CARTESIAN_POINT('Ctrl Pts',(3.08556467203787,138.61965526003,12.185326793539));
#80958=CARTESIAN_POINT('Ctrl Pts',(3.08502801103589,138.612126783704,12.1879240782118));
#80959=CARTESIAN_POINT('Ctrl Pts',(3.08359225929201,138.591902064861,12.1951318769706));
#80960=CARTESIAN_POINT('Ctrl Pts',(3.08270098694365,138.579257439121,12.1998849015177));
#80961=CARTESIAN_POINT('Ctrl Pts',(3.07720264407398,138.500920871212,12.2308794096361));
#80962=CARTESIAN_POINT('Ctrl Pts',(3.07285651860873,138.43761494184,12.2627804745131));
#80963=CARTESIAN_POINT('Ctrl Pts',(3.06411762173651,138.317566322302,12.3375179041533));
#80964=CARTESIAN_POINT('Ctrl Pts',(3.05973944968749,138.261071989804,12.3801785864653));
#80965=CARTESIAN_POINT('Ctrl Pts',(3.05388674823547,138.194102149079,12.4409223129584));
#80966=CARTESIAN_POINT('Ctrl Pts',(3.05259371580389,138.179797767602,12.4545687240624));
#80967=CARTESIAN_POINT('Ctrl Pts',(3.05039454783694,138.156343957378,12.4780993698694));
#80968=CARTESIAN_POINT('Ctrl Pts',(3.04949682700704,138.147008125544,12.4877925137365));
#80969=CARTESIAN_POINT('Ctrl Pts',(3.04766943956062,138.12849675394,12.5076836015772));
#80970=CARTESIAN_POINT('Ctrl Pts',(3.04673963356958,138.11932922425,12.5178861079576));
#80971=CARTESIAN_POINT('Ctrl Pts',(3.04435391411528,138.096455146639,12.5442547438014));
#80972=CARTESIAN_POINT('Ctrl Pts',(3.04288795252716,138.083003477047,12.5606344138111));
#80973=CARTESIAN_POINT('Ctrl Pts',(3.03738147642545,138.03472191734,12.622770764814));
#80974=CARTESIAN_POINT('Ctrl Pts',(3.03323581444742,138.002819103006,12.6706909550478));
#80975=CARTESIAN_POINT('Ctrl Pts',(3.02303387021577,137.93420670332,12.7921548859122));
#80976=CARTESIAN_POINT('Ctrl Pts',(3.01693586612402,137.901435833194,12.8675880044185));
#80977=CARTESIAN_POINT('Ctrl Pts',(3.01023981030961,137.872882901291,12.9581388769779));
#80978=CARTESIAN_POINT('Ctrl Pts',(3.00933727578236,137.869200383165,12.9705242908488));
#80979=CARTESIAN_POINT('Ctrl Pts',(3.00790405585608,137.863611049326,12.9905218478332));
#80980=CARTESIAN_POINT('Ctrl Pts',(3.00736666509325,137.861575270655,12.9980965050352));
#80981=CARTESIAN_POINT('Ctrl Pts',(3.0062901193871,137.857616142088,13.0134372999262));
#80982=CARTESIAN_POINT('Ctrl Pts',(3.00575114704534,137.855695957887,13.021203786753));
#80983=CARTESIAN_POINT('Ctrl Pts',(3.00430151962512,137.850706174465,13.0423063484932));
#80984=CARTESIAN_POINT('Ctrl Pts',(3.00339894570211,137.847789517265,13.0556777562563));
#80985=CARTESIAN_POINT('Ctrl Pts',(2.9980588046626,137.831739586346,13.1359539549935));
#80986=CARTESIAN_POINT('Ctrl Pts',(2.99386158844297,137.824201746464,13.2038531112635));
#80987=CARTESIAN_POINT('Ctrl Pts',(2.98507619683986,137.820825215976,13.3459900454161));
#80988=CARTESIAN_POINT('Ctrl Pts',(2.98049928156362,137.826040736481,13.4199428737051));
#80989=CARTESIAN_POINT('Ctrl Pts',(2.9744562608184,137.841314131111,13.5119283728539));
#80990=CARTESIAN_POINT('Ctrl Pts',(2.97319422149151,137.84493744974,13.5308614603078));
#80991=CARTESIAN_POINT('Ctrl Pts',(2.97103179804789,137.851858618572,13.5627646291086));
#80992=CARTESIAN_POINT('Ctrl Pts',(2.97013916613176,137.854915965702,13.5757832689906));
#80993=CARTESIAN_POINT('Ctrl Pts',(2.96841900833703,137.861183027981,13.6005654422242));
#80994=CARTESIAN_POINT('Ctrl Pts',(2.96759280119882,137.864355071985,13.6123367714931));
#80995=CARTESIAN_POINT('Ctrl Pts',(2.96537867397912,137.873279503437,13.6435197784572));
#80996=CARTESIAN_POINT('Ctrl Pts',(2.96398063800157,137.879350437252,13.6628352031284));
#80997=CARTESIAN_POINT('Ctrl Pts',(2.96255039632898,137.88599320387,13.6822093374455));
#80998=CARTESIAN_POINT('Ctrl Pts',(2.96253372896323,137.886070674307,13.6824350622175));
#80999=CARTESIAN_POINT('Ctrl Pts',(2.96251705962155,137.886148212665,13.6826607614475));
#81000=CARTESIAN_POINT('Ctrl Pts',(2.86376176824068,137.886148206833,13.6826607444707));
#81001=CARTESIAN_POINT('Ctrl Pts',(2.86725567767849,137.868440945227,13.6311183132772));
#81002=CARTESIAN_POINT('Ctrl Pts',(2.87062046861302,137.854326414844,13.5783907776995));
#81003=CARTESIAN_POINT('Ctrl Pts',(2.87713906771859,137.834185868406,13.4748394318849));
#81004=CARTESIAN_POINT('Ctrl Pts',(2.88028484405678,137.82771416093,13.4242454806967));
#81005=CARTESIAN_POINT('Ctrl Pts',(2.88499619080121,137.823071471942,13.3498891616564));
#81006=CARTESIAN_POINT('Ctrl Pts',(2.88650018847356,137.822309281961,13.3263468935304));
#81007=CARTESIAN_POINT('Ctrl Pts',(2.88931634634091,137.822205861884,13.2828247150978));
#81008=CARTESIAN_POINT('Ctrl Pts',(2.89062246892688,137.822666525777,13.2628538517397));
#81009=CARTESIAN_POINT('Ctrl Pts',(2.892841326005,137.824291837794,13.2293663373899));
#81010=CARTESIAN_POINT('Ctrl Pts',(2.89374542417892,137.825182605914,13.2158402617338));
#81011=CARTESIAN_POINT('Ctrl Pts',(2.89558407723261,137.82744997144,13.1885926453274));
#81012=CARTESIAN_POINT('Ctrl Pts',(2.89651874310581,137.828834509547,13.1748739277128));
#81013=CARTESIAN_POINT('Ctrl Pts',(2.8989141149303,137.832965523065,13.1400698801915));
#81014=CARTESIAN_POINT('Ctrl Pts',(2.90038490369175,137.836042643655,13.1190296045035));
#81015=CARTESIAN_POINT('Ctrl Pts',(2.90728800563884,137.852953535013,13.0218503576638));
#81016=CARTESIAN_POINT('Ctrl Pts',(2.91292945815507,137.87369859987,12.9471198244522));
#81017=CARTESIAN_POINT('Ctrl Pts',(2.9230931726133,137.923632998348,12.8180751906311));
#81018=CARTESIAN_POINT('Ctrl Pts',(2.92757963674675,137.950040652123,12.7629673611171));
#81019=CARTESIAN_POINT('Ctrl Pts',(2.93284330922091,137.987363313571,12.6984650745539));
#81020=CARTESIAN_POINT('Ctrl Pts',(2.93378764430336,137.994325513776,12.6868962631589));
#81021=CARTESIAN_POINT('Ctrl Pts',(2.93527260690719,138.005724024588,12.6686726417028));
#81022=CARTESIAN_POINT('Ctrl Pts',(2.93582070534413,138.010031613605,12.6619392254268));
#81023=CARTESIAN_POINT('Ctrl Pts',(2.93683893748925,138.018229610334,12.6494074182241));
#81024=CARTESIAN_POINT('Ctrl Pts',(2.93731013035026,138.022103634643,12.6435988192708));
#81025=CARTESIAN_POINT('Ctrl Pts',(2.93859937393458,138.032918134826,12.6276921408359));
#81026=CARTESIAN_POINT('Ctrl Pts',(2.9394106703059,138.039965112964,12.6176670631507));
#81027=CARTESIAN_POINT('Ctrl Pts',(2.94423117158354,138.083200826815,12.5581559250762));
#81028=CARTESIAN_POINT('Ctrl Pts',(2.94803691158806,138.123056303952,12.5114411958815));
#81029=CARTESIAN_POINT('Ctrl Pts',(2.95528846212442,138.205882640744,12.4284490964462));
#81030=CARTESIAN_POINT('Ctrl Pts',(2.95872792589386,138.248161375517,12.3917259884215));
#81031=CARTESIAN_POINT('Ctrl Pts',(2.96381525364608,138.312636962533,12.3433197910511));
#81032=CARTESIAN_POINT('Ctrl Pts',(2.96538906575527,138.332847143474,12.3291179687968));
#81033=CARTESIAN_POINT('Ctrl Pts',(2.96832033726247,138.370773429674,12.3042105425882));
#81034=CARTESIAN_POINT('Ctrl Pts',(2.96967081299137,138.388354052668,12.2933163995666));
#81035=CARTESIAN_POINT('Ctrl Pts',(2.97194270105114,138.418027383992,12.2759930980345));
#81036=CARTESIAN_POINT('Ctrl Pts',(2.97285449386152,138.429962113949,12.2693016722268));
#81037=CARTESIAN_POINT('Ctrl Pts',(2.97469106963597,138.454032240892,12.2563522498827));
#81038=CARTESIAN_POINT('Ctrl Pts',(2.97561567689895,138.466165267372,12.2500943512662));
#81039=CARTESIAN_POINT('Ctrl Pts',(2.97794818804247,138.496792909123,12.2349655636982));
#81040=CARTESIAN_POINT('Ctrl Pts',(2.97936510920751,138.515414985312,12.2263645877426));
#81041=CARTESIAN_POINT('Ctrl Pts',(2.98674826259363,138.612474285438,12.1845754024765));
#81042=CARTESIAN_POINT('Ctrl Pts',(2.99297793832906,138.694107739314,12.1594854405036));
#81043=CARTESIAN_POINT('Ctrl Pts',(3.00210023764756,138.81608290532,12.1360429606042));
#81044=CARTESIAN_POINT('Ctrl Pts',(3.00496449352447,138.854795268941,12.1305824669314));
#81045=CARTESIAN_POINT('Ctrl Pts',(3.00896490474615,138.910141794031,12.125567022961));
#81046=CARTESIAN_POINT('Ctrl Pts',(3.01014290383602,138.926604861565,12.124423323036));
#81047=CARTESIAN_POINT('Ctrl Pts',(3.01222956436317,138.956146998181,12.1229940819346));
#81048=CARTESIAN_POINT('Ctrl Pts',(3.01314321927118,138.969216991939,12.1225797440055));
#81049=CARTESIAN_POINT('Ctrl Pts',(3.01459178329804,138.990197096921,12.1222642601981));
#81050=CARTESIAN_POINT('Ctrl Pts',(3.0151335793853,138.998103691501,12.1222249856122));
#81051=CARTESIAN_POINT('Ctrl Pts',(3.01621736838379,139.014052370774,12.1223063776968));
#81052=CARTESIAN_POINT('Ctrl Pts',(3.01675919825521,139.022093986797,12.1224297887329));
#81053=CARTESIAN_POINT('Ctrl Pts',(3.01821521393192,139.043867219511,12.1229870628074));
#81054=CARTESIAN_POINT('Ctrl Pts',(3.01912126697991,139.057593972395,12.1235788330994));
#81055=CARTESIAN_POINT('Ctrl Pts',(3.02443280326578,139.138879148907,12.1285093636998));
#81056=CARTESIAN_POINT('Ctrl Pts',(3.02860177066926,139.205979646122,12.1384267861221));
#81057=CARTESIAN_POINT('Ctrl Pts',(3.03587154333044,139.320451898672,12.1655841039019));
#81058=CARTESIAN_POINT('Ctrl Pts',(3.03895721604081,139.368256843347,12.180189590136));
#81059=CARTESIAN_POINT('Ctrl Pts',(3.04359096529599,139.436797037097,12.2059952215988));
#81060=CARTESIAN_POINT('Ctrl Pts',(3.04507989190951,139.45835620476,12.2148513481974));
#81061=CARTESIAN_POINT('Ctrl Pts',(3.04787113758353,139.497739910478,12.232412582544));
#81062=CARTESIAN_POINT('Ctrl Pts',(3.04916761574667,139.515634685109,12.2409397046497));
#81063=CARTESIAN_POINT('Ctrl Pts',(3.05137504973147,139.54536716872,12.2560398771981));
#81064=CARTESIAN_POINT('Ctrl Pts',(3.05227758045623,139.557322461036,12.2623730269015));
#81065=CARTESIAN_POINT('Ctrl Pts',(3.05411717887723,139.581267379282,12.2755907191006));
#81066=CARTESIAN_POINT('Ctrl Pts',(3.05505442439103,139.593250139573,12.2824832264138));
#81067=CARTESIAN_POINT('Ctrl Pts',(3.05746550176222,139.623509289031,12.3006045539693));
#81068=CARTESIAN_POINT('Ctrl Pts',(3.05894968522338,139.641604608392,12.3121242422439));
#81069=CARTESIAN_POINT('Ctrl Pts',(3.06554215939757,139.719627556223,12.3648427175057));
#81070=CARTESIAN_POINT('Ctrl Pts',(3.07083120899781,139.775971951013,12.4110413421109));
#81071=CARTESIAN_POINT('Ctrl Pts',(3.08102015697254,139.874688967301,12.5085590680788));
#81072=CARTESIAN_POINT('Ctrl Pts',(3.08589031281501,139.917701954065,12.5588629897604));
#81073=CARTESIAN_POINT('Ctrl Pts',(3.09147544082007,139.963911016168,12.623138209892));
#81074=CARTESIAN_POINT('Ctrl Pts',(3.09238996024387,139.971373009591,12.6338912684786));
#81075=CARTESIAN_POINT('Ctrl Pts',(3.09383953643681,139.983054365944,12.6513385176718));
#81076=CARTESIAN_POINT('Ctrl Pts',(3.0943814968792,139.987388028676,12.6579544434954));
#81077=CARTESIAN_POINT('Ctrl Pts',(3.09546525106988,139.995991877487,12.6713825741562));
#81078=CARTESIAN_POINT('Ctrl Pts',(3.09600688713132,140.000259596855,12.6781958213678));
#81079=CARTESIAN_POINT('Ctrl Pts',(3.09746176495002,140.011622790804,12.6967565012132));
#81080=CARTESIAN_POINT('Ctrl Pts',(3.09836689536958,140.018583480987,12.7085854903961));
#81081=CARTESIAN_POINT('Ctrl Pts',(3.1037043528733,140.058844002044,12.7798244821335));
#81082=CARTESIAN_POINT('Ctrl Pts',(3.10789707547799,140.087150147747,12.841917041871));
#81083=CARTESIAN_POINT('Ctrl Pts',(3.11660390358061,140.134274451286,12.974708996856));
#81084=CARTESIAN_POINT('Ctrl Pts',(3.12110633430577,140.152203248312,13.0454043933486));
#81085=CARTESIAN_POINT('Ctrl Pts',(3.12710258391186,140.166575295225,13.1369293866387));
#81086=CARTESIAN_POINT('Ctrl Pts',(3.1284022787735,140.169160448075,13.1566343284718));
#81087=CARTESIAN_POINT('Ctrl Pts',(3.130613529084,140.172666559752,13.1898570665235));
#81088=CARTESIAN_POINT('Ctrl Pts',(3.13151658938389,140.173855052481,13.2033427910992));
#81089=CARTESIAN_POINT('Ctrl Pts',(3.13335588486105,140.1757859432,13.2306225227783));
#81090=CARTESIAN_POINT('Ctrl Pts',(3.13429227554078,140.176518637259,13.2444150519524));
#81091=CARTESIAN_POINT('Ctrl Pts',(3.13669811018278,140.177767300632,13.2795891609969));
#81092=CARTESIAN_POINT('Ctrl Pts',(3.13817781536176,140.177943699201,13.3009769358588));
#81093=CARTESIAN_POINT('Ctrl Pts',(3.14492597166112,140.176113793225,13.3973598105194));
#81094=CARTESIAN_POINT('Ctrl Pts',(3.15038878228982,140.16752732199,13.4720444052847));
#81095=CARTESIAN_POINT('Ctrl Pts',(3.15918286321279,140.142578784104,13.5891553028662));
#81096=CARTESIAN_POINT('Ctrl Pts',(3.1624741893984,140.130769465302,13.6323519161863));
#81097=CARTESIAN_POINT('Ctrl Pts',(3.16698646687943,140.110873191644,13.6916272156261));
#81098=CARTESIAN_POINT('Ctrl Pts',(3.16825890618291,140.104834800466,13.7083518745864));
#81099=CARTESIAN_POINT('Ctrl Pts',(3.17049235453672,140.093435330735,13.7378185588005));
#81100=CARTESIAN_POINT('Ctrl Pts',(3.17145936623848,140.088224315112,13.7506149071824));
#81101=CARTESIAN_POINT('Ctrl Pts',(3.17297126890723,140.079619191058,13.7707253903087));
#81102=CARTESIAN_POINT('Ctrl Pts',(3.17352407284625,140.07637325241,13.7781010583297));
#81103=CARTESIAN_POINT('Ctrl Pts',(3.17460907842506,140.069798816063,13.7926335759461));
#81104=CARTESIAN_POINT('Ctrl Pts',(3.17514140838906,140.066473596856,13.7997913779438));
#81105=CARTESIAN_POINT('Ctrl Pts',(3.17654017180158,140.057478845261,13.818654701699));
#81106=CARTESIAN_POINT('Ctrl Pts',(3.17739954485955,140.051686754446,13.8303010588967));
#81107=CARTESIAN_POINT('Ctrl Pts',(3.18319503653078,140.010899055936,13.9090162568064));
#81108=CARTESIAN_POINT('Ctrl Pts',(3.18782625949251,139.96970051007,13.9726823967365));
#81109=CARTESIAN_POINT('Ctrl Pts',(3.19641049371281,139.883404792626,14.0814623062347));
#81110=CARTESIAN_POINT('Ctrl Pts',(3.20033522734364,139.840220335692,14.1277173593056));
#81111=CARTESIAN_POINT('Ctrl Pts',(3.2057955295871,139.777654015267,14.1847662548646));
#81112=CARTESIAN_POINT('Ctrl Pts',(3.2071971611452,139.761377998941,14.1988106265807));
#81113=CARTESIAN_POINT('Ctrl Pts',(3.20953050962994,139.734012143579,14.2211474117913));
#81114=CARTESIAN_POINT('Ctrl Pts',(3.21045142993331,139.72314382849,14.2297039082591));
#81115=CARTESIAN_POINT('Ctrl Pts',(3.21227731070719,139.701482611836,14.2461478909197));
#81116=CARTESIAN_POINT('Ctrl Pts',(3.21318162661513,139.690701116982,14.2540469734759));
#81117=CARTESIAN_POINT('Ctrl Pts',(3.21543335115408,139.663740597074,14.2731031039808));
#81118=CARTESIAN_POINT('Ctrl Pts',(3.21678875017656,139.647412817364,14.2840415611368));
#81119=CARTESIAN_POINT('Ctrl Pts',(3.22454817257749,139.553442105099,14.3436440393997));
#81120=CARTESIAN_POINT('Ctrl Pts',(3.23126726862673,139.470613359239,14.3835166309028));
#81121=CARTESIAN_POINT('Ctrl Pts',(3.24063725328227,139.349936070279,14.4251399231868));
#81122=CARTESIAN_POINT('Ctrl Pts',(3.24327494504001,139.315326856751,14.4353256545533));
#81123=CARTESIAN_POINT('Ctrl Pts',(3.24699933282617,139.264994642047,14.4476590642556));
#81124=CARTESIAN_POINT('Ctrl Pts',(3.2481228561815,139.249611481914,14.4511027953175));
#81125=CARTESIAN_POINT('Ctrl Pts',(3.25012410412826,139.221777515382,14.4567495461543));
#81126=CARTESIAN_POINT('Ctrl Pts',(3.25100627506426,139.209351642828,14.4590628547352));
#81127=CARTESIAN_POINT('Ctrl Pts',(3.25241755901399,139.189181689514,14.4624828955083));
#81128=CARTESIAN_POINT('Ctrl Pts',(3.25295297300493,139.181459857275,14.4637132492362));
#81129=CARTESIAN_POINT('Ctrl Pts',(3.25403740322027,139.165665589892,14.4660687755178));
#81130=CARTESIAN_POINT('Ctrl Pts',(3.25458605855115,139.157592672277,14.4671872328251));
#81131=CARTESIAN_POINT('Ctrl Pts',(3.25608317894581,139.135360394056,14.4700325096001));
#81132=CARTESIAN_POINT('Ctrl Pts',(3.25702271025748,139.121179785555,14.4715861103672));
#81133=CARTESIAN_POINT('Ctrl Pts',(3.26206992472539,139.043999212449,14.4786254307757));
#81134=CARTESIAN_POINT('Ctrl Pts',(3.26597626222497,138.980656890449,14.4792885652085));
#81135=CARTESIAN_POINT('Ctrl Pts',(3.27310977456839,138.865508511641,14.4712087642711));
#81136=CARTESIAN_POINT('Ctrl Pts',(3.27632805108019,138.813757416287,14.4641010452671));
#81137=CARTESIAN_POINT('Ctrl Pts',(3.28113272894299,138.739296470765,14.4487807598787));
#81138=CARTESIAN_POINT('Ctrl Pts',(3.28265458379954,138.716094883765,14.4432678355518));
#81139=CARTESIAN_POINT('Ctrl Pts',(3.28550025631884,138.673618388168,14.431802260449));
#81140=CARTESIAN_POINT('Ctrl Pts',(3.28681780100397,138.654298223247,14.4260512939375));
#81141=CARTESIAN_POINT('Ctrl Pts',(3.28905030627665,138.622216897484,14.4155983204253));
#81142=CARTESIAN_POINT('Ctrl Pts',(3.28995638114752,138.609372076202,14.4111658220458));
#81143=CARTESIAN_POINT('Ctrl Pts',(3.29179435789067,138.583688219458,14.4018024539359));
#81144=CARTESIAN_POINT('Ctrl Pts',(3.29272629481365,138.570853160238,14.3968669509632));
#81145=CARTESIAN_POINT('Ctrl Pts',(3.29510456870969,138.538589229407,14.3838074376025));
#81146=CARTESIAN_POINT('Ctrl Pts',(3.29656069414595,138.519287112543,14.3753852712255));
#81147=CARTESIAN_POINT('Ctrl Pts',(3.30363154586529,138.427758085779,14.3324914178884));
#81148=CARTESIAN_POINT('Ctrl Pts',(3.30947288778961,138.358954888242,14.2912399278952));
#81149=CARTESIAN_POINT('Ctrl Pts',(3.31976884540246,138.246687697056,14.2073230276489));
#81150=CARTESIAN_POINT('Ctrl Pts',(3.32418713544667,138.20132626255,14.1676612575244));
#81151=CARTESIAN_POINT('Ctrl Pts',(3.3293289804994,138.15024866075,14.1155861806615));
#81152=CARTESIAN_POINT('Ctrl Pts',(3.33022072606745,138.141454474181,14.106323613946));
#81153=CARTESIAN_POINT('Ctrl Pts',(3.33164332530257,138.127504042292,14.0911431025031));
#81154=CARTESIAN_POINT('Ctrl Pts',(3.33218065729488,138.122253423961,14.0853136729776));
#81155=CARTESIAN_POINT('Ctrl Pts',(3.33326475098052,138.111690696451,14.0733482380002));
#81156=CARTESIAN_POINT('Ctrl Pts',(3.33381121399088,138.106383020429,14.067208980407));
#81157=CARTESIAN_POINT('Ctrl Pts',(3.33529511167421,138.092031858323,14.0502583324014));
#81158=CARTESIAN_POINT('Ctrl Pts',(3.33622387349157,138.083118013998,14.0393383383797));
#81159=CARTESIAN_POINT('Ctrl Pts',(3.34108484292572,138.036986249448,13.9807061839521));
#81160=CARTESIAN_POINT('Ctrl Pts',(3.34483233938821,138.003286588448,13.9303335909428));
#81161=CARTESIAN_POINT('Ctrl Pts',(3.35192145539169,137.947047072064,13.8303940708217));
#81162=CARTESIAN_POINT('Ctrl Pts',(3.35525618173679,137.923776416898,13.7814251357171));
#81163=CARTESIAN_POINT('Ctrl Pts',(3.35976079208708,137.897668992085,13.7150382436852));
#81164=CARTESIAN_POINT('Ctrl Pts',(3.36085355029375,137.891730902631,13.6989108969421));
#81165=CARTESIAN_POINT('Ctrl Pts',(3.36195598355709,137.886148212184,13.682660760046));
#81166=CARTESIAN_POINT('Origin',(1.13913288526384,139.,13.3));
#81167=CARTESIAN_POINT('',(3.96044919307343,137.886148212663,13.6826607614402));
#81168=CARTESIAN_POINT('',(3.86234166189399,137.886148208814,13.6826607502373));
#81169=CARTESIAN_POINT('',(1.13913288526384,137.88614821265,13.6826607614027));
#81170=CARTESIAN_POINT('',(3.48683023682326,137.822250041178,13.300311439502));
#81171=CARTESIAN_POINT('Ctrl Pts',(3.96044919307343,137.886148212676,13.6826607614778));
#81172=CARTESIAN_POINT('Ctrl Pts',(3.96015776463529,137.887508143234,13.6866192574491));
#81173=CARTESIAN_POINT('Ctrl Pts',(3.9598673740692,137.888889210441,13.6905706046321));
#81174=CARTESIAN_POINT('Ctrl Pts',(3.95902514688492,137.892971474364,13.7020533816354));
#81175=CARTESIAN_POINT('Ctrl Pts',(3.95847628523608,137.895728441424,13.7095649065459));
#81176=CARTESIAN_POINT('Ctrl Pts',(3.95739856836759,137.901338771655,13.7243819812995));
#81177=CARTESIAN_POINT('Ctrl Pts',(3.9568695917225,137.904188957588,13.7316882291937));
#81178=CARTESIAN_POINT('Ctrl Pts',(3.95548012561848,137.911925627858,13.7509501318349));
#81179=CARTESIAN_POINT('Ctrl Pts',(3.95462659678981,137.916936314258,13.7628552121782));
#81180=CARTESIAN_POINT('Ctrl Pts',(3.95004470906071,137.945179112336,13.8269867884242));
#81181=CARTESIAN_POINT('Ctrl Pts',(3.94648761168793,137.971996572454,13.8775575001408));
#81182=CARTESIAN_POINT('Ctrl Pts',(3.93778423811119,138.046745328549,13.996682584095));
#81183=CARTESIAN_POINT('Ctrl Pts',(3.93266995385278,138.098491056627,14.0624573599495));
#81184=CARTESIAN_POINT('Ctrl Pts',(3.92594424512489,138.171173226379,14.136999392843));
#81185=CARTESIAN_POINT('Ctrl Pts',(3.92459527004339,138.185980641409,14.1514071907126));
#81186=CARTESIAN_POINT('Ctrl Pts',(3.92232926683204,138.211164474853,14.1746536465654));
#81187=CARTESIAN_POINT('Ctrl Pts',(3.92142188797792,138.22132943502,14.1837152325005));
#81188=CARTESIAN_POINT('Ctrl Pts',(3.91959724557429,138.241912327093,14.201433045302));
#81189=CARTESIAN_POINT('Ctrl Pts',(3.91868020238066,138.252327007952,14.2100898446223));
#81190=CARTESIAN_POINT('Ctrl Pts',(3.9163738095617,138.278678201926,14.2312356291197));
#81191=CARTESIAN_POINT('Ctrl Pts',(3.91497574236692,138.294791303743,14.2434964438661));
#81192=CARTESIAN_POINT('Ctrl Pts',(3.90857607814368,138.369128731626,14.2970930849324));
#81193=CARTESIAN_POINT('Ctrl Pts',(3.90339699772107,138.430714388301,14.3334912300905));
#81194=CARTESIAN_POINT('Ctrl Pts',(3.89311766151282,138.557269618509,14.3935280693941));
#81195=CARTESIAN_POINT('Ctrl Pts',(3.88804368875238,138.621794456477,14.4174863569865));
#81196=CARTESIAN_POINT('Ctrl Pts',(3.88222344565931,138.701215876073,14.4393022889455));
#81197=CARTESIAN_POINT('Ctrl Pts',(3.88126754943301,138.714450664671,14.4426912425384));
#81198=CARTESIAN_POINT('Ctrl Pts',(3.87977095098395,138.735520494207,14.4476975091276));
#81199=CARTESIAN_POINT('Ctrl Pts',(3.87922252781066,138.743317783362,14.4494664982435));
#81200=CARTESIAN_POINT('Ctrl Pts',(3.87814490592969,138.758802919911,14.4528142139738));
#81201=CARTESIAN_POINT('Ctrl Pts',(3.87761559652486,138.766489678663,14.4543957642497));
#81202=CARTESIAN_POINT('Ctrl Pts',(3.8762240980337,138.786892901242,14.45838158592));
#81203=CARTESIAN_POINT('Ctrl Pts',(3.87536890679318,138.79963458745,14.4606533805918));
#81204=CARTESIAN_POINT('Ctrl Pts',(3.87058201000085,138.871916405253,14.4723150692809));
#81205=CARTESIAN_POINT('Ctrl Pts',(3.86684152384165,138.93207770322,14.4773344184108));
#81206=CARTESIAN_POINT('Ctrl Pts',(3.85819792898884,139.071844141519,14.4782405035428));
#81207=CARTESIAN_POINT('Ctrl Pts',(3.85331561147581,139.151163420014,14.4707093713224));
#81208=CARTESIAN_POINT('Ctrl Pts',(3.84682729065043,139.249766186659,14.4511538051818));
#81209=CARTESIAN_POINT('Ctrl Pts',(3.84545358254944,139.270300942082,14.4465057974875));
#81210=CARTESIAN_POINT('Ctrl Pts',(3.843157867969,139.303965112743,14.4379313141833));
#81211=CARTESIAN_POINT('Ctrl Pts',(3.84224607310668,139.317170664146,14.4343214750324));
#81212=CARTESIAN_POINT('Ctrl Pts',(3.84042158748146,139.343247417855,14.4267022424632));
#81213=CARTESIAN_POINT('Ctrl Pts',(3.8395092642167,139.356118658441,14.4227004087814));
#81214=CARTESIAN_POINT('Ctrl Pts',(3.83723270299145,139.387804862289,14.4122490619253));
#81215=CARTESIAN_POINT('Ctrl Pts',(3.83586023482043,139.406529892719,14.4055423779088));
#81216=CARTESIAN_POINT('Ctrl Pts',(3.82960759071628,139.490101878828,14.3731994202034));
#81217=CARTESIAN_POINT('Ctrl Pts',(3.82455807089613,139.552755321523,14.3423126266406));
#81218=CARTESIAN_POINT('Ctrl Pts',(3.8141963485541,139.673431807308,14.2688683247508));
#81219=CARTESIAN_POINT('Ctrl Pts',(3.80890316081983,139.731048497991,14.2261672294806));
#81220=CARTESIAN_POINT('Ctrl Pts',(3.80290028417302,139.794450651987,14.169553632052));
#81221=CARTESIAN_POINT('Ctrl Pts',(3.80196116231918,139.804313168165,14.1604392619546));
#81222=CARTESIAN_POINT('Ctrl Pts',(3.80048448420287,139.819761473143,14.1456650312962));
#81223=CARTESIAN_POINT('Ctrl Pts',(3.79993953222665,139.825449259723,14.1401141273428));
#81224=CARTESIAN_POINT('Ctrl Pts',(3.79886253248985,139.836671893302,14.1289375572586));
#81225=CARTESIAN_POINT('Ctrl Pts',(3.79833046011748,139.842207243204,14.1233130017159));
#81226=CARTESIAN_POINT('Ctrl Pts',(3.79692220936045,139.856818795379,14.108164389781));
#81227=CARTESIAN_POINT('Ctrl Pts',(3.79605333733977,139.865792948763,14.098542882218));
#81228=CARTESIAN_POINT('Ctrl Pts',(3.79211768698261,139.90613538509,14.0538104998538));
#81229=CARTESIAN_POINT('Ctrl Pts',(3.78916301506082,139.935545025994,14.0169853870527));
#81230=CARTESIAN_POINT('Ctrl Pts',(3.78036759505297,140.017124249449,13.9012377717556));
#81231=CARTESIAN_POINT('Ctrl Pts',(3.77462167143407,140.062072970699,13.8177145472912));
#81232=CARTESIAN_POINT('Ctrl Pts',(3.76721354109111,140.103851055827,13.7111053363814));
#81233=CARTESIAN_POINT('Ctrl Pts',(3.76590638509228,140.110669994167,13.6923096208639));
#81234=CARTESIAN_POINT('Ctrl Pts',(3.76377952641901,140.120858627309,13.6618267917514));
#81235=CARTESIAN_POINT('Ctrl Pts',(3.76296986172559,140.124531594255,13.65024472087));
#81236=CARTESIAN_POINT('Ctrl Pts',(3.76125396351118,140.131880709298,13.6257622031382));
#81237=CARTESIAN_POINT('Ctrl Pts',(3.7603465663144,140.135516947882,13.6128517033324));
#81238=CARTESIAN_POINT('Ctrl Pts',(3.7581015738672,140.143899111256,13.5810168466342));
#81239=CARTESIAN_POINT('Ctrl Pts',(3.75675625709921,140.148396650425,13.5620318659954));
#81240=CARTESIAN_POINT('Ctrl Pts',(3.75044123120765,140.167082814234,13.4733931797274));
#81241=CARTESIAN_POINT('Ctrl Pts',(3.74529334605313,140.175416456501,13.4026677939246));
#81242=CARTESIAN_POINT('Ctrl Pts',(3.73487808904619,140.179230029919,13.2607371967239));
#81243=CARTESIAN_POINT('Ctrl Pts',(3.72963381280529,140.174727340141,13.1898087607957));
#81244=CARTESIAN_POINT('Ctrl Pts',(3.72367069765558,140.161804126306,13.1063812395129));
#81245=CARTESIAN_POINT('Ctrl Pts',(3.72272703590348,140.159510037494,13.0930856111926));
#81246=CARTESIAN_POINT('Ctrl Pts',(3.72124496447285,140.155499837138,13.0720119503117));
#81247=CARTESIAN_POINT('Ctrl Pts',(3.72069907154485,140.153932499023,13.0642072488425));
#81248=CARTESIAN_POINT('Ctrl Pts',(3.71962192658602,140.150656598908,13.0487102669889));
#81249=CARTESIAN_POINT('Ctrl Pts',(3.71909062639947,140.148949741658,13.0410180744253));
#81250=CARTESIAN_POINT('Ctrl Pts',(3.71768703672218,140.144200701203,13.0205875454658));
#81251=CARTESIAN_POINT('Ctrl Pts',(3.71682196743311,140.1410229364,13.0078814309226));
#81252=CARTESIAN_POINT('Ctrl Pts',(3.71210761707385,140.122354549357,12.9381967205246));
#81253=CARTESIAN_POINT('Ctrl Pts',(3.70844041445968,140.1028061407,12.8823858134711));
#81254=CARTESIAN_POINT('Ctrl Pts',(3.6998004201543,140.046857668103,12.7543951504766));
#81255=CARTESIAN_POINT('Ctrl Pts',(3.69485131314189,140.007067153053,12.6840374098686));
#81256=CARTESIAN_POINT('Ctrl Pts',(3.68829417997797,139.948278366409,12.6012138331182));
#81257=CARTESIAN_POINT('Ctrl Pts',(3.6869268460941,139.935699084951,12.5844574767372));
#81258=CARTESIAN_POINT('Ctrl Pts',(3.68463879650462,139.914184062106,12.5573362449958));
#81259=CARTESIAN_POINT('Ctrl Pts',(3.68372814649029,139.905502373739,12.5467753475822));
#81260=CARTESIAN_POINT('Ctrl Pts',(3.68190367393702,139.887889679922,12.5260949190062));
#81261=CARTESIAN_POINT('Ctrl Pts',(3.68099018158458,139.878964649269,12.515973038045));
#81262=CARTESIAN_POINT('Ctrl Pts',(3.67870619779968,139.856400404893,12.4912525225724));
#81263=CARTESIAN_POINT('Ctrl Pts',(3.67732735551821,139.842560370669,12.4768438346986));
#81264=CARTESIAN_POINT('Ctrl Pts',(3.67094858481372,139.777587840458,12.4125576460861));
#81265=CARTESIAN_POINT('Ctrl Pts',(3.66577010803782,139.722357453954,12.3670511700812));
#81266=CARTESIAN_POINT('Ctrl Pts',(3.65544480934813,139.606085562461,12.2877949039917));
#81267=CARTESIAN_POINT('Ctrl Pts',(3.65032375135953,139.545477530907,12.2538859999674));
#81268=CARTESIAN_POINT('Ctrl Pts',(3.64446311470459,139.46980635545,12.2199247031927));
#81269=CARTESIAN_POINT('Ctrl Pts',(3.64350986180661,139.457280816154,12.214562321617));
#81270=CARTESIAN_POINT('Ctrl Pts',(3.64201640107588,139.437268164405,12.2064025359347));
#81271=CARTESIAN_POINT('Ctrl Pts',(3.64146852387238,139.429841171078,12.2034620671792));
#81272=CARTESIAN_POINT('Ctrl Pts',(3.64039101527643,139.415053050234,12.1977805513095));
#81273=CARTESIAN_POINT('Ctrl Pts',(3.63986128658951,139.407693323009,12.1950371456818));
#81274=CARTESIAN_POINT('Ctrl Pts',(3.6384672320587,139.388105049335,12.1879578005358));
#81275=CARTESIAN_POINT('Ctrl Pts',(3.63760995092967,139.375830959692,12.1837498009107));
#81276=CARTESIAN_POINT('Ctrl Pts',(3.63289601013944,139.307243035411,12.1614950666583));
#81277=CARTESIAN_POINT('Ctrl Pts',(3.62922284791983,139.249695234406,12.1475045697928));
#81278=CARTESIAN_POINT('Ctrl Pts',(3.62056617207898,139.111604178754,12.1247686468326));
#81279=CARTESIAN_POINT('Ctrl Pts',(3.61560673885947,139.030743099405,12.1198823701455));
#81280=CARTESIAN_POINT('Ctrl Pts',(3.60903900459623,138.929107147146,12.1241992199487));
#81281=CARTESIAN_POINT('Ctrl Pts',(3.60767271457875,138.908221097989,12.1256449356169));
#81282=CARTESIAN_POINT('Ctrl Pts',(3.60538591974876,138.873780571632,12.1289532355704));
#81283=CARTESIAN_POINT('Ctrl Pts',(3.60447545679667,138.860199782263,12.1304967972824));
#81284=CARTESIAN_POINT('Ctrl Pts',(3.6026509829604,138.833267393687,12.1340336767718));
#81285=CARTESIAN_POINT('Ctrl Pts',(3.60173729611322,138.819917097004,12.1360208977051));
#81286=CARTESIAN_POINT('Ctrl Pts',(3.59945207975801,138.786884142316,12.1415198069981));
#81287=CARTESIAN_POINT('Ctrl Pts',(3.59807217932877,138.767251825228,12.1453039671509));
#81288=CARTESIAN_POINT('Ctrl Pts',(3.59170956579801,138.678201420607,12.1648317784664));
#81289=CARTESIAN_POINT('Ctrl Pts',(3.58654976558408,138.610212418041,12.1863465906194));
#81290=CARTESIAN_POINT('Ctrl Pts',(3.57622490560696,138.480442781481,12.2407579136326));
#81291=CARTESIAN_POINT('Ctrl Pts',(3.57108479195691,138.418799135787,12.2732865867026));
#81292=CARTESIAN_POINT('Ctrl Pts',(3.56520802955033,138.348959074238,12.318457388931));
#81293=CARTESIAN_POINT('Ctrl Pts',(3.56425603221813,138.337662720374,12.3260443786691));
#81294=CARTESIAN_POINT('Ctrl Pts',(3.56276406206246,138.31995022417,12.3383913965552));
#81295=CARTESIAN_POINT('Ctrl Pts',(3.56221644432537,138.313447001667,12.3430236190217));
#81296=CARTESIAN_POINT('Ctrl Pts',(3.56113898754398,138.300638180529,12.3523450822805));
#81297=CARTESIAN_POINT('Ctrl Pts',(3.56060905759279,138.294331441897,12.357031977602));
#81298=CARTESIAN_POINT('Ctrl Pts',(3.5592137781077,138.277724190548,12.3696337038068));
#81299=CARTESIAN_POINT('Ctrl Pts',(3.55835549577434,138.267506567273,12.3776566823256));
#81300=CARTESIAN_POINT('Ctrl Pts',(3.5564354978976,138.244709044667,12.3961753753526));
#81301=CARTESIAN_POINT('Ctrl Pts',(3.5553793500769,138.232211034531,12.406767926361));
#81302=CARTESIAN_POINT('Ctrl Pts',(3.5518658918916,138.190965416043,12.4432307864417));
#81303=CARTESIAN_POINT('Ctrl Pts',(3.54945897851472,138.163270519238,12.4702563109205));
#81304=CARTESIAN_POINT('Ctrl Pts',(3.54173447847104,138.078385651491,12.5616704197462));
#81305=CARTESIAN_POINT('Ctrl Pts',(3.53646858814523,138.026913350294,12.6309675312097));
#81306=CARTESIAN_POINT('Ctrl Pts',(3.52958953609531,137.973176913908,12.7228142105224));
#81307=CARTESIAN_POINT('Ctrl Pts',(3.52826004731341,137.963359056369,12.7406391510084));
#81308=CARTESIAN_POINT('Ctrl Pts',(3.52601738952816,137.947775802657,12.7707522381477));
#81309=CARTESIAN_POINT('Ctrl Pts',(3.52511343399577,137.941752039337,12.782902153663));
#81310=CARTESIAN_POINT('Ctrl Pts',(3.52328824497287,137.93011090896,12.8074380320375));
#81311=CARTESIAN_POINT('Ctrl Pts',(3.52236711111442,137.924495626892,12.819822662089));
#81312=CARTESIAN_POINT('Ctrl Pts',(3.52003511523346,137.910934975582,12.8511628372026));
#81313=CARTESIAN_POINT('Ctrl Pts',(3.51861511185837,137.90326930228,12.8702336560898));
#81314=CARTESIAN_POINT('Ctrl Pts',(3.51546510033011,137.88755743913,12.9124845090497));
#81315=CARTESIAN_POINT('Ctrl Pts',(3.51372902428973,137.879728870532,12.9357347661782));
#81316=CARTESIAN_POINT('Ctrl Pts',(3.50803170725098,137.856689738697,13.0119507942234));
#81317=CARTESIAN_POINT('Ctrl Pts',(3.50399726602573,137.844468960527,13.0657399807676));
#81318=CARTESIAN_POINT('Ctrl Pts',(3.49552094071799,137.826850658652,13.179781295226));
#81319=CARTESIAN_POINT('Ctrl Pts',(3.49108936154799,137.82223409131,13.2399948902523));
#81320=CARTESIAN_POINT('Ctrl Pts',(3.48683023682335,137.822250041178,13.300311439502));
#81321=CARTESIAN_POINT('Ctrl Pts',(3.48683023682336,137.822250041178,13.3003114395019));
#81322=CARTESIAN_POINT('Ctrl Pts',(3.48596619464028,137.822253276903,13.3125477665077));
#81323=CARTESIAN_POINT('Ctrl Pts',(3.48511045956081,137.822446998391,13.3247739288273));
#81324=CARTESIAN_POINT('Ctrl Pts',(3.48378069926075,137.823050592295,13.3439746885546));
#81325=CARTESIAN_POINT('Ctrl Pts',(3.48330109326705,137.8233315726,13.3509421207309));
#81326=CARTESIAN_POINT('Ctrl Pts',(3.48232487836774,137.824034391365,13.3652192482236));
#81327=CARTESIAN_POINT('Ctrl Pts',(3.48182878743761,137.824462509499,13.3725277516578));
#81328=CARTESIAN_POINT('Ctrl Pts',(3.48062054569804,137.825680116448,13.3904495324128));
#81329=CARTESIAN_POINT('Ctrl Pts',(3.47991244642756,137.826545343786,13.4010568989226));
#81330=CARTESIAN_POINT('Ctrl Pts',(3.4773123081919,137.830284806035,13.4403247518565));
#81331=CARTESIAN_POINT('Ctrl Pts',(3.47546267205911,137.834066512121,13.4688906677266));
#81332=CARTESIAN_POINT('Ctrl Pts',(3.47172975987481,137.84395172549,13.5270675258845));
#81333=CARTESIAN_POINT('Ctrl Pts',(3.46985054954414,137.850154913566,13.5566392528942));
#81334=CARTESIAN_POINT('Ctrl Pts',(3.46677831503639,137.862197397912,13.6047564622898));
#81335=CARTESIAN_POINT('Ctrl Pts',(3.46558093876604,137.8673705408,13.6234528984423));
#81336=CARTESIAN_POINT('Ctrl Pts',(3.46350161923839,137.877140051955,13.6556452581504));
#81337=CARTESIAN_POINT('Ctrl Pts',(3.46262081792885,137.881522651725,13.6691966452519));
#81338=CARTESIAN_POINT('Ctrl Pts',(3.46173780698925,137.886148221013,13.6826607857451));
#81339=CARTESIAN_POINT('Ctrl Pts',(3.36195598355709,137.886148212184,13.682660760046));
#81340=CARTESIAN_POINT('Ctrl Pts',(3.36241237182347,137.883837075084,13.6759334849782));
#81341=CARTESIAN_POINT('Ctrl Pts',(3.36287041208775,137.881586846862,13.6691851655125));
#81342=CARTESIAN_POINT('Ctrl Pts',(3.3646512225657,137.873108986812,13.6429713885228));
#81343=CARTESIAN_POINT('Ctrl Pts',(3.36598643499762,137.867327686068,13.6233667838123));
#81344=CARTESIAN_POINT('Ctrl Pts',(3.36824003654619,137.858543767653,13.5904457321609));
#81345=CARTESIAN_POINT('Ctrl Pts',(3.36914914820719,137.855257213339,13.5772092705302));
#81346=CARTESIAN_POINT('Ctrl Pts',(3.37098619450111,137.849132410593,13.5505721754297));
#81347=CARTESIAN_POINT('Ctrl Pts',(3.37191404927104,137.8462966229,13.5371731720421));
#81348=CARTESIAN_POINT('Ctrl Pts',(3.37426695052869,137.839752734046,13.5033520960691));
#81349=CARTESIAN_POINT('Ctrl Pts',(3.37570135621474,137.836349759909,13.4828765067076));
#81350=CARTESIAN_POINT('Ctrl Pts',(3.3829584133633,137.822041920829,13.3800551942519));
#81351=CARTESIAN_POINT('Ctrl Pts',(3.38902897133321,137.819330863159,13.2968199616939));
#81352=CARTESIAN_POINT('Ctrl Pts',(3.39807601646271,137.828323987451,13.1739792352492));
#81353=CARTESIAN_POINT('Ctrl Pts',(3.40102047205989,137.833298792102,13.1341250377483));
#81354=CARTESIAN_POINT('Ctrl Pts',(3.40511781261743,137.843220397392,13.0781067613406));
#81355=CARTESIAN_POINT('Ctrl Pts',(3.40631434047634,137.846493477373,13.0616758138232));
#81356=CARTESIAN_POINT('Ctrl Pts',(3.4084299222341,137.852975258874,13.0324105356111));
#81357=CARTESIAN_POINT('Ctrl Pts',(3.40935416190632,137.856051713428,13.0195499459066));
#81358=CARTESIAN_POINT('Ctrl Pts',(3.4108152745144,137.861320269585,12.9990572938999));
#81359=CARTESIAN_POINT('Ctrl Pts',(3.41135923425297,137.863373999396,12.9913912091947));
#81360=CARTESIAN_POINT('Ctrl Pts',(3.4124430282484,137.867655756815,12.9760312951153));
#81361=CARTESIAN_POINT('Ctrl Pts',(3.41298276217872,137.869885085676,12.9683382796906));
#81362=CARTESIAN_POINT('Ctrl Pts',(3.41442621482104,137.876104644351,12.9476668731876));
#81363=CARTESIAN_POINT('Ctrl Pts',(3.41532203935336,137.880241225149,12.934733346848));
#81364=CARTESIAN_POINT('Ctrl Pts',(3.42079692728527,137.907177593431,12.8552763113865));
#81365=CARTESIAN_POINT('Ctrl Pts',(3.42511868834227,137.935676453949,12.7908263511326));
#81366=CARTESIAN_POINT('Ctrl Pts',(3.43380871729351,138.003818548769,12.667815068597));
#81367=CARTESIAN_POINT('Ctrl Pts',(3.43816263513904,138.043308840823,12.6095104157656));
#81368=CARTESIAN_POINT('Ctrl Pts',(3.44401017102428,138.100487858893,12.5394883225751));
#81369=CARTESIAN_POINT('Ctrl Pts',(3.44532582852851,138.113614072183,12.5242294072873));
#81370=CARTESIAN_POINT('Ctrl Pts',(3.44755608421039,138.136242641866,12.4992486236562));
#81371=CARTESIAN_POINT('Ctrl Pts',(3.44846183822241,138.145534236986,12.4893411481007));
#81372=CARTESIAN_POINT('Ctrl Pts',(3.45029993731405,138.164577671986,12.4697266410326));
#81373=CARTESIAN_POINT('Ctrl Pts',(3.45123232997283,138.174332402686,12.4600254125638));
#81374=CARTESIAN_POINT('Ctrl Pts',(3.45361342668149,138.199467048716,12.4358895471716));
#81375=CARTESIAN_POINT('Ctrl Pts',(3.45507196727483,138.215068356333,12.4216936207663));
#81376=CARTESIAN_POINT('Ctrl Pts',(3.46309465989909,138.301931639212,12.3468184662482));
#81377=CARTESIAN_POINT('Ctrl Pts',(3.4699820893236,138.379842980158,12.294388804727));
#81378=CARTESIAN_POINT('Ctrl Pts',(3.48036913911613,138.505937879985,12.2298073432981));
#81379=CARTESIAN_POINT('Ctrl Pts',(3.48387180715933,138.550067040572,12.2105180379852));
#81380=CARTESIAN_POINT('Ctrl Pts',(3.48809896371012,138.606513260801,12.1898617500924));
#81381=CARTESIAN_POINT('Ctrl Pts',(3.48893427713972,138.617832876857,12.1859142464915));
#81382=CARTESIAN_POINT('Ctrl Pts',(3.49028523651756,138.636443087598,12.1797413306903));
#81383=CARTESIAN_POINT('Ctrl Pts',(3.4908064053045,138.643698310538,12.1774127054966));
#81384=CARTESIAN_POINT('Ctrl Pts',(3.49188745750944,138.65891671153,12.1726906470384));
#81385=CARTESIAN_POINT('Ctrl Pts',(3.49244659286099,138.666883520382,12.1703108354951));
#81386=CARTESIAN_POINT('Ctrl Pts',(3.49400742384673,138.689369390241,12.1638525184366));
#81387=CARTESIAN_POINT('Ctrl Pts',(3.49499888336913,138.703943070141,12.159968061096));
#81388=CARTESIAN_POINT('Ctrl Pts',(3.4972815514475,138.738055901977,12.1515739931941));
#81389=CARTESIAN_POINT('Ctrl Pts',(3.49856357481888,138.757643883482,12.1472812119887));
#81390=CARTESIAN_POINT('Ctrl Pts',(3.50341875097642,138.832996659859,12.1327732635331));
#81391=CARTESIAN_POINT('Ctrl Pts',(3.50689443931797,138.889364323222,12.1260882507653));
#81392=CARTESIAN_POINT('Ctrl Pts',(3.51403761257599,139.004676866257,12.1207952662246));
#81393=CARTESIAN_POINT('Ctrl Pts',(3.51769866205715,139.063470571353,12.1224957895716));
#81394=CARTESIAN_POINT('Ctrl Pts',(3.52286147547534,139.143063494294,12.130777553757));
#81395=CARTESIAN_POINT('Ctrl Pts',(3.52425019959525,139.164173581776,12.1335544435307));
#81396=CARTESIAN_POINT('Ctrl Pts',(3.52656800458119,139.19881782905,12.1390707183034));
#81397=CARTESIAN_POINT('Ctrl Pts',(3.52748658991739,139.212400174396,12.1414787594018));
#81398=CARTESIAN_POINT('Ctrl Pts',(3.52932282082344,139.239236747527,12.1467244504931));
#81399=CARTESIAN_POINT('Ctrl Pts',(3.5302400612073,139.252490500797,12.1495534628818));
#81400=CARTESIAN_POINT('Ctrl Pts',(3.53252607210383,139.285130803349,12.1571117223191));
#81401=CARTESIAN_POINT('Ctrl Pts',(3.53390309486758,139.304450947544,12.1621060128241));
#81402=CARTESIAN_POINT('Ctrl Pts',(3.54019137834316,139.391098824605,12.1868692633379));
#81403=CARTESIAN_POINT('Ctrl Pts',(3.54527426339156,139.456695396699,12.2121375057453));
#81404=CARTESIAN_POINT('Ctrl Pts',(3.55562246577164,139.583290210715,12.274379399949));
#81405=CARTESIAN_POINT('Ctrl Pts',(3.56086681788583,139.643983682482,12.3113587598672));
#81406=CARTESIAN_POINT('Ctrl Pts',(3.56683243050722,139.711850679058,12.3616255883316));
#81407=CARTESIAN_POINT('Ctrl Pts',(3.56777836572911,139.722578492947,12.3698611466092));
#81408=CARTESIAN_POINT('Ctrl Pts',(3.56926525265173,139.739421798109,12.3832587978587));
#81409=CARTESIAN_POINT('Ctrl Pts',(3.5698137054281,139.745630317725,12.3883013293743));
#81410=CARTESIAN_POINT('Ctrl Pts',(3.57089791418575,139.757904212338,12.3984793872533));
#81411=CARTESIAN_POINT('Ctrl Pts',(3.57143369004956,139.763969925577,12.4036138266559));
#81412=CARTESIAN_POINT('Ctrl Pts',(3.57285338884438,139.780027452261,12.417487435491));
#81413=CARTESIAN_POINT('Ctrl Pts',(3.57372986304751,139.789924595509,12.4263350625362));
#81414=CARTESIAN_POINT('Ctrl Pts',(3.578456686363,139.843053967571,12.4754716197305));
#81415=CARTESIAN_POINT('Ctrl Pts',(3.58212575599146,139.883361452405,12.5188078193927));
#81416=CARTESIAN_POINT('Ctrl Pts',(3.59073898875675,139.970271904251,12.6276218639937));
#81417=CARTESIAN_POINT('Ctrl Pts',(3.59566049872391,140.013766105479,12.6951886647184));
#81418=CARTESIAN_POINT('Ctrl Pts',(3.6021924666431,140.059591321606,12.7854087275828));
#81419=CARTESIAN_POINT('Ctrl Pts',(3.60356585260536,140.068616515949,12.804422962466));
#81420=CARTESIAN_POINT('Ctrl Pts',(3.60586521440667,140.082687572064,12.8362417593078));
#81421=CARTESIAN_POINT('Ctrl Pts',(3.6067810488211,140.088027252898,12.8489115890893));
#81422=CARTESIAN_POINT('Ctrl Pts',(3.60861723779828,140.098201413881,12.874284845953));
#81423=CARTESIAN_POINT('Ctrl Pts',(3.60953727726179,140.103040208997,12.8869842518208));
#81424=CARTESIAN_POINT('Ctrl Pts',(3.61184108729313,140.114511259055,12.9187305300396));
#81425=CARTESIAN_POINT('Ctrl Pts',(3.6132334013076,140.120875835878,12.9378687691318));
#81426=CARTESIAN_POINT('Ctrl Pts',(3.61924604796346,140.145946437036,13.0202634392441));
#81427=CARTESIAN_POINT('Ctrl Pts',(3.62401479966679,140.159809358087,13.084859005461));
#81428=CARTESIAN_POINT('Ctrl Pts',(3.63439034052384,140.177808784029,13.2252865173418));
#81429=CARTESIAN_POINT('Ctrl Pts',(3.63999523230505,140.180176251222,13.3010633326068));
#81430=CARTESIAN_POINT('Ctrl Pts',(3.64624858796237,140.174414308321,13.3895282399384));
#81431=CARTESIAN_POINT('Ctrl Pts',(3.64715742750856,140.173353807826,13.4024946358839));
#81432=CARTESIAN_POINT('Ctrl Pts',(3.64860026944275,140.171305031423,13.4232958898383));
#81433=CARTESIAN_POINT('Ctrl Pts',(3.64914106889275,140.170452458468,13.4311426955614));
#81434=CARTESIAN_POINT('Ctrl Pts',(3.65022485608359,140.168570225911,13.4469816631424));
#81435=CARTESIAN_POINT('Ctrl Pts',(3.65076765180375,140.167537309942,13.4549729708839));
#81436=CARTESIAN_POINT('Ctrl Pts',(3.65222948327559,140.16451138398,13.476632593384));
#81437=CARTESIAN_POINT('Ctrl Pts',(3.65314027461669,140.162359753237,13.4902779057982));
#81438=CARTESIAN_POINT('Ctrl Pts',(3.65849884545204,140.148134453274,13.5712111136521));
#81439=CARTESIAN_POINT('Ctrl Pts',(3.66270592696095,140.13045951786,13.6373895818358));
#81440=CARTESIAN_POINT('Ctrl Pts',(3.67119864960379,140.083586309109,13.7665891470757));
#81441=CARTESIAN_POINT('Ctrl Pts',(3.67547120883528,140.054370517278,13.8293073323675));
#81442=CARTESIAN_POINT('Ctrl Pts',(3.68130814915284,140.00910199199,13.9076744869996));
#81443=CARTESIAN_POINT('Ctrl Pts',(3.68270688660635,139.997868707795,13.9259497275824));
#81444=CARTESIAN_POINT('Ctrl Pts',(3.68503674684559,139.978585767844,13.9554815316255));
#81445=CARTESIAN_POINT('Ctrl Pts',(3.68595714072617,139.970825358354,13.9669214642655));
#81446=CARTESIAN_POINT('Ctrl Pts',(3.68779350536935,139.955075094265,13.9892819802223));
#81447=CARTESIAN_POINT('Ctrl Pts',(3.68870901336687,139.947094824133,14.0002067205409));
#81448=CARTESIAN_POINT('Ctrl Pts',(3.6909839352324,139.92696338637,14.0267921120005));
#81449=CARTESIAN_POINT('Ctrl Pts',(3.6923514210906,139.91460207103,14.0422875873205));
#81450=CARTESIAN_POINT('Ctrl Pts',(3.69856311300457,139.857331980322,14.1104749330372));
#81451=CARTESIAN_POINT('Ctrl Pts',(3.70357422042904,139.808227123204,14.1594497745731));
#81452=CARTESIAN_POINT('Ctrl Pts',(3.71396196866625,139.69952420593,14.250267498483));
#81453=CARTESIAN_POINT('Ctrl Pts',(3.71932219536306,139.639763858105,14.2914867961921));
#81454=CARTESIAN_POINT('Ctrl Pts',(3.72538139581134,139.564935664206,14.333499606884));
#81455=CARTESIAN_POINT('Ctrl Pts',(3.72631611186194,139.553168827342,14.3398451945717));
#81456=CARTESIAN_POINT('Ctrl Pts',(3.72778966891356,139.534221328444,14.3496504597366));
#81457=CARTESIAN_POINT('Ctrl Pts',(3.72833579527716,139.527109531827,14.3532397953035));
#81458=CARTESIAN_POINT('Ctrl Pts',(3.72941973324274,139.512803151647,14.3602790385105));
#81459=CARTESIAN_POINT('Ctrl Pts',(3.72995750469923,139.505608834922,14.3637285496196));
#81460=CARTESIAN_POINT('Ctrl Pts',(3.73138919203561,139.486214288058,14.3727865628801));
#81461=CARTESIAN_POINT('Ctrl Pts',(3.73227543482366,139.473951904242,14.378260160526));
#81462=CARTESIAN_POINT('Ctrl Pts',(3.73683763652325,139.40966221112,14.4056485847371));
#81463=CARTESIAN_POINT('Ctrl Pts',(3.74034992680729,139.356196658669,14.4240139296472));
#81464=CARTESIAN_POINT('Ctrl Pts',(3.74898877104284,139.221252018408,14.4597646392731));
#81465=CARTESIAN_POINT('Ctrl Pts',(3.75408385317169,139.13886923152,14.4724846800504));
#81466=CARTESIAN_POINT('Ctrl Pts',(3.76079320739871,139.035115397669,14.4774091526065));
#81467=CARTESIAN_POINT('Ctrl Pts',(3.76214774979994,139.014372791898,14.4778449566465));
#81468=CARTESIAN_POINT('Ctrl Pts',(3.76442449573541,138.979937075474,14.477658717995));
#81469=CARTESIAN_POINT('Ctrl Pts',(3.76533698738087,138.966246528022,14.4773458512391));
#81470=CARTESIAN_POINT('Ctrl Pts',(3.76717341750225,138.938936596162,14.4762450250355));
#81471=CARTESIAN_POINT('Ctrl Pts',(3.76809715491837,138.925319267852,14.4754589993785));
#81472=CARTESIAN_POINT('Ctrl Pts',(3.77042428982301,138.89133070851,14.4729041242417));
#81473=CARTESIAN_POINT('Ctrl Pts',(3.77183661596766,138.870986829986,14.4708409842814));
#81474=CARTESIAN_POINT('Ctrl Pts',(3.77496332499627,138.826589667418,14.4651674184899));
#81475=CARTESIAN_POINT('Ctrl Pts',(3.77668356875944,138.802574083427,14.4613393666294));
#81476=CARTESIAN_POINT('Ctrl Pts',(3.78230049541797,138.725440305582,14.4465827306297));
#81477=CARTESIAN_POINT('Ctrl Pts',(3.78626816478442,138.672956510601,14.4327297149224));
#81478=CARTESIAN_POINT('Ctrl Pts',(3.79468713727952,138.564413637379,14.3959053673396));
#81479=CARTESIAN_POINT('Ctrl Pts',(3.79913018828996,138.508782442564,14.3721243087026));
#81480=CARTESIAN_POINT('Ctrl Pts',(3.80440142765512,138.44271891374,14.3376567850524));
#81481=CARTESIAN_POINT('Ctrl Pts',(3.80538886508177,138.430337307749,14.3309113801462));
#81482=CARTESIAN_POINT('Ctrl Pts',(3.80692498298134,138.411023250858,14.3199349571874));
#81483=CARTESIAN_POINT('Ctrl Pts',(3.80748198290369,138.404008723537,14.3158520247486));
#81484=CARTESIAN_POINT('Ctrl Pts',(3.80856808693406,138.390298207881,14.3076806654435));
#81485=CARTESIAN_POINT('Ctrl Pts',(3.80909742091858,138.383599843808,14.3035972560907));
#81486=CARTESIAN_POINT('Ctrl Pts',(3.81047768361035,138.366107611113,14.2926925621302));
#81487=CARTESIAN_POINT('Ctrl Pts',(3.81132189109702,138.355382621629,14.2857619145525));
#81488=CARTESIAN_POINT('Ctrl Pts',(3.81608774883458,138.294848230974,14.245233111747));
#81489=CARTESIAN_POINT('Ctrl Pts',(3.81981808406148,138.247549018368,14.2080329938247));
#81490=CARTESIAN_POINT('Ctrl Pts',(3.8284904768729,138.144281287434,14.1131792843514));
#81491=CARTESIAN_POINT('Ctrl Pts',(3.83341021764234,138.090962193914,14.0531028302434));
#81492=CARTESIAN_POINT('Ctrl Pts',(3.83994036460814,138.031859088223,13.9710001760125));
#81493=CARTESIAN_POINT('Ctrl Pts',(3.84131392176737,138.020023168778,13.9535926738573));
#81494=CARTESIAN_POINT('Ctrl Pts',(3.84361348930118,138.001237309109,13.9243053624643));
#81495=CARTESIAN_POINT('Ctrl Pts',(3.84452935432236,137.994017579342,13.9126038202928));
#81496=CARTESIAN_POINT('Ctrl Pts',(3.84636554275031,137.980072700224,13.8890908497109));
#81497=CARTESIAN_POINT('Ctrl Pts',(3.84728555003971,137.97334387554,13.8772840732483));
#81498=CARTESIAN_POINT('Ctrl Pts',(3.84958915601224,137.957141519708,13.8476749462109));
#81499=CARTESIAN_POINT('Ctrl Pts',(3.8509812947885,137.94791839133,13.8297413122385));
#81500=CARTESIAN_POINT('Ctrl Pts',(3.8556364864431,137.918954180526,13.7696796720604));
#81501=CARTESIAN_POINT('Ctrl Pts',(3.85896366269804,137.901253914743,13.7266305527279));
#81502=CARTESIAN_POINT('Ctrl Pts',(3.86234166104071,137.886148208794,13.6826607501787));
#81503=CARTESIAN_POINT('Origin',(1.13913288526384,139.,13.3));
#81504=CARTESIAN_POINT('',(4.46223878927246,137.886148213663,13.6826607643511));
#81505=CARTESIAN_POINT('',(4.36393196101569,137.88614821266,13.6826607614313));
#81506=CARTESIAN_POINT('',(1.13913288526384,137.88614821265,13.6826607614027));
#81507=CARTESIAN_POINT('Ctrl Pts',(4.46223878927246,137.886148214676,13.6826607672995));
#81508=CARTESIAN_POINT('Ctrl Pts',(4.45883984757335,137.901538260174,13.7274582253084));
#81509=CARTESIAN_POINT('Ctrl Pts',(4.45537582733297,137.919617125364,13.7712873632294));
#81510=CARTESIAN_POINT('Ctrl Pts',(4.44726731267853,137.967797810042,13.8706389399772));
#81511=CARTESIAN_POINT('Ctrl Pts',(4.442622440193,137.999821846321,13.9250720199846));
#81512=CARTESIAN_POINT('Ctrl Pts',(4.43715156406992,138.044237488671,13.9883429697029));
#81513=CARTESIAN_POINT('Ctrl Pts',(4.43615335261791,138.052634187618,13.9998543310981));
#81514=CARTESIAN_POINT('Ctrl Pts',(4.43460660152402,138.066138494095,14.0176793164653));
#81515=CARTESIAN_POINT('Ctrl Pts',(4.43404949841628,138.071105742906,14.0240969427439));
#81516=CARTESIAN_POINT('Ctrl Pts',(4.43296938357515,138.080947272155,14.0365441229199));
#81517=CARTESIAN_POINT('Ctrl Pts',(4.43244605420597,138.085815451089,14.0425777921083));
#81518=CARTESIAN_POINT('Ctrl Pts',(4.4310916979544,138.098664698075,14.0581853851372));
#81519=CARTESIAN_POINT('Ctrl Pts',(4.43026699553161,138.106739069333,14.0676817996047));
#81520=CARTESIAN_POINT('Ctrl Pts',(4.42541626619723,138.155614040048,14.1233490357373));
#81521=CARTESIAN_POINT('Ctrl Pts',(4.42159405130105,138.19984090546,14.1663940138214));
#81522=CARTESIAN_POINT('Ctrl Pts',(4.41289925732351,138.307979880114,14.256264069738));
#81523=CARTESIAN_POINT('Ctrl Pts',(4.40804619480079,138.373638761826,14.3005013590557));
#81524=CARTESIAN_POINT('Ctrl Pts',(4.40158816018715,138.461814227166,14.3478053413701));
#81525=CARTESIAN_POINT('Ctrl Pts',(4.40021187739387,138.480664531222,14.3572750548741));
#81526=CARTESIAN_POINT('Ctrl Pts',(4.39791306533311,138.512158212797,14.3720508682451));
#81527=CARTESIAN_POINT('Ctrl Pts',(4.397000806824,138.524658479204,14.3776516530701));
#81528=CARTESIAN_POINT('Ctrl Pts',(4.39517630591881,138.549641960991,14.3883263304494));
#81529=CARTESIAN_POINT('Ctrl Pts',(4.39426444597717,138.56212021756,14.3934065276689));
#81530=CARTESIAN_POINT('Ctrl Pts',(4.39199083313674,138.593195146005,14.4054406324546));
#81531=CARTESIAN_POINT('Ctrl Pts',(4.39062089783546,138.61188511634,14.4121402495605));
#81532=CARTESIAN_POINT('Ctrl Pts',(4.38411576409656,138.700422223433,14.4413737525114));
#81533=CARTESIAN_POINT('Ctrl Pts',(4.37879027301252,138.77209714738,14.4578160350299));
#81534=CARTESIAN_POINT('Ctrl Pts',(4.36845327184661,138.911700192532,14.4763713952914));
#81535=CARTESIAN_POINT('Ctrl Pts',(4.3634732240909,138.979221341052,14.4794982430917));
#81536=CARTESIAN_POINT('Ctrl Pts',(4.35773579559411,139.060339039161,14.4762831904497));
#81537=CARTESIAN_POINT('Ctrl Pts',(4.35677651128038,139.074025502447,14.4755012588335));
#81538=CARTESIAN_POINT('Ctrl Pts',(4.35527589183683,139.095678275676,14.4738844932215));
#81539=CARTESIAN_POINT('Ctrl Pts',(4.35472676946382,139.103654653727,14.4732070823743));
#81540=CARTESIAN_POINT('Ctrl Pts',(4.35364899444119,139.119427482003,14.4717054188381));
#81541=CARTESIAN_POINT('Ctrl Pts',(4.35312021400177,139.127223777123,14.4708845500855));
#81542=CARTESIAN_POINT('Ctrl Pts',(4.35173194788079,139.147826140412,14.4685071227221));
#81543=CARTESIAN_POINT('Ctrl Pts',(4.3508794008774,139.160616256457,14.4668178588765));
#81544=CARTESIAN_POINT('Ctrl Pts',(4.34897470980326,139.189427692726,14.4625298076386));
#81545=CARTESIAN_POINT('Ctrl Pts',(4.34792800012487,139.205428428913,14.4598093021381));
#81546=CARTESIAN_POINT('Ctrl Pts',(4.34446323982024,139.258728114645,14.4496093571142));
#81547=CARTESIAN_POINT('Ctrl Pts',(4.34209412215202,139.295721751769,14.4406537229038));
#81548=CARTESIAN_POINT('Ctrl Pts',(4.33432497097638,139.416058457358,14.4052724124232));
#81549=CARTESIAN_POINT('Ctrl Pts',(4.32898282799453,139.496885753533,14.3713705178584));
#81550=CARTESIAN_POINT('Ctrl Pts',(4.32202694378543,139.590845735638,14.3190209005579));
#81551=CARTESIAN_POINT('Ctrl Pts',(4.32070800932295,139.608217705487,14.3087484440332));
#81552=CARTESIAN_POINT('Ctrl Pts',(4.31856728609634,139.635638199719,14.2915682042359));
#81553=CARTESIAN_POINT('Ctrl Pts',(4.31775579915853,139.645858684081,14.2849416053744));
#81554=CARTESIAN_POINT('Ctrl Pts',(4.31604025158083,139.66708876973,14.2707042419827));
#81555=CARTESIAN_POINT('Ctrl Pts',(4.31513508841991,139.67807503198,14.2630619800493));
#81556=CARTESIAN_POINT('Ctrl Pts',(4.31290459713402,139.704609389953,14.2439250336748));
#81557=CARTESIAN_POINT('Ctrl Pts',(4.31157177889594,139.720008745971,14.2322318327998));
#81558=CARTESIAN_POINT('Ctrl Pts',(4.30865214745907,139.752743788209,14.2060800796655));
#81559=CARTESIAN_POINT('Ctrl Pts',(4.30706072335657,139.769965467499,14.1914916637237));
#81560=CARTESIAN_POINT('Ctrl Pts',(4.30209177922903,139.821848796696,14.1449162480972));
#81561=CARTESIAN_POINT('Ctrl Pts',(4.29866046480935,139.85501434169,14.1113375841883));
#81562=CARTESIAN_POINT('Ctrl Pts',(4.2898472743371,139.934192371447,14.0209123679554));
#81563=CARTESIAN_POINT('Ctrl Pts',(4.28444103841335,139.977096104843,13.9616000841065));
#81564=CARTESIAN_POINT('Ctrl Pts',(4.27834744578894,140.020975857553,13.8872643767603));
#81565=CARTESIAN_POINT('Ctrl Pts',(4.27741968537076,140.027528112962,13.8757231663888));
#81566=CARTESIAN_POINT('Ctrl Pts',(4.27595651050231,140.03767482986,13.857125344645));
#81567=CARTESIAN_POINT('Ctrl Pts',(4.27541391759355,140.041395434055,13.8501393109333));
#81568=CARTESIAN_POINT('Ctrl Pts',(4.27433720048232,140.048699062977,13.836085915959));
#81569=CARTESIAN_POINT('Ctrl Pts',(4.2738031118734,140.052281762572,13.8290188421305));
#81570=CARTESIAN_POINT('Ctrl Pts',(4.27238275705343,140.061691326891,13.8099840660879));
#81571=CARTESIAN_POINT('Ctrl Pts',(4.27150402194782,140.067387270411,13.7979524808835));
#81572=CARTESIAN_POINT('Ctrl Pts',(4.26952918233838,140.079861508819,13.770404898972));
#81573=CARTESIAN_POINT('Ctrl Pts',(4.26843913697486,140.086511757881,13.7548339315658));
#81574=CARTESIAN_POINT('Ctrl Pts',(4.26474657679644,140.108115316652,13.7010703443708));
#81575=CARTESIAN_POINT('Ctrl Pts',(4.26220000385717,140.121409211381,13.6622413140163));
#81576=CARTESIAN_POINT('Ctrl Pts',(4.25462151029059,140.154985078119,13.5444277020347));
#81577=CARTESIAN_POINT('Ctrl Pts',(4.24962214760114,140.169123891407,13.4639612278263));
#81578=CARTESIAN_POINT('Ctrl Pts',(4.24301350762205,140.176309023071,13.3618673914798));
#81579=CARTESIAN_POINT('Ctrl Pts',(4.24165139255027,140.177220432482,13.3410177904647));
#81580=CARTESIAN_POINT('Ctrl Pts',(4.23936961470675,140.177811212067,13.3065025107405));
#81581=CARTESIAN_POINT('Ctrl Pts',(4.23845989866968,140.177807427122,13.2928465347871));
#81582=CARTESIAN_POINT('Ctrl Pts',(4.23663540983044,140.177327590376,13.2656887699477));
#81583=CARTESIAN_POINT('Ctrl Pts',(4.23572093635781,140.176856658747,13.2521889773352));
#81584=CARTESIAN_POINT('Ctrl Pts',(4.23343074134145,140.175110049721,13.218676651758));
#81585=CARTESIAN_POINT('Ctrl Pts',(4.23204656768424,140.173555291358,13.198683623914));
#81586=CARTESIAN_POINT('Ctrl Pts',(4.22899174975599,140.169049348557,13.1551514016407));
#81587=CARTESIAN_POINT('Ctrl Pts',(4.22731566280452,140.165895823589,13.1316423629123));
#81588=CARTESIAN_POINT('Ctrl Pts',(4.22192166952304,140.153602640877,13.0571453659457));
#81589=CARTESIAN_POINT('Ctrl Pts',(4.21813886193538,140.141809436159,13.0066609810062));
#81590=CARTESIAN_POINT('Ctrl Pts',(4.20962252947812,140.108043336665,12.8957023586665));
#81591=CARTESIAN_POINT('Ctrl Pts',(4.20489053403361,140.084360967074,12.8359103970641));
#81592=CARTESIAN_POINT('Ctrl Pts',(4.19935221576864,140.049684424948,12.7657192386257));
#81593=CARTESIAN_POINT('Ctrl Pts',(4.19836597707902,140.043221543054,12.7532073703155));
#81594=CARTESIAN_POINT('Ctrl Pts',(4.19683340086377,140.032698650515,12.7337016126807));
#81595=CARTESIAN_POINT('Ctrl Pts',(4.19627874147077,140.028788579058,12.7266288849215));
#81596=CARTESIAN_POINT('Ctrl Pts',(4.19519945239944,140.020973205864,12.7128294450961));
#81597=CARTESIAN_POINT('Ctrl Pts',(4.19467456224787,140.017073517697,12.7061001658846));
#81598=CARTESIAN_POINT('Ctrl Pts',(4.19331037065193,140.006686924027,12.6885795083732));
#81599=CARTESIAN_POINT('Ctrl Pts',(4.19247757065418,140.000092909207,12.6778522801052));
#81600=CARTESIAN_POINT('Ctrl Pts',(4.18763637439323,139.960354628201,12.6154705537781));
#81601=CARTESIAN_POINT('Ctrl Pts',(4.18382917001659,139.923381698074,12.5663586264395));
#81602=CARTESIAN_POINT('Ctrl Pts',(4.17514977927128,139.830466074514,12.4611568800536));
#81603=CARTESIAN_POINT('Ctrl Pts',(4.17029713669324,139.772372342863,12.4073795892837));
#81604=CARTESIAN_POINT('Ctrl Pts',(4.16383953751664,139.692499081472,12.3471175278124));
#81605=CARTESIAN_POINT('Ctrl Pts',(4.16246321877293,139.675323426076,12.3348688352704));
#81606=CARTESIAN_POINT('Ctrl Pts',(4.16016436345579,139.646467503178,12.3154379432019));
#81607=CARTESIAN_POINT('Ctrl Pts',(4.15925209846732,139.634973858544,12.3079864675178));
#81608=CARTESIAN_POINT('Ctrl Pts',(4.15742759730676,139.61192278093,12.2936068995195));
#81609=CARTESIAN_POINT('Ctrl Pts',(4.15651574379753,139.600371218434,12.2866733318614));
#81610=CARTESIAN_POINT('Ctrl Pts',(4.15424217192136,139.571509725801,12.2700166045455));
#81611=CARTESIAN_POINT('Ctrl Pts',(4.15287227181573,139.554068616706,12.2605304015603));
#81612=CARTESIAN_POINT('Ctrl Pts',(4.14649639509764,139.472710868938,12.2189093867736));
#81613=CARTESIAN_POINT('Ctrl Pts',(4.14131081953153,139.406198693131,12.1922039408861));
#81614=CARTESIAN_POINT('Ctrl Pts',(4.13096433975432,139.271110897189,12.1517738831739));
#81615=CARTESIAN_POINT('Ctrl Pts',(4.12582926277561,139.202898331166,12.137778860655));
#81616=CARTESIAN_POINT('Ctrl Pts',(4.11995675104902,139.120323250853,12.12833339702));
#81617=CARTESIAN_POINT('Ctrl Pts',(4.1190044122164,139.106774203128,12.1270210476052));
#81618=CARTESIAN_POINT('Ctrl Pts',(4.11751203662919,139.085244994571,12.1253119093653));
#81619=CARTESIAN_POINT('Ctrl Pts',(4.11696434831162,139.077278729014,12.1247609490538));
#81620=CARTESIAN_POINT('Ctrl Pts',(4.1158868775848,139.061464499495,12.1238287117657));
#81621=CARTESIAN_POINT('Ctrl Pts',(4.11535700252979,139.053617147161,12.1234448618862));
#81622=CARTESIAN_POINT('Ctrl Pts',(4.11396205697664,139.032790869798,12.1226349598366));
#81623=CARTESIAN_POINT('Ctrl Pts',(4.11310404754831,139.019807311156,12.1223449639349));
#81624=CARTESIAN_POINT('Ctrl Pts',(4.11118477871192,138.990448123899,12.1221749268985));
#81625=CARTESIAN_POINT('Ctrl Pts',(4.11012908063906,138.97407426414,12.1224215309074));
#81626=CARTESIAN_POINT('Ctrl Pts',(4.10661795418094,138.919095177664,12.1243969597955));
#81627=CARTESIAN_POINT('Ctrl Pts',(4.10421285225986,138.880569461679,12.1276839954234));
#81628=CARTESIAN_POINT('Ctrl Pts',(4.09648626112016,138.756913829389,12.1443947797012));
#81629=CARTESIAN_POINT('Ctrl Pts',(4.0912167546949,138.673086100112,12.1652576904566));
#81630=CARTESIAN_POINT('Ctrl Pts',(4.08433405569668,138.573203056165,12.2021142422659));
#81631=CARTESIAN_POINT('Ctrl Pts',(4.08300505710345,138.554307555417,12.2096482526637));
#81632=CARTESIAN_POINT('Ctrl Pts',(4.08085246850904,138.524399964962,12.2224803175672));
#81633=CARTESIAN_POINT('Ctrl Pts',(4.08003940761502,138.513258335464,12.2274672068139));
#81634=CARTESIAN_POINT('Ctrl Pts',(4.07832404442594,138.490090188883,12.238272402639));
#81635=CARTESIAN_POINT('Ctrl Pts',(4.07742069060003,138.47808119861,12.2441239439785));
#81636=CARTESIAN_POINT('Ctrl Pts',(4.07520204452629,138.449068280091,12.2588767616139));
#81637=CARTESIAN_POINT('Ctrl Pts',(4.07387945019642,138.432177912427,12.2679915897651));
#81638=CARTESIAN_POINT('Ctrl Pts',(4.06739663749784,138.351381900692,12.3141768591782));
#81639=CARTESIAN_POINT('Ctrl Pts',(4.0620409255153,138.290847261586,12.3567864633664));
#81640=CARTESIAN_POINT('Ctrl Pts',(4.05159333881989,138.182635933775,12.4492917819815));
#81641=CARTESIAN_POINT('Ctrl Pts',(4.04653348150186,138.13454146534,12.4982697631419));
#81642=CARTESIAN_POINT('Ctrl Pts',(4.0407255093698,138.082284346631,12.5617047430064));
#81643=CARTESIAN_POINT('Ctrl Pts',(4.0397689569501,138.073777007686,12.5724060776149));
#81644=CARTESIAN_POINT('Ctrl Pts',(4.03827157965962,138.060590830572,12.5895991105448));
#81645=CARTESIAN_POINT('Ctrl Pts',(4.03772302101481,138.055788767651,12.5959941977968));
#81646=CARTESIAN_POINT('Ctrl Pts',(4.03664537016418,138.046405152408,12.6087594598157));
#81647=CARTESIAN_POINT('Ctrl Pts',(4.03611616394323,138.041821411729,12.6151274439781));
#81648=CARTESIAN_POINT('Ctrl Pts',(4.03472529530285,138.029851273586,12.632112454111));
#81649=CARTESIAN_POINT('Ctrl Pts',(4.03387061919083,138.022575286856,12.642806505144));
#81650=CARTESIAN_POINT('Ctrl Pts',(4.0289660098986,137.981405004415,12.7055142484427));
#81651=CARTESIAN_POINT('Ctrl Pts',(4.0251195025581,137.951485670696,12.7600290313087));
#81652=CARTESIAN_POINT('Ctrl Pts',(4.01649748653914,137.894250419969,12.8872063188554));
#81653=CARTESIAN_POINT('Ctrl Pts',(4.01173855375662,137.869531004189,12.9607078250999));
#81654=CARTESIAN_POINT('Ctrl Pts',(4.00537865271191,137.847444882588,13.0567684620347));
#81655=CARTESIAN_POINT('Ctrl Pts',(4.00399506805886,137.843252005322,13.0775615444864));
#81656=CARTESIAN_POINT('Ctrl Pts',(4.00168746726154,137.837275326005,13.1119718177466));
#81657=CARTESIAN_POINT('Ctrl Pts',(4.00077389022519,137.835164120319,13.1255276198361));
#81658=CARTESIAN_POINT('Ctrl Pts',(3.9989493155907,137.831452273062,13.1524455747605));
#81659=CARTESIAN_POINT('Ctrl Pts',(3.99803874251361,137.82984290811,13.1658044236526));
#81660=CARTESIAN_POINT('Ctrl Pts',(3.99577333998866,137.826436475754,13.1988371011533));
#81661=CARTESIAN_POINT('Ctrl Pts',(3.99441046093843,137.82490493676,13.2185335185329));
#81662=CARTESIAN_POINT('Ctrl Pts',(3.9914118735987,137.82265130905,13.2614632296254));
#81663=CARTESIAN_POINT('Ctrl Pts',(3.98977107650809,137.822120233597,13.2846978653725));
#81664=CARTESIAN_POINT('Ctrl Pts',(3.98455776885865,137.822612178877,13.3577431471365));
#81665=CARTESIAN_POINT('Ctrl Pts',(3.9809252128372,137.826107399488,13.4074789277716));
#81666=CARTESIAN_POINT('Ctrl Pts',(3.97227842026258,137.841796571579,13.5242435099982));
#81667=CARTESIAN_POINT('Ctrl Pts',(3.96725672351583,137.856675228393,13.5907406938577));
#81668=CARTESIAN_POINT('Ctrl Pts',(3.96177807351904,137.88008103812,13.6646462785259));
#81669=CARTESIAN_POINT('Ctrl Pts',(3.96111095830634,137.883060131196,13.6736719509654));
#81670=CARTESIAN_POINT('Ctrl Pts',(3.96044919307343,137.886148212676,13.6826607614778));
#81671=CARTESIAN_POINT('Ctrl Pts',(3.86234166104071,137.886148208794,13.6826607501787));
#81672=CARTESIAN_POINT('Ctrl Pts',(3.863044184664,137.883006669279,13.6735163333174));
#81673=CARTESIAN_POINT('Ctrl Pts',(3.86374880232695,137.87997734707,13.6643320879671));
#81674=CARTESIAN_POINT('Ctrl Pts',(3.87062727730392,137.851575758721,13.5745197877842));
#81675=CARTESIAN_POINT('Ctrl Pts',(3.87692097289799,137.834839327831,13.4914185579036));
#81676=CARTESIAN_POINT('Ctrl Pts',(3.8838435464494,137.825914792403,13.3938124442637));
#81677=CARTESIAN_POINT('Ctrl Pts',(3.88478660732029,137.824917709719,13.3803647899413));
#81678=CARTESIAN_POINT('Ctrl Pts',(3.88627007993735,137.823697883064,13.3589255944686));
#81679=CARTESIAN_POINT('Ctrl Pts',(3.88681793719884,137.82332519609,13.3509441980889));
#81680=CARTESIAN_POINT('Ctrl Pts',(3.88790206571254,137.822743603264,13.3350101729448));
#81681=CARTESIAN_POINT('Ctrl Pts',(3.88843834175249,137.822533987937,13.3270579966016));
#81682=CARTESIAN_POINT('Ctrl Pts',(3.88986105329992,137.822189017246,13.3057935938219));
#81683=CARTESIAN_POINT('Ctrl Pts',(3.89073998378341,137.822198760501,13.2924797543214));
#81684=CARTESIAN_POINT('Ctrl Pts',(3.89540832308217,137.823463100492,13.2210098048795));
#81685=CARTESIAN_POINT('Ctrl Pts',(3.89902262471667,137.828799245817,13.1630003930873));
#81686=CARTESIAN_POINT('Ctrl Pts',(3.90764572898961,137.851806010317,13.0255159015268));
#81687=CARTESIAN_POINT('Ctrl Pts',(3.91262902588312,137.873457832592,12.9470237483517));
#81688=CARTESIAN_POINT('Ctrl Pts',(3.91922440940153,137.910633308223,12.8518772809854));
#81689=CARTESIAN_POINT('Ctrl Pts',(3.92059153722713,137.918774431264,12.8325762704663));
#81690=CARTESIAN_POINT('Ctrl Pts',(3.92288338263702,137.933097014266,12.8009993982069));
#81691=CARTESIAN_POINT('Ctrl Pts',(3.92379810211894,137.938986608803,12.788595914807));
#81692=CARTESIAN_POINT('Ctrl Pts',(3.92563433408657,137.951141418996,12.7641120885698));
#81693=CARTESIAN_POINT('Ctrl Pts',(3.92655556892097,137.957401834685,12.7520317388586));
#81694=CARTESIAN_POINT('Ctrl Pts',(3.92886694038054,137.973500777671,12.7222416038312));
#81695=CARTESIAN_POINT('Ctrl Pts',(3.93026574486999,137.983589286966,12.7046727021241));
#81696=CARTESIAN_POINT('Ctrl Pts',(3.93647404406036,138.02983654806,12.6287390669985));
#81697=CARTESIAN_POINT('Ctrl Pts',(3.94144587200666,138.070600854173,12.5733481309762));
#81698=CARTESIAN_POINT('Ctrl Pts',(3.95175854232748,138.163506789647,12.4678011336225));
#81699=CARTESIAN_POINT('Ctrl Pts',(3.9570835177498,138.215920007638,12.4182427606383));
#81700=CARTESIAN_POINT('Ctrl Pts',(3.96311442826415,138.28308441392,12.3654909836635));
#81701=CARTESIAN_POINT('Ctrl Pts',(3.96405268996194,138.293776834541,12.3573845226047));
#81702=CARTESIAN_POINT('Ctrl Pts',(3.965530460591,138.311043161827,12.3447528319018));
#81703=CARTESIAN_POINT('Ctrl Pts',(3.96607732259554,138.317528237061,12.3401088711434));
#81704=CARTESIAN_POINT('Ctrl Pts',(3.96716133334605,138.330585207647,12.3309580061969));
#81705=CARTESIAN_POINT('Ctrl Pts',(3.96769846150726,138.33715666421,12.3264511972035));
#81706=CARTESIAN_POINT('Ctrl Pts',(3.96912629279859,138.354882192617,12.3145574407366));
#81707=CARTESIAN_POINT('Ctrl Pts',(3.9700093949864,138.366117570292,12.3072930312282));
#81708=CARTESIAN_POINT('Ctrl Pts',(3.97478027087287,138.428142352453,12.2686725000216));
#81709=CARTESIAN_POINT('Ctrl Pts',(3.97848364990891,138.481141040819,12.2410171718372));
#81710=CARTESIAN_POINT('Ctrl Pts',(3.98707301726176,138.608805655808,12.1862970875214));
#81711=CARTESIAN_POINT('Ctrl Pts',(3.99193861258386,138.684551617322,12.1625211813024));
#81712=CARTESIAN_POINT('Ctrl Pts',(3.99841287816808,138.782798876687,12.1422586217277));
#81713=CARTESIAN_POINT('Ctrl Pts',(3.99979144442897,138.803600695929,12.1385489028142));
#81714=CARTESIAN_POINT('Ctrl Pts',(4.00209703201997,138.838100074831,12.1333497024605));
#81715=CARTESIAN_POINT('Ctrl Pts',(4.00301379278357,138.851744506969,12.1315374271211));
#81716=CARTESIAN_POINT('Ctrl Pts',(4.00484997318898,138.878904672416,12.1284133383298));
#81717=CARTESIAN_POINT('Ctrl Pts',(4.00576904704223,138.892417553609,12.1270953258911));
#81718=CARTESIAN_POINT('Ctrl Pts',(4.00806673190948,138.925978746086,12.1244066804823));
#81719=CARTESIAN_POINT('Ctrl Pts',(4.00945378589659,138.946044402116,12.1233150354261));
#81720=CARTESIAN_POINT('Ctrl Pts',(4.01590713115923,139.038458687569,12.1206560395116));
#81721=CARTESIAN_POINT('Ctrl Pts',(4.02115697858442,139.110816955669,12.1252456511503));
#81722=CARTESIAN_POINT('Ctrl Pts',(4.03146088357986,139.249519309731,12.1469750639376));
#81723=CARTESIAN_POINT('Ctrl Pts',(4.03648604885995,139.315718338391,12.1633163723464));
#81724=CARTESIAN_POINT('Ctrl Pts',(4.04226631500642,139.393128952584,12.1897148811974));
#81725=CARTESIAN_POINT('Ctrl Pts',(4.04322679105769,139.406040985135,12.1943715914929));
#81726=CARTESIAN_POINT('Ctrl Pts',(4.04473094170385,139.426382976811,12.2021123695186));
#81727=CARTESIAN_POINT('Ctrl Pts',(4.04528240065399,139.433867420922,12.2050485112206));
#81728=CARTESIAN_POINT('Ctrl Pts',(4.04636712325934,139.448653627604,12.2110245517681));
#81729=CARTESIAN_POINT('Ctrl Pts',(4.04690048201913,139.455955956674,12.2140617984208));
#81730=CARTESIAN_POINT('Ctrl Pts',(4.04830553178762,139.475258833131,12.2223194574133));
#81731=CARTESIAN_POINT('Ctrl Pts',(4.04917004630636,139.487204309322,12.2276668863286));
#81732=CARTESIAN_POINT('Ctrl Pts',(4.05110498771915,139.514021677953,12.240212444166));
#81733=CARTESIAN_POINT('Ctrl Pts',(4.0521697442321,139.528836410017,12.24752669628));
#81734=CARTESIAN_POINT('Ctrl Pts',(4.05572143299817,139.578225222409,12.2732169789663));
#81735=CARTESIAN_POINT('Ctrl Pts',(4.05815692151328,139.612037170705,12.2930051339613));
#81736=CARTESIAN_POINT('Ctrl Pts',(4.06584296724123,139.715931877936,12.3609783543525));
#81737=CARTESIAN_POINT('Ctrl Pts',(4.07104648270154,139.781807688376,12.4150732538963));
#81738=CARTESIAN_POINT('Ctrl Pts',(4.07786568259445,139.855653334548,12.4904483478774));
#81739=CARTESIAN_POINT('Ctrl Pts',(4.07920668689932,139.86963343173,12.505484979092));
#81740=CARTESIAN_POINT('Ctrl Pts',(4.08146721712582,139.892245704048,12.5311182722933));
#81741=CARTESIAN_POINT('Ctrl Pts',(4.08237733608271,139.901099516073,12.5415139136248));
#81742=CARTESIAN_POINT('Ctrl Pts',(4.08421415692083,139.91845665087,12.5626265990101));
#81743=CARTESIAN_POINT('Ctrl Pts',(4.08514074215499,139.926957956123,12.5733425345301));
#81744=CARTESIAN_POINT('Ctrl Pts',(4.08748571731678,139.947826438644,12.6006096138682));
#81745=CARTESIAN_POINT('Ctrl Pts',(4.08891333341489,139.959947883799,12.6173420794325));
#81746=CARTESIAN_POINT('Ctrl Pts',(4.0920807929871,139.985560860128,12.6547302026406));
#81747=CARTESIAN_POINT('Ctrl Pts',(4.09382677070315,139.998855882451,12.6755081253717));
#81748=CARTESIAN_POINT('Ctrl Pts',(4.09958412488075,140.04006275325,12.7445937437427));
#81749=CARTESIAN_POINT('Ctrl Pts',(4.10367059351438,140.065195490999,12.7944663958533));
#81750=CARTESIAN_POINT('Ctrl Pts',(4.11195730571419,140.1086890359,12.8985562526817));
#81751=CARTESIAN_POINT('Ctrl Pts',(4.11614694660291,140.126829313793,12.9527174174099));
#81752=CARTESIAN_POINT('Ctrl Pts',(4.12122732478859,140.144610884334,13.0221940472427));
#81753=CARTESIAN_POINT('Ctrl Pts',(4.12225596707458,140.147982242468,13.0364719296508));
#81754=CARTESIAN_POINT('Ctrl Pts',(4.12384081880359,140.152827789133,13.0588550045718));
#81755=CARTESIAN_POINT('Ctrl Pts',(4.12440619028848,140.154485099265,13.066918499123));
#81756=CARTESIAN_POINT('Ctrl Pts',(4.12549530239638,140.157540678443,13.0826181014993));
#81757=CARTESIAN_POINT('Ctrl Pts',(4.1260194683181,140.158948231242,13.0902517844252));
#81758=CARTESIAN_POINT('Ctrl Pts',(4.12736690079609,140.162398491818,13.1100600443844));
#81759=CARTESIAN_POINT('Ctrl Pts',(4.12818403990934,140.164325520632,13.1222542469693));
#81760=CARTESIAN_POINT('Ctrl Pts',(4.13305057899264,140.174765558045,13.1958012608342));
#81761=CARTESIAN_POINT('Ctrl Pts',(4.1368928406087,140.178620466317,13.257724628146));
#81762=CARTESIAN_POINT('Ctrl Pts',(4.14560146851328,140.176268320244,13.3985379795315));
#81763=CARTESIAN_POINT('Ctrl Pts',(4.15044849390026,140.167031755995,13.4770658970451));
#81764=CARTESIAN_POINT('Ctrl Pts',(4.15690352262628,140.145453726776,13.5747330931787));
#81765=CARTESIAN_POINT('Ctrl Pts',(4.15828370065542,140.140334965799,13.5952602056001));
#81766=CARTESIAN_POINT('Ctrl Pts',(4.16059122597909,140.1309765661,13.6289021736007));
#81767=CARTESIAN_POINT('Ctrl Pts',(4.16150827554353,140.127054431181,13.6421007379544));
#81768=CARTESIAN_POINT('Ctrl Pts',(4.16334445807152,140.118808279858,13.668167500933));
#81769=CARTESIAN_POINT('Ctrl Pts',(4.16426323575358,140.114491376416,13.681035721279));
#81770=CARTESIAN_POINT('Ctrl Pts',(4.16655903885429,140.103241826412,13.7127412809699));
#81771=CARTESIAN_POINT('Ctrl Pts',(4.16794447643526,140.096048407646,13.7314808158143));
#81772=CARTESIAN_POINT('Ctrl Pts',(4.17099985047535,140.079321879548,13.7719335935678));
#81773=CARTESIAN_POINT('Ctrl Pts',(4.17267518388653,140.069604863876,13.7935608790472));
#81774=CARTESIAN_POINT('Ctrl Pts',(4.1780547896094,140.036683170128,13.8612895158023));
#81775=CARTESIAN_POINT('Ctrl Pts',(4.18182339601313,140.011099937413,13.9061633292076));
#81776=CARTESIAN_POINT('Ctrl Pts',(4.19035047334182,139.947084298549,14.0030586809752));
#81777=CARTESIAN_POINT('Ctrl Pts',(4.19510806201368,139.907140701683,14.0538946776807));
#81778=CARTESIAN_POINT('Ctrl Pts',(4.20066676073147,139.853677786797,14.1114964363587));
#81779=CARTESIAN_POINT('Ctrl Pts',(4.20165013783448,139.843941659251,14.1216171548754));
#81780=CARTESIAN_POINT('Ctrl Pts',(4.20318144533018,139.828304239512,14.1373009186825));
#81781=CARTESIAN_POINT('Ctrl Pts',(4.20373761376925,139.822522842852,14.1429809751423));
#81782=CARTESIAN_POINT('Ctrl Pts',(4.20482347704923,139.811024340808,14.1540469892431));
#81783=CARTESIAN_POINT('Ctrl Pts',(4.20535338184087,139.805311151524,14.1594362668702));
#81784=CARTESIAN_POINT('Ctrl Pts',(4.20673719494012,139.790135862876,14.1734669826889));
#81785=CARTESIAN_POINT('Ctrl Pts',(4.20758431720912,139.78058558091,14.182012151804));
#81786=CARTESIAN_POINT('Ctrl Pts',(4.20947287529198,139.758757792836,14.2009103757974));
#81787=CARTESIAN_POINT('Ctrl Pts',(4.21050904345583,139.746404046763,14.2111717419622));
#81788=CARTESIAN_POINT('Ctrl Pts',(4.2139136676338,139.704715992399,14.2443819634546));
#81789=CARTESIAN_POINT('Ctrl Pts',(4.21623507960074,139.674502187942,14.2661930787221));
#81790=CARTESIAN_POINT('Ctrl Pts',(4.22405775170889,139.568755265612,14.335148844342));
#81791=CARTESIAN_POINT('Ctrl Pts',(4.22949294553982,139.488944500588,14.3751499681993));
#81792=CARTESIAN_POINT('Ctrl Pts',(4.23654555759565,139.386600936416,14.412670383838));
#81793=CARTESIAN_POINT('Ctrl Pts',(4.23785427001054,139.367637298898,14.4190792674328));
#81794=CARTESIAN_POINT('Ctrl Pts',(4.23998668599268,139.33685795315,14.4286145707674));
#81795=CARTESIAN_POINT('Ctrl Pts',(4.24080036841133,139.325140370329,14.4320458694704));
#81796=CARTESIAN_POINT('Ctrl Pts',(4.24252755420066,139.300341246337,14.4388910983532));
#81797=CARTESIAN_POINT('Ctrl Pts',(4.24344227492753,139.287250105735,14.442263169512));
#81798=CARTESIAN_POINT('Ctrl Pts',(4.24571213738936,139.254887704861,14.4500077152275));
#81799=CARTESIAN_POINT('Ctrl Pts',(4.24707526915934,139.235559524803,14.4541217938672));
#81800=CARTESIAN_POINT('Ctrl Pts',(4.25007177527111,139.193326942467,14.4620061251788));
#81801=CARTESIAN_POINT('Ctrl Pts',(4.25171017753887,139.170396420552,14.4655893267413));
#81802=CARTESIAN_POINT('Ctrl Pts',(4.25690135201986,139.098224813765,14.4746919794484));
#81803=CARTESIAN_POINT('Ctrl Pts',(4.2605134260896,139.048735289351,14.4777832766728));
#81804=CARTESIAN_POINT('Ctrl Pts',(4.26916697635402,138.930821355767,14.4777034180323));
#81805=CARTESIAN_POINT('Ctrl Pts',(4.27421714700351,138.862569582109,14.4717018650513));
#81806=CARTESIAN_POINT('Ctrl Pts',(4.28001937562035,138.781718469343,14.4574265510309));
#81807=CARTESIAN_POINT('Ctrl Pts',(4.28097887678128,138.768258454996,14.4548068863584));
#81808=CARTESIAN_POINT('Ctrl Pts',(4.28248187046343,138.746986105409,14.4502797992677));
#81809=CARTESIAN_POINT('Ctrl Pts',(4.28303312823117,138.739142691218,14.4485265001495));
#81810=CARTESIAN_POINT('Ctrl Pts',(4.28411781100202,138.723615338628,14.4448882751248));
#81811=CARTESIAN_POINT('Ctrl Pts',(4.28465132612426,138.715931269189,14.4430059525042));
#81812=CARTESIAN_POINT('Ctrl Pts',(4.28605732832364,138.695576341321,14.437801769148));
#81813=CARTESIAN_POINT('Ctrl Pts',(4.28692262128515,138.682940520705,14.4343456051301));
#81814=CARTESIAN_POINT('Ctrl Pts',(4.2888596454158,138.654485328609,14.4260498427597));
#81815=CARTESIAN_POINT('Ctrl Pts',(4.28992568776206,138.638704781494,14.4210862841359));
#81816=CARTESIAN_POINT('Ctrl Pts',(4.29348409797901,138.585859886533,14.4032328019405));
#81817=CARTESIAN_POINT('Ctrl Pts',(4.29592481694604,138.549334961245,14.38882324173));
#81818=CARTESIAN_POINT('Ctrl Pts',(4.30360507289333,138.43634369359,14.3375845565311));
#81819=CARTESIAN_POINT('Ctrl Pts',(4.30879834105075,138.363109819112,14.2943136048585));
#81820=CARTESIAN_POINT('Ctrl Pts',(4.3156071833194,138.278696391242,14.2312563983944));
#81821=CARTESIAN_POINT('Ctrl Pts',(4.31694951655112,138.262558123966,14.218529679677));
#81822=CARTESIAN_POINT('Ctrl Pts',(4.31921163723704,138.236262045307,14.1966526354109));
#81823=CARTESIAN_POINT('Ctrl Pts',(4.32012198792993,138.225915443102,14.1877357063215));
#81824=CARTESIAN_POINT('Ctrl Pts',(4.32195876188461,138.205525209974,14.1695354239991));
#81825=CARTESIAN_POINT('Ctrl Pts',(4.32288506011634,138.195483563498,14.1602530566789));
#81826=CARTESIAN_POINT('Ctrl Pts',(4.32522824159195,138.170697503094,14.1365275567089));
#81827=CARTESIAN_POINT('Ctrl Pts',(4.32665432097801,138.156167400717,14.1218682590884));
#81828=CARTESIAN_POINT('Ctrl Pts',(4.32981767871815,138.125159018708,14.0888947001723));
#81829=CARTESIAN_POINT('Ctrl Pts',(4.33156106352158,138.108855347333,14.0704301746894));
#81830=CARTESIAN_POINT('Ctrl Pts',(4.33730411268014,138.057653330605,14.0086407010644));
#81831=CARTESIAN_POINT('Ctrl Pts',(4.34137844510893,138.025244732418,13.9633551692109));
#81832=CARTESIAN_POINT('Ctrl Pts',(4.34967225567738,137.966194692202,13.867119329472));
#81833=CARTESIAN_POINT('Ctrl Pts',(4.35388127828011,137.939831059775,13.8161594791115));
#81834=CARTESIAN_POINT('Ctrl Pts',(4.35897900498236,137.911511664804,13.7500034285213));
#81835=CARTESIAN_POINT('Ctrl Pts',(4.36000695149036,137.905994771712,13.7364201540833));
#81836=CARTESIAN_POINT('Ctrl Pts',(4.36159098162245,137.897778735615,13.7150555054399));
#81837=CARTESIAN_POINT('Ctrl Pts',(4.36215621281117,137.89490532634,13.7073432959549));
#81838=CARTESIAN_POINT('Ctrl Pts',(4.36312428911873,137.89008165393,13.693969755074));
#81839=CARTESIAN_POINT('Ctrl Pts',(4.36352933703883,137.888093373265,13.6883227493715));
#81840=CARTESIAN_POINT('Ctrl Pts',(4.36393196101569,137.88614821267,13.68266076146));
#81841=CARTESIAN_POINT('Origin',(1.13913288526384,139.,13.3));
#81842=CARTESIAN_POINT('',(4.96216798774592,137.886148228644,13.6826608079585));
#81843=CARTESIAN_POINT('',(4.86231567683355,137.88614821265,13.6826607614027));
#81844=CARTESIAN_POINT('',(1.13913288526384,137.88614821265,13.6826607614027));
#81845=CARTESIAN_POINT('Ctrl Pts',(4.96216799084082,137.886148228708,13.6826608081431));
#81846=CARTESIAN_POINT('Ctrl Pts',(4.9613252995471,137.89048591061,13.6952869631277));
#81847=CARTESIAN_POINT('Ctrl Pts',(4.96047762550991,137.8950399563,13.7078442468175));
#81848=CARTESIAN_POINT('Ctrl Pts',(4.95792916134544,137.909276554256,13.7451080279077));
#81849=CARTESIAN_POINT('Ctrl Pts',(4.95621286131286,137.919578019688,13.7695604010044));
#81850=CARTESIAN_POINT('Ctrl Pts',(4.95350210532465,137.936863001935,13.807002265906));
#81851=CARTESIAN_POINT('Ctrl Pts',(4.95252681100481,137.943279953068,13.8202444465315));
#81852=CARTESIAN_POINT('Ctrl Pts',(4.95067059480853,137.955850200518,13.8449921117628));
#81853=CARTESIAN_POINT('Ctrl Pts',(4.94979165683997,137.961949909538,13.8565224089485));
#81854=CARTESIAN_POINT('Ctrl Pts',(4.94777226926544,137.976289436622,13.8825722215191));
#81855=CARTESIAN_POINT('Ctrl Pts',(4.94662768265399,137.984648825597,13.8970223224393));
#81856=CARTESIAN_POINT('Ctrl Pts',(4.94291149710467,138.012511706058,13.9429076759284));
#81857=CARTESIAN_POINT('Ctrl Pts',(4.9402986399165,138.033188292644,13.973600797449));
#81858=CARTESIAN_POINT('Ctrl Pts',(4.93627484675891,138.066660717844,14.0185656259162));
#81859=CARTESIAN_POINT('Ctrl Pts',(4.93489550304426,138.078418169034,14.0335841144089));
#81860=CARTESIAN_POINT('Ctrl Pts',(4.92866410203643,138.132853176199,14.0997421921198));
#81861=CARTESIAN_POINT('Ctrl Pts',(4.92372821192867,138.179456688207,14.1474901430497));
#81862=CARTESIAN_POINT('Ctrl Pts',(4.91732836829574,138.246143999636,14.205129992097));
#81863=CARTESIAN_POINT('Ctrl Pts',(4.91577667980507,138.262827191691,14.2187684830071));
#81864=CARTESIAN_POINT('Ctrl Pts',(4.91311936018036,138.292427893299,14.2416413313572));
#81865=CARTESIAN_POINT('Ctrl Pts',(4.91200430023662,138.305175196318,14.2510863440971));
#81866=CARTESIAN_POINT('Ctrl Pts',(4.9103199526921,138.324989139761,14.2651562472053));
#81867=CARTESIAN_POINT('Ctrl Pts',(4.90973960676602,138.331920707704,14.269967171942));
#81868=CARTESIAN_POINT('Ctrl Pts',(4.90864787105764,138.345171151997,14.2789543374092));
#81869=CARTESIAN_POINT('Ctrl Pts',(4.90813565327589,138.351479523497,14.283144755104));
#81870=CARTESIAN_POINT('Ctrl Pts',(4.90685641495799,138.367454352868,14.2935355747707));
#81871=CARTESIAN_POINT('Ctrl Pts',(4.90609439039589,138.377172187341,14.2996561782074));
#81872=CARTESIAN_POINT('Ctrl Pts',(4.90265881191537,138.421819303103,14.3268724874282));
#81873=CARTESIAN_POINT('Ctrl Pts',(4.90007373103673,138.457744163936,14.3462883582678));
#81874=CARTESIAN_POINT('Ctrl Pts',(4.89321998972087,138.556833765062,14.3933639494403));
#81875=CARTESIAN_POINT('Ctrl Pts',(4.88902376597599,138.621533098448,14.4174095427146));
#81876=CARTESIAN_POINT('Ctrl Pts',(4.88211734985537,138.727804245728,14.446608742687));
#81877=CARTESIAN_POINT('Ctrl Pts',(4.87949152513504,138.768189360058,14.4554503232474));
#81878=CARTESIAN_POINT('Ctrl Pts',(4.87568232269473,138.825895553563,14.4649367022087));
#81879=CARTESIAN_POINT('Ctrl Pts',(4.87455338219,138.842896466133,14.4673509789729));
#81880=CARTESIAN_POINT('Ctrl Pts',(4.87254245815222,138.872951369964,14.4709506150809));
#81881=CARTESIAN_POINT('Ctrl Pts',(4.87166549338506,138.885983972806,14.4722913542373));
#81882=CARTESIAN_POINT('Ctrl Pts',(4.86980605784833,138.913442240746,14.4746539486601));
#81883=CARTESIAN_POINT('Ctrl Pts',(4.86882224137559,138.927869704442,14.4756280588304));
#81884=CARTESIAN_POINT('Ctrl Pts',(4.86610451712464,138.967428420489,14.4775680709763));
#81885=CARTESIAN_POINT('Ctrl Pts',(4.86435434618052,138.992577150795,14.4779949933377));
#81886=CARTESIAN_POINT('Ctrl Pts',(4.85927096061618,139.064659954666,14.4769104184862));
#81887=CARTESIAN_POINT('Ctrl Pts',(4.85588360827625,139.111512114175,14.4733981652422));
#81888=CARTESIAN_POINT('Ctrl Pts',(4.84632440991366,139.241212121811,14.4558367887005));
#81889=CARTESIAN_POINT('Ctrl Pts',(4.84007526894427,139.322958176544,14.4357117140014));
#81890=CARTESIAN_POINT('Ctrl Pts',(4.83318649233745,139.414616168242,14.4024392536724));
#81891=CARTESIAN_POINT('Ctrl Pts',(4.83223797125018,139.427280092607,14.3975931108697));
#81892=CARTESIAN_POINT('Ctrl Pts',(4.83075012865868,139.447255080425,14.3895510720333));
#81893=CARTESIAN_POINT('Ctrl Pts',(4.83020322980795,139.454621835428,14.3864978792897));
#81894=CARTESIAN_POINT('Ctrl Pts',(4.8291259101538,139.469193014806,14.3802846165405));
#81895=CARTESIAN_POINT('Ctrl Pts',(4.82859541619746,139.476397882888,14.3771267348045));
#81896=CARTESIAN_POINT('Ctrl Pts',(4.82719670964036,139.495454913528,14.3685454414609));
#81897=CARTESIAN_POINT('Ctrl Pts',(4.82633562724428,139.507249995601,14.3629968996757));
#81898=CARTESIAN_POINT('Ctrl Pts',(4.82440814501577,139.53372266143,14.3500028343377));
#81899=CARTESIAN_POINT('Ctrl Pts',(4.82334737870692,139.54834136322,14.3424431087491));
#81900=CARTESIAN_POINT('Ctrl Pts',(4.81980990964581,139.597041397762,14.3159509259341));
#81901=CARTESIAN_POINT('Ctrl Pts',(4.8173843326595,139.630341466459,14.2956328269391));
#81902=CARTESIAN_POINT('Ctrl Pts',(4.80968108270087,139.733207006002,14.2256358049688));
#81903=CARTESIAN_POINT('Ctrl Pts',(4.80445221475622,139.798393634498,14.1700346312013));
#81904=CARTESIAN_POINT('Ctrl Pts',(4.79761052412415,139.871002775977,14.0930110123185));
#81905=CARTESIAN_POINT('Ctrl Pts',(4.79627607992906,139.884624445623,14.077786481273));
#81906=CARTESIAN_POINT('Ctrl Pts',(4.79402749124873,139.906628177206,14.0518674686578));
#81907=CARTESIAN_POINT('Ctrl Pts',(4.79312267046347,139.915233716945,14.0413680323928));
#81908=CARTESIAN_POINT('Ctrl Pts',(4.79129765868563,139.932083064938,14.0200699435258));
#81909=CARTESIAN_POINT('Ctrl Pts',(4.790377598455,139.940325325732,14.0092727390762));
#81910=CARTESIAN_POINT('Ctrl Pts',(4.78805230267445,139.960517041506,13.9818512694132));
#81911=CARTESIAN_POINT('Ctrl Pts',(4.78663803717632,139.972222797628,13.9650540436754));
#81912=CARTESIAN_POINT('Ctrl Pts',(4.78097552468065,140.016812226229,13.8973756040288));
#81913=CARTESIAN_POINT('Ctrl Pts',(4.77660621608246,140.04618308808,13.8443011909821));
#81914=CARTESIAN_POINT('Ctrl Pts',(4.76682337943164,140.101715711064,13.7226884379973));
#81915=CARTESIAN_POINT('Ctrl Pts',(4.76139931737264,140.12583128198,13.6534795450859));
#81916=CARTESIAN_POINT('Ctrl Pts',(4.75496914222423,140.147484467288,13.5658352417451));
#81917=CARTESIAN_POINT('Ctrl Pts',(4.75376120304258,140.151232750708,13.5491028030434));
#81918=CARTESIAN_POINT('Ctrl Pts',(4.75196854485953,140.156326798652,13.5237828407258));
#81919=CARTESIAN_POINT('Ctrl Pts',(4.75137061678066,140.157944945356,13.5152532007076));
#81920=CARTESIAN_POINT('Ctrl Pts',(4.75026676002308,140.160782935531,13.4993341715396));
#81921=CARTESIAN_POINT('Ctrl Pts',(4.74975966750834,140.162026783495,13.4919502356081));
#81922=CARTESIAN_POINT('Ctrl Pts',(4.74852142361377,140.164913631506,13.4737551502107));
#81923=CARTESIAN_POINT('Ctrl Pts',(4.74779457164697,140.166476647137,13.4629321162488));
#81924=CARTESIAN_POINT('Ctrl Pts',(4.74485017356674,140.172251567791,13.4185864259944));
#81925=CARTESIAN_POINT('Ctrl Pts',(4.74269258476664,140.175171213505,13.384908955409));
#81926=CARTESIAN_POINT('Ctrl Pts',(4.73554572198398,140.180105707555,13.2713964457361));
#81927=CARTESIAN_POINT('Ctrl Pts',(4.73070949697103,140.175455430474,13.1914965531398));
#81928=CARTESIAN_POINT('Ctrl Pts',(4.72321844326576,140.15647967358,13.0737081938852));
#81929=CARTESIAN_POINT('Ctrl Pts',(4.72070459667175,140.148246756207,13.035080877252));
#81930=CARTESIAN_POINT('Ctrl Pts',(4.71703321833284,140.133757077295,12.9806669095727));
#81931=CARTESIAN_POINT('Ctrl Pts',(4.71592490155441,140.1290747447,12.964487099358));
#81932=CARTESIAN_POINT('Ctrl Pts',(4.71393715717662,140.120148383291,12.9359488486083));
#81933=CARTESIAN_POINT('Ctrl Pts',(4.7130623511339,140.116042556198,12.9235499625691));
#81934=CARTESIAN_POINT('Ctrl Pts',(4.71119308973944,140.106902386145,12.8974131340711));
#81935=CARTESIAN_POINT('Ctrl Pts',(4.71019705197139,140.101816572499,12.8836956835069));
#81936=CARTESIAN_POINT('Ctrl Pts',(4.70740270616179,140.086962644944,12.8458121831326));
#81937=CARTESIAN_POINT('Ctrl Pts',(4.70558653630758,140.07664638402,12.8218716244175));
#81938=CARTESIAN_POINT('Ctrl Pts',(4.69702201018986,140.024987822691,12.712156798395));
#81939=CARTESIAN_POINT('Ctrl Pts',(4.68996517977603,139.974138513674,12.6312633341923));
#81940=CARTESIAN_POINT('Ctrl Pts',(4.68244742533774,139.909202371822,12.5513298344739));
#81941=CARTESIAN_POINT('Ctrl Pts',(4.68187890052142,139.904221332689,12.5453214232013));
#81942=CARTESIAN_POINT('Ctrl Pts',(4.6790217057882,139.878820360923,12.5152938740889));
#81943=CARTESIAN_POINT('Ctrl Pts',(4.67675761584631,139.857499753496,12.4920498436192));
#81944=CARTESIAN_POINT('Ctrl Pts',(4.67377944302391,139.827546088066,12.461917322213));
#81945=CARTESIAN_POINT('Ctrl Pts',(4.67301813342315,139.819713506166,12.454254829944));
#81946=CARTESIAN_POINT('Ctrl Pts',(4.67174970788768,139.806347543848,12.441539276432));
#81947=CARTESIAN_POINT('Ctrl Pts',(4.67123843646845,139.800870977784,12.4364278459563));
#81948=CARTESIAN_POINT('Ctrl Pts',(4.67014415123697,139.78895099407,12.4255135426399));
#81949=CARTESIAN_POINT('Ctrl Pts',(4.66956241667986,139.782491701871,12.4197290284814));
#81950=CARTESIAN_POINT('Ctrl Pts',(4.66784838941719,139.76311613002,12.4027593730804));
#81951=CARTESIAN_POINT('Ctrl Pts',(4.66672986621822,139.750019157291,12.3917828967142));
#81952=CARTESIAN_POINT('Ctrl Pts',(4.6640785088692,139.718019701095,12.3661289065347));
#81953=CARTESIAN_POINT('Ctrl Pts',(4.66255962362434,139.698899397505,12.3517345962688));
#81954=CARTESIAN_POINT('Ctrl Pts',(4.65555368993483,139.607801821801,12.2874071340989));
#81955=CARTESIAN_POINT('Ctrl Pts',(4.65026248277115,139.530838404914,12.2450219357949));
#81956=CARTESIAN_POINT('Ctrl Pts',(4.64260116432481,139.418888895284,12.198749778483));
#81957=CARTESIAN_POINT('Ctrl Pts',(4.64045004234308,139.387362140476,12.187269026011));
#81958=CARTESIAN_POINT('Ctrl Pts',(4.63721540920876,139.340232943176,12.1723522828684));
#81959=CARTESIAN_POINT('Ctrl Pts',(4.63616584470166,139.32498044869,12.1678624212858));
#81960=CARTESIAN_POINT('Ctrl Pts',(4.63424175816761,139.297128528458,12.1602728733271));
#81961=CARTESIAN_POINT('Ctrl Pts',(4.63337073457056,139.28455969946,12.1570699758933));
#81962=CARTESIAN_POINT('Ctrl Pts',(4.63144491741864,139.256874525638,12.1504999687944));
#81963=CARTESIAN_POINT('Ctrl Pts',(4.63038743311304,139.241739707553,12.1472221734113));
#81964=CARTESIAN_POINT('Ctrl Pts',(4.62718781068581,139.196173571643,12.1382905377861));
#81965=CARTESIAN_POINT('Ctrl Pts',(4.62501822496883,139.165581647883,12.1335372445353));
#81966=CARTESIAN_POINT('Ctrl Pts',(4.61964954794539,139.090630107562,12.1248992589631));
#81967=CARTESIAN_POINT('Ctrl Pts',(4.61641907960809,139.04617038347,12.1223144581953));
#81968=CARTESIAN_POINT('Ctrl Pts',(4.60750829287687,138.924494747572,12.1221414500323));
#81969=CARTESIAN_POINT('Ctrl Pts',(4.60178273094873,138.847487272822,12.1296184158409));
#81970=CARTESIAN_POINT('Ctrl Pts',(4.59538602336788,138.758620544359,12.1471728450399));
#81971=CARTESIAN_POINT('Ctrl Pts',(4.59444923097471,138.74552392104,12.1499928459592));
#81972=CARTESIAN_POINT('Ctrl Pts',(4.59297532076422,138.724744761439,12.1548394585048));
#81973=CARTESIAN_POINT('Ctrl Pts',(4.59243085200732,138.717030087759,12.1567213155882));
#81974=CARTESIAN_POINT('Ctrl Pts',(4.59135391983659,138.701681644032,12.1606301785878));
#81975=CARTESIAN_POINT('Ctrl Pts',(4.59082144396414,138.694048065588,12.1626562288044));
#81976=CARTESIAN_POINT('Ctrl Pts',(4.58941076345201,138.673724598745,12.1682697717036));
#81977=CARTESIAN_POINT('Ctrl Pts',(4.58853991019236,138.661073209767,12.1719939654237));
#81978=CARTESIAN_POINT('Ctrl Pts',(4.58407605119098,138.595859410489,12.1923873027835));
#81979=CARTESIAN_POINT('Ctrl Pts',(4.58064013229017,138.544446853908,12.2125220829568));
#81980=CARTESIAN_POINT('Ctrl Pts',(4.57193430950254,138.417435340018,12.2728596702846));
#81981=CARTESIAN_POINT('Ctrl Pts',(4.56670385088533,138.344469215051,12.3178204197468));
#81982=CARTESIAN_POINT('Ctrl Pts',(4.55986055406412,138.260889796805,12.382815028404));
#81983=CARTESIAN_POINT('Ctrl Pts',(4.55852632032026,138.245097389695,12.395768761651));
#81984=CARTESIAN_POINT('Ctrl Pts',(4.55627798356501,138.219382540497,12.4180047009295));
#81985=CARTESIAN_POINT('Ctrl Pts',(4.55537319956294,138.209269269964,12.427060017984));
#81986=CARTESIAN_POINT('Ctrl Pts',(4.55354818068691,138.189353378723,12.4455225950455));
#81987=CARTESIAN_POINT('Ctrl Pts',(4.55262807525838,138.179552537963,12.454928692182));
#81988=CARTESIAN_POINT('Ctrl Pts',(4.55030249735283,138.155392075785,12.4789325648475));
#81989=CARTESIAN_POINT('Ctrl Pts',(4.54888799024572,138.14124686072,12.4937387315138));
#81990=CARTESIAN_POINT('Ctrl Pts',(4.54272492976738,138.081995900503,12.559087076731));
#81991=CARTESIAN_POINT('Ctrl Pts',(4.53781971062446,138.040917127637,12.6130931730742));
#81992=CARTESIAN_POINT('Ctrl Pts',(4.52753839709693,137.965961330011,12.7315704520613));
#81993=CARTESIAN_POINT('Ctrl Pts',(4.5221752102372,137.932945399868,12.7962698811426));
#81994=CARTESIAN_POINT('Ctrl Pts',(4.51611600925115,137.901146070876,12.8759801560607));
#81995=CARTESIAN_POINT('Ctrl Pts',(4.51518381645701,137.896416639259,12.8884461283159));
#81996=CARTESIAN_POINT('Ctrl Pts',(4.51371537260885,137.889213996671,12.9084487797378));
#81997=CARTESIAN_POINT('Ctrl Pts',(4.51317185874504,137.886603606834,12.9159344011284));
#81998=CARTESIAN_POINT('Ctrl Pts',(4.51209504567939,137.881539828194,12.9309410914345));
#81999=CARTESIAN_POINT('Ctrl Pts',(4.51156175816356,137.879086234145,12.938461658508));
#82000=CARTESIAN_POINT('Ctrl Pts',(4.51014620188852,137.872726347014,12.9586428481712));
#82001=CARTESIAN_POINT('Ctrl Pts',(4.50927137505273,137.868957478702,12.9713460096499));
#82002=CARTESIAN_POINT('Ctrl Pts',(4.50730704624036,137.860891289261,13.0003177730212));
#82003=CARTESIAN_POINT('Ctrl Pts',(4.50622350755357,137.856726541701,13.0166204862463));
#82004=CARTESIAN_POINT('Ctrl Pts',(4.50256585321356,137.843719040175,13.072505022373));
#82005=CARTESIAN_POINT('Ctrl Pts',(4.50004657915196,137.836571316656,13.112453402786));
#82006=CARTESIAN_POINT('Ctrl Pts',(4.49244192208725,137.821198628009,13.234396142371));
#82007=CARTESIAN_POINT('Ctrl Pts',(4.48739240194791,137.819496763251,13.3169459879458));
#82008=CARTESIAN_POINT('Ctrl Pts',(4.48073255667064,137.828164430568,13.4197005283594));
#82009=CARTESIAN_POINT('Ctrl Pts',(4.47937598140029,137.830458521735,13.4403547783222));
#82010=CARTESIAN_POINT('Ctrl Pts',(4.47710085707123,137.835161371434,13.4744478740848));
#82011=CARTESIAN_POINT('Ctrl Pts',(4.47619212898237,137.837259635268,13.4879252756146));
#82012=CARTESIAN_POINT('Ctrl Pts',(4.47436759543913,137.841903277184,13.5146855496282));
#82013=CARTESIAN_POINT('Ctrl Pts',(4.4734520562467,137.844444332442,13.5279670530128));
#82014=CARTESIAN_POINT('Ctrl Pts',(4.47115513176393,137.851336379611,13.5609065787977));
#82015=CARTESIAN_POINT('Ctrl Pts',(4.46976518431913,137.855963689517,13.580501673713));
#82016=CARTESIAN_POINT('Ctrl Pts',(4.46669507625253,137.8671641113,13.6230271568453));
#82017=CARTESIAN_POINT('Ctrl Pts',(4.46500937475407,137.873936130758,13.645895540348));
#82018=CARTESIAN_POINT('Ctrl Pts',(4.46295069534819,137.882951217905,13.6732582824354));
#82019=CARTESIAN_POINT('Ctrl Pts',(4.46259508558876,137.884534942957,13.6779648440736));
#82020=CARTESIAN_POINT('Ctrl Pts',(4.46223878927246,137.886148214676,13.6826607672995));
#82021=CARTESIAN_POINT('Ctrl Pts',(4.36393196101569,137.88614821267,13.68266076146));
#82022=CARTESIAN_POINT('Ctrl Pts',(4.36405144554922,137.885570957912,13.6809804840216));
#82023=CARTESIAN_POINT('Ctrl Pts',(4.36417071710138,137.884997500726,13.6792988871397));
#82024=CARTESIAN_POINT('Ctrl Pts',(4.36511745336918,137.880467884761,13.6659172675373));
#82025=CARTESIAN_POINT('Ctrl Pts',(4.36593501476838,137.876691993988,13.6541564027392));
#82026=CARTESIAN_POINT('Ctrl Pts',(4.36774537884669,137.868659432261,13.6277150273824));
#82027=CARTESIAN_POINT('Ctrl Pts',(4.36873355853044,137.864502055418,13.6130065211228));
#82028=CARTESIAN_POINT('Ctrl Pts',(4.37190087553844,137.851974119104,13.5651428538918));
#82029=CARTESIAN_POINT('Ctrl Pts',(4.37403970187651,137.844760289681,13.5317016580991));
#82030=CARTESIAN_POINT('Ctrl Pts',(4.38212051367179,137.822880257343,13.4034012443494));
#82031=CARTESIAN_POINT('Ctrl Pts',(4.38795625824047,137.818370028255,13.3072028793761));
#82032=CARTESIAN_POINT('Ctrl Pts',(4.39541264590132,137.827006824096,13.1925575619454));
#82033=CARTESIAN_POINT('Ctrl Pts',(4.39665886850501,137.828894951517,13.1736284566379));
#82034=CARTESIAN_POINT('Ctrl Pts',(4.39879815104802,137.832875922405,13.1415945001671));
#82035=CARTESIAN_POINT('Ctrl Pts',(4.39968372209413,137.834733406378,13.1284638339523));
#82036=CARTESIAN_POINT('Ctrl Pts',(4.40151837989025,137.839005956364,13.1015466574256));
#82037=CARTESIAN_POINT('Ctrl Pts',(4.40246812080317,137.841445848996,13.0877662885772));
#82038=CARTESIAN_POINT('Ctrl Pts',(4.40495594458373,137.848421139151,13.0520861656815));
#82039=CARTESIAN_POINT('Ctrl Pts',(4.40650573473733,137.853335598707,13.0302672166213));
#82040=CARTESIAN_POINT('Ctrl Pts',(4.41000398135935,137.865675142677,12.9819447172741));
#82041=CARTESIAN_POINT('Ctrl Pts',(4.41196102243564,137.873414009073,12.9555354072992));
#82042=CARTESIAN_POINT('Ctrl Pts',(4.41903390439452,137.904350128257,12.8622095710433));
#82043=CARTESIAN_POINT('Ctrl Pts',(4.42427000287582,137.932645617921,12.7971457821304));
#82044=CARTESIAN_POINT('Ctrl Pts',(4.43246509954726,137.98640693346,12.6988116605395));
#82045=CARTESIAN_POINT('Ctrl Pts',(4.43545465610256,138.008096517766,12.6636616749825));
#82046=CARTESIAN_POINT('Ctrl Pts',(4.43918092603017,138.038273979434,12.6200616940964));
#82047=CARTESIAN_POINT('Ctrl Pts',(4.43999893617289,138.045103481009,12.6105032970942));
#82048=CARTESIAN_POINT('Ctrl Pts',(4.44132976945041,138.056571872968,12.5949497583282));
#82049=CARTESIAN_POINT('Ctrl Pts',(4.44184780296393,138.061127541206,12.5888945271764));
#82050=CARTESIAN_POINT('Ctrl Pts',(4.44293118427199,138.070854880423,12.5762217671127));
#82051=CARTESIAN_POINT('Ctrl Pts',(4.44349564910471,138.076039418751,12.5696148696357));
#82052=CARTESIAN_POINT('Ctrl Pts',(4.44508926513067,138.090993969594,12.5509716969043));
#82053=CARTESIAN_POINT('Ctrl Pts',(4.44610748031988,138.10093191704,12.5390716195291));
#82054=CARTESIAN_POINT('Ctrl Pts',(4.44846565436185,138.124767264935,12.5116494425902));
#82055=CARTESIAN_POINT('Ctrl Pts',(4.44979554667951,138.138847483882,12.4962927260749));
#82056=CARTESIAN_POINT('Ctrl Pts',(4.45499881528896,138.196104154233,12.4370786174421));
#82057=CARTESIAN_POINT('Ctrl Pts',(4.45876049827389,138.242283140347,12.3962590278988));
#82058=CARTESIAN_POINT('Ctrl Pts',(4.46618139536436,138.337889763152,12.324250936474));
#82059=CARTESIAN_POINT('Ctrl Pts',(4.46982493899011,138.386858839811,12.2927597084906));
#82060=CARTESIAN_POINT('Ctrl Pts',(4.47480937433507,138.454333158549,12.2561176562691));
#82061=CARTESIAN_POINT('Ctrl Pts',(4.47603184899913,138.470925040854,12.2476111583778));
#82062=CARTESIAN_POINT('Ctrl Pts',(4.47815216226197,138.499717156917,12.233702705061));
#82063=CARTESIAN_POINT('Ctrl Pts',(4.4790431412539,138.511820390467,12.228107520195));
#82064=CARTESIAN_POINT('Ctrl Pts',(4.48089399240221,138.536952672647,12.2170031039055));
#82065=CARTESIAN_POINT('Ctrl Pts',(4.48185460619846,138.549991150139,12.2115207356431));
#82066=CARTESIAN_POINT('Ctrl Pts',(4.48440903809402,138.584628060835,12.1976854423856));
#82067=CARTESIAN_POINT('Ctrl Pts',(4.48601578559118,138.606378616602,12.1897327766417));
#82068=CARTESIAN_POINT('Ctrl Pts',(4.4931325853762,138.702505440369,12.1577655545326));
#82069=CARTESIAN_POINT('Ctrl Pts',(4.49884882926304,138.77892303634,12.140550100256));
#82070=CARTESIAN_POINT('Ctrl Pts',(4.50860860000882,138.91080441141,12.1243571727766));
#82071=CARTESIAN_POINT('Ctrl Pts',(4.51262373042449,138.965543450837,12.1214815909853));
#82072=CARTESIAN_POINT('Ctrl Pts',(4.51752718940067,139.034780684684,12.1226744405384));
#82073=CARTESIAN_POINT('Ctrl Pts',(4.51854330849807,139.049268575211,12.1231916792009));
#82074=CARTESIAN_POINT('Ctrl Pts',(4.52011336535685,139.071928489867,12.1244199145468));
#82075=CARTESIAN_POINT('Ctrl Pts',(4.52067620589444,139.08010842505,12.12494898181));
#82076=CARTESIAN_POINT('Ctrl Pts',(4.52176430268376,139.096045946824,12.1261470063593));
#82077=CARTESIAN_POINT('Ctrl Pts',(4.52228992609296,139.103803579192,12.1268075620268));
#82078=CARTESIAN_POINT('Ctrl Pts',(4.5236467585367,139.123964052179,12.1287257481483));
#82079=CARTESIAN_POINT('Ctrl Pts',(4.52447167108756,139.136354925762,12.1301034983764));
#82080=CARTESIAN_POINT('Ctrl Pts',(4.52630140630557,139.164072242667,12.1336317889699));
#82081=CARTESIAN_POINT('Ctrl Pts',(4.52730145025654,139.17938304448,12.1358882036811));
#82082=CARTESIAN_POINT('Ctrl Pts',(4.53052638323222,139.229093759829,12.1442184000523));
#82083=CARTESIAN_POINT('Ctrl Pts',(4.532709368715,139.263270248595,12.1515209462001));
#82084=CARTESIAN_POINT('Ctrl Pts',(4.54072345642699,139.388240783638,12.1840966097589));
#82085=CARTESIAN_POINT('Ctrl Pts',(4.54645924088612,139.476218579563,12.2187111005218));
#82086=CARTESIAN_POINT('Ctrl Pts',(4.55381453348094,139.576097718916,12.272586698782));
#82087=CARTESIAN_POINT('Ctrl Pts',(4.55507685762903,139.592835939148,12.2821531778624));
#82088=CARTESIAN_POINT('Ctrl Pts',(4.5572350369178,139.620714909347,12.2990079817026));
#82089=CARTESIAN_POINT('Ctrl Pts',(4.558123062895,139.631980867963,12.3060824092028));
#82090=CARTESIAN_POINT('Ctrl Pts',(4.55995520291427,139.654789228345,12.3209494316444));
#82091=CARTESIAN_POINT('Ctrl Pts',(4.56089984990756,139.666318031238,12.3287589376558));
#82092=CARTESIAN_POINT('Ctrl Pts',(4.56335644337155,139.695690389042,12.3494246312138));
#82093=CARTESIAN_POINT('Ctrl Pts',(4.56487953888226,139.713316464095,12.3625789854718));
#82094=CARTESIAN_POINT('Ctrl Pts',(4.56830469299409,139.751646645332,12.3928920044727));
#82095=CARTESIAN_POINT('Ctrl Pts',(4.57021475860546,139.772151814534,12.4102815121178));
#82096=CARTESIAN_POINT('Ctrl Pts',(4.57696380766331,139.841659938885,12.473441964599));
#82097=CARTESIAN_POINT('Ctrl Pts',(4.58191072974019,139.887333722784,12.5226794632737));
#82098=CARTESIAN_POINT('Ctrl Pts',(4.59019301095787,139.956868001116,12.6118027880748));
#82099=CARTESIAN_POINT('Ctrl Pts',(4.59353759076802,139.98302189817,12.6497073321664));
#82100=CARTESIAN_POINT('Ctrl Pts',(4.59761241334511,140.013083434356,12.69925094068));
#82101=CARTESIAN_POINT('Ctrl Pts',(4.59844390567549,140.019118895127,12.709547476215));
#82102=CARTESIAN_POINT('Ctrl Pts',(4.59979041105337,140.028745040424,12.7265572283095));
#82103=CARTESIAN_POINT('Ctrl Pts',(4.60031087778232,140.032428901258,12.7332164897527));
#82104=CARTESIAN_POINT('Ctrl Pts',(4.60139239095569,140.040010484408,12.7472408522745));
#82105=CARTESIAN_POINT('Ctrl Pts',(4.60195266030373,140.043895048661,12.7546124121708));
#82106=CARTESIAN_POINT('Ctrl Pts',(4.60352044291731,140.054630357284,12.7755193180085));
#82107=CARTESIAN_POINT('Ctrl Pts',(4.60451757337406,140.061298553084,12.789147173642));
#82108=CARTESIAN_POINT('Ctrl Pts',(4.60681617704818,140.076233332756,12.8212250652354));
#82109=CARTESIAN_POINT('Ctrl Pts',(4.60810828263103,140.084292041307,12.8397669248675));
#82110=CARTESIAN_POINT('Ctrl Pts',(4.61303441236683,140.113487929548,12.9119723362309));
#82111=CARTESIAN_POINT('Ctrl Pts',(4.61656813258606,140.131150968644,12.9669549354017));
#82112=CARTESIAN_POINT('Ctrl Pts',(4.62369915489038,140.158243925247,13.0789229725753));
#82113=CARTESIAN_POINT('Ctrl Pts',(4.62728745852814,140.167657048175,13.1357437981369));
#82114=CARTESIAN_POINT('Ctrl Pts',(4.63236949198691,140.174811387542,13.2141818495386));
#82115=CARTESIAN_POINT('Ctrl Pts',(4.63375564769825,140.176168330469,13.235389481568));
#82116=CARTESIAN_POINT('Ctrl Pts',(4.63607036238583,140.177458633001,13.2703978877468));
#82117=CARTESIAN_POINT('Ctrl Pts',(4.63698848541258,140.177724449237,13.2841819109652));
#82118=CARTESIAN_POINT('Ctrl Pts',(4.63882469534848,140.177771649256,13.3115248904123));
#82119=CARTESIAN_POINT('Ctrl Pts',(4.63974239199469,140.177560937698,13.3250817097173));
#82120=CARTESIAN_POINT('Ctrl Pts',(4.64203131354055,140.176460626093,13.3586087089169));
#82121=CARTESIAN_POINT('Ctrl Pts',(4.64341083814956,140.175296578742,13.3785649559327));
#82122=CARTESIAN_POINT('Ctrl Pts',(4.64645058016099,140.171654284553,13.4219712288838));
#82123=CARTESIAN_POINT('Ctrl Pts',(4.64811609531217,140.168978497663,13.445395622061));
#82124=CARTESIAN_POINT('Ctrl Pts',(4.65344504089559,140.158288955321,13.5192431442962));
#82125=CARTESIAN_POINT('Ctrl Pts',(4.65717143103521,140.147699848218,13.5692305437004));
#82126=CARTESIAN_POINT('Ctrl Pts',(4.66574541046944,140.116130651548,13.6816673058308));
#82127=CARTESIAN_POINT('Ctrl Pts',(4.67059451055174,140.093087961002,13.7433706977481));
#82128=CARTESIAN_POINT('Ctrl Pts',(4.67622267179672,140.059099350073,13.8153596334413));
#82129=CARTESIAN_POINT('Ctrl Pts',(4.67719247943068,140.052963739254,13.8277825223399));
#82130=CARTESIAN_POINT('Ctrl Pts',(4.67870770080726,140.042911202402,13.8472625908496));
#82131=CARTESIAN_POINT('Ctrl Pts',(4.67926108265696,140.039138703909,13.854392354927));
#82132=CARTESIAN_POINT('Ctrl Pts',(4.68034622370873,140.031533877106,13.8684145496831));
#82133=CARTESIAN_POINT('Ctrl Pts',(4.68087812532943,140.027705017169,13.8753083040336));
#82134=CARTESIAN_POINT('Ctrl Pts',(4.68227426409516,140.017395059978,13.8934396559565));
#82135=CARTESIAN_POINT('Ctrl Pts',(4.68313148917211,140.010796828725,13.9046099063863));
#82136=CARTESIAN_POINT('Ctrl Pts',(4.68774662151028,139.97389519895,13.9647879669938));
#82137=CARTESIAN_POINT('Ctrl Pts',(4.69133062532774,139.940207737117,14.0116360525169));
#82138=CARTESIAN_POINT('Ctrl Pts',(4.70001614916104,139.85012668372,14.1192829645026));
#82139=CARTESIAN_POINT('Ctrl Pts',(4.70508789445232,139.790499139157,14.1769547209795));
#82140=CARTESIAN_POINT('Ctrl Pts',(4.71177352565144,139.708945158725,14.2407039839293));
#82141=CARTESIAN_POINT('Ctrl Pts',(4.71313081911521,139.692231536635,14.2530701117452));
#82142=CARTESIAN_POINT('Ctrl Pts',(4.71541086370179,139.663973860387,14.272841975089));
#82143=CARTESIAN_POINT('Ctrl Pts',(4.7163238406002,139.652611701981,14.2805002475559));
#82144=CARTESIAN_POINT('Ctrl Pts',(4.71816021423738,139.629683740871,14.2953789623037));
#82145=CARTESIAN_POINT('Ctrl Pts',(4.71908339302365,139.618121027329,14.3026002496012));
#82146=CARTESIAN_POINT('Ctrl Pts',(4.7214070166361,139.588944843933,14.3201251657542));
#82147=CARTESIAN_POINT('Ctrl Pts',(4.72281633185988,139.571184650181,14.3301744453635));
#82148=CARTESIAN_POINT('Ctrl Pts',(4.72593503232002,139.531768091603,14.3511449146905));
#82149=CARTESIAN_POINT('Ctrl Pts',(4.72765022542898,139.510017646029,14.3618685404456));
#82150=CARTESIAN_POINT('Ctrl Pts',(4.7332399845748,139.438878371924,14.3942523548073));
#82151=CARTESIAN_POINT('Ctrl Pts',(4.7371847574608,139.388331487331,14.4131936820384));
#82152=CARTESIAN_POINT('Ctrl Pts',(4.74561494293015,139.278345973876,14.446003020223));
#82153=CARTESIAN_POINT('Ctrl Pts',(4.75009272050613,139.218756826673,14.4588554843534));
#82154=CARTESIAN_POINT('Ctrl Pts',(4.75539634104214,139.144466347125,14.4689411098155));
#82155=CARTESIAN_POINT('Ctrl Pts',(4.75638385783457,139.130461806291,14.4705868634003));
#82156=CARTESIAN_POINT('Ctrl Pts',(4.75792006975012,139.10835411962,14.4727831497456));
#82157=CARTESIAN_POINT('Ctrl Pts',(4.75847708591668,139.100269516016,14.4735020092046));
#82158=CARTESIAN_POINT('Ctrl Pts',(4.75956319476192,139.084357557645,14.4747512070803));
#82159=CARTESIAN_POINT('Ctrl Pts',(4.76009251770535,139.076531162586,14.4752870217027));
#82160=CARTESIAN_POINT('Ctrl Pts',(4.76147271160568,139.055954446016,14.4764893373811));
#82161=CARTESIAN_POINT('Ctrl Pts',(4.76231686259653,139.043197181486,14.4770268041078));
#82162=CARTESIAN_POINT('Ctrl Pts',(4.76708106937081,138.970397808263,14.4789085684375));
#82163=CARTESIAN_POINT('Ctrl Pts',(4.77080996691682,138.910324180704,14.4758663584762));
#82164=CARTESIAN_POINT('Ctrl Pts',(4.7794828824598,138.771227878268,14.4580947938973));
#82165=CARTESIAN_POINT('Ctrl Pts',(4.78440450500348,138.692969663893,14.4398469853316));
#82166=CARTESIAN_POINT('Ctrl Pts',(4.79093658881197,138.597271989458,14.4069544203392));
#82167=CARTESIAN_POINT('Ctrl Pts',(4.79230996391295,138.577558127979,14.399582064135));
#82168=CARTESIAN_POINT('Ctrl Pts',(4.79460931270489,138.545309446201,14.3865268445546));
#82169=CARTESIAN_POINT('Ctrl Pts',(4.79552514522176,138.532657413872,14.3811452094138));
#82170=CARTESIAN_POINT('Ctrl Pts',(4.7973613343609,138.507692682811,14.3700061887944));
#82171=CARTESIAN_POINT('Ctrl Pts',(4.79828137594904,138.495379685096,14.3642546920139));
#82172=CARTESIAN_POINT('Ctrl Pts',(4.80058519922273,138.465048114944,14.3494418718262));
#82173=CARTESIAN_POINT('Ctrl Pts',(4.80197752457061,138.447158170469,14.3401286390274));
#82174=CARTESIAN_POINT('Ctrl Pts',(4.80839431260371,138.366747332532,14.295607347492));
#82175=CARTESIAN_POINT('Ctrl Pts',(4.81359856872788,138.307294340155,14.2551956895674));
#82176=CARTESIAN_POINT('Ctrl Pts',(4.82389289207144,138.198952880956,14.1660931398391));
#82177=CARTESIAN_POINT('Ctrl Pts',(4.82895578127485,138.149908999472,14.1180100622798));
#82178=CARTESIAN_POINT('Ctrl Pts',(4.8347690927021,138.096412414699,14.0555212151996));
#82179=CARTESIAN_POINT('Ctrl Pts',(4.83572802351223,138.087682832753,14.0449565477353));
#82180=CARTESIAN_POINT('Ctrl Pts',(4.83723034029155,138.074130023621,14.0279590704146));
#82181=CARTESIAN_POINT('Ctrl Pts',(4.83778148033555,138.069185109359,14.0216254363205));
#82182=CARTESIAN_POINT('Ctrl Pts',(4.83886614018695,138.05950013888,14.0089553425991));
#82183=CARTESIAN_POINT('Ctrl Pts',(4.8393997471927,138.054758377273,14.002620771819));
#82184=CARTESIAN_POINT('Ctrl Pts',(4.84080630864375,138.04233319953,13.9856683723449));
#82185=CARTESIAN_POINT('Ctrl Pts',(4.84167205862026,138.034762301955,13.9749689173073));
#82186=CARTESIAN_POINT('Ctrl Pts',(4.84613570953641,137.996245534011,13.9185617610804));
#82187=CARTESIAN_POINT('Ctrl Pts',(4.84957558321192,137.968359073284,13.8708415493272));
#82188=CARTESIAN_POINT('Ctrl Pts',(4.85609982431312,137.921714791742,13.7763534625273));
#82189=CARTESIAN_POINT('Ctrl Pts',(4.85917930024266,137.902422683108,13.7300326109271));
#82190=CARTESIAN_POINT('Ctrl Pts',(4.86231567683356,137.88614821265,13.6826607614027));
#82191=CARTESIAN_POINT('Origin',(1.13913288526384,139.,13.3));
#82192=CARTESIAN_POINT('',(5.46043320712868,137.886148212654,13.6826607614143));
#82193=CARTESIAN_POINT('',(5.36197089565136,137.88614821265,13.6826607614027));
#82194=CARTESIAN_POINT('',(1.13913288526384,137.88614821265,13.6826607614027));
#82195=CARTESIAN_POINT('Ctrl Pts',(5.46043320712869,137.886148212658,13.6826607614259));
#82196=CARTESIAN_POINT('Ctrl Pts',(5.46002446106101,137.88816324508,13.6885261327719));
#82197=CARTESIAN_POINT('Ctrl Pts',(5.45961795346396,137.890224662102,13.6943757490642));
#82198=CARTESIAN_POINT('Ctrl Pts',(5.45489137935915,137.914852864487,13.7625397852664));
#82199=CARTESIAN_POINT('Ctrl Pts',(5.45080521369556,137.942597297947,13.8228661278637));
#82200=CARTESIAN_POINT('Ctrl Pts',(5.44214953865667,138.011644698042,13.9447428096011));
#82201=CARTESIAN_POINT('Ctrl Pts',(5.43759116393617,138.053964360087,14.0053754723978));
#82202=CARTESIAN_POINT('Ctrl Pts',(5.43151568350696,138.114716689762,14.0770297290376));
#82203=CARTESIAN_POINT('Ctrl Pts',(5.43019758881392,138.128150371337,14.0920731568807));
#82204=CARTESIAN_POINT('Ctrl Pts',(5.42796853572488,138.151229936349,14.1166195299311));
#82205=CARTESIAN_POINT('Ctrl Pts',(5.42706653844709,138.160665667421,14.1263146676485));
#82206=CARTESIAN_POINT('Ctrl Pts',(5.42524078930307,138.179941204172,14.1454492829544));
#82207=CARTESIAN_POINT('Ctrl Pts',(5.42431706408592,138.189782089481,14.154884687505));
#82208=CARTESIAN_POINT('Ctrl Pts',(5.4219690256319,138.215003859897,14.1782405098876));
#82209=CARTESIAN_POINT('Ctrl Pts',(5.42053530355722,138.230592306832,14.1919288311764));
#82210=CARTESIAN_POINT('Ctrl Pts',(5.41330437062935,138.31008937633,14.2581004539301));
#82211=CARTESIAN_POINT('Ctrl Pts',(5.40726178334422,138.379030729362,14.3041543804792));
#82212=CARTESIAN_POINT('Ctrl Pts',(5.39822406142292,138.487953202648,14.36138270757));
#82213=CARTESIAN_POINT('Ctrl Pts',(5.39526166879702,138.524638566486,14.3783120996047));
#82214=CARTESIAN_POINT('Ctrl Pts',(5.39114456469103,138.577701543385,14.399563874362));
#82215=CARTESIAN_POINT('Ctrl Pts',(5.38994572947525,138.593413005586,14.405469933359));
#82216=CARTESIAN_POINT('Ctrl Pts',(5.38782761132128,138.621721748052,14.4154261609528));
#82217=CARTESIAN_POINT('Ctrl Pts',(5.38690309948158,138.634271093557,14.4196036621991));
#82218=CARTESIAN_POINT('Ctrl Pts',(5.38544377375865,138.654430520457,14.42593929359));
#82219=CARTESIAN_POINT('Ctrl Pts',(5.38490184316546,138.661996217212,14.428233579714));
#82220=CARTESIAN_POINT('Ctrl Pts',(5.38382515754415,138.677198661235,14.4326770425865));
#82221=CARTESIAN_POINT('Ctrl Pts',(5.3832904565881,138.684835163802,14.4348255911629));
#82222=CARTESIAN_POINT('Ctrl Pts',(5.3818664506311,138.705386448751,14.4403842856765));
#82223=CARTESIAN_POINT('Ctrl Pts',(5.38098474433417,138.718338897941,14.4436522743087));
#82224=CARTESIAN_POINT('Ctrl Pts',(5.37539625060192,138.801670046327,14.4631755655884));
#82225=CARTESIAN_POINT('Ctrl Pts',(5.37096328308412,138.873371013347,14.4731495620282));
#82226=CARTESIAN_POINT('Ctrl Pts',(5.36226309479941,139.013993082003,14.4796588156711));
#82227=CARTESIAN_POINT('Ctrl Pts',(5.35801364830462,139.08258331411,14.4768472077239));
#82228=CARTESIAN_POINT('Ctrl Pts',(5.35227702900749,139.17056402731,14.4655087941148));
#82229=CARTESIAN_POINT('Ctrl Pts',(5.3509572262854,139.190521077112,14.4624132127218));
#82230=CARTESIAN_POINT('Ctrl Pts',(5.34872614789819,139.223703056358,14.4563888385664));
#82231=CARTESIAN_POINT('Ctrl Pts',(5.34782387136277,139.236975189682,14.4537421449516));
#82232=CARTESIAN_POINT('Ctrl Pts',(5.34599825365736,139.263514417396,14.4479725229121));
#82233=CARTESIAN_POINT('Ctrl Pts',(5.34507495036747,139.276778758361,14.4448468252501));
#82234=CARTESIAN_POINT('Ctrl Pts',(5.34272945845369,139.310060455339,14.4363919186335));
#82235=CARTESIAN_POINT('Ctrl Pts',(5.34129790299485,139.329996284705,14.4307636517813));
#82236=CARTESIAN_POINT('Ctrl Pts',(5.33404962410678,139.429006375878,14.3999699582176));
#82237=CARTESIAN_POINT('Ctrl Pts',(5.32798546452156,139.505402157916,14.3670261015879));
#82238=CARTESIAN_POINT('Ctrl Pts',(5.31773151608493,139.627055005208,14.298552000968));
#82239=CARTESIAN_POINT('Ctrl Pts',(5.31357696525345,139.674355879607,14.2672380012395));
#82240=CARTESIAN_POINT('Ctrl Pts',(5.3086305678388,139.729824927433,14.224461954189));
#82241=CARTESIAN_POINT('Ctrl Pts',(5.30769420943759,139.740287853526,14.2161049402823));
#82242=CARTESIAN_POINT('Ctrl Pts',(5.3062208159242,139.756724393485,14.2025110993704));
#82243=CARTESIAN_POINT('Ctrl Pts',(5.30567643815709,139.762791170154,14.1973893983234));
#82244=CARTESIAN_POINT('Ctrl Pts',(5.30459952369469,139.774789452427,14.1870505924745));
#82245=CARTESIAN_POINT('Ctrl Pts',(5.30406697676924,139.780721181815,14.1818343915343));
#82246=CARTESIAN_POINT('Ctrl Pts',(5.30265585783676,139.796418659861,14.1677478976448));
#82247=CARTESIAN_POINT('Ctrl Pts',(5.30178464546688,139.806088913321,14.1587722606016));
#82248=CARTESIAN_POINT('Ctrl Pts',(5.29610633496943,139.868792904912,14.0985796278385));
#82249=CARTESIAN_POINT('Ctrl Pts',(5.29158645602547,139.917074461824,14.0426356746975));
#82250=CARTESIAN_POINT('Ctrl Pts',(5.28413421484998,139.98694569906,13.944379941946));
#82251=CARTESIAN_POINT('Ctrl Pts',(5.28123303980634,140.011779282716,13.9046400816903));
#82252=CARTESIAN_POINT('Ctrl Pts',(5.27684118012883,140.044936647546,13.8437902210852));
#82253=CARTESIAN_POINT('Ctrl Pts',(5.27540258427144,140.055124874687,13.8237478491097));
#82254=CARTESIAN_POINT('Ctrl Pts',(5.27269643377183,140.072973752593,13.7859980168318));
#82255=CARTESIAN_POINT('Ctrl Pts',(5.27143412006633,140.080784959081,13.7683700985155));
#82256=CARTESIAN_POINT('Ctrl Pts',(5.26927137251866,140.093275667117,13.7382033973851));
#82257=CARTESIAN_POINT('Ctrl Pts',(5.26837869667091,140.098180658948,13.7257618079418));
#82258=CARTESIAN_POINT('Ctrl Pts',(5.2666585518942,140.107149749537,13.701824705116));
#82259=CARTESIAN_POINT('Ctrl Pts',(5.26583240325275,140.111249295488,13.690344265179));
#82260=CARTESIAN_POINT('Ctrl Pts',(5.26361867636485,140.1216796052,13.6596381261013));
#82261=CARTESIAN_POINT('Ctrl Pts',(5.26222098908987,140.127693956648,13.6403101089013));
#82262=CARTESIAN_POINT('Ctrl Pts',(5.25473715352687,140.156889013847,13.5371924231291));
#82263=CARTESIAN_POINT('Ctrl Pts',(5.24837389754839,140.171233318188,13.4511951666371));
#82264=CARTESIAN_POINT('Ctrl Pts',(5.23918242482233,140.178079517161,13.3262192177704));
#82265=CARTESIAN_POINT('Ctrl Pts',(5.23637918385243,140.178309618161,13.287936508896));
#82266=CARTESIAN_POINT('Ctrl Pts',(5.23245462858375,140.175980543361,13.2334424843269));
#82267=CARTESIAN_POINT('Ctrl Pts',(5.23129275563309,140.174948055718,13.2171914202445));
#82268=CARTESIAN_POINT('Ctrl Pts',(5.22923237313752,140.172491529246,13.1880808747246));
#82269=CARTESIAN_POINT('Ctrl Pts',(5.22832901591736,140.171191988838,13.1752136352076));
#82270=CARTESIAN_POINT('Ctrl Pts',(5.2268948228637,140.168763938468,13.1545783176251));
#82271=CARTESIAN_POINT('Ctrl Pts',(5.22635726625967,140.167769292725,13.146795890166));
#82272=CARTESIAN_POINT('Ctrl Pts',(5.22528072541546,140.165603837945,13.1311014771666));
#82273=CARTESIAN_POINT('Ctrl Pts',(5.22474191885508,140.164430065478,13.1231903563779));
#82274=CARTESIAN_POINT('Ctrl Pts',(5.22329330009636,140.161031692572,13.1017895798923));
#82275=CARTESIAN_POINT('Ctrl Pts',(5.22239154968564,140.158652585027,13.0883252760078));
#82276=CARTESIAN_POINT('Ctrl Pts',(5.21703254643454,140.142951649458,13.007688742377));
#82277=CARTESIAN_POINT('Ctrl Pts',(5.2128179361966,140.124024881949,12.9417337691464));
#82278=CARTESIAN_POINT('Ctrl Pts',(5.20402911219146,140.073036587565,12.8089555546234));
#82279=CARTESIAN_POINT('Ctrl Pts',(5.19946635320272,140.040200148925,12.7427619809579));
#82280=CARTESIAN_POINT('Ctrl Pts',(5.19343985944495,139.991255398892,12.6636991460309));
#82281=CARTESIAN_POINT('Ctrl Pts',(5.19217869330606,139.980717500391,12.6475744042077));
#82282=CARTESIAN_POINT('Ctrl Pts',(5.19001729450854,139.962202929968,12.6207067323857));
#82283=CARTESIAN_POINT('Ctrl Pts',(5.18912479540248,139.954429773761,12.609827844783));
#82284=CARTESIAN_POINT('Ctrl Pts',(5.18740457711586,139.939216574442,12.5892848864221));
#82285=CARTESIAN_POINT('Ctrl Pts',(5.18657817167717,139.931808286969,12.579599386985));
#82286=CARTESIAN_POINT('Ctrl Pts',(5.1843627215402,139.911693527125,12.5541310590791));
#82287=CARTESIAN_POINT('Ctrl Pts',(5.18296353854975,139.898728391906,12.5385587656547));
#82288=CARTESIAN_POINT('Ctrl Pts',(5.17548930001018,139.828148157338,12.4581005444611));
#82289=CARTESIAN_POINT('Ctrl Pts',(5.1691384084212,139.763903116814,12.3994051145462));
#82290=CARTESIAN_POINT('Ctrl Pts',(5.15995310227539,139.662832474261,12.325721871847));
#82291=CARTESIAN_POINT('Ctrl Pts',(5.15714400860173,139.630768346918,12.3046626998926));
#82292=CARTESIAN_POINT('Ctrl Pts',(5.15321234242267,139.583687971997,12.2769315243276));
#82293=CARTESIAN_POINT('Ctrl Pts',(5.15204908140638,139.569472242263,12.2689509355662));
#82294=CARTESIAN_POINT('Ctrl Pts',(5.14998652473619,139.543680150179,12.2551677366288));
#82295=CARTESIAN_POINT('Ctrl Pts',(5.14908236737525,139.532165184006,12.2492560654022));
#82296=CARTESIAN_POINT('Ctrl Pts',(5.14764722153498,139.513515163085,12.2400665949988));
#82297=CARTESIAN_POINT('Ctrl Pts',(5.14710949749855,139.506441005316,12.2366683656637));
#82298=CARTESIAN_POINT('Ctrl Pts',(5.14603295479684,139.492092509752,12.2299514312896));
#82299=CARTESIAN_POINT('Ctrl Pts',(5.14549430901002,139.484817326175,12.2266355944024));
#82300=CARTESIAN_POINT('Ctrl Pts',(5.1440466535762,139.465022873531,12.2178561312979));
#82301=CARTESIAN_POINT('Ctrl Pts',(5.14314568740958,139.452441012194,12.2125356117842));
#82302=CARTESIAN_POINT('Ctrl Pts',(5.13777132229715,139.376016312284,12.1817738775187));
#82303=CARTESIAN_POINT('Ctrl Pts',(5.13354246770266,139.310132088449,12.1617389053632));
#82304=CARTESIAN_POINT('Ctrl Pts',(5.12624270275035,139.194537873567,12.137378054485));
#82305=CARTESIAN_POINT('Ctrl Pts',(5.1231891490699,139.14561508974,12.1302433457637));
#82306=CARTESIAN_POINT('Ctrl Pts',(5.11859910323767,139.073335254997,12.1243077918332));
#82307=CARTESIAN_POINT('Ctrl Pts',(5.117120571124,139.050229598418,12.1230942614668));
#82308=CARTESIAN_POINT('Ctrl Pts',(5.11434817995884,139.007420022483,12.1221088004746));
#82309=CARTESIAN_POINT('Ctrl Pts',(5.1130600619896,138.987728580659,12.1221493840044));
#82310=CARTESIAN_POINT('Ctrl Pts',(5.11086673756029,138.954609548468,12.1230482157722));
#82311=CARTESIAN_POINT('Ctrl Pts',(5.10996983981387,138.941178525143,12.1236429945711));
#82312=CARTESIAN_POINT('Ctrl Pts',(5.10814203211504,138.914053806901,12.1253098649754));
#82313=CARTESIAN_POINT('Ctrl Pts',(5.10721094914297,138.900362844717,12.1263918580319));
#82314=CARTESIAN_POINT('Ctrl Pts',(5.10481735263694,138.865506493577,12.1297608443803));
#82315=CARTESIAN_POINT('Ctrl Pts',(5.10334465581804,138.844379268575,12.1323826525394));
#82316=CARTESIAN_POINT('Ctrl Pts',(5.09653517714688,138.748189667766,12.146976345681));
#82317=CARTESIAN_POINT('Ctrl Pts',(5.09099781490139,138.674334791385,12.1656231760198));
#82318=CARTESIAN_POINT('Ctrl Pts',(5.0807052314438,138.542410946377,12.2128833947779));
#82319=CARTESIAN_POINT('Ctrl Pts',(5.07598418768399,138.483882653435,12.2394178119525));
#82320=CARTESIAN_POINT('Ctrl Pts',(5.07058511479857,138.41688720055,12.2766571974022));
#82321=CARTESIAN_POINT('Ctrl Pts',(5.06971362324848,138.406068165333,12.28289821751));
#82322=CARTESIAN_POINT('Ctrl Pts',(5.06831714345676,138.388693213285,12.2932928696371));
#82323=CARTESIAN_POINT('Ctrl Pts',(5.06778602303979,138.382075689661,12.2973411384468));
#82324=CARTESIAN_POINT('Ctrl Pts',(5.06670867198228,138.3686239485,12.3057540118932));
#82325=CARTESIAN_POINT('Ctrl Pts',(5.0661628204404,138.361793916912,12.310124346928));
#82326=CARTESIAN_POINT('Ctrl Pts',(5.06467182065119,138.343117147358,12.3223487380023));
#82327=CARTESIAN_POINT('Ctrl Pts',(5.06373555662262,138.331366201462,12.3303475056441));
#82328=CARTESIAN_POINT('Ctrl Pts',(5.05957846210499,138.279261701283,12.3672123663483));
#82329=CARTESIAN_POINT('Ctrl Pts',(5.05647780331447,138.240607803186,12.3984008790417));
#82330=CARTESIAN_POINT('Ctrl Pts',(5.05060708043993,138.170805706264,12.4624056776712));
#82331=CARTESIAN_POINT('Ctrl Pts',(5.04783747499948,138.139355236226,12.494755946986));
#82332=CARTESIAN_POINT('Ctrl Pts',(5.04292485313103,138.087712923279,12.5543667268897));
#82333=CARTESIAN_POINT('Ctrl Pts',(5.04080139912755,138.066699627232,12.580842943958));
#82334=CARTESIAN_POINT('Ctrl Pts',(5.03698922707229,138.031690088361,12.6290771750032));
#82335=CARTESIAN_POINT('Ctrl Pts',(5.03531732380184,138.01721773161,12.6504614092324));
#82336=CARTESIAN_POINT('Ctrl Pts',(5.03266041366201,137.995687870691,12.6846424682279));
#82337=CARTESIAN_POINT('Ctrl Pts',(5.03169328023659,137.988145504196,12.697125060604));
#82338=CARTESIAN_POINT('Ctrl Pts',(5.0298432118675,137.97428657834,12.7210545138869));
#82339=CARTESIAN_POINT('Ctrl Pts',(5.02896208102689,137.967925001276,12.7324728443154));
#82340=CARTESIAN_POINT('Ctrl Pts',(5.02692405597387,137.953764085184,12.7589159192927));
#82341=CARTESIAN_POINT('Ctrl Pts',(5.02576274515258,137.946096181072,12.7740073572942));
#82342=CARTESIAN_POINT('Ctrl Pts',(5.02180595820455,137.921326529643,12.8254749058475));
#82343=CARTESIAN_POINT('Ctrl Pts',(5.01896016010826,137.905763816309,12.862556216599));
#82344=CARTESIAN_POINT('Ctrl Pts',(5.01519767867307,137.888031356643,12.9117133153927));
#82345=CARTESIAN_POINT('Ctrl Pts',(5.01432451051326,137.884109697194,12.9231318098902));
#82346=CARTESIAN_POINT('Ctrl Pts',(5.008428959518,137.858915564422,13.00033184331));
#82347=CARTESIAN_POINT('Ctrl Pts',(5.00330320730206,137.843296298042,13.0678131511312));
#82348=CARTESIAN_POINT('Ctrl Pts',(4.996691753016,137.830643370314,13.1579467092443));
#82349=CARTESIAN_POINT('Ctrl Pts',(4.99511456189243,137.828205392505,13.1797021648625));
#82350=CARTESIAN_POINT('Ctrl Pts',(4.99241906058703,137.82503353028,13.2175002153568));
#82351=CARTESIAN_POINT('Ctrl Pts',(4.99129097947808,137.824018718384,13.2335131066865));
#82352=CARTESIAN_POINT('Ctrl Pts',(4.9895913875169,137.822968395752,13.2580067050428));
#82353=CARTESIAN_POINT('Ctrl Pts',(4.9890085287092,137.822696766944,13.2664747451221));
#82354=CARTESIAN_POINT('Ctrl Pts',(4.98792111465327,137.822357571273,13.2824157577345));
#82355=CARTESIAN_POINT('Ctrl Pts',(4.98741558349857,137.822269709671,13.289887550912));
#82356=CARTESIAN_POINT('Ctrl Pts',(4.98615363360918,137.822227583227,13.308679943909));
#82357=CARTESIAN_POINT('Ctrl Pts',(4.98540207172252,137.822365413987,13.3200003207807));
#82358=CARTESIAN_POINT('Ctrl Pts',(4.98228754559904,137.823625123722,13.3673572273729));
#82359=CARTESIAN_POINT('Ctrl Pts',(4.97999250369455,137.826238230008,13.4033375990253));
#82360=CARTESIAN_POINT('Ctrl Pts',(4.97249045344082,137.840368030264,13.5220976898578));
#82361=CARTESIAN_POINT('Ctrl Pts',(4.96743625790818,137.859030271177,13.6037256666642));
#82362=CARTESIAN_POINT('Ctrl Pts',(4.96216799084082,137.886148228708,13.6826608081431));
#82363=CARTESIAN_POINT('',(4.88847248670267,137.822250347659,13.2990950627804));
#82364=CARTESIAN_POINT('Ctrl Pts',(4.86231567683356,137.88614821265,13.6826607614027));
#82365=CARTESIAN_POINT('Ctrl Pts',(4.8645148585283,137.874736790429,13.6494443088179));
#82366=CARTESIAN_POINT('Ctrl Pts',(4.86674140775455,137.864808999366,13.6157110894406));
#82367=CARTESIAN_POINT('Ctrl Pts',(4.87034394071392,137.851480583466,13.5615755602647));
#82368=CARTESIAN_POINT('Ctrl Pts',(4.87168818012219,137.847085384947,13.5414672469751));
#82369=CARTESIAN_POINT('Ctrl Pts',(4.8739525826596,137.840652522983,13.5078345245234));
#82370=CARTESIAN_POINT('Ctrl Pts',(4.87486326623803,137.838319446138,13.494370847295));
#82371=CARTESIAN_POINT('Ctrl Pts',(4.87660826881864,137.83433165814,13.4687120827688));
#82372=CARTESIAN_POINT('Ctrl Pts',(4.87744106128916,137.832632809573,13.456525629891));
#82373=CARTESIAN_POINT('Ctrl Pts',(4.87919781499112,137.829475592632,13.4309538852708));
#82374=CARTESIAN_POINT('Ctrl Pts',(4.88012284173155,137.828055219537,13.417565784355));
#82375=CARTESIAN_POINT('Ctrl Pts',(4.88348366316469,137.823762478546,13.3692159067949));
#82376=CARTESIAN_POINT('Ctrl Pts',(4.88595853238333,137.822223399548,13.334167250912));
#82377=CARTESIAN_POINT('Ctrl Pts',(4.88847248670261,137.822250347659,13.2990950627804));
#82378=CARTESIAN_POINT('Ctrl Pts',(4.88847248670253,137.822250347659,13.2990950627817));
#82379=CARTESIAN_POINT('Ctrl Pts',(4.89548691716877,137.822325538226,13.2012367114737));
#82380=CARTESIAN_POINT('Ctrl Pts',(4.90280164485462,137.834594185474,13.1037919136678));
#82381=CARTESIAN_POINT('Ctrl Pts',(4.91101803388777,137.862807609492,12.9931524352178));
#82382=CARTESIAN_POINT('Ctrl Pts',(4.91218400364322,137.867173579335,12.9774068887808));
#82383=CARTESIAN_POINT('Ctrl Pts',(4.9142518460924,137.875593462271,12.9493242876122));
#82384=CARTESIAN_POINT('Ctrl Pts',(4.91515858947528,137.879526417949,12.936953853555));
#82385=CARTESIAN_POINT('Ctrl Pts',(4.91659894685295,137.886176724171,12.9171750130038));
#82386=CARTESIAN_POINT('Ctrl Pts',(4.91713931866423,137.8887653124,12.9097247885511));
#82387=CARTESIAN_POINT('Ctrl Pts',(4.91822312495569,137.894151730001,12.8947103552642));
#82388=CARTESIAN_POINT('Ctrl Pts',(4.91876635462145,137.896952783002,12.8871477999224));
#82389=CARTESIAN_POINT('Ctrl Pts',(4.92023079385646,137.904773381943,12.8666809331957));
#82390=CARTESIAN_POINT('Ctrl Pts',(4.92114370883561,137.909943313797,12.8538349850063));
#82391=CARTESIAN_POINT('Ctrl Pts',(4.92633665979877,137.940976276048,12.780487924144));
#82392=CARTESIAN_POINT('Ctrl Pts',(4.93039460301909,137.971649482345,12.7221407443561));
#82393=CARTESIAN_POINT('Ctrl Pts',(4.93867632660916,138.043721744807,12.6091454758047));
#82394=CARTESIAN_POINT('Ctrl Pts',(4.94288825183901,138.085327219999,12.5549358029972));
#82395=CARTESIAN_POINT('Ctrl Pts',(4.94876112406876,138.147036562156,12.4875436089103));
#82396=CARTESIAN_POINT('Ctrl Pts',(4.95026787409135,138.163185420687,12.4709202338304));
#82397=CARTESIAN_POINT('Ctrl Pts',(4.95272829058628,138.189965726914,12.4449329434705));
#82398=CARTESIAN_POINT('Ctrl Pts',(4.95366859643321,138.200294511792,12.4352651865165));
#82399=CARTESIAN_POINT('Ctrl Pts',(4.95551064907986,138.220690535582,12.4168524685625));
#82400=CARTESIAN_POINT('Ctrl Pts',(4.95641136289903,138.230737116543,12.4080877877379));
#82401=CARTESIAN_POINT('Ctrl Pts',(4.95858815728105,138.255177390207,12.3874861290406));
#82402=CARTESIAN_POINT('Ctrl Pts',(4.95987074853258,138.26970706829,12.3758168745592));
#82403=CARTESIAN_POINT('Ctrl Pts',(4.96518096151397,138.330349347986,12.3294362889367));
#82404=CARTESIAN_POINT('Ctrl Pts',(4.9693216187203,138.378700522267,12.2977968469521));
#82405=CARTESIAN_POINT('Ctrl Pts',(4.97804710156335,138.483309238536,12.2398316819389));
#82406=CARTESIAN_POINT('Ctrl Pts',(4.98262935600328,138.539729166617,12.2141469177833));
#82407=CARTESIAN_POINT('Ctrl Pts',(4.98863411312278,138.617535407589,12.1858850821486));
#82408=CARTESIAN_POINT('Ctrl Pts',(4.99013683475325,138.637352125695,12.1792779873097));
#82409=CARTESIAN_POINT('Ctrl Pts',(4.99272179291685,138.672193915788,12.1686824334877));
#82410=CARTESIAN_POINT('Ctrl Pts',(4.99381279315654,138.687141562379,12.1644578738543));
#82411=CARTESIAN_POINT('Ctrl Pts',(4.99547108090021,138.710299538721,12.1584049217417));
#82412=CARTESIAN_POINT('Ctrl Pts',(4.99604886287629,138.718452651805,12.1563668501076));
#82413=CARTESIAN_POINT('Ctrl Pts',(4.99713793574227,138.733995002267,12.1526579500413));
#82414=CARTESIAN_POINT('Ctrl Pts',(4.9976500276137,138.741379640292,12.1509708658229));
#82415=CARTESIAN_POINT('Ctrl Pts',(4.9989454030387,138.760240847919,12.1468529067516));
#82416=CARTESIAN_POINT('Ctrl Pts',(4.99972331713554,138.771738778229,12.1445219558062));
#82417=CARTESIAN_POINT('Ctrl Pts',(5.00319414739933,138.823703159234,12.1347933164909));
#82418=CARTESIAN_POINT('Ctrl Pts',(5.00579797082261,138.864509372924,12.1293462570487));
#82419=CARTESIAN_POINT('Ctrl Pts',(5.01279583783542,138.97622235101,12.1203556606684));
#82420=CARTESIAN_POINT('Ctrl Pts',(5.01711398169721,139.047292718552,12.1210641516306));
#82421=CARTESIAN_POINT('Ctrl Pts',(5.02329689418963,139.14526284541,12.1309183799633));
#82422=CARTESIAN_POINT('Ctrl Pts',(5.02504297554812,139.17255106472,12.1346334868185));
#82423=CARTESIAN_POINT('Ctrl Pts',(5.02825541464193,139.221732904367,12.1430945677038));
#82424=CARTESIAN_POINT('Ctrl Pts',(5.02971217104078,139.243669192754,12.1475153448818));
#82425=CARTESIAN_POINT('Ctrl Pts',(5.03211206445923,139.27910134506,12.1557127113435));
#82426=CARTESIAN_POINT('Ctrl Pts',(5.03304308536084,139.292679658213,12.1591101941476));
#82427=CARTESIAN_POINT('Ctrl Pts',(5.03487144783709,139.318997470438,12.1661960063663));
#82428=CARTESIAN_POINT('Ctrl Pts',(5.0357678511595,139.331741607803,12.1698591402838));
#82429=CARTESIAN_POINT('Ctrl Pts',(5.03796686386794,139.362603059582,12.1792968291271));
#82430=CARTESIAN_POINT('Ctrl Pts',(5.03927661799051,139.380647072588,12.18529631354));
#82431=CARTESIAN_POINT('Ctrl Pts',(5.04728537750681,139.488893427004,12.22422200111));
#82432=CARTESIAN_POINT('Ctrl Pts',(5.05433785458231,139.57492257982,12.267637470714));
#82433=CARTESIAN_POINT('Ctrl Pts',(5.06388572184568,139.683114468292,12.3399910098731));
#82434=CARTESIAN_POINT('Ctrl Pts',(5.06638171421552,139.710679569353,12.3602141536061));
#82435=CARTESIAN_POINT('Ctrl Pts',(5.06993176157421,139.749240021854,12.3911722778309));
#82436=CARTESIAN_POINT('Ctrl Pts',(5.07101955893555,139.76096592023,12.4009675463331));
#82437=CARTESIAN_POINT('Ctrl Pts',(5.07296449655076,139.78181860446,12.4190872997647));
#82438=CARTESIAN_POINT('Ctrl Pts',(5.07382573824142,139.791011291121,12.4273324322755));
#82439=CARTESIAN_POINT('Ctrl Pts',(5.0752123483365,139.805769389134,12.4409941743897));
#82440=CARTESIAN_POINT('Ctrl Pts',(5.07574363308372,139.811413736149,12.4463237858243));
#82441=CARTESIAN_POINT('Ctrl Pts',(5.07682923786249,139.822933510383,12.4574187024086));
#82442=CARTESIAN_POINT('Ctrl Pts',(5.07738305432876,139.828801935657,12.4631904833319));
#82443=CARTESIAN_POINT('Ctrl Pts',(5.07891143861902,139.844955927516,12.47941510213));
#82444=CARTESIAN_POINT('Ctrl Pts',(5.07987644302062,139.855107871583,12.4899995863565));
#82445=CARTESIAN_POINT('Ctrl Pts',(5.08454913630464,139.903852919213,12.5427597075515));
#82446=CARTESIAN_POINT('Ctrl Pts',(5.08809658011121,139.939541679852,12.5875213628603));
#82447=CARTESIAN_POINT('Ctrl Pts',(5.0950770509931,140.003304030637,12.6806629648027));
#82448=CARTESIAN_POINT('Ctrl Pts',(5.09850278284048,140.031466495772,12.7287961430419));
#82449=CARTESIAN_POINT('Ctrl Pts',(5.10357264011236,140.067024079663,12.8008386589504));
#82450=CARTESIAN_POINT('Ctrl Pts',(5.10514332159243,140.077234741274,12.8232740527716));
#82451=CARTESIAN_POINT('Ctrl Pts',(5.10806943810135,140.094693040769,12.8650648737518));
#82452=CARTESIAN_POINT('Ctrl Pts',(5.10941793304798,140.102149530959,12.8843225465763));
#82453=CARTESIAN_POINT('Ctrl Pts',(5.11168743209757,140.113696748738,12.9166442256051));
#82454=CARTESIAN_POINT('Ctrl Pts',(5.11259886091066,140.118072998512,12.9296017801158));
#82455=CARTESIAN_POINT('Ctrl Pts',(5.11443544278927,140.126366286183,12.9556447325436));
#82456=CARTESIAN_POINT('Ctrl Pts',(5.11536043223832,140.130283295829,12.9687278992948));
#82457=CARTESIAN_POINT('Ctrl Pts',(5.11769542107772,140.139519865744,13.0016521727685));
#82458=CARTESIAN_POINT('Ctrl Pts',(5.11911447977523,140.144549317113,13.0215691848301));
#82459=CARTESIAN_POINT('Ctrl Pts',(5.12648317879188,140.167686637851,13.1244589837867));
#82460=CARTESIAN_POINT('Ctrl Pts',(5.13269443692922,140.177299446669,13.2090708636872));
#82461=CARTESIAN_POINT('Ctrl Pts',(5.1418080795938,140.177935397526,13.3331563898544));
#82462=CARTESIAN_POINT('Ctrl Pts',(5.14468163177423,140.176179790566,13.3723363073986));
#82463=CARTESIAN_POINT('Ctrl Pts',(5.14869329247567,140.170910844511,13.4278126584891));
#82464=CARTESIAN_POINT('Ctrl Pts',(5.14987345516513,140.169001654566,13.4442340748865));
#82465=CARTESIAN_POINT('Ctrl Pts',(5.15196349165263,140.164961933777,13.4735804065548));
#82466=CARTESIAN_POINT('Ctrl Pts',(5.15287838148664,140.162960326218,13.4865201874951));
#82467=CARTESIAN_POINT('Ctrl Pts',(5.1543283981841,140.159403975766,13.5072197935339));
#82468=CARTESIAN_POINT('Ctrl Pts',(5.1548704356357,140.157986145424,13.5150016734491));
#82469=CARTESIAN_POINT('Ctrl Pts',(5.15595419496341,140.154969608166,13.5306618187313));
#82470=CARTESIAN_POINT('Ctrl Pts',(5.1564957613229,140.153368438275,13.5385391489142));
#82471=CARTESIAN_POINT('Ctrl Pts',(5.15795021078446,140.148816766828,13.5598139238433));
#82472=CARTESIAN_POINT('Ctrl Pts',(5.15885499084909,140.145712552598,13.5731776450399));
#82473=CARTESIAN_POINT('Ctrl Pts',(5.16420095360714,140.125776584273,13.6526735253499));
#82474=CARTESIAN_POINT('Ctrl Pts',(5.1684015065631,140.103454654598,13.7173027914359));
#82475=CARTESIAN_POINT('Ctrl Pts',(5.17709537390135,140.046156106398,13.8458022633954));
#82476=CARTESIAN_POINT('Ctrl Pts',(5.18157683249815,140.010616835694,13.9090934417462));
#82477=CARTESIAN_POINT('Ctrl Pts',(5.18755591983171,139.958151133315,13.9851571965144));
#82478=CARTESIAN_POINT('Ctrl Pts',(5.18886197794427,139.94639490831,14.0013063377811));
#82479=CARTESIAN_POINT('Ctrl Pts',(5.19108079996645,139.925980315064,14.027900586971));
#82480=CARTESIAN_POINT('Ctrl Pts',(5.19198493013701,139.917541601826,14.0385094388955));
#82481=CARTESIAN_POINT('Ctrl Pts',(5.19382371495782,139.900152883245,14.0596117391659));
#82482=CARTESIAN_POINT('Ctrl Pts',(5.1947584816693,139.891197933404,14.0700983202328));
#82483=CARTESIAN_POINT('Ctrl Pts',(5.19715427000131,139.867969545495,14.0963517898346));
#82484=CARTESIAN_POINT('Ctrl Pts',(5.19862537963258,139.853449903096,14.1118931369253));
#82485=CARTESIAN_POINT('Ctrl Pts',(5.20552403999925,139.78422887007,14.1820755449686));
#82486=CARTESIAN_POINT('Ctrl Pts',(5.21116027523093,139.724659602014,14.2316314206108));
#82487=CARTESIAN_POINT('Ctrl Pts',(5.22132278042843,139.610124934469,14.309243050884));
#82488=CARTESIAN_POINT('Ctrl Pts',(5.22581329326415,139.556981271851,14.3395177144443));
#82489=CARTESIAN_POINT('Ctrl Pts',(5.23108082421731,139.489510191581,14.3712876033704));
#82490=CARTESIAN_POINT('Ctrl Pts',(5.2320252411473,139.477196293732,14.3768291847769));
#82491=CARTESIAN_POINT('Ctrl Pts',(5.23351032439833,139.457444512307,14.3853126167136));
#82492=CARTESIAN_POINT('Ctrl Pts',(5.23405846243536,139.4500676439,14.3883924307198));
#82493=CARTESIAN_POINT('Ctrl Pts',(5.23507673492042,139.436189982178,14.3940210716225));
#82494=CARTESIAN_POINT('Ctrl Pts',(5.23554792879041,139.429696842429,14.3965876322717));
#82495=CARTESIAN_POINT('Ctrl Pts',(5.23683717483486,139.411746604088,14.4034989470134));
#82496=CARTESIAN_POINT('Ctrl Pts',(5.23764847261467,139.400243568925,14.4077230281826));
#82497=CARTESIAN_POINT('Ctrl Pts',(5.24246520709872,139.330860070976,14.4319796486134));
#82498=CARTESIAN_POINT('Ctrl Pts',(5.24626757305046,139.271547788967,14.4476541219496));
#82499=CARTESIAN_POINT('Ctrl Pts',(5.25351799155964,139.156217720196,14.468684571268));
#82500=CARTESIAN_POINT('Ctrl Pts',(5.25695968664792,139.100512193876,14.4747870199149));
#82501=CARTESIAN_POINT('Ctrl Pts',(5.26204983975474,139.019899740251,14.4778409781601));
#82502=CARTESIAN_POINT('Ctrl Pts',(5.2636241456482,138.995191027162,14.4779992055164));
#82503=CARTESIAN_POINT('Ctrl Pts',(5.26655622101752,138.949818475238,14.4768622413893));
#82504=CARTESIAN_POINT('Ctrl Pts',(5.26790699961545,138.929158572957,14.4757994424078));
#82505=CARTESIAN_POINT('Ctrl Pts',(5.27017923438846,138.894896966168,14.4731306963648));
#82506=CARTESIAN_POINT('Ctrl Pts',(5.27109106375583,138.881275661597,14.4718305266946));
#82507=CARTESIAN_POINT('Ctrl Pts',(5.27292758330604,138.854117010114,14.4687598289257));
#82508=CARTESIAN_POINT('Ctrl Pts',(5.27385209567943,138.840581659259,14.4669906382592));
#82509=CARTESIAN_POINT('Ctrl Pts',(5.27618409523374,138.806798640559,14.4619762121945));
#82510=CARTESIAN_POINT('Ctrl Pts',(5.27760059194484,138.786599950158,14.4584367958131));
#82511=CARTESIAN_POINT('Ctrl Pts',(5.28498690746441,138.682978640334,14.4374772997715));
#82512=CARTESIAN_POINT('Ctrl Pts',(5.29122057227595,138.601545557684,14.4115693959577));
#82513=CARTESIAN_POINT('Ctrl Pts',(5.30034502742721,138.48792490543,14.3613193499744));
#82514=CARTESIAN_POINT('Ctrl Pts',(5.3032075404861,138.453020919967,14.3437594762598));
#82515=CARTESIAN_POINT('Ctrl Pts',(5.30720583402013,138.404704164047,14.3163611549259));
#82516=CARTESIAN_POINT('Ctrl Pts',(5.30838342192403,138.390527780937,14.3079240044388));
#82517=CARTESIAN_POINT('Ctrl Pts',(5.31046943494251,138.365442821813,14.2922716950244));
#82518=CARTESIAN_POINT('Ctrl Pts',(5.31138284959304,138.354468385578,14.2851674475823));
#82519=CARTESIAN_POINT('Ctrl Pts',(5.31283111679029,138.337050207783,14.2734757979603));
#82520=CARTESIAN_POINT('Ctrl Pts',(5.31337285220417,138.330530709874,14.2690038372454));
#82521=CARTESIAN_POINT('Ctrl Pts',(5.31445661808999,138.317470303601,14.2598504882824));
#82522=CARTESIAN_POINT('Ctrl Pts',(5.31499848416948,138.310931361057,14.2551670883812));
#82523=CARTESIAN_POINT('Ctrl Pts',(5.31645472452214,138.293352321636,14.2423019289567));
#82524=CARTESIAN_POINT('Ctrl Pts',(5.31736096164767,138.282406241601,14.2339930968185));
#82525=CARTESIAN_POINT('Ctrl Pts',(5.32266653879621,138.218484935483,14.1836850546494));
#82526=CARTESIAN_POINT('Ctrl Pts',(5.32683006210891,138.169054047073,14.1373745306261));
#82527=CARTESIAN_POINT('Ctrl Pts',(5.33560138245444,138.074191093655,14.031777369083));
#82528=CARTESIAN_POINT('Ctrl Pts',(5.34019818028491,138.029868043393,13.9719096856994));
#82529=CARTESIAN_POINT('Ctrl Pts',(5.34627003764482,137.981472087225,13.8916686045324));
#82530=CARTESIAN_POINT('Ctrl Pts',(5.34753915001645,137.971872167549,13.8748251356476));
#82531=CARTESIAN_POINT('Ctrl Pts',(5.34971417390312,137.956321207567,13.8459035183746));
#82532=CARTESIAN_POINT('Ctrl Pts',(5.35061224843461,137.95015346722,13.8339459760118));
#82533=CARTESIAN_POINT('Ctrl Pts',(5.35234354011832,137.938753398529,13.810882918818));
#82534=CARTESIAN_POINT('Ctrl Pts',(5.35317542956792,137.93348718595,13.7997960618861));
#82535=CARTESIAN_POINT('Ctrl Pts',(5.35540713930006,137.919925425752,13.7700539946723));
#82536=CARTESIAN_POINT('Ctrl Pts',(5.35681726335248,137.911940384338,13.7512627016996));
#82537=CARTESIAN_POINT('Ctrl Pts',(5.35947526120786,137.897974245769,13.7158670586819));
#82538=CARTESIAN_POINT('Ctrl Pts',(5.36071819853113,137.891873122424,13.6993248713083));
#82539=CARTESIAN_POINT('Ctrl Pts',(5.36197089565136,137.88614821265,13.6826607614027));
#82540=CARTESIAN_POINT('Origin',(1.13913288526384,139.,13.3));
#82541=CARTESIAN_POINT('',(5.96182583603507,137.88614821265,13.6826607614027));
#82542=CARTESIAN_POINT('',(5.8638006232474,137.886148212564,13.6826607611511));
#82543=CARTESIAN_POINT('',(1.13913288526384,137.88614821265,13.6826607614027));
#82544=CARTESIAN_POINT('Ctrl Pts',(5.96182583603505,137.88614821265,13.6826607614027));
#82545=CARTESIAN_POINT('Ctrl Pts',(5.96011823121893,137.893737617578,13.7047520576529));
#82546=CARTESIAN_POINT('Ctrl Pts',(5.95840141063008,137.90198616988,13.7266232135534));
#82547=CARTESIAN_POINT('Ctrl Pts',(5.95211510907587,137.934534674042,13.8057074043303));
#82548=CARTESIAN_POINT('Ctrl Pts',(5.9475447436074,137.96269723102,13.8612135973465));
#82549=CARTESIAN_POINT('Ctrl Pts',(5.94228481536763,138.001629159891,13.9249055316043));
#82550=CARTESIAN_POINT('Ctrl Pts',(5.94141243344031,138.008316912279,13.9354651393033));
#82551=CARTESIAN_POINT('Ctrl Pts',(5.94001680258528,138.019411871242,13.9523816028852));
#82552=CARTESIAN_POINT('Ctrl Pts',(5.93948734669202,138.023715684227,13.9588048129372));
#82553=CARTESIAN_POINT('Ctrl Pts',(5.93841366855325,138.032644380719,13.9718507291547));
#82554=CARTESIAN_POINT('Ctrl Pts',(5.93786980837908,138.037274688495,13.9784690712705));
#82555=CARTESIAN_POINT('Ctrl Pts',(5.93639078171179,138.050150845936,13.9964763656915));
#82556=CARTESIAN_POINT('Ctrl Pts',(5.93546426459298,138.058533394493,14.0077664989763));
#82557=CARTESIAN_POINT('Ctrl Pts',(5.9303590919216,138.106358145992,14.0698260967524));
#82558=CARTESIAN_POINT('Ctrl Pts',(5.92639031211371,138.149707998658,14.1174554577033));
#82559=CARTESIAN_POINT('Ctrl Pts',(5.91921569174844,138.234617431066,14.1966426184107));
#82560=CARTESIAN_POINT('Ctrl Pts',(5.91601972492253,138.274789295956,14.2294339716529));
#82561=CARTESIAN_POINT('Ctrl Pts',(5.91124512842704,138.336318920303,14.2732345976469));
#82562=CARTESIAN_POINT('Ctrl Pts',(5.90973019464238,138.356061147215,14.2864080327878));
#82563=CARTESIAN_POINT('Ctrl Pts',(5.90689712771635,138.39320825991,14.3096046499102));
#82564=CARTESIAN_POINT('Ctrl Pts',(5.90558519653706,138.410497602901,14.3197963578745));
#82565=CARTESIAN_POINT('Ctrl Pts',(5.9033626306518,138.439860043723,14.3361086747282));
#82566=CARTESIAN_POINT('Ctrl Pts',(5.90246079971189,138.45179383174,14.3424720273424));
#82567=CARTESIAN_POINT('Ctrl Pts',(5.90063208098384,138.47601249583,14.3548550818232));
#82568=CARTESIAN_POINT('Ctrl Pts',(5.89970516694265,138.488297933249,14.3608690379197));
#82569=CARTESIAN_POINT('Ctrl Pts',(5.89734161949195,138.519631265975,14.3755364082752));
#82570=CARTESIAN_POINT('Ctrl Pts',(5.89589535788382,138.538809453353,14.383898458643));
#82571=CARTESIAN_POINT('Ctrl Pts',(5.88879460938716,138.63293656073,14.4219892592371));
#82572=CARTESIAN_POINT('Ctrl Pts',(5.88290966751907,138.710570835203,14.4444746595592));
#82573=CARTESIAN_POINT('Ctrl Pts',(5.87396041223407,138.830491382721,14.4662184857584));
#82574=CARTESIAN_POINT('Ctrl Pts',(5.87093113828985,138.871465522935,14.4714426660526));
#82575=CARTESIAN_POINT('Ctrl Pts',(5.86673321892935,138.929575724571,14.4757653670297));
#82576=CARTESIAN_POINT('Ctrl Pts',(5.86551913838495,138.946546686428,14.4766590750894));
#82577=CARTESIAN_POINT('Ctrl Pts',(5.86337698717866,138.976875814769,14.4775986440174));
#82578=CARTESIAN_POINT('Ctrl Pts',(5.86244354722315,138.99022654906,14.4777851297341));
#82579=CARTESIAN_POINT('Ctrl Pts',(5.86097283727908,139.011520787886,14.4777204330298));
#82580=CARTESIAN_POINT('Ctrl Pts',(5.86042830871534,139.019463170119,14.4776159565997));
#82581=CARTESIAN_POINT('Ctrl Pts',(5.85934958939536,139.035325980885,14.4772467568723));
#82582=CARTESIAN_POINT('Ctrl Pts',(5.85881541382726,139.04324599714,14.4769824314348));
#82583=CARTESIAN_POINT('Ctrl Pts',(5.85739605001381,139.064444022689,14.4760606910822));
#82584=CARTESIAN_POINT('Ctrl Pts',(5.8565183556189,139.077714997452,14.4752583533737));
#82585=CARTESIAN_POINT('Ctrl Pts',(5.85089284080241,139.163593226909,14.4686051832654));
#82586=CARTESIAN_POINT('Ctrl Pts',(5.84642396385226,139.235547158018,14.4562530173298));
#82587=CARTESIAN_POINT('Ctrl Pts',(5.83900115377145,139.351512807176,14.4250619092679));
#82588=CARTESIAN_POINT('Ctrl Pts',(5.83607563632052,139.396338858637,14.4100633690781));
#82589=CARTESIAN_POINT('Ctrl Pts',(5.83165195637274,139.461091345754,14.3839741643022));
#82590=CARTESIAN_POINT('Ctrl Pts',(5.83020674910058,139.481793247242,14.3749327386346));
#82591=CARTESIAN_POINT('Ctrl Pts',(5.82748953566476,139.519722021184,14.3570517580433));
#82592=CARTESIAN_POINT('Ctrl Pts',(5.82622284606153,139.537015685281,14.3483718245154));
#82593=CARTESIAN_POINT('Ctrl Pts',(5.82405458779701,139.565902199651,14.3329709793861));
#82594=CARTESIAN_POINT('Ctrl Pts',(5.82316085990642,139.577608733563,14.3264708810573));
#82595=CARTESIAN_POINT('Ctrl Pts',(5.82143998438085,139.599752720506,14.3136765899579));
#82596=CARTESIAN_POINT('Ctrl Pts',(5.82061417845938,139.610208321068,14.3074171629726));
#82597=CARTESIAN_POINT('Ctrl Pts',(5.8184045395303,139.637721463053,14.2903604840786));
#82598=CARTESIAN_POINT('Ctrl Pts',(5.81701068083554,139.654601059972,14.2792854116494));
#82599=CARTESIAN_POINT('Ctrl Pts',(5.80949571061924,139.743042536861,14.2179485420254));
#82600=CARTESIAN_POINT('Ctrl Pts',(5.80309361467179,139.809113398461,14.1602744838695));
#82601=CARTESIAN_POINT('Ctrl Pts',(5.79388054169744,139.89388896505,14.0677921588766));
#82602=CARTESIAN_POINT('Ctrl Pts',(5.79109352662553,139.918222608693,14.0385186581146));
#82603=CARTESIAN_POINT('Ctrl Pts',(5.7871885583161,139.950856256386,13.9951480957466));
#82604=CARTESIAN_POINT('Ctrl Pts',(5.78603040691135,139.960346211489,13.9819777872256));
#82605=CARTESIAN_POINT('Ctrl Pts',(5.78397579042687,139.976885930995,13.9579934684279));
#82606=CARTESIAN_POINT('Ctrl Pts',(5.78307451665183,139.984035879364,13.9472518438628));
#82607=CARTESIAN_POINT('Ctrl Pts',(5.78164272385419,139.995244693554,13.9297972152336));
#82608=CARTESIAN_POINT('Ctrl Pts',(5.78110552454486,139.999415368156,13.9231576565738));
#82609=CARTESIAN_POINT('Ctrl Pts',(5.78002913189269,140.007707355316,13.9096597055595));
#82610=CARTESIAN_POINT('Ctrl Pts',(5.77949012598819,140.011825689545,13.9028000115705));
#82611=CARTESIAN_POINT('Ctrl Pts',(5.77803953038277,140.022804837136,13.8840830193521));
#82612=CARTESIAN_POINT('Ctrl Pts',(5.7771360497345,140.029529426851,13.8721467535701));
#82613=CARTESIAN_POINT('Ctrl Pts',(5.77182655191937,140.068240233469,13.8005408595235));
#82614=CARTESIAN_POINT('Ctrl Pts',(5.76765739848215,140.095244972066,13.7383138376469));
#82615=CARTESIAN_POINT('Ctrl Pts',(5.76038419398895,140.13263494729,13.626699489664));
#82616=CARTESIAN_POINT('Ctrl Pts',(5.75729523096722,140.145480113471,13.5783332550406));
#82617=CARTESIAN_POINT('Ctrl Pts',(5.7526595334823,140.159745071315,13.5064662959409));
#82618=CARTESIAN_POINT('Ctrl Pts',(5.75117220086569,140.163599090439,13.483504819973));
#82619=CARTESIAN_POINT('Ctrl Pts',(5.74838539174638,140.169464360754,13.4408521229527));
#82620=CARTESIAN_POINT('Ctrl Pts',(5.74709177561977,140.17166456223,13.4211952596649));
#82621=CARTESIAN_POINT('Ctrl Pts',(5.74489229785851,140.174528094547,13.38808980171));
#82622=CARTESIAN_POINT('Ctrl Pts',(5.74399487414104,140.175457664827,13.3746680040289));
#82623=CARTESIAN_POINT('Ctrl Pts',(5.74216870547368,140.176869511108,13.3475497109395));
#82624=CARTESIAN_POINT('Ctrl Pts',(5.74123983092785,140.177343043011,13.333854875685));
#82625=CARTESIAN_POINT('Ctrl Pts',(5.73885796269891,140.177939490723,13.2990074426091));
#82626=CARTESIAN_POINT('Ctrl Pts',(5.73739496875569,140.177731684799,13.2778548660421));
#82627=CARTESIAN_POINT('Ctrl Pts',(5.73044158027849,140.174079960356,13.1785488992596));
#82628=CARTESIAN_POINT('Ctrl Pts',(5.72473632171545,140.163424968954,13.1008699019074));
#82629=CARTESIAN_POINT('Ctrl Pts',(5.71443334966285,140.130656661637,12.9644988971715));
#82630=CARTESIAN_POINT('Ctrl Pts',(5.70987162177614,140.111412196429,12.9053992202477));
#82631=CARTESIAN_POINT('Ctrl Pts',(5.70461132926718,140.082766585667,12.8364591300526));
#82632=CARTESIAN_POINT('Ctrl Pts',(5.70373238358566,140.077748563387,12.8249087627956));
#82633=CARTESIAN_POINT('Ctrl Pts',(5.70232730544245,140.069334244965,12.8063606836711));
#82634=CARTESIAN_POINT('Ctrl Pts',(5.70179489757434,140.066052305493,12.7993124767048));
#82635=CARTESIAN_POINT('Ctrl Pts',(5.70071822097289,140.059218390662,12.7850080414531));
#82636=CARTESIAN_POINT('Ctrl Pts',(5.7001742815189,140.055661111946,12.77775490153));
#82637=CARTESIAN_POINT('Ctrl Pts',(5.698694872363,140.045706583019,12.7579754463378));
#82638=CARTESIAN_POINT('Ctrl Pts',(5.69776805799494,140.039158930058,12.7455258026106));
#82639=CARTESIAN_POINT('Ctrl Pts',(5.6926646769622,140.001465363884,12.6768699253258));
#82640=CARTESIAN_POINT('Ctrl Pts',(5.68869771561106,139.965979740144,12.6231624762119));
#82641=CARTESIAN_POINT('Ctrl Pts',(5.68001394235995,139.879191715745,12.5126428405012));
#82642=CARTESIAN_POINT('Ctrl Pts',(5.67530830155633,139.826390953846,12.4573934737635));
#82643=CARTESIAN_POINT('Ctrl Pts',(5.66909597460168,139.753685133914,12.3947693477996));
#82644=CARTESIAN_POINT('Ctrl Pts',(5.66780612502901,139.738426009796,12.3822795800316));
#82645=CARTESIAN_POINT('Ctrl Pts',(5.66561061823598,139.712242373337,12.3619238963418));
#82646=CARTESIAN_POINT('Ctrl Pts',(5.66471330389447,139.701483214879,12.3538513602601));
#82647=CARTESIAN_POINT('Ctrl Pts',(5.66288526993955,139.679466075503,12.337914014108));
#82648=CARTESIAN_POINT('Ctrl Pts',(5.6619543873137,139.668204104716,12.3300583323489));
#82649=CARTESIAN_POINT('Ctrl Pts',(5.65956262261753,139.639157815825,12.3105433366179));
#82650=CARTESIAN_POINT('Ctrl Pts',(5.65809159474552,139.621191026125,12.2991659432353));
#82651=CARTESIAN_POINT('Ctrl Pts',(5.65125654899255,139.537297079988,12.2491698781763));
#82652=CARTESIAN_POINT('Ctrl Pts',(5.64568953666921,139.46802680662,12.2165427676249));
#82653=CARTESIAN_POINT('Ctrl Pts',(5.63553434896756,139.33781508253,12.1700415315658));
#82654=CARTESIAN_POINT('Ctrl Pts',(5.63098134508052,139.277977521562,12.153852133142));
#82655=CARTESIAN_POINT('Ctrl Pts',(5.62565780568099,139.203897184205,12.1399557943558));
#82656=CARTESIAN_POINT('Ctrl Pts',(5.62471531338484,139.190611436747,12.1376988600848));
#82657=CARTESIAN_POINT('Ctrl Pts',(5.62323453114311,139.169421700438,12.1344723587735));
#82658=CARTESIAN_POINT('Ctrl Pts',(5.62268878413256,139.161541974721,12.1333541262194));
#82659=CARTESIAN_POINT('Ctrl Pts',(5.62161145564149,139.145834716709,12.1312872663778));
#82660=CARTESIAN_POINT('Ctrl Pts',(5.62107983316652,139.138007814677,12.1303371983461));
#82661=CARTESIAN_POINT('Ctrl Pts',(5.61967445894418,139.11713379565,12.1280158594219));
#82662=CARTESIAN_POINT('Ctrl Pts',(5.61880795836829,139.104071892936,12.1267838099828));
#82663=CARTESIAN_POINT('Ctrl Pts',(5.61309025665132,139.016831634641,12.1200235325787));
#82664=CARTESIAN_POINT('Ctrl Pts',(5.6085322527808,138.942284339824,12.1213144954013));
#82665=CARTESIAN_POINT('Ctrl Pts',(5.59978100013999,138.80159967119,12.1371396193206));
#82666=CARTESIAN_POINT('Ctrl Pts',(5.59561024351538,138.735621860578,12.1503436133796));
#82667=CARTESIAN_POINT('Ctrl Pts',(5.58996977868262,138.651902036324,12.1746893929856));
#82668=CARTESIAN_POINT('Ctrl Pts',(5.58866041278935,138.632818138689,12.1807709982124));
#82669=CARTESIAN_POINT('Ctrl Pts',(5.58644177020448,138.601142089389,12.1917627615633));
#82670=CARTESIAN_POINT('Ctrl Pts',(5.58554126267944,138.588462294832,12.1964085443104));
#82671=CARTESIAN_POINT('Ctrl Pts',(5.58371499454321,138.563121207182,12.2061907819345));
#82672=CARTESIAN_POINT('Ctrl Pts',(5.58278920357777,138.550463853287,12.2113315883345));
#82673=CARTESIAN_POINT('Ctrl Pts',(5.5804284017653,138.518679587267,12.2248896189564));
#82674=CARTESIAN_POINT('Ctrl Pts',(5.57898376739546,138.499682673687,12.2335975679513));
#82675=CARTESIAN_POINT('Ctrl Pts',(5.57184231958782,138.408016573631,12.2786046844823));
#82676=CARTESIAN_POINT('Ctrl Pts',(5.5659105059868,138.339014820911,12.3218449599085));
#82677=CARTESIAN_POINT('Ctrl Pts',(5.55563458038244,138.228767722104,12.407957155959));
#82678=CARTESIAN_POINT('Ctrl Pts',(5.55132669574459,138.185275319068,12.4474951161085));
#82679=CARTESIAN_POINT('Ctrl Pts',(5.54626578317972,138.135944832477,12.4995790662128));
#82680=CARTESIAN_POINT('Ctrl Pts',(5.54535485810406,138.127137740602,12.5091924915245));
#82681=CARTESIAN_POINT('Ctrl Pts',(5.54391168352428,138.113274769112,12.5248385263968));
#82682=CARTESIAN_POINT('Ctrl Pts',(5.54337257195953,138.108116800488,12.5307787613485));
#82683=CARTESIAN_POINT('Ctrl Pts',(5.54229607643484,138.097851869321,12.5428425676033));
#82684=CARTESIAN_POINT('Ctrl Pts',(5.54175882467009,138.092746811157,12.5489671859373));
#82685=CARTESIAN_POINT('Ctrl Pts',(5.5403194320846,138.079132384123,12.5656420535104));
#82686=CARTESIAN_POINT('Ctrl Pts',(5.53942517943703,138.070742021189,12.5762884502685));
#82687=CARTESIAN_POINT('Ctrl Pts',(5.53395895523541,138.020036812751,12.6429637024989));
#82688=CARTESIAN_POINT('Ctrl Pts',(5.52964353645112,137.982613808703,12.7025451332079));
#82689=CARTESIAN_POINT('Ctrl Pts',(5.52086388672032,137.918088483729,12.8291234519681));
#82690=CARTESIAN_POINT('Ctrl Pts',(5.51641309961538,137.891387041568,12.8959789339011));
#82691=CARTESIAN_POINT('Ctrl Pts',(5.5105006318927,137.865415890983,12.9834698235924));
#82692=CARTESIAN_POINT('Ctrl Pts',(5.50922904837508,137.860349560329,13.0022261634588));
#82693=CARTESIAN_POINT('Ctrl Pts',(5.50705537625462,137.852576937392,13.0341149227774));
#82694=CARTESIAN_POINT('Ctrl Pts',(5.50616124339647,137.849626714765,13.0471841809013));
#82695=CARTESIAN_POINT('Ctrl Pts',(5.50444158497547,137.844424697014,13.0722090358037));
#82696=CARTESIAN_POINT('Ctrl Pts',(5.50361743191009,137.842133926922,13.0841548200102));
#82697=CARTESIAN_POINT('Ctrl Pts',(5.50141720173685,137.836553502458,13.1159066498313));
#82698=CARTESIAN_POINT('Ctrl Pts',(5.50003124455126,137.833584705413,13.1357642290293));
#82699=CARTESIAN_POINT('Ctrl Pts',(5.49247408934862,137.820319170475,13.2432094903203));
#82700=CARTESIAN_POINT('Ctrl Pts',(5.48601590191447,137.819379492195,13.3316551585687));
#82701=CARTESIAN_POINT('Ctrl Pts',(5.47677675407356,137.832131187445,13.4568321164502));
#82702=CARTESIAN_POINT('Ctrl Pts',(5.47401798799671,137.837744278816,13.494102544814));
#82703=CARTESIAN_POINT('Ctrl Pts',(5.47014753393553,137.848299941047,13.5468652462176));
#82704=CARTESIAN_POINT('Ctrl Pts',(5.46899627388069,137.85179068066,13.5626230886353));
#82705=CARTESIAN_POINT('Ctrl Pts',(5.46695252278782,137.85863990202,13.5907872258973));
#82706=CARTESIAN_POINT('Ctrl Pts',(5.46605529100999,137.861879635933,13.6032196482534));
#82707=CARTESIAN_POINT('Ctrl Pts',(5.46462838066217,137.867419868687,13.6231386417839));
#82708=CARTESIAN_POINT('Ctrl Pts',(5.46409209458997,137.869592658602,13.6306593250235));
#82709=CARTESIAN_POINT('Ctrl Pts',(5.46301552798629,137.874142244438,13.6458376060974));
#82710=CARTESIAN_POINT('Ctrl Pts',(5.46247546231711,137.876522553658,13.6534936669756));
#82711=CARTESIAN_POINT('Ctrl Pts',(5.46143383519277,137.881300782265,13.6683264361376));
#82712=CARTESIAN_POINT('Ctrl Pts',(5.46093185542975,137.883689981072,13.6755053226633));
#82713=CARTESIAN_POINT('Ctrl Pts',(5.46043320712869,137.886148212658,13.6826607614259));
#82714=CARTESIAN_POINT('Ctrl Pts',(5.36197089565136,137.88614821265,13.6826607614027));
#82715=CARTESIAN_POINT('Ctrl Pts',(5.36682188552324,137.863978863903,13.6181300563578));
#82716=CARTESIAN_POINT('Ctrl Pts',(5.37182980528586,137.847451361312,13.5517717427999));
#82717=CARTESIAN_POINT('Ctrl Pts',(5.38086387332755,137.828198566571,13.4302761780259));
#82718=CARTESIAN_POINT('Ctrl Pts',(5.38487227722085,137.823410219707,13.3756838698077));
#82719=CARTESIAN_POINT('Ctrl Pts',(5.38966919771979,137.822201126917,13.3077301872115));
#82720=CARTESIAN_POINT('Ctrl Pts',(5.39059360907863,137.822188565055,13.2945043702931));
#82721=CARTESIAN_POINT('Ctrl Pts',(5.3920549261728,137.822524919861,13.2733450876296));
#82722=CARTESIAN_POINT('Ctrl Pts',(5.39259892193165,137.822731275235,13.2654108603999));
#82723=CARTESIAN_POINT('Ctrl Pts',(5.39368271419258,137.823306963659,13.2494757895673));
#82724=CARTESIAN_POINT('Ctrl Pts',(5.3942224114107,137.823677730356,13.2414754322686));
#82725=CARTESIAN_POINT('Ctrl Pts',(5.39566565615187,137.824896799688,13.2199262831634));
#82726=CARTESIAN_POINT('Ctrl Pts',(5.39656131327966,137.825897805532,13.2063869266585));
#82727=CARTESIAN_POINT('Ctrl Pts',(5.40203800174505,137.833532014225,13.1228092222845));
#82728=CARTESIAN_POINT('Ctrl Pts',(5.4063614819717,137.84619633229,13.0534565422798));
#82729=CARTESIAN_POINT('Ctrl Pts',(5.41503137365049,137.883643820636,12.9182483767596));
#82730=CARTESIAN_POINT('Ctrl Pts',(5.41936322646518,137.908272466742,12.8526578414945));
#82731=CARTESIAN_POINT('Ctrl Pts',(5.42519570062476,137.947359574834,12.7713654548078));
#82732=CARTESIAN_POINT('Ctrl Pts',(5.42652106620689,137.956617779177,12.7533192808238));
#82733=CARTESIAN_POINT('Ctrl Pts',(5.42876289862504,137.972859738674,12.7235772645878));
#82734=CARTESIAN_POINT('Ctrl Pts',(5.429670306822,137.979588973214,12.7117469961956));
#82735=CARTESIAN_POINT('Ctrl Pts',(5.43150781347319,137.993513461199,12.6882252865167));
#82736=CARTESIAN_POINT('Ctrl Pts',(5.43243789553479,138.00071112128,12.6765377622134));
#82737=CARTESIAN_POINT('Ctrl Pts',(5.43480468031454,138.019390766301,12.6473605614756));
#82738=CARTESIAN_POINT('Ctrl Pts',(5.43625097664947,138.031137151095,12.6300467265993));
#82739=CARTESIAN_POINT('Ctrl Pts',(5.44341168610429,138.09086175676,12.546872174651));
#82740=CARTESIAN_POINT('Ctrl Pts',(5.44936274420983,138.145118311036,12.4858089584843));
#82741=CARTESIAN_POINT('Ctrl Pts',(5.45835521298162,138.23546263142,12.4031967946221));
#82742=CARTESIAN_POINT('Ctrl Pts',(5.46136226373166,138.267118942544,12.3771462536125));
#82743=CARTESIAN_POINT('Ctrl Pts',(5.46553499211145,138.31369631189,12.342728155423));
#82744=CARTESIAN_POINT('Ctrl Pts',(5.46674572066487,138.327539309158,12.3329535612546));
#82745=CARTESIAN_POINT('Ctrl Pts',(5.468883428963,138.352644662601,12.3160264638716));
#82746=CARTESIAN_POINT('Ctrl Pts',(5.46981574364695,138.36382663477,12.3087602006212));
#82747=CARTESIAN_POINT('Ctrl Pts',(5.47128644511262,138.381876454392,12.2974623757708));
#82748=CARTESIAN_POINT('Ctrl Pts',(5.4718320716982,138.388665622955,12.2933080437457));
#82749=CARTESIAN_POINT('Ctrl Pts',(5.47291596152569,138.402349558227,12.2851242580265));
#82750=CARTESIAN_POINT('Ctrl Pts',(5.47345417100921,138.409244231173,12.2810954641386));
#82751=CARTESIAN_POINT('Ctrl Pts',(5.47488848877806,138.42786988857,12.2704644819648));
#82752=CARTESIAN_POINT('Ctrl Pts',(5.47577687469264,138.439674327441,12.263992554982));
#82753=CARTESIAN_POINT('Ctrl Pts',(5.48132573606793,138.514898910071,12.224411784423));
#82754=CARTESIAN_POINT('Ctrl Pts',(5.4857185384777,138.581121825655,12.1969330431389));
#82755=CARTESIAN_POINT('Ctrl Pts',(5.49440436971266,138.715298149315,12.1550985405107));
#82756=CARTESIAN_POINT('Ctrl Pts',(5.49868088550042,138.782829577452,12.1403922561227));
#82757=CARTESIAN_POINT('Ctrl Pts',(5.504451557816,138.871356907183,12.1291214330861));
#82758=CARTESIAN_POINT('Ctrl Pts',(5.50577586535948,138.891519599696,12.1270815940121));
#82759=CARTESIAN_POINT('Ctrl Pts',(5.50801644032936,138.925292438844,12.1245430731091));
#82760=CARTESIAN_POINT('Ctrl Pts',(5.50892367270809,138.938877082432,12.123758456197));
#82761=CARTESIAN_POINT('Ctrl Pts',(5.51076125356541,138.966189655999,12.1226553565063));
#82762=CARTESIAN_POINT('Ctrl Pts',(5.51169159263162,138.979915615594,12.1223412469484));
#82763=CARTESIAN_POINT('Ctrl Pts',(5.51405994577189,139.014581725053,12.1221541440527));
#82764=CARTESIAN_POINT('Ctrl Pts',(5.51550757974184,139.035518048069,12.1225995338542));
#82765=CARTESIAN_POINT('Ctrl Pts',(5.52265668607394,139.137627038583,12.1274975702691));
#82766=CARTESIAN_POINT('Ctrl Pts',(5.52859348008077,139.218190073044,12.1397878829998));
#82767=CARTESIAN_POINT('Ctrl Pts',(5.53886463003402,139.353504388969,12.1750291775378));
#82768=CARTESIAN_POINT('Ctrl Pts',(5.54316288031464,139.409002349907,12.1939968366965));
#82769=CARTESIAN_POINT('Ctrl Pts',(5.54821765706877,139.474884686811,12.2221546852387));
#82770=CARTESIAN_POINT('Ctrl Pts',(5.54913123439586,139.486820825186,12.2274928865683));
#82771=CARTESIAN_POINT('Ctrl Pts',(5.55057969761034,139.505828385554,12.2363763783334));
#82772=CARTESIAN_POINT('Ctrl Pts',(5.55112146934786,139.51295699207,12.2397959162087));
#82773=CARTESIAN_POINT('Ctrl Pts',(5.55220525987916,139.527266846377,12.246838371377));
#82774=CARTESIAN_POINT('Ctrl Pts',(5.55274711503062,139.534446466314,12.2504635654175));
#82775=CARTESIAN_POINT('Ctrl Pts',(5.55420323507417,139.553788757455,12.2604799990579));
#82776=CARTESIAN_POINT('Ctrl Pts',(5.55510936576549,139.565878035677,12.2670111765799));
#82777=CARTESIAN_POINT('Ctrl Pts',(5.56041828001316,139.636802180623,12.3069465628515));
#82778=CARTESIAN_POINT('Ctrl Pts',(5.56458486368812,139.692791083732,12.3451623834168));
#82779=CARTESIAN_POINT('Ctrl Pts',(5.57329425858792,139.801936855504,12.4343431609599));
#82780=CARTESIAN_POINT('Ctrl Pts',(5.57782570260514,139.854223497474,12.485896096615));
#82781=CARTESIAN_POINT('Ctrl Pts',(5.58385202193002,139.914147309965,12.5571519076069));
#82782=CARTESIAN_POINT('Ctrl Pts',(5.5851495800213,139.926529019252,12.5726538002598));
#82783=CARTESIAN_POINT('Ctrl Pts',(5.58735831220056,139.946688095044,12.5992433914044));
#82784=CARTESIAN_POINT('Ctrl Pts',(5.58826103824763,139.954676642614,12.6101662113392));
#82785=CARTESIAN_POINT('Ctrl Pts',(5.59010058705978,139.970439696361,12.6325175341307));
#82786=CARTESIAN_POINT('Ctrl Pts',(5.59103758041169,139.978204736135,12.6439500686964));
#82787=CARTESIAN_POINT('Ctrl Pts',(5.59344702684949,139.997492648709,12.6734517847421));
#82788=CARTESIAN_POINT('Ctrl Pts',(5.59492980259,140.008726366072,12.6917029803105));
#82789=CARTESIAN_POINT('Ctrl Pts',(5.60159010376457,140.056365412248,12.7740528516412));
#82790=CARTESIAN_POINT('Ctrl Pts',(5.6069541650649,140.087198753013,12.8411710030868));
#82791=CARTESIAN_POINT('Ctrl Pts',(5.61698541386664,140.132348926649,12.9700929585311));
#82792=CARTESIAN_POINT('Ctrl Pts',(5.621619834382,140.148353484114,13.0310423328067));
#82793=CARTESIAN_POINT('Ctrl Pts',(5.62708408981924,140.161924378232,13.1070468534625));
#82794=CARTESIAN_POINT('Ctrl Pts',(5.62808517315643,140.164179656184,13.1211566293868));
#82795=CARTESIAN_POINT('Ctrl Pts',(5.62963745027156,140.167318029675,13.1433788881588));
#82796=CARTESIAN_POINT('Ctrl Pts',(5.63019723912315,140.168374476613,13.1514649957636));
#82797=CARTESIAN_POINT('Ctrl Pts',(5.63128419683653,140.170278751526,13.1673207724025));
#82798=CARTESIAN_POINT('Ctrl Pts',(5.63181166198327,140.171133381566,13.1750890643912));
#82799=CARTESIAN_POINT('Ctrl Pts',(5.63318032130447,140.173165669468,13.1954217536104));
#82800=CARTESIAN_POINT('Ctrl Pts',(5.63401500409069,140.174218874817,13.207998023348));
#82801=CARTESIAN_POINT('Ctrl Pts',(5.63879696128575,140.179144999282,13.2808918321207));
#82802=CARTESIAN_POINT('Ctrl Pts',(5.64254940791926,140.178572740028,13.3414262097369));
#82803=CARTESIAN_POINT('Ctrl Pts',(5.65123880748795,140.166445947691,13.4813995121271));
#82804=CARTESIAN_POINT('Ctrl Pts',(5.65615372363999,140.151426958968,13.5602238133784));
#82805=CARTESIAN_POINT('Ctrl Pts',(5.66267891362915,140.122509026128,13.6570880227883));
#82806=CARTESIAN_POINT('Ctrl Pts',(5.66405292482351,140.115946369976,13.6770967790771));
#82807=CARTESIAN_POINT('Ctrl Pts',(5.66635299728729,140.104217435125,13.7098633610865));
#82808=CARTESIAN_POINT('Ctrl Pts',(5.6672689013546,140.099357403154,13.7227261429256));
#82809=CARTESIAN_POINT('Ctrl Pts',(5.66910496668744,140.089249430018,13.7481242495252));
#82810=CARTESIAN_POINT('Ctrl Pts',(5.6700248085621,140.084007514727,13.7606596844854));
#82811=CARTESIAN_POINT('Ctrl Pts',(5.67232758836512,140.070453950662,13.7915583552907));
#82812=CARTESIAN_POINT('Ctrl Pts',(5.67371905473031,140.061885815778,13.8098035936312));
#82813=CARTESIAN_POINT('Ctrl Pts',(5.67679041771837,140.042169092015,13.8491330471507));
#82814=CARTESIAN_POINT('Ctrl Pts',(5.67847581454526,140.030839853676,13.8701162895264));
#82815=CARTESIAN_POINT('Ctrl Pts',(5.6839078867832,139.992709798467,13.9358813150836));
#82816=CARTESIAN_POINT('Ctrl Pts',(5.6877203422653,139.963568432228,13.9792295622909));
#82817=CARTESIAN_POINT('Ctrl Pts',(5.69619546502041,139.892964018112,14.0705256025989));
#82818=CARTESIAN_POINT('Ctrl Pts',(5.70085502399822,139.850306624853,14.1173581207714));
#82819=CARTESIAN_POINT('Ctrl Pts',(5.70634091658295,139.793668346083,14.1702810647204));
#82820=CARTESIAN_POINT('Ctrl Pts',(5.70734048050977,139.783068130794,14.1798311901365));
#82821=CARTESIAN_POINT('Ctrl Pts',(5.70889093767647,139.76614352106,14.1945309301579));
#82822=CARTESIAN_POINT('Ctrl Pts',(5.70945039581487,139.759935071139,14.1998111899257));
#82823=CARTESIAN_POINT('Ctrl Pts',(5.71053724938134,139.74766424837,14.2100298672042));
#82824=CARTESIAN_POINT('Ctrl Pts',(5.7110649335467,139.741606621542,14.2149731209203));
#82825=CARTESIAN_POINT('Ctrl Pts',(5.71243486977979,139.725631779048,14.2277463160764));
#82826=CARTESIAN_POINT('Ctrl Pts',(5.71327058834887,139.715636652824,14.2354779094405));
#82827=CARTESIAN_POINT('Ctrl Pts',(5.71807770182441,139.656825463542,14.2794760992685));
#82828=CARTESIAN_POINT('Ctrl Pts',(5.72185189642722,139.605377842012,14.3120832946091));
#82829=CARTESIAN_POINT('Ctrl Pts',(5.73053358443415,139.481345643389,14.3778361135982));
#82830=CARTESIAN_POINT('Ctrl Pts',(5.7354201748421,139.40746773503,14.4078776600163));
#82831=CARTESIAN_POINT('Ctrl Pts',(5.74191623340544,139.310881346831,14.4361747250445));
#82832=CARTESIAN_POINT('Ctrl Pts',(5.74329300544873,139.290479060936,14.4415612309419));
#82833=CARTESIAN_POINT('Ctrl Pts',(5.74559646017639,139.256551573897,14.4495501975841));
#82834=CARTESIAN_POINT('Ctrl Pts',(5.74651292423807,139.243105332055,14.4524687142399));
#82835=CARTESIAN_POINT('Ctrl Pts',(5.74834917249006,139.216290525029,14.4577987437709));
#82836=CARTESIAN_POINT('Ctrl Pts',(5.7492686217734,139.20292524099,14.4602158600819));
#82837=CARTESIAN_POINT('Ctrl Pts',(5.75156856492829,139.169663841002,14.4656389052601));
#82838=CARTESIAN_POINT('Ctrl Pts',(5.75295753760276,139.149727499954,14.4683670079621));
#82839=CARTESIAN_POINT('Ctrl Pts',(5.75916946047362,139.061280563168,14.478169308158));
#82840=CARTESIAN_POINT('Ctrl Pts',(5.76415635910438,138.992305898096,14.4797357087017));
#82841=CARTESIAN_POINT('Ctrl Pts',(5.77449130118481,138.851683660659,14.4705943404318));
#82842=CARTESIAN_POINT('Ctrl Pts',(5.77982313106866,138.780343914151,14.4593280257754));
#82843=CARTESIAN_POINT('Ctrl Pts',(5.78585957697632,138.697482296256,14.4383135992868));
#82844=CARTESIAN_POINT('Ctrl Pts',(5.78679716732042,138.684543177039,14.4347959475824));
#82845=CARTESIAN_POINT('Ctrl Pts',(5.78827417049479,138.664008007576,14.4288348129303));
#82846=CARTESIAN_POINT('Ctrl Pts',(5.78882092268096,138.656372224463,14.4265338943831));
#82847=CARTESIAN_POINT('Ctrl Pts',(5.78990515185667,138.641150085642,14.4217777711124));
#82848=CARTESIAN_POINT('Ctrl Pts',(5.79044260290603,138.63356410951,14.4193227310849));
#82849=CARTESIAN_POINT('Ctrl Pts',(5.79187186642266,138.613302138685,14.4125372981453));
#82850=CARTESIAN_POINT('Ctrl Pts',(5.79275605677644,138.600673720773,14.4080672525052));
#82851=CARTESIAN_POINT('Ctrl Pts',(5.79739757632423,138.534075080732,14.3832069670563));
#82852=CARTESIAN_POINT('Ctrl Pts',(5.80098340406711,138.481575453042,14.3590849292308));
#82853=CARTESIAN_POINT('Ctrl Pts',(5.80960056734649,138.359622209106,14.2917996029529));
#82854=CARTESIAN_POINT('Ctrl Pts',(5.814605247174,138.292488523141,14.2450799999782));
#82855=CARTESIAN_POINT('Ctrl Pts',(5.82122224019893,138.214893499294,14.1781457080737));
#82856=CARTESIAN_POINT('Ctrl Pts',(5.82258689779781,138.199430936439,14.1640724448636));
#82857=CARTESIAN_POINT('Ctrl Pts',(5.82487589799893,138.174451134215,14.1400907700195));
#82858=CARTESIAN_POINT('Ctrl Pts',(5.82579030349428,138.164717750215,14.1304137330231));
#82859=CARTESIAN_POINT('Ctrl Pts',(5.82762693125639,138.145669640668,14.1108021250543));
#82860=CARTESIAN_POINT('Ctrl Pts',(5.82854889259997,138.136353698801,14.1008717052129));
#82861=CARTESIAN_POINT('Ctrl Pts',(5.83086418808924,138.113580343084,14.0757367189011));
#82862=CARTESIAN_POINT('Ctrl Pts',(5.83226624931656,138.100340469371,14.0603419658106));
#82863=CARTESIAN_POINT('Ctrl Pts',(5.83864515977085,138.042590394452,13.9895715476658));
#82864=CARTESIAN_POINT('Ctrl Pts',(5.84379732247673,138.002754144235,13.930586924838));
#82865=CARTESIAN_POINT('Ctrl Pts',(5.85398720208869,137.935738527889,13.8089646980205));
#82866=CARTESIAN_POINT('Ctrl Pts',(5.85899827146271,137.908192168437,13.7468264717829));
#82867=CARTESIAN_POINT('Ctrl Pts',(5.8638006232474,137.886148212477,13.6826607608994));
#82868=CARTESIAN_POINT('Origin',(1.13913288526384,139.,13.3));
#82869=CARTESIAN_POINT('',(6.33649999999995,138.079525356866,14.0347254547431));
#82870=CARTESIAN_POINT('Ctrl Pts',(5.8638006232474,137.886148212477,13.6826607608994));
#82871=CARTESIAN_POINT('Ctrl Pts',(5.86388429847287,137.885764122958,13.6815427502732));
#82872=CARTESIAN_POINT('Ctrl Pts',(5.86396790781912,137.885381703865,13.6804241239518));
#82873=CARTESIAN_POINT('Ctrl Pts',(5.86501791222874,137.880596250179,13.6663568749282));
#82874=CARTESIAN_POINT('Ctrl Pts',(5.86597495468775,137.876417174238,13.653332405962));
#82875=CARTESIAN_POINT('Ctrl Pts',(5.8674750424359,137.870146044216,13.6325501113088));
#82876=CARTESIAN_POINT('Ctrl Pts',(5.86802580447681,137.867904963955,13.624839001515));
#82877=CARTESIAN_POINT('Ctrl Pts',(5.86911002365038,137.863612681198,13.6094858914516));
#82878=CARTESIAN_POINT('Ctrl Pts',(5.86964356156651,137.861559283325,13.6018449894409));
#82879=CARTESIAN_POINT('Ctrl Pts',(5.87105082358635,137.856306395664,13.5814819248007));
#82880=CARTESIAN_POINT('Ctrl Pts',(5.87191731820684,137.853242080742,13.5687255939068));
#82881=CARTESIAN_POINT('Ctrl Pts',(5.87650062730565,137.838001074446,13.500262063147));
#82882=CARTESIAN_POINT('Ctrl Pts',(5.88004814748423,137.829667640453,13.4437709197346));
#82883=CARTESIAN_POINT('Ctrl Pts',(5.88872563356953,137.819321165168,13.3039161097475));
#82884=CARTESIAN_POINT('Ctrl Pts',(5.89382425388596,137.821992770914,13.2205309687608));
#82885=CARTESIAN_POINT('Ctrl Pts',(5.90053741610881,137.83627768483,13.1175841704042));
#82886=CARTESIAN_POINT('Ctrl Pts',(5.90189153896307,137.839670027961,13.0971221230352));
#82887=CARTESIAN_POINT('Ctrl Pts',(5.90416740850559,137.846194945665,13.0633223863018));
#82888=CARTESIAN_POINT('Ctrl Pts',(5.90507943996471,137.849023241986,13.0499302656062));
#82889=CARTESIAN_POINT('Ctrl Pts',(5.90691475243274,137.855132599291,13.0233061707394));
#82890=CARTESIAN_POINT('Ctrl Pts',(5.90783782953162,137.858411285979,13.0100758354617));
#82891=CARTESIAN_POINT('Ctrl Pts',(5.91016281059429,137.867175000761,12.9771691638174));
#82892=CARTESIAN_POINT('Ctrl Pts',(5.91157362505443,137.872943493823,12.9575737032044));
#82893=CARTESIAN_POINT('Ctrl Pts',(5.91469660230516,137.886679352213,12.9150300031026));
#82894=CARTESIAN_POINT('Ctrl Pts',(5.91641460950508,137.894852937134,12.892158617108));
#82895=CARTESIAN_POINT('Ctrl Pts',(5.92202047917009,137.923499488783,12.8192001206648));
#82896=CARTESIAN_POINT('Ctrl Pts',(5.92597906404474,137.946716545242,12.7702690223766));
#82897=CARTESIAN_POINT('Ctrl Pts',(5.93440413821536,138.002898876133,12.6702717100563));
#82898=CARTESIAN_POINT('Ctrl Pts',(5.93886262816819,138.03662278238,12.6197986465558));
#82899=CARTESIAN_POINT('Ctrl Pts',(5.94414752971355,138.08279209635,12.5610661509843));
#82900=CARTESIAN_POINT('Ctrl Pts',(5.94513437790824,138.091697949538,12.5501460136798));
#82901=CARTESIAN_POINT('Ctrl Pts',(5.94666964013626,138.106036766014,12.5331945500879));
#82902=CARTESIAN_POINT('Ctrl Pts',(5.94722636665947,138.1113394724,12.5270554105948));
#82903=CARTESIAN_POINT('Ctrl Pts',(5.94831229026802,138.121894983259,12.5150871400933));
#82904=CARTESIAN_POINT('Ctrl Pts',(5.94884171400997,138.127143379395,12.5092548171225));
#82905=CARTESIAN_POINT('Ctrl Pts',(5.95022221904615,138.141086339032,12.4940685759916));
#82906=CARTESIAN_POINT('Ctrl Pts',(5.95106657794797,138.149875733096,12.4848025385747));
#82907=CARTESIAN_POINT('Ctrl Pts',(5.95583182697117,138.200856274503,12.432778890627));
#82908=CARTESIAN_POINT('Ctrl Pts',(5.95956152283631,138.2461238645,12.3931506946587));
#82909=CARTESIAN_POINT('Ctrl Pts',(5.96823776050969,138.358425199584,12.3090870509977));
#82910=CARTESIAN_POINT('Ctrl Pts',(5.97316187064017,138.427361911429,12.2677157093157));
#82911=CARTESIAN_POINT('Ctrl Pts',(5.97969718534888,138.519025009362,12.2247319724928));
#82912=CARTESIAN_POINT('Ctrl Pts',(5.98107110326613,138.538321106448,12.2163068775723));
#82913=CARTESIAN_POINT('Ctrl Pts',(5.983371425969,138.570580197344,12.2032398227215));
#82914=CARTESIAN_POINT('Ctrl Pts',(5.98428768673723,138.5834177004,12.198299762182));
#82915=CARTESIAN_POINT('Ctrl Pts',(5.98612480738559,138.609111535501,12.188925680898));
#82916=CARTESIAN_POINT('Ctrl Pts',(5.98704535313974,138.621963993435,12.1844872546537));
#82917=CARTESIAN_POINT('Ctrl Pts',(5.98935065813083,138.654076438949,12.1740163353991));
#82918=CARTESIAN_POINT('Ctrl Pts',(5.99074396974486,138.673419445305,12.1682547209062));
#82919=CARTESIAN_POINT('Ctrl Pts',(5.99719328657417,138.762601404431,12.1441671026697));
#82920=CARTESIAN_POINT('Ctrl Pts',(6.00243146976876,138.83387563574,12.1317930686623));
#82921=CARTESIAN_POINT('Ctrl Pts',(6.01271796100407,138.973593038792,12.1205848377712));
#82922=CARTESIAN_POINT('Ctrl Pts',(6.01773769207363,139.041711692283,12.1210263213067));
#82923=CARTESIAN_POINT('Ctrl Pts',(6.0235134845494,139.123086667609,12.1286190809397));
#82924=CARTESIAN_POINT('Ctrl Pts',(6.02447434600472,139.136735052204,12.1301337034884));
#82925=CARTESIAN_POINT('Ctrl Pts',(6.02597925489503,139.158333691631,12.1329137880145));
#82926=CARTESIAN_POINT('Ctrl Pts',(6.02653108535776,139.166302406915,12.1340225974664));
#82927=CARTESIAN_POINT('Ctrl Pts',(6.02761771237501,139.182103367527,12.1363865201235));
#82928=CARTESIAN_POINT('Ctrl Pts',(6.02815259224737,139.189935507188,12.1376392649964));
#82929=CARTESIAN_POINT('Ctrl Pts',(6.02956289708903,139.210710750106,12.1411778511123));
#82930=CARTESIAN_POINT('Ctrl Pts',(6.03043109134659,139.223629679946,12.1436014549905));
#82931=CARTESIAN_POINT('Ctrl Pts',(6.03516709088313,139.294624084771,12.1581544083189));
#82932=CARTESIAN_POINT('Ctrl Pts',(6.03885169377139,139.35176610428,12.1744437060111));
#82933=CARTESIAN_POINT('Ctrl Pts',(6.04746113527142,139.482323087329,12.2225823026564));
#82934=CARTESIAN_POINT('Ctrl Pts',(6.05236386339738,139.554196096006,12.25772858667));
#82935=CARTESIAN_POINT('Ctrl Pts',(6.05887427098244,139.639832034485,12.3109838574783));
#82936=CARTESIAN_POINT('Ctrl Pts',(6.06024780836079,139.657401276196,12.3225740761671));
#82937=CARTESIAN_POINT('Ctrl Pts',(6.06254821060037,139.685929728721,12.342511175626));
#82938=CARTESIAN_POINT('Ctrl Pts',(6.06346496497236,139.697070232362,12.3505909703074));
#82939=CARTESIAN_POINT('Ctrl Pts',(6.0653037997633,139.718945455063,12.3670488504726));
#82940=CARTESIAN_POINT('Ctrl Pts',(6.06622557742651,139.7296815297,12.3754215809716));
#82941=CARTESIAN_POINT('Ctrl Pts',(6.06853559039883,139.756004406844,12.3966940316266));
#82942=CARTESIAN_POINT('Ctrl Pts',(6.06993243201465,139.771407984662,12.4098123969246));
#82943=CARTESIAN_POINT('Ctrl Pts',(6.07643963134985,139.840781980793,12.4720474844551));
#82944=CARTESIAN_POINT('Ctrl Pts',(6.08173647831567,139.890444298323,12.5257096608265));
#82945=CARTESIAN_POINT('Ctrl Pts',(6.09202481613722,139.975699416828,12.6369592013763));
#82946=CARTESIAN_POINT('Ctrl Pts',(6.09698564163917,140.011943350347,12.6937125725571));
#82947=CARTESIAN_POINT('Ctrl Pts',(6.10270897611318,140.049534863066,12.7654339929871));
#82948=CARTESIAN_POINT('Ctrl Pts',(6.10367162538994,140.055706518563,12.7777280091128));
#82949=CARTESIAN_POINT('Ctrl Pts',(6.1051783486569,140.065144686429,12.7973802763873));
#82950=CARTESIAN_POINT('Ctrl Pts',(6.10573024972679,140.06855339559,12.8046683534998));
#82951=CARTESIAN_POINT('Ctrl Pts',(6.10681154309127,140.075140461854,12.8191365156545));
#82952=CARTESIAN_POINT('Ctrl Pts',(6.10734107359761,140.078322190201,12.8263144888929));
#82953=CARTESIAN_POINT('Ctrl Pts',(6.10873289475328,140.086559034315,12.8454099734943));
#82954=CARTESIAN_POINT('Ctrl Pts',(6.10958814465885,140.091490042094,12.8573803553823));
#82955=CARTESIAN_POINT('Ctrl Pts',(6.11149963342392,140.102181672413,12.8846010537757));
#82956=CARTESIAN_POINT('Ctrl Pts',(6.11255034177036,140.107825143979,12.8998947298897));
#82957=CARTESIAN_POINT('Ctrl Pts',(6.1160336449756,140.125657726872,12.9514944258997));
#82958=CARTESIAN_POINT('Ctrl Pts',(6.11841633888561,140.136394045716,12.9882783405537));
#82959=CARTESIAN_POINT('Ctrl Pts',(6.12619450308222,140.165688472636,13.1105157674858));
#82960=CARTESIAN_POINT('Ctrl Pts',(6.13153281417446,140.176531747214,13.1975040863691));
#82961=CARTESIAN_POINT('Ctrl Pts',(6.13849101411962,140.177912996264,13.3051464559415));
#82962=CARTESIAN_POINT('Ctrl Pts',(6.13981462610736,140.177650175574,13.3254066310971));
#82963=CARTESIAN_POINT('Ctrl Pts',(6.14196154838472,140.176391992006,13.3578435269128));
#82964=CARTESIAN_POINT('Ctrl Pts',(6.14277439314997,140.175729490964,13.37002954761));
#82965=CARTESIAN_POINT('Ctrl Pts',(6.144491614268,140.173943284059,13.3955588173051));
#82966=CARTESIAN_POINT('Ctrl Pts',(6.14539708349905,140.172781149451,13.4088975269846));
#82967=CARTESIAN_POINT('Ctrl Pts',(6.14762574436898,140.169388815348,13.4414124868713));
#82968=CARTESIAN_POINT('Ctrl Pts',(6.14895641344086,140.166914101173,13.4605586998893));
#82969=CARTESIAN_POINT('Ctrl Pts',(6.15546449213715,140.152668980707,13.552862208939));
#82970=CARTESIAN_POINT('Ctrl Pts',(6.16083926999172,140.134484603582,13.6248482794014));
#82971=CARTESIAN_POINT('Ctrl Pts',(6.1712657504787,140.08689667474,13.758658557791));
#82972=CARTESIAN_POINT('Ctrl Pts',(6.17628455711596,140.058629469,13.8205929803066));
#82973=CARTESIAN_POINT('Ctrl Pts',(6.18205739065044,140.018429411803,13.8916793828944));
#82974=CARTESIAN_POINT('Ctrl Pts',(6.18301687708695,140.011473709464,13.9034931109229));
#82975=CARTESIAN_POINT('Ctrl Pts',(6.18451858419541,140.000125392176,13.9220197219643));
#82976=CARTESIAN_POINT('Ctrl Pts',(6.18506860854523,139.99586795791,13.928813450086));
#82977=CARTESIAN_POINT('Ctrl Pts',(6.18615345272547,139.987262114329,13.9422394104626));
#82978=CARTESIAN_POINT('Ctrl Pts',(6.18668835008692,139.982915440471,13.9488722438488));
#82979=CARTESIAN_POINT('Ctrl Pts',(6.18809594195657,139.971212033487,13.9663436236591));
#82980=CARTESIAN_POINT('Ctrl Pts',(6.18896148509673,139.96374069779,13.9771045277775));
#82981=CARTESIAN_POINT('Ctrl Pts',(6.1908979520067,139.946442957386,14.0011517491167));
#82982=CARTESIAN_POINT('Ctrl Pts',(6.19196323820623,139.93651324492,14.0143605836771));
#82983=CARTESIAN_POINT('Ctrl Pts',(6.19551184805883,139.902173847614,14.0580927311291));
#82984=CARTESIAN_POINT('Ctrl Pts',(6.19794411082411,139.876522923783,14.0876104242493));
#82985=CARTESIAN_POINT('Ctrl Pts',(6.20565321818898,139.790303402123,14.1773863973868));
#82986=CARTESIAN_POINT('Ctrl Pts',(6.21088197070647,139.724640383652,14.2323524911233));
#82987=CARTESIAN_POINT('Ctrl Pts',(6.21773137317214,139.636502016156,14.2911525821974));
#82988=CARTESIAN_POINT('Ctrl Pts',(6.21907557877539,139.619093728675,14.3021183215479));
#82989=CARTESIAN_POINT('Ctrl Pts',(6.22125317388596,139.590790530953,14.3189279199268));
#82990=CARTESIAN_POINT('Ctrl Pts',(6.2220758493248,139.5800748715,14.3250661839411));
#82991=CARTESIAN_POINT('Ctrl Pts',(6.22381244859305,139.557422870829,14.3375730299381));
#82992=CARTESIAN_POINT('Ctrl Pts',(6.22472745425368,139.545469413245,14.3439066731371));
#82993=CARTESIAN_POINT('Ctrl Pts',(6.22697818111198,139.516039678553,14.3588567897391));
#82994=CARTESIAN_POINT('Ctrl Pts',(6.22832141127089,139.498454098391,14.3672479020036));
#82995=CARTESIAN_POINT('Ctrl Pts',(6.23126341524257,139.459914175857,14.3844772403081));
#82996=CARTESIAN_POINT('Ctrl Pts',(6.23286681494723,139.438895909499,14.3931524135736));
#82997=CARTESIAN_POINT('Ctrl Pts',(6.23787848328468,139.373146103655,14.4180883670959));
#82998=CARTESIAN_POINT('Ctrl Pts',(6.24134087382142,139.327673173329,14.4322496142402));
#82999=CARTESIAN_POINT('Ctrl Pts',(6.25008232148965,139.211863221704,14.4607531885076));
#83000=CARTESIAN_POINT('Ctrl Pts',(6.25538087482368,139.140831027734,14.4714956345091));
#83001=CARTESIAN_POINT('Ctrl Pts',(6.26139339108035,139.055800987709,14.4765045931462));
#83002=CARTESIAN_POINT('Ctrl Pts',(6.26233584792604,139.042329668211,14.4770662877853));
#83003=CARTESIAN_POINT('Ctrl Pts',(6.26382162079893,139.020819220759,14.4775933807646));
#83004=CARTESIAN_POINT('Ctrl Pts',(6.2643722898191,139.012785277379,14.4777080111588));
#83005=CARTESIAN_POINT('Ctrl Pts',(6.26547263791033,138.996595007922,14.4777733143393));
#83006=CARTESIAN_POINT('Ctrl Pts',(6.26602218910655,138.98843919673,14.4777215000115));
#83007=CARTESIAN_POINT('Ctrl Pts',(6.26749412076351,138.966427977915,14.4773529771649));
#83008=CARTESIAN_POINT('Ctrl Pts',(6.26840842260547,138.952576110722,14.4768764288358));
#83009=CARTESIAN_POINT('Ctrl Pts',(6.27229242752807,138.893139300363,14.4737804212127));
#83010=CARTESIAN_POINT('Ctrl Pts',(6.27516254570757,138.847715446294,14.4687557134296));
#83011=CARTESIAN_POINT('Ctrl Pts',(6.28386509981517,138.709938874972,14.445343439677));
#83012=CARTESIAN_POINT('Ctrl Pts',(6.28960799220818,138.619414917274,14.4185261274396));
#83013=CARTESIAN_POINT('Ctrl Pts',(6.29694413515152,138.515680411153,14.3737259717958));
#83014=CARTESIAN_POINT('Ctrl Pts',(6.29818458587999,138.498497570866,14.365808695567));
#83015=CARTESIAN_POINT('Ctrl Pts',(6.30033228925,138.469417692123,14.3515507408203));
#83016=CARTESIAN_POINT('Ctrl Pts',(6.30123250840675,138.45742488312,14.3454132021188));
#83017=CARTESIAN_POINT('Ctrl Pts',(6.30310052824236,138.432959625793,14.3323582806929));
#83018=CARTESIAN_POINT('Ctrl Pts',(6.30406904216647,138.420502321822,14.325417386115));
#83019=CARTESIAN_POINT('Ctrl Pts',(6.30664165626679,138.388026725982,14.3065420210254));
#83020=CARTESIAN_POINT('Ctrl Pts',(6.30825873548165,138.368232218685,14.2942371275064));
#83021=CARTESIAN_POINT('Ctrl Pts',(6.31401487686354,138.299965394141,14.2489382771781));
#83022=CARTESIAN_POINT('Ctrl Pts',(6.3182578918509,138.253608771117,14.2129243242085));
#83023=CARTESIAN_POINT('Ctrl Pts',(6.32721731896174,138.162912781018,14.1309224802077));
#83024=CARTESIAN_POINT('Ctrl Pts',(6.33192829751966,138.119239112282,14.0844794201302));
#83025=CARTESIAN_POINT('Ctrl Pts',(6.33649999999999,138.079525356866,14.0347254547424));
#83026=CARTESIAN_POINT('',(6.3365,139.383133178262,14.4136893777957));
#83027=CARTESIAN_POINT('Origin',(6.3365,139.,13.3));
#83028=CARTESIAN_POINT('Ctrl Pts',(6.33649999999995,139.383133178262,14.4136893777957));
#83029=CARTESIAN_POINT('Ctrl Pts',(6.33587794040813,139.39183892307,14.4106944137203));
#83030=CARTESIAN_POINT('Ctrl Pts',(6.33526140785785,139.400500155674,14.4076007669009));
#83031=CARTESIAN_POINT('Ctrl Pts',(6.33378043727113,139.42136007669,14.3998730575355));
#83032=CARTESIAN_POINT('Ctrl Pts',(6.33292104407913,139.433510703543,14.3951408829234));
#83033=CARTESIAN_POINT('Ctrl Pts',(6.32882557181164,139.491493715694,14.371442544551));
#83034=CARTESIAN_POINT('Ctrl Pts',(6.32568526225882,139.536179075507,14.3497942400076));
#83035=CARTESIAN_POINT('Ctrl Pts',(6.318988600977,139.628593333067,14.2975781068897));
#83036=CARTESIAN_POINT('Ctrl Pts',(6.31544253077134,139.675749179254,14.2662579152729));
#83037=CARTESIAN_POINT('Ctrl Pts',(6.30987331788833,139.744370761575,14.2131921608729));
#83038=CARTESIAN_POINT('Ctrl Pts',(6.30791276280052,139.767547955054,14.1937995801075));
#83039=CARTESIAN_POINT('Ctrl Pts',(6.30484934575064,139.802011204962,14.162633990819));
#83040=CARTESIAN_POINT('Ctrl Pts',(6.30376892420992,139.81384200014,14.1514813766365));
#83041=CARTESIAN_POINT('Ctrl Pts',(6.30170981439692,139.835747906835,14.1299574825064));
#83042=CARTESIAN_POINT('Ctrl Pts',(6.30073331251273,139.845870329287,14.1196385441256));
#83043=CARTESIAN_POINT('Ctrl Pts',(6.29847275148654,139.868675127387,14.0955185719317));
#83044=CARTESIAN_POINT('Ctrl Pts',(6.29718369276969,139.881222804303,14.0815961731514));
#83045=CARTESIAN_POINT('Ctrl Pts',(6.29280036627322,139.922325179097,14.0337422456227));
#83046=CARTESIAN_POINT('Ctrl Pts',(6.28964809556392,139.949291733903,13.9985025433935));
#83047=CARTESIAN_POINT('Ctrl Pts',(6.2803038503246,140.021832340654,13.8917237514861));
#83048=CARTESIAN_POINT('Ctrl Pts',(6.2739700929141,140.061751209004,13.8166825090063));
#83049=CARTESIAN_POINT('Ctrl Pts',(6.26516849211967,140.106506857402,13.7049750073844));
#83050=CARTESIAN_POINT('Ctrl Pts',(6.2625966176464,140.118242129848,13.6713451527501));
#83051=CARTESIAN_POINT('Ctrl Pts',(6.25930437465062,140.13165283657,13.6264706348102));
#83052=CARTESIAN_POINT('Ctrl Pts',(6.25852192277366,140.134714976903,13.61566305327));
#83053=CARTESIAN_POINT('Ctrl Pts',(6.25722804877182,140.139574209788,13.5975274275939));
#83054=CARTESIAN_POINT('Ctrl Pts',(6.25671206725283,140.141456306223,13.5902231235643));
#83055=CARTESIAN_POINT('Ctrl Pts',(6.25563622157122,140.145264962526,13.5748314592414));
#83056=CARTESIAN_POINT('Ctrl Pts',(6.25507724415385,140.14717632589,13.566740798136));
#83057=CARTESIAN_POINT('Ctrl Pts',(6.25346529163954,140.152483708809,13.5431619907188));
#83058=CARTESIAN_POINT('Ctrl Pts',(6.25242437088168,140.155652981513,13.5276240325921));
#83059=CARTESIAN_POINT('Ctrl Pts',(6.24664106555966,140.171710079176,13.4398881854822));
#83060=CARTESIAN_POINT('Ctrl Pts',(6.24216368030448,140.178147377323,13.3666666991411));
#83061=CARTESIAN_POINT('Ctrl Pts',(6.23367171165806,140.177367646384,13.2292952048428));
#83062=CARTESIAN_POINT('Ctrl Pts',(6.22968485762245,140.171785098228,13.1654188036648));
#83063=CARTESIAN_POINT('Ctrl Pts',(6.22434810456065,140.157970918278,13.0842849758959));
#83064=CARTESIAN_POINT('Ctrl Pts',(6.22315005479749,140.154481336154,13.0663284299189));
#83065=CARTESIAN_POINT('Ctrl Pts',(6.22108935133543,140.147837752813,13.0359397092644));
#83066=CARTESIAN_POINT('Ctrl Pts',(6.22023375211713,140.14489618224,13.0234641920897));
#83067=CARTESIAN_POINT('Ctrl Pts',(6.21847475026451,140.138482613059,12.9981226466729));
#83068=CARTESIAN_POINT('Ctrl Pts',(6.2175709263667,140.134994692483,12.9852626200945));
#83069=CARTESIAN_POINT('Ctrl Pts',(6.21522089935695,140.125438827419,12.9522571413018));
#83070=CARTESIAN_POINT('Ctrl Pts',(6.2137640401135,140.119048149415,12.9322109495601));
#83071=CARTESIAN_POINT('Ctrl Pts',(6.20542411609103,140.079883470612,12.8198525194929));
#83072=CARTESIAN_POINT('Ctrl Pts',(6.19816376487795,140.03623399904,12.7317555443674));
#83073=CARTESIAN_POINT('Ctrl Pts',(6.18729018849101,139.954915097848,12.608857867791));
#83074=CARTESIAN_POINT('Ctrl Pts',(6.18367046043542,139.925054842858,12.5693736222591));
#83075=CARTESIAN_POINT('Ctrl Pts',(6.17936549517341,139.885210100701,12.5230614720746));
#83076=CARTESIAN_POINT('Ctrl Pts',(6.17855351202164,139.877492241763,12.5143551744783));
#83077=CARTESIAN_POINT('Ctrl Pts',(6.17724071745705,139.864659934817,12.5003044754389));
#83078=CARTESIAN_POINT('Ctrl Pts',(6.17673445690185,139.859622224225,12.4948916978854));
#83079=CARTESIAN_POINT('Ctrl Pts',(6.17568476850692,139.848986849656,12.4836781540236));
#83080=CARTESIAN_POINT('Ctrl Pts',(6.17514201853855,139.843380189957,12.4778869348197));
#83081=CARTESIAN_POINT('Ctrl Pts',(6.17366403807553,139.827830937322,12.4621523369892));
#83082=CARTESIAN_POINT('Ctrl Pts',(6.17273751171188,139.817768713229,12.4523283996942));
#83083=CARTESIAN_POINT('Ctrl Pts',(6.16786670119043,139.763349017796,12.401068657847));
#83084=CARTESIAN_POINT('Ctrl Pts',(6.16410924810126,139.716009098028,12.3629237241216));
#83085=CARTESIAN_POINT('Ctrl Pts',(6.15698739044969,139.620939412451,12.2977498813693));
#83086=CARTESIAN_POINT('Ctrl Pts',(6.15363002542191,139.573857077063,12.2700685817626));
#83087=CARTESIAN_POINT('Ctrl Pts',(6.14864347910845,139.503146395696,12.2348538474898));
#83088=CARTESIAN_POINT('Ctrl Pts',(6.14708496247102,139.480931893025,12.2246409792109));
#83089=CARTESIAN_POINT('Ctrl Pts',(6.14417688147737,139.439480426757,12.207125521602));
#83090=CARTESIAN_POINT('Ctrl Pts',(6.14283403650462,139.420338883423,12.1996215143352));
#83091=CARTESIAN_POINT('Ctrl Pts',(6.14056946290329,139.388140348323,12.1879615434827));
#83092=CARTESIAN_POINT('Ctrl Pts',(6.13965710046634,139.375189223157,12.1835254238978));
#83093=CARTESIAN_POINT('Ctrl Pts',(6.13781463795178,139.349098664167,12.1750939060503));
#83094=CARTESIAN_POINT('Ctrl Pts',(6.13688463648514,139.33596082673,12.1711005833429));
#83095=CARTESIAN_POINT('Ctrl Pts',(6.13452672103908,139.302749010543,12.161636741288));
#83096=CARTESIAN_POINT('Ctrl Pts',(6.13308952080128,139.282595000403,12.1564669468993));
#83097=CARTESIAN_POINT('Ctrl Pts',(6.12611070324,139.185209126124,12.1342176891967));
#83098=CARTESIAN_POINT('Ctrl Pts',(6.12035125975786,139.106535278959,12.1244161565));
#83099=CARTESIAN_POINT('Ctrl Pts',(6.11037352358319,138.97033370826,12.1212365702705));
#83100=CARTESIAN_POINT('Ctrl Pts',(6.10618894148885,138.913154572245,12.1240653671204));
#83101=CARTESIAN_POINT('Ctrl Pts',(6.10120983535162,138.843082076121,12.1326731580598));
#83102=CARTESIAN_POINT('Ctrl Pts',(6.10027221132328,138.829789255615,12.1345372031516));
#83103=CARTESIAN_POINT('Ctrl Pts',(6.09879126409641,138.808594429436,12.1378797316031));
#83104=CARTESIAN_POINT('Ctrl Pts',(6.09824079294063,138.80067104579,12.1392125137941));
#83105=CARTESIAN_POINT('Ctrl Pts',(6.09714820740042,138.78484146926,12.1420420549567));
#83106=CARTESIAN_POINT('Ctrl Pts',(6.09660616383184,138.776935779286,12.1435389513021));
#83107=CARTESIAN_POINT('Ctrl Pts',(6.09515253223934,138.755613655991,12.1478029614718));
#83108=CARTESIAN_POINT('Ctrl Pts',(6.09424892139357,138.742228675843,12.1507234080612));
#83109=CARTESIAN_POINT('Ctrl Pts',(6.0888727288714,138.662042145758,12.1696906621856));
#83110=CARTESIAN_POINT('Ctrl Pts',(6.08464196497185,138.596690819988,12.1913257080514));
#83111=CARTESIAN_POINT('Ctrl Pts',(6.07599618407227,138.468326522112,12.246686028101));
#83112=CARTESIAN_POINT('Ctrl Pts',(6.07159376738645,138.405749282804,12.2806807813327));
#83113=CARTESIAN_POINT('Ctrl Pts',(6.0656847280062,138.329749861848,12.3313560979192));
#83114=CARTESIAN_POINT('Ctrl Pts',(6.06435902184899,138.313172757481,12.3430389158782));
#83115=CARTESIAN_POINT('Ctrl Pts',(6.06211712410808,138.285993203161,12.363263966436));
#83116=CARTESIAN_POINT('Ctrl Pts',(6.06120994534497,138.275222078557,12.3715728132982));
#83117=CARTESIAN_POINT('Ctrl Pts',(6.05937326178053,138.253885178608,12.3886296973627));
#83118=CARTESIAN_POINT('Ctrl Pts',(6.05844377825641,138.243323523094,12.397379461259));
#83119=CARTESIAN_POINT('Ctrl Pts',(6.05607937311395,138.21706407043,12.4199188189206));
#83120=CARTESIAN_POINT('Ctrl Pts',(6.05463493662559,138.201576527818,12.4339449107868));
#83121=CARTESIAN_POINT('Ctrl Pts',(6.04743259840784,138.127101750642,12.5050881606315));
#83122=CARTESIAN_POINT('Ctrl Pts',(6.04143480755699,138.073834723535,12.5678457268086));
#83123=CARTESIAN_POINT('Ctrl Pts',(6.03112116172141,137.994628320282,12.6837814662704));
#83124=CARTESIAN_POINT('Ctrl Pts',(6.02684136351919,137.965344031437,12.7343271797954));
#83125=CARTESIAN_POINT('Ctrl Pts',(6.02181025751106,137.934265838573,12.7985277616593));
#83126=CARTESIAN_POINT('Ctrl Pts',(6.02090293458051,137.928800917957,12.8103100262251));
#83127=CARTESIAN_POINT('Ctrl Pts',(6.01946269897096,137.920336708624,12.8293788583717));
#83128=CARTESIAN_POINT('Ctrl Pts',(6.01892303046263,137.917213847464,12.8366089786531));
#83129=CARTESIAN_POINT('Ctrl Pts',(6.01784651703916,137.911078749687,12.851213837669));
#83130=CARTESIAN_POINT('Ctrl Pts',(6.01730980898099,137.908068336218,12.8585888996861));
#83131=CARTESIAN_POINT('Ctrl Pts',(6.0158674917216,137.900118689835,12.8786434851459));
#83132=CARTESIAN_POINT('Ctrl Pts',(6.01496990071557,137.895323824892,12.8913793976777));
#83133=CARTESIAN_POINT('Ctrl Pts',(6.00956463698503,137.867479259642,12.9694144516724));
#83134=CARTESIAN_POINT('Ctrl Pts',(6.00530681642411,137.850002139698,13.0365662976106));
#83135=CARTESIAN_POINT('Ctrl Pts',(5.9979945997241,137.830389763774,13.153306239501));
#83136=CARTESIAN_POINT('Ctrl Pts',(5.99495875092827,137.825290680581,13.2022002515034));
#83137=CARTESIAN_POINT('Ctrl Pts',(5.99039335744201,137.822305560256,13.2742816498389));
#83138=CARTESIAN_POINT('Ctrl Pts',(5.98892135908821,137.822027871612,13.2973177590696));
#83139=CARTESIAN_POINT('Ctrl Pts',(5.98616117183293,137.822764447314,13.3399484609698));
#83140=CARTESIAN_POINT('Ctrl Pts',(5.98487869485107,137.823592522017,13.359538215335));
#83141=CARTESIAN_POINT('Ctrl Pts',(5.98269547525246,137.82580757907,13.3924457060391));
#83142=CARTESIAN_POINT('Ctrl Pts',(5.98180301197179,137.82693343009,13.4057773481816));
#83143=CARTESIAN_POINT('Ctrl Pts',(5.97998507793252,137.829666723415,13.4326707298876));
#83144=CARTESIAN_POINT('Ctrl Pts',(5.97905944708958,137.831283427442,13.4462294306781));
#83145=CARTESIAN_POINT('Ctrl Pts',(5.97668281431759,137.836000444955,13.4806826231297));
#83146=CARTESIAN_POINT('Ctrl Pts',(5.97522176016338,137.839427690418,13.5015266432647));
#83147=CARTESIAN_POINT('Ctrl Pts',(5.96986450289777,137.853874809079,13.5767038446651));
#83148=CARTESIAN_POINT('Ctrl Pts',(5.96587313711761,137.868160088882,13.6303007970922));
#83149=CARTESIAN_POINT('Ctrl Pts',(5.96182583603505,137.88614821265,13.6826607614027));
#83150=CARTESIAN_POINT('Origin',(4.2,139.,13.3));
#83151=CARTESIAN_POINT('',(6.33581728267915,139.984084034254,12.216529393001));
#83152=CARTESIAN_POINT('Ctrl Pts',(6.1539436045687,137.5365,13.30000001305));
#83153=CARTESIAN_POINT('Ctrl Pts',(6.1554786574661,137.536499999732,13.2699840581504));
#83154=CARTESIAN_POINT('Ctrl Pts',(6.15698912438489,137.537423421588,13.2399696452689));
#83155=CARTESIAN_POINT('Ctrl Pts',(6.16301247270492,137.544873150686,13.1190592179742));
#83156=CARTESIAN_POINT('Ctrl Pts',(6.16735318751567,137.558955974813,13.0288441755545));
#83157=CARTESIAN_POINT('Ctrl Pts',(6.17441326870151,137.594203252006,12.8897411341594));
#83158=CARTESIAN_POINT('Ctrl Pts',(6.17703614862449,137.609787875827,12.8396890894236));
#83159=CARTESIAN_POINT('Ctrl Pts',(6.18046202158408,137.632490066651,12.7785465162853));
#83160=CARTESIAN_POINT('Ctrl Pts',(6.18114415247651,137.637118028538,12.7665678460758));
#83161=CARTESIAN_POINT('Ctrl Pts',(6.18225778792567,137.644829249767,12.7473643497358));
#83162=CARTESIAN_POINT('Ctrl Pts',(6.18268371592634,137.647814198765,12.7401004747614));
#83163=CARTESIAN_POINT('Ctrl Pts',(6.18354056333019,137.653885016315,12.7256588648311));
#83164=CARTESIAN_POINT('Ctrl Pts',(6.1839714168684,137.656970178306,12.7184811429848));
#83165=CARTESIAN_POINT('Ctrl Pts',(6.18509851049286,137.665129330271,12.6999099235027));
#83166=CARTESIAN_POINT('Ctrl Pts',(6.18579971501334,137.670291667982,12.6885561879562));
#83167=CARTESIAN_POINT('Ctrl Pts',(6.18925072263128,137.696149901868,12.633561726867));
#83168=CARTESIAN_POINT('Ctrl Pts',(6.19209590039935,137.718851069005,12.5909007773802));
#83169=CARTESIAN_POINT('Ctrl Pts',(6.19857832719303,137.77451708012,12.4977194534767));
#83170=CARTESIAN_POINT('Ctrl Pts',(6.20222981230084,137.808581485361,12.4479528045884));
#83171=CARTESIAN_POINT('Ctrl Pts',(6.2105982694274,137.894424984897,12.3377934616047));
#83172=CARTESIAN_POINT('Ctrl Pts',(6.21526610569149,137.948255083061,12.2792291732169));
#83173=CARTESIAN_POINT('Ctrl Pts',(6.22091590879112,138.021923785183,12.211130919032));
#83174=CARTESIAN_POINT('Ctrl Pts',(6.22207936157765,138.037571949193,12.1972755249741));
#83175=CARTESIAN_POINT('Ctrl Pts',(6.22398660281612,138.064015143859,12.1748536864594));
#83176=CARTESIAN_POINT('Ctrl Pts',(6.22473809064365,138.074643620022,12.1660963595008));
#83177=CARTESIAN_POINT('Ctrl Pts',(6.22621473616527,138.095938219664,12.1490495390382));
#83178=CARTESIAN_POINT('Ctrl Pts',(6.22694004981319,138.106598630742,12.1407551266783));
#83179=CARTESIAN_POINT('Ctrl Pts',(6.22869876679474,138.132928346004,12.1208480569078));
#83180=CARTESIAN_POINT('Ctrl Pts',(6.22972583123008,138.148718081361,12.1093985972315));
#83181=CARTESIAN_POINT('Ctrl Pts',(6.2338556578144,138.213811823827,12.0641549984346));
#83182=CARTESIAN_POINT('Ctrl Pts',(6.23685873488663,138.264937137236,12.0330792284287));
#83183=CARTESIAN_POINT('Ctrl Pts',(6.24271668789267,138.370046182637,11.9777009997802));
#83184=CARTESIAN_POINT('Ctrl Pts',(6.24556792817733,138.423885940875,11.9533711964888));
#83185=CARTESIAN_POINT('Ctrl Pts',(6.25158895180208,138.539193975956,11.9094488321205));
#83186=CARTESIAN_POINT('Ctrl Pts',(6.25475813478067,138.600781412457,11.8905327782686));
#83187=CARTESIAN_POINT('Ctrl Pts',(6.25894564638718,138.679168607552,11.8720077897916));
#83188=CARTESIAN_POINT('Ctrl Pts',(6.25979860346928,138.694989784608,11.8685450543358));
#83189=CARTESIAN_POINT('Ctrl Pts',(6.26113117679804,138.71940425859,11.8636246419722));
#83190=CARTESIAN_POINT('Ctrl Pts',(6.26160116768587,138.727958979957,11.8619798975694));
#83191=CARTESIAN_POINT('Ctrl Pts',(6.26248606736094,138.743946714965,11.8590538346815));
#83192=CARTESIAN_POINT('Ctrl Pts',(6.26289995063702,138.75137574914,11.8577534507989));
#83193=CARTESIAN_POINT('Ctrl Pts',(6.26390376041198,138.769284295069,11.8547611980756));
#83194=CARTESIAN_POINT('Ctrl Pts',(6.26449662373628,138.779772705817,11.8531258324743));
#83195=CARTESIAN_POINT('Ctrl Pts',(6.26666758929046,138.817901695638,11.8476048940681));
#83196=CARTESIAN_POINT('Ctrl Pts',(6.26827632551352,138.845632915376,11.8443963614928));
#83197=CARTESIAN_POINT('Ctrl Pts',(6.27268950693175,138.920828653854,11.8378690112076));
#83198=CARTESIAN_POINT('Ctrl Pts',(6.27553469976765,138.968390696068,11.8360684402671));
#83199=CARTESIAN_POINT('Ctrl Pts',(6.28488460824947,139.124206895131,11.8377671044424));
#83200=CARTESIAN_POINT('Ctrl Pts',(6.29136819594589,139.232011520982,11.8509556525554));
#83201=CARTESIAN_POINT('Ctrl Pts',(6.29877276116309,139.359532179131,11.8811670544271));
#83202=CARTESIAN_POINT('Ctrl Pts',(6.30004325818092,139.38155552074,11.8869303695283));
#83203=CARTESIAN_POINT('Ctrl Pts',(6.30207853915382,139.417059412984,11.8971120691932));
#83204=CARTESIAN_POINT('Ctrl Pts',(6.3028531305527,139.43062531054,11.9012166136492));
#83205=CARTESIAN_POINT('Ctrl Pts',(6.30434486547773,139.456846794755,11.9095679150505));
#83206=CARTESIAN_POINT('Ctrl Pts',(6.30506265447024,139.469508073344,11.9137920206932));
#83207=CARTESIAN_POINT('Ctrl Pts',(6.30675423957324,139.499437623015,11.9242343577401));
#83208=CARTESIAN_POINT('Ctrl Pts',(6.30772293539835,139.516650382419,11.9306054389544));
#83209=CARTESIAN_POINT('Ctrl Pts',(6.31119487038767,139.578533603564,11.954843698852));
#83210=CARTESIAN_POINT('Ctrl Pts',(6.31363640017759,139.622437722751,11.974587443636));
#83211=CARTESIAN_POINT('Ctrl Pts',(6.32248788948386,139.780818738265,12.0554209057177));
#83212=CARTESIAN_POINT('Ctrl Pts',(6.3285183382369,139.887978107783,12.1294691105776));
#83213=CARTESIAN_POINT('Ctrl Pts',(6.33515505794404,139.983968635079,12.2166542679363));
#83214=CARTESIAN_POINT('',(6.3365,138.768242272558,11.854966918797));
#83215=CARTESIAN_POINT('Origin',(6.3365,139.,13.3));
#83216=CARTESIAN_POINT('Ctrl Pts',(6.3365,138.768242272558,11.854966918797));
#83217=CARTESIAN_POINT('Ctrl Pts',(6.333427091055,138.712441868313,11.8639163159052));
#83218=CARTESIAN_POINT('Ctrl Pts',(6.33035418211001,138.657111795352,11.8761099408742));
#83219=CARTESIAN_POINT('Ctrl Pts',(6.32728127316501,138.602642967625,11.8914760780085));
#83220=CARTESIAN_POINT('Ctrl Pts',(6.32421010161006,138.548204935994,11.9068335272924));
#83221=CARTESIAN_POINT('Ctrl Pts',(6.3211389300551,138.494627660216,11.9253597967244));
#83222=CARTESIAN_POINT('Ctrl Pts',(6.31806775850014,138.442289751673,11.9469325482774));
#83223=CARTESIAN_POINT('Ctrl Pts',(6.31499745988565,138.389966719498,11.9684991680571));
#83224=CARTESIAN_POINT('Ctrl Pts',(6.31192716127116,138.338882813531,11.9931103620133));
#83225=CARTESIAN_POINT('Ctrl Pts',(6.30885686265668,138.289397569585,12.0205952806525));
#83226=CARTESIAN_POINT('Ctrl Pts',(6.30578645390265,138.239910550476,12.0480811852466));
#83227=CARTESIAN_POINT('Ctrl Pts',(6.30271604514863,138.192022740535,12.0784407778119));
#83228=CARTESIAN_POINT('Ctrl Pts',(6.2996456363946,138.146068226617,12.1114577094582));
#83229=CARTESIAN_POINT('Ctrl Pts',(6.29657413458961,138.100097353109,12.1444863949758));
#83230=CARTESIAN_POINT('Ctrl Pts',(6.29350263278462,138.056061544296,12.1801740077873));
#83231=CARTESIAN_POINT('Ctrl Pts',(6.29043113097963,138.014263541637,12.2182625620544));
#83232=CARTESIAN_POINT('Ctrl Pts',(6.2873549864972,137.972402359902,12.2564086884418));
#83233=CARTESIAN_POINT('Ctrl Pts',(6.28427884201478,137.932786103428,12.2969626653084));
#83234=CARTESIAN_POINT('Ctrl Pts',(6.28120269753236,137.895681512845,12.3396287546333));
#83235=CARTESIAN_POINT('Ctrl Pts',(6.27812408406556,137.858547141263,12.3823290887437));
#83236=CARTESIAN_POINT('Ctrl Pts',(6.27504547059876,137.823928754659,12.4271445193177));
#83237=CARTESIAN_POINT('Ctrl Pts',(6.27196685713195,137.792051561807,12.4737477257723));
#83238=CARTESIAN_POINT('Ctrl Pts',(6.2688817646213,137.760107282348,12.5204490102162));
#83239=CARTESIAN_POINT('Ctrl Pts',(6.26579667211064,137.730915976882,12.5689451607239));
#83240=CARTESIAN_POINT('Ctrl Pts',(6.26271157959998,137.704658045929,12.6188821893213));
#83241=CARTESIAN_POINT('Ctrl Pts',(6.26089118497487,137.68916424916,12.6483481123491));
#83242=CARTESIAN_POINT('Ctrl Pts',(6.25907079034975,137.674690878593,12.6783152763757));
#83243=CARTESIAN_POINT('Ctrl Pts',(6.25725039572463,137.661267039855,12.7087079305276));
#83244=CARTESIAN_POINT('Ctrl Pts',(6.25400139029006,137.637308429776,12.7629521571078));
#83245=CARTESIAN_POINT('Ctrl Pts',(6.2507523848555,137.616608298453,12.8187501037437));
#83246=CARTESIAN_POINT('Ctrl Pts',(6.24750337942093,137.599354462676,12.8757072605205));
#83247=CARTESIAN_POINT('Ctrl Pts',(6.24426477152369,137.582155842998,12.9324821417746));
#83248=CARTESIAN_POINT('Ctrl Pts',(6.24102616362645,137.568381705114,12.9904084882188));
#83249=CARTESIAN_POINT('Ctrl Pts',(6.23778755572921,137.558172270461,13.0490716270891));
#83250=CARTESIAN_POINT('Ctrl Pts',(6.23456397913116,137.548010220693,13.1074624936685));
#83251=CARTESIAN_POINT('Ctrl Pts',(6.23134040253311,137.541380020528,13.1665829659533));
#83252=CARTESIAN_POINT('Ctrl Pts',(6.22811682593506,137.538371771148,13.2260056041077));
#83253=CARTESIAN_POINT('Ctrl Pts',(6.22679639588331,137.537139542671,13.2503460951079));
#83254=CARTESIAN_POINT('Ctrl Pts',(6.22547596583156,137.536514449846,13.2747370999646));
#83255=CARTESIAN_POINT('Ctrl Pts',(6.22415553577981,137.536500247676,13.2991485609046));
#83256=CARTESIAN_POINT('Origin',(6.3365,139.,13.3));
#83257=CARTESIAN_POINT('',(6.3365,140.003135769676,12.2343777040633));
#83258=CARTESIAN_POINT('',(6.3365,137.5365,13.3));
#83259=CARTESIAN_POINT('Origin',(6.3365,139.,13.3));
#83260=CARTESIAN_POINT('Ctrl Pts',(6.33650000000013,140.003135769676,12.2343777040634));
#83261=CARTESIAN_POINT('Ctrl Pts',(6.33650010571933,140.023669124737,12.2575147919222));
#83262=CARTESIAN_POINT('Ctrl Pts',(6.33649999999991,140.043388634716,12.281323949763));
#83263=CARTESIAN_POINT('Ctrl Pts',(6.33649999999995,140.062245685488,12.3057933133457));
#83264=CARTESIAN_POINT('Ctrl Pts',(6.33650000000002,140.097351486145,12.3513474464139));
#83265=CARTESIAN_POINT('Ctrl Pts',(6.33649999999986,140.129470426597,12.3991893725647));
#83266=CARTESIAN_POINT('Ctrl Pts',(6.33649999999998,140.158546998602,12.4489806897978));
#83267=CARTESIAN_POINT('Ctrl Pts',(6.33650000000002,140.168444534924,12.4659294336432));
#83268=CARTESIAN_POINT('Ctrl Pts',(6.33649999999992,140.177989140738,12.4831041762642));
#83269=CARTESIAN_POINT('Ctrl Pts',(6.33649999999992,140.187177335336,12.5004918282147));
#83270=CARTESIAN_POINT('Ctrl Pts',(6.33649999999991,140.193295770393,12.5120702964443));
#83271=CARTESIAN_POINT('Ctrl Pts',(6.33649999999975,140.199256942011,12.5237447867508));
#83272=CARTESIAN_POINT('Ctrl Pts',(6.33649999999976,140.205057168636,12.5355063710712));
#83273=CARTESIAN_POINT('Ctrl Pts',(6.33649999999984,140.230497025639,12.5870928077041));
#83274=CARTESIAN_POINT('Ctrl Pts',(6.3365000000001,140.252774622926,12.6402088612707));
#83275=CARTESIAN_POINT('Ctrl Pts',(6.33650000000003,140.271842328215,12.694511980783));
#83276=CARTESIAN_POINT('Ctrl Pts',(6.33649999999999,140.284881330078,12.7316458920614));
#83277=CARTESIAN_POINT('Ctrl Pts',(6.33649999999986,140.296418268899,12.7693353313234));
#83278=CARTESIAN_POINT('Ctrl Pts',(6.33649999999978,140.306423950697,12.8074719159752));
#83279=CARTESIAN_POINT('Ctrl Pts',(6.33649999999973,140.312377619302,12.8301642813083));
#83280=CARTESIAN_POINT('Ctrl Pts',(6.3365,140.317788915002,12.8530149598051));
#83281=CARTESIAN_POINT('Ctrl Pts',(6.33649999999981,140.322649755792,12.8760008063365));
#83282=CARTESIAN_POINT('Ctrl Pts',(6.33649999999971,140.325116583677,12.8876658926093));
#83283=CARTESIAN_POINT('Ctrl Pts',(6.33649999999987,140.32744178589,12.8993673010087));
#83284=CARTESIAN_POINT('Ctrl Pts',(6.3364999999999,140.329621093748,12.911083574289));
#83285=CARTESIAN_POINT('Ctrl Pts',(6.33650000000003,140.339905172661,12.9663722653945));
#83286=CARTESIAN_POINT('Ctrl Pts',(6.33650000000014,140.346964990818,13.02208316699));
#83287=CARTESIAN_POINT('Ctrl Pts',(6.33649999999991,140.35074615215,13.077899282583));
#83288=CARTESIAN_POINT('Ctrl Pts',(6.33649999999968,140.354434057332,13.1323387851239));
#83289=CARTESIAN_POINT('Ctrl Pts',(6.33650000000022,140.355002858764,13.1868794089901));
#83290=CARTESIAN_POINT('Ctrl Pts',(6.33650000000013,140.352354170508,13.2412187064025));
#83291=CARTESIAN_POINT('Ctrl Pts',(6.33650000000008,140.350787573337,13.2733583096162));
#83292=CARTESIAN_POINT('Ctrl Pts',(6.33650000000018,140.348094513887,13.3054272487336));
#83293=CARTESIAN_POINT('Ctrl Pts',(6.33650000000003,140.344246789072,13.3373593705737));
#83294=CARTESIAN_POINT('Ctrl Pts',(6.33649999999992,140.34158830054,13.3594220657457));
#83295=CARTESIAN_POINT('Ctrl Pts',(6.33650000000016,140.338378479852,13.3814193878785));
#83296=CARTESIAN_POINT('Ctrl Pts',(6.33649999999988,140.334606388925,13.4033284402217));
#83297=CARTESIAN_POINT('Ctrl Pts',(6.33649999999974,140.332808145722,13.413772993446));
#83298=CARTESIAN_POINT('Ctrl Pts',(6.3364999999999,140.330881741628,13.4241986892914));
#83299=CARTESIAN_POINT('Ctrl Pts',(6.33649999999994,140.328829643233,13.4345857047938));
#83300=CARTESIAN_POINT('Ctrl Pts',(6.33650000000012,140.318607036849,13.4863290184844));
#83301=CARTESIAN_POINT('Ctrl Pts',(6.33650000000002,140.305253098095,13.5372133729786));
#83302=CARTESIAN_POINT('Ctrl Pts',(6.3365000000001,140.288686037652,13.5869599067306));
#83303=CARTESIAN_POINT('Ctrl Pts',(6.33650000000012,140.285264455959,13.5972340184094));
#83304=CARTESIAN_POINT('Ctrl Pts',(6.33649999999969,140.281705658798,13.6074595259337));
#83305=CARTESIAN_POINT('Ctrl Pts',(6.33649999999975,140.278008672999,13.617633847654));
#83306=CARTESIAN_POINT('Ctrl Pts',(6.33650000000007,140.258790862416,13.6705223893568));
#83307=CARTESIAN_POINT('Ctrl Pts',(6.33650000000009,140.235842698297,13.7220312770223));
#83308=CARTESIAN_POINT('Ctrl Pts',(6.33650000000012,140.209434727541,13.7718972245888));
#83309=CARTESIAN_POINT('Ctrl Pts',(6.33650000000013,140.198177428881,13.7931542863272));
#83310=CARTESIAN_POINT('Ctrl Pts',(6.33649999999972,140.186290854219,13.8141122491807));
#83311=CARTESIAN_POINT('Ctrl Pts',(6.33649999999995,140.173793812567,13.8347480026074));
#83312=CARTESIAN_POINT('Ctrl Pts',(6.33650000000012,140.164796388131,13.8496050093537));
#83313=CARTESIAN_POINT('Ctrl Pts',(6.33649999999985,140.155482503734,13.8642949643968));
#83314=CARTESIAN_POINT('Ctrl Pts',(6.33649999999996,140.145858880467,13.8788086379537));
#83315=CARTESIAN_POINT('Ctrl Pts',(6.33650000000002,140.140281862567,13.8872195051469));
#83316=CARTESIAN_POINT('Ctrl Pts',(6.3365000000001,140.134605724196,13.8955637071506));
#83317=CARTESIAN_POINT('Ctrl Pts',(6.33650000000005,140.12883463953,13.9038364795333));
#83318=CARTESIAN_POINT('Ctrl Pts',(6.33649999999979,140.098780117204,13.9469192337569));
#83319=CARTESIAN_POINT('Ctrl Pts',(6.33649999999984,140.066133347015,13.9880983065987));
#83320=CARTESIAN_POINT('Ctrl Pts',(6.33649999999986,140.031132767185,14.0271737952641));
#83321=CARTESIAN_POINT('Ctrl Pts',(6.33649999999987,139.996314247044,14.0660460281165));
#83322=CARTESIAN_POINT('Ctrl Pts',(6.33650000000004,139.959165325295,14.1028371364767));
#83323=CARTESIAN_POINT('Ctrl Pts',(6.33650000000007,139.919892602426,14.1373077738618));
#83324=CARTESIAN_POINT('Ctrl Pts',(6.33650000000009,139.90024019132,14.1545571797462));
#83325=CARTESIAN_POINT('Ctrl Pts',(6.33649999999998,139.880055615327,14.1712247927656));
#83326=CARTESIAN_POINT('Ctrl Pts',(6.33650000000002,139.85936328841,14.1872758437228));
#83327=CARTESIAN_POINT('Ctrl Pts',(6.33650000000005,139.844113211276,14.1991053381126));
#83328=CARTESIAN_POINT('Ctrl Pts',(6.3364999999999,139.82858732605,14.2105998760627));
#83329=CARTESIAN_POINT('Ctrl Pts',(6.33649999999999,139.812795253445,14.2217443028877));
#83330=CARTESIAN_POINT('Ctrl Pts',(6.33650000000003,139.805156698168,14.2271348125736));
#83331=CARTESIAN_POINT('Ctrl Pts',(6.33650000000006,139.797456635723,14.2324427334948));
#83332=CARTESIAN_POINT('Ctrl Pts',(6.33650000000006,139.789706961736,14.2376594028882));
#83333=CARTESIAN_POINT('Ctrl Pts',(6.33650000000004,139.747876492251,14.2658174557627));
#83334=CARTESIAN_POINT('Ctrl Pts',(6.33649999999994,139.704520414613,14.2913790256126));
#83335=CARTESIAN_POINT('Ctrl Pts',(6.33649999999996,139.659834778768,14.3141386345366));
#83336=CARTESIAN_POINT('Ctrl Pts',(6.33649999999999,139.616041415194,14.3364437849408));
#83337=CARTESIAN_POINT('Ctrl Pts',(6.33649999999992,139.570970180933,14.3560581029554));
#83338=CARTESIAN_POINT('Ctrl Pts',(6.33649999999999,139.524795264372,14.3727395718669));
#83339=CARTESIAN_POINT('Ctrl Pts',(6.33650000000005,139.47862034781,14.3894210407783));
#83340=CARTESIAN_POINT('Ctrl Pts',(6.33650000000002,139.431340955144,14.4031701381045));
#83341=CARTESIAN_POINT('Ctrl Pts',(6.33649999999999,139.383133178262,14.4136893777957));
#83342=CARTESIAN_POINT('Ctrl Pts',(6.3365,138.079525356882,14.0347254547586));
#83343=CARTESIAN_POINT('Ctrl Pts',(6.3365,137.962361692323,13.9203814964881));
#83344=CARTESIAN_POINT('Ctrl Pts',(6.3364999999999,137.883433374858,13.7925889625522));
#83345=CARTESIAN_POINT('Ctrl Pts',(6.3364999999999,137.767824722722,13.5228369694544));
#83346=CARTESIAN_POINT('Ctrl Pts',(6.3364999999999,137.733244296092,13.3670757711572));
#83347=CARTESIAN_POINT('Ctrl Pts',(6.3364999999999,137.719950578003,13.0662072487722));
#83348=CARTESIAN_POINT('Ctrl Pts',(6.3364999999999,137.736602493462,12.9093813376879));
#83349=CARTESIAN_POINT('Ctrl Pts',(6.3364999999999,137.838995140157,12.6008328994218));
#83350=CARTESIAN_POINT('Ctrl Pts',(6.3364999999999,137.919392261343,12.4595666959715));
#83351=CARTESIAN_POINT('Ctrl Pts',(6.3364999999999,138.114949192507,12.2208706205168));
#83352=CARTESIAN_POINT('Ctrl Pts',(6.3364999999999,138.227112966334,12.1207931450485));
#83353=CARTESIAN_POINT('Ctrl Pts',(6.3364999999999,138.479316622589,11.9564560277444));
#83354=CARTESIAN_POINT('Ctrl Pts',(6.3365,138.620334945868,11.8931959685327));
#83355=CARTESIAN_POINT('Ctrl Pts',(6.3365,138.768242272558,11.854966918797));
#83356=CARTESIAN_POINT('Origin',(6.3365,139.,13.3));
#83357=CARTESIAN_POINT('Ctrl Pts',(1.89724981368824,138.491031839177,14.3596959507936));
#83358=CARTESIAN_POINT('Ctrl Pts',(1.92367413820389,138.139145735096,14.1906964941018));
#83359=CARTESIAN_POINT('Ctrl Pts',(1.97651499747799,137.623293427453,13.4770766030293));
#83360=CARTESIAN_POINT('Ctrl Pts',(2.05577239151056,138.103026646,12.2387996208986));
#83361=CARTESIAN_POINT('Ctrl Pts',(2.13502199578593,139.402779510252,11.971181393986));
#83362=CARTESIAN_POINT('Ctrl Pts',(2.21427160006131,140.334245953224,12.9149808566737));
#83363=CARTESIAN_POINT('Ctrl Pts',(2.29352120433668,140.048621811314,14.2106232938627));
#83364=CARTESIAN_POINT('Ctrl Pts',(2.37277080861206,138.805982047616,14.6750947012087));
#83365=CARTESIAN_POINT('Ctrl Pts',(2.45202041288743,137.740464633512,13.8849554560984));
#83366=CARTESIAN_POINT('Ctrl Pts',(2.5312700171628,137.824194363192,12.5610019680181));
#83367=CARTESIAN_POINT('Ctrl Pts',(2.61051962143818,138.980832587105,11.9113913495609));
#83368=CARTESIAN_POINT('Ctrl Pts',(2.68976922571355,140.154950676288,12.5288314630997));
#83369=CARTESIAN_POINT('Ctrl Pts',(2.76901882998892,140.275214890819,13.8499470203793));
#83370=CARTESIAN_POINT('Ctrl Pts',(2.8482684342643,139.231880590669,14.6692487692842));
#83371=CARTESIAN_POINT('Ctrl Pts',(2.92751803853967,137.976963165223,14.2391527366441));
#83372=CARTESIAN_POINT('Ctrl Pts',(3.00676764281505,137.655536323194,12.9521065933296));
#83373=CARTESIAN_POINT('Ctrl Pts',(3.08601724709042,138.560893438705,11.9825033575352));
#83374=CARTESIAN_POINT('Ctrl Pts',(3.16526685136579,139.866922293386,12.2150770092107));
#83375=CARTESIAN_POINT('Ctrl Pts',(3.24451645564117,140.381910028251,13.4376111754579));
#83376=CARTESIAN_POINT('Ctrl Pts',(3.32376605991654,139.635945339619,14.5345791356308));
#83377=CARTESIAN_POINT('Ctrl Pts',(3.40301566419192,138.309699184017,14.5050298433538));
#83378=CARTESIAN_POINT('Ctrl Pts',(3.48226526846729,137.613332281705,13.3759261313631));
#83379=CARTESIAN_POINT('Ctrl Pts',(3.56151487274267,138.182259029248,12.1775420548631));
#83380=CARTESIAN_POINT('Ctrl Pts',(3.64076447701804,139.497350441074,12.003367949123));
#83381=CARTESIAN_POINT('Ctrl Pts',(3.72001408129341,140.358624154713,13.0123325836223));
#83382=CARTESIAN_POINT('Ctrl Pts',(3.79926368556878,139.980193151235,14.2837853028199));
#83383=CARTESIAN_POINT('Ctrl Pts',(3.87851328984416,138.707364629187,14.657562770499));
#83384=CARTESIAN_POINT('Ctrl Pts',(3.95776289411953,137.701557305092,13.7926040032988));
#83385=CARTESIAN_POINT('Ctrl Pts',(4.03701249839491,137.880540879759,12.478158522525));
#83386=CARTESIAN_POINT('Ctrl Pts',(4.11626210267028,139.080998087674,11.9136192998211));
#83387=CARTESIAN_POINT('Ctrl Pts',(4.19551170694565,140.207546914827,12.6141118280076));
#83388=CARTESIAN_POINT('Ctrl Pts',(4.27476131122103,140.232244578235,13.9404572081215));
#83389=CARTESIAN_POINT('Ctrl Pts',(4.3540109154964,139.132555183917,14.682404159178));
#83390=CARTESIAN_POINT('Ctrl Pts',(4.43326051977178,137.911913069879,14.1629478363558));
#83391=CARTESIAN_POINT('Ctrl Pts',(4.51251012404715,137.684118384997,12.8560769081125));
#83392=CARTESIAN_POINT('Ctrl Pts',(4.59175972832253,138.657027102691,11.9542727883001));
#83393=CARTESIAN_POINT('Ctrl Pts',(4.6710093325979,139.942888534928,12.2804053037847));
#83394=CARTESIAN_POINT('Ctrl Pts',(4.75025893687327,140.368391819196,13.5368880907559));
#83395=CARTESIAN_POINT('Ctrl Pts',(4.82950854114865,139.545277675295,14.5772174430167));
#83396=CARTESIAN_POINT('Ctrl Pts',(4.90875814542402,138.224613644119,14.4521233077368));
#83397=CARTESIAN_POINT('Ctrl Pts',(4.9880077496994,137.611466917631,13.2757504441729));
#83398=CARTESIAN_POINT('Ctrl Pts',(5.06725735397477,138.265315962094,12.121504551065));
#83399=CARTESIAN_POINT('Ctrl Pts',(5.14650695825016,139.589542584736,12.0426012900189));
#83400=CARTESIAN_POINT('Ctrl Pts',(5.22575656252551,140.375829026531,13.1110373306486));
#83401=CARTESIAN_POINT('Ctrl Pts',(5.30500616680089,139.906711507075,14.3518966066086));
#83402=CARTESIAN_POINT('Ctrl Pts',(5.38425577107627,138.61024694163,14.6329303635249));
#83403=CARTESIAN_POINT('Ctrl Pts',(5.46350537535164,137.669419323723,13.6977056787498));
#83404=CARTESIAN_POINT('Ctrl Pts',(5.54275497962702,137.942710242223,12.3995832381271));
#83405=CARTESIAN_POINT('Ctrl Pts',(5.62200458390239,139.180741555268,11.9230708573093));
#83406=CARTESIAN_POINT('Ctrl Pts',(5.70125418817776,140.253862892755,12.7029532405301));
#83407=CARTESIAN_POINT('Ctrl Pts',(5.78050379245314,140.182847559272,14.0276495561597));
#83408=CARTESIAN_POINT('Ctrl Pts',(5.85975339672852,139.032567105703,14.6883327363301));
#83409=CARTESIAN_POINT('Ctrl Pts',(5.93900300100388,137.852469738973,14.0823150174432));
#83410=CARTESIAN_POINT('Ctrl Pts',(6.01825260527925,137.719667412237,12.762226377427));
#83411=CARTESIAN_POINT('Ctrl Pts',(6.09750220955463,138.754702766038,11.9333180733695));
#83412=CARTESIAN_POINT('Ctrl Pts',(6.17675181383001,140.014448367052,12.3504727739682));
#83413=CARTESIAN_POINT('Ctrl Pts',(6.25600804413745,140.34671451531,13.636171520518));
#83414=CARTESIAN_POINT('Ctrl Pts',(6.30884773968643,139.751301345624,14.2848551797266));
#83415=CARTESIAN_POINT('Ctrl Pts',(6.33527090047694,139.382151741646,14.4117392436421));
#83416=CARTESIAN_POINT('Ctrl Pts',(1.9531481975811,138.449114295271,14.4469702735566));
#83417=CARTESIAN_POINT('Ctrl Pts',(1.97957252209675,138.068247594067,14.2640523781665));
#83418=CARTESIAN_POINT('Ctrl Pts',(2.03241338137086,137.509910778712,13.4916602584589));
#83419=CARTESIAN_POINT('Ctrl Pts',(2.11167077540342,138.029153812998,12.1514013965941));
#83420=CARTESIAN_POINT('Ctrl Pts',(2.19092037967879,139.435951580932,11.8617426971333));
#83421=CARTESIAN_POINT('Ctrl Pts',(2.27016998395417,140.444131634942,12.8832714923419));
#83422=CARTESIAN_POINT('Ctrl Pts',(2.34941958822954,140.134984091314,14.2856203071142));
#83423=CARTESIAN_POINT('Ctrl Pts',(2.42866919250492,138.790003138397,14.7883445996285));
#83424=CARTESIAN_POINT('Ctrl Pts',(2.50791879678029,137.636731958093,13.933131153325));
#83425=CARTESIAN_POINT('Ctrl Pts',(2.58716840105567,137.727357491656,12.5001396492404));
#83426=CARTESIAN_POINT('Ctrl Pts',(2.66641800533104,138.979253999418,11.7970284707942));
#83427=CARTESIAN_POINT('Ctrl Pts',(2.74566760960641,140.250069977274,12.4653196494102));
#83428=CARTESIAN_POINT('Ctrl Pts',(2.82491721388179,140.380238898782,13.8952394967008));
#83429=CARTESIAN_POINT('Ctrl Pts',(2.90416681815716,139.250977786895,14.7820172090845));
#83430=CARTESIAN_POINT('Ctrl Pts',(2.98341642243253,137.892708009911,14.3164993746116));
#83431=CARTESIAN_POINT('Ctrl Pts',(3.06266602670791,137.544809131318,12.9234548263411));
#83432=CARTESIAN_POINT('Ctrl Pts',(3.14191563098328,138.524729548743,11.8739971137133));
#83433=CARTESIAN_POINT('Ctrl Pts',(3.22116523525866,139.938320184439,12.1257250406574));
#83434=CARTESIAN_POINT('Ctrl Pts',(3.30041483953403,140.495721222627,13.4489445415368));
#83435=CARTESIAN_POINT('Ctrl Pts',(3.3796644438094,139.688320456074,14.6362564685289));
#83436=CARTESIAN_POINT('Ctrl Pts',(3.45891404808478,138.252847465207,14.6042735588831));
#83437=CARTESIAN_POINT('Ctrl Pts',(3.53816365236015,137.499129254014,13.3821792473534));
#83438=CARTESIAN_POINT('Ctrl Pts',(3.61741325663553,138.114911608165,12.0850987866609));
#83439=CARTESIAN_POINT('Ctrl Pts',(3.6966628609109,139.538311174092,11.8965800690441));
#83440=CARTESIAN_POINT('Ctrl Pts',(3.77591246518627,140.470517573672,12.9886409021295));
#83441=CARTESIAN_POINT('Ctrl Pts',(3.85516206946165,140.060919791161,14.3648077847721));
#83442=CARTESIAN_POINT('Ctrl Pts',(3.93441167373702,138.683263797448,14.7693687760942));
#83443=CARTESIAN_POINT('Ctrl Pts',(4.01366127801239,137.594620304191,13.8331738297156));
#83444=CARTESIAN_POINT('Ctrl Pts',(4.09291088228777,137.788344588448,12.4104733923595));
#83445=CARTESIAN_POINT('Ctrl Pts',(4.17216048656314,139.087668919285,11.7994399103375));
#83446=CARTESIAN_POINT('Ctrl Pts',(4.25141009083852,140.306997931053,12.5576235252477));
#83447=CARTESIAN_POINT('Ctrl Pts',(4.33065969511389,140.333729641912,13.9932039125471));
#83448=CARTESIAN_POINT('Ctrl Pts',(4.40990929938927,139.1434721492,14.7962560491346));
#83449=CARTESIAN_POINT('Ctrl Pts',(4.48915890366464,137.822300525957,14.2340183995126));
#83450=CARTESIAN_POINT('Ctrl Pts',(4.56840850794001,137.57574515143,12.8195163388526));
#83451=CARTESIAN_POINT('Ctrl Pts',(4.64765811221539,138.628780578472,11.8434415343569));
#83452=CARTESIAN_POINT('Ctrl Pts',(4.72690771649076,140.02054284536,12.1964336357431));
#83453=CARTESIAN_POINT('Ctrl Pts',(4.80615732076614,140.481089682396,13.5563976941245));
#83454=CARTESIAN_POINT('Ctrl Pts',(4.88540692504151,139.590185594206,14.6824063769528));
#83455=CARTESIAN_POINT('Ctrl Pts',(4.96465652931688,138.160754459757,14.5470097526149));
#83456=CARTESIAN_POINT('Ctrl Pts',(5.04390613359226,137.49711026249,13.2737533019168));
#83457=CARTESIAN_POINT('Ctrl Pts',(5.12315573786763,138.204808934767,12.0244461522779));
#83458=CARTESIAN_POINT('Ctrl Pts',(5.202405342143,139.638096068199,11.939044585122));
#83459=CARTESIAN_POINT('Ctrl Pts',(5.28165494641838,140.489139402435,13.0954747638737));
#83460=CARTESIAN_POINT('Ctrl Pts',(5.36090455069375,139.98138635382,14.4385285918397));
#83461=CARTESIAN_POINT('Ctrl Pts',(5.44015415496912,138.578147702043,14.7427076960513));
#83462=CARTESIAN_POINT('Ctrl Pts',(5.5194037592445,137.55983550648,13.7304598793731));
#83463=CARTESIAN_POINT('Ctrl Pts',(5.59865336351987,137.85563408844,12.3254268133166));
#83464=CARTESIAN_POINT('Ctrl Pts',(5.67790296779525,139.195627048432,11.8096698781595));
#83465=CARTESIAN_POINT('Ctrl Pts',(5.75715257207062,140.357128395206,12.6537817290681));
#83466=CARTESIAN_POINT('Ctrl Pts',(5.836402176346,140.280264388684,14.0875772384116));
#83467=CARTESIAN_POINT('Ctrl Pts',(5.91565178062137,139.035249263818,14.8026728913928));
#83468=CARTESIAN_POINT('Ctrl Pts',(5.99490138489674,137.757961567731,14.1467448317533));
#83469=CARTESIAN_POINT('Ctrl Pts',(6.07415098917212,137.614221921552,12.7179364764654));
#83470=CARTESIAN_POINT('Ctrl Pts',(6.1534005934475,138.734500603377,11.8207610333147));
#83471=CARTESIAN_POINT('Ctrl Pts',(6.23265019772286,140.097996194282,12.2722717149427));
#83472=CARTESIAN_POINT('Ctrl Pts',(6.31190642803031,140.457627081495,13.6638578976939));
#83473=CARTESIAN_POINT('Ctrl Pts',(6.36474612357929,139.813176939356,14.3659657744835));
#83474=CARTESIAN_POINT('Ctrl Pts',(6.39116928436981,139.413624952825,14.5032997422034));
#83475=CARTESIAN_POINT('Ctrl Pts',(2.00904658147396,138.407196751365,14.5342445963199));
#83476=CARTESIAN_POINT('Ctrl Pts',(2.03547090598961,137.997349453038,14.3374082622313));
#83477=CARTESIAN_POINT('Ctrl Pts',(2.08831176526372,137.396528129969,13.5062439138887));
#83478=CARTESIAN_POINT('Ctrl Pts',(2.16756915929628,137.955280979994,12.0640031722895));
#83479=CARTESIAN_POINT('Ctrl Pts',(2.24681876357166,139.469123651614,11.7523040002805));
#83480=CARTESIAN_POINT('Ctrl Pts',(2.32606836784703,140.55401731666,12.8515621280101));
#83481=CARTESIAN_POINT('Ctrl Pts',(2.4053179721224,140.221346371314,14.3606173203656));
#83482=CARTESIAN_POINT('Ctrl Pts',(2.48456757639778,138.774024229176,14.9015944980482));
#83483=CARTESIAN_POINT('Ctrl Pts',(2.56381718067315,137.532999282673,13.9813068505515));
#83484=CARTESIAN_POINT('Ctrl Pts',(2.64306678494853,137.630520620122,12.4392773304629));
#83485=CARTESIAN_POINT('Ctrl Pts',(2.7223163892239,138.977675411732,11.6826655920275));
#83486=CARTESIAN_POINT('Ctrl Pts',(2.80156599349928,140.345189278261,12.4018078357209));
#83487=CARTESIAN_POINT('Ctrl Pts',(2.88081559777465,140.485262906743,13.940531973022));
#83488=CARTESIAN_POINT('Ctrl Pts',(2.96006520205002,139.270074983123,14.8947856488846));
#83489=CARTESIAN_POINT('Ctrl Pts',(3.0393148063254,137.8084528546,14.3938460125793));
#83490=CARTESIAN_POINT('Ctrl Pts',(3.11856441060077,137.434081939444,12.8948030593524));
#83491=CARTESIAN_POINT('Ctrl Pts',(3.19781401487614,138.48856565878,11.7654908698915));
#83492=CARTESIAN_POINT('Ctrl Pts',(3.27706361915152,140.009718075492,12.0363730721043));
#83493=CARTESIAN_POINT('Ctrl Pts',(3.35631322342689,140.609532417002,13.4602779076157));
#83494=CARTESIAN_POINT('Ctrl Pts',(3.43556282770226,139.740695572528,14.7379338014271));
#83495=CARTESIAN_POINT('Ctrl Pts',(3.51481243197764,138.195995746398,14.7035172744123));
#83496=CARTESIAN_POINT('Ctrl Pts',(3.59406203625301,137.384926226324,13.3884323633436));
#83497=CARTESIAN_POINT('Ctrl Pts',(3.67331164052839,138.047564187082,11.9926555184588));
#83498=CARTESIAN_POINT('Ctrl Pts',(3.75256124480376,139.57927190711,11.7897921889655));
#83499=CARTESIAN_POINT('Ctrl Pts',(3.83181084907914,140.582410992633,12.9649492206368));
#83500=CARTESIAN_POINT('Ctrl Pts',(3.91106045335451,140.141646431087,14.4458302667241));
#83501=CARTESIAN_POINT('Ctrl Pts',(3.99031005762989,138.659162965709,14.8811747816896));
#83502=CARTESIAN_POINT('Ctrl Pts',(4.06955966190525,137.48768330329,13.8737436561324));
#83503=CARTESIAN_POINT('Ctrl Pts',(4.14880926618063,137.696148297138,12.3427882621941));
#83504=CARTESIAN_POINT('Ctrl Pts',(4.228058870456,139.094339750897,11.6852605208537));
#83505=CARTESIAN_POINT('Ctrl Pts',(4.30730847473138,140.406448947278,12.5011352224877));
#83506=CARTESIAN_POINT('Ctrl Pts',(4.38655807900675,140.435214705589,14.0459506169728));
#83507=CARTESIAN_POINT('Ctrl Pts',(4.46580768328213,139.154389114483,14.9101079390912));
#83508=CARTESIAN_POINT('Ctrl Pts',(4.5450572875575,137.732687982037,14.3050889626694));
#83509=CARTESIAN_POINT('Ctrl Pts',(4.62430689183287,137.467371917862,12.7829557695927));
#83510=CARTESIAN_POINT('Ctrl Pts',(4.70355649610825,138.600534054253,11.7326102804137));
#83511=CARTESIAN_POINT('Ctrl Pts',(4.78280610038362,140.098197155792,12.1124619677015));
#83512=CARTESIAN_POINT('Ctrl Pts',(4.862055704659,140.593787545595,13.5759072974933));
#83513=CARTESIAN_POINT('Ctrl Pts',(4.94130530893437,139.635093513118,14.7875953108892));
#83514=CARTESIAN_POINT('Ctrl Pts',(5.02055491320974,138.096895275395,14.6418961974928));
#83515=CARTESIAN_POINT('Ctrl Pts',(5.09980451748512,137.382753607351,13.2717561596606));
#83516=CARTESIAN_POINT('Ctrl Pts',(5.17905412176049,138.14430190744,11.9273877534907));
#83517=CARTESIAN_POINT('Ctrl Pts',(5.25830372603587,139.686649551662,11.835487880225));
#83518=CARTESIAN_POINT('Ctrl Pts',(5.33755333031124,140.60244977834,13.0799121970989));
#83519=CARTESIAN_POINT('Ctrl Pts',(5.41680293458661,140.056061200564,14.5251605770708));
#83520=CARTESIAN_POINT('Ctrl Pts',(5.49605253886199,138.546048462455,14.8524850285775));
#83521=CARTESIAN_POINT('Ctrl Pts',(5.57530214313737,137.45025168924,13.7632140799964));
#83522=CARTESIAN_POINT('Ctrl Pts',(5.65455174741274,137.768557934658,12.251270388506));
#83523=CARTESIAN_POINT('Ctrl Pts',(5.73380135168811,139.210512541595,11.6962688990097));
#83524=CARTESIAN_POINT('Ctrl Pts',(5.81305095596348,140.460393897656,12.6046102176062));
#83525=CARTESIAN_POINT('Ctrl Pts',(5.89230056023886,140.377681218095,14.1475049206634));
#83526=CARTESIAN_POINT('Ctrl Pts',(5.97155016451423,139.037931421934,14.9170130464555));
#83527=CARTESIAN_POINT('Ctrl Pts',(6.05079976878961,137.663453396491,14.2111746460634));
#83528=CARTESIAN_POINT('Ctrl Pts',(6.13004937306498,137.508776430867,12.673646575504));
#83529=CARTESIAN_POINT('Ctrl Pts',(6.20929897734035,138.714298440715,11.70820399326));
#83530=CARTESIAN_POINT('Ctrl Pts',(6.28854858161573,140.181544021511,12.1940706559173));
#83531=CARTESIAN_POINT('Ctrl Pts',(6.36780481192318,140.56853964768,13.6915442748698));
#83532=CARTESIAN_POINT('Ctrl Pts',(6.42064450747215,139.875052533088,14.4470763692405));
#83533=CARTESIAN_POINT('Ctrl Pts',(6.44706766826268,139.445098164004,14.5948602407648));
#83534=CARTESIAN_POINT('Ctrl Pts',(2.06494496536683,138.36527920746,14.621518919083));
#83535=CARTESIAN_POINT('Ctrl Pts',(2.09136928988247,137.926451312009,14.4107641462959));
#83536=CARTESIAN_POINT('Ctrl Pts',(2.14421014915659,137.283145481227,13.5208275693184));
#83537=CARTESIAN_POINT('Ctrl Pts',(2.22346754318915,137.881408146991,11.976604947985));
#83538=CARTESIAN_POINT('Ctrl Pts',(2.30271714746453,139.502295722294,11.6428653034279));
#83539=CARTESIAN_POINT('Ctrl Pts',(2.3819667517399,140.663902998379,12.8198527636783));
#83540=CARTESIAN_POINT('Ctrl Pts',(2.46121635601528,140.307708651313,14.4356143336172));
#83541=CARTESIAN_POINT('Ctrl Pts',(2.54046596029065,138.758045319957,15.014844396468));
#83542=CARTESIAN_POINT('Ctrl Pts',(2.61971556456603,137.429266607254,14.0294825477779));
#83543=CARTESIAN_POINT('Ctrl Pts',(2.6989651688414,137.533683748586,12.3784150116853));
#83544=CARTESIAN_POINT('Ctrl Pts',(2.77821477311677,138.976096824046,11.5683027132609));
#83545=CARTESIAN_POINT('Ctrl Pts',(2.85746437739215,140.440308579247,12.3382960220315));
#83546=CARTESIAN_POINT('Ctrl Pts',(2.93671398166752,140.590286914707,13.9858244493435));
#83547=CARTESIAN_POINT('Ctrl Pts',(3.0159635859429,139.289172179348,15.0075540886847));
#83548=CARTESIAN_POINT('Ctrl Pts',(3.09521319021827,137.724197699289,14.4711926505468));
#83549=CARTESIAN_POINT('Ctrl Pts',(3.17446279449364,137.323354747568,12.8661512923638));
#83550=CARTESIAN_POINT('Ctrl Pts',(3.25371239876901,138.452401768818,11.6569846260696));
#83551=CARTESIAN_POINT('Ctrl Pts',(3.33296200304439,140.081115966545,11.9470211035511));
#83552=CARTESIAN_POINT('Ctrl Pts',(3.41221160731976,140.72334361138,13.4716112736946));
#83553=CARTESIAN_POINT('Ctrl Pts',(3.49146121159514,139.793070688983,14.8396111343253));
#83554=CARTESIAN_POINT('Ctrl Pts',(3.57071081587051,138.139144027589,14.8027609899417));
#83555=CARTESIAN_POINT('Ctrl Pts',(3.64996042014589,137.270723198634,13.3946854793339));
#83556=CARTESIAN_POINT('Ctrl Pts',(3.72921002442126,137.980216765998,11.9002122502566));
#83557=CARTESIAN_POINT('Ctrl Pts',(3.80845962869663,139.620232640128,11.6830043088867));
#83558=CARTESIAN_POINT('Ctrl Pts',(3.88770923297201,140.694304411592,12.941257539144));
#83559=CARTESIAN_POINT('Ctrl Pts',(3.96695883724738,140.222373071014,14.5268527486763));
#83560=CARTESIAN_POINT('Ctrl Pts',(4.04620844152276,138.63506213397,14.9929807872849));
#83561=CARTESIAN_POINT('Ctrl Pts',(4.12545804579813,137.380746302389,13.9143134825491));
#83562=CARTESIAN_POINT('Ctrl Pts',(4.2047076500735,137.603952005827,12.2751031320286));
#83563=CARTESIAN_POINT('Ctrl Pts',(4.28395725434888,139.101010582507,11.57108113137));
#83564=CARTESIAN_POINT('Ctrl Pts',(4.36320685862425,140.505899963503,12.4446469197279));
#83565=CARTESIAN_POINT('Ctrl Pts',(4.44245646289962,140.536699769265,14.0986973213983));
#83566=CARTESIAN_POINT('Ctrl Pts',(4.521706067175,139.165306079766,15.0239598290478));
#83567=CARTESIAN_POINT('Ctrl Pts',(4.60095567145037,137.643075438114,14.3761595258263));
#83568=CARTESIAN_POINT('Ctrl Pts',(4.68020527572575,137.358998684294,12.7463952003328));
#83569=CARTESIAN_POINT('Ctrl Pts',(4.75945488000112,138.572287530034,11.6217790264705));
#83570=CARTESIAN_POINT('Ctrl Pts',(4.8387044842765,140.175851466226,12.02849029966));
#83571=CARTESIAN_POINT('Ctrl Pts',(4.91795408855187,140.706485408794,13.595416900862));
#83572=CARTESIAN_POINT('Ctrl Pts',(4.99720369282725,139.68000143203,14.8927842448254));
#83573=CARTESIAN_POINT('Ctrl Pts',(5.07645329710261,138.033036091033,14.7367826423707));
#83574=CARTESIAN_POINT('Ctrl Pts',(5.15570290137799,137.268396952211,13.2697590174042));
#83575=CARTESIAN_POINT('Ctrl Pts',(5.23495250565336,138.083794880113,11.8303293547037));
#83576=CARTESIAN_POINT('Ctrl Pts',(5.31420210992873,139.735203035125,11.7319311753281));
#83577=CARTESIAN_POINT('Ctrl Pts',(5.39345171420411,140.715760154244,13.0643496303242));
#83578=CARTESIAN_POINT('Ctrl Pts',(5.47270131847949,140.130736047309,14.6117925623019));
#83579=CARTESIAN_POINT('Ctrl Pts',(5.55195092275486,138.513949222868,14.9622623611039));
#83580=CARTESIAN_POINT('Ctrl Pts',(5.63120052703023,137.340667871997,13.7959682806195));
#83581=CARTESIAN_POINT('Ctrl Pts',(5.71045013130561,137.681481780874,12.1771139636956));
#83582=CARTESIAN_POINT('Ctrl Pts',(5.78969973558099,139.225398034759,11.5828679198597));
#83583=CARTESIAN_POINT('Ctrl Pts',(5.86894933985634,140.563659400107,12.5554387061441));
#83584=CARTESIAN_POINT('Ctrl Pts',(5.94819894413173,140.475098047509,14.2074326029153));
#83585=CARTESIAN_POINT('Ctrl Pts',(6.02744854840711,139.040613580049,15.0313532015183));
#83586=CARTESIAN_POINT('Ctrl Pts',(6.10669815268248,137.568945225249,14.2756044603734));
#83587=CARTESIAN_POINT('Ctrl Pts',(6.18594775695784,137.403330940182,12.6293566745424));
#83588=CARTESIAN_POINT('Ctrl Pts',(6.26519736123323,138.694096278053,11.5956469532053));
#83589=CARTESIAN_POINT('Ctrl Pts',(6.34444696550859,140.265091848741,12.1158695968918));
#83590=CARTESIAN_POINT('Ctrl Pts',(6.42370319581604,140.679452213867,13.7192306520457));
#83591=CARTESIAN_POINT('Ctrl Pts',(6.47654289136502,139.936928126819,14.5281869639975));
#83592=CARTESIAN_POINT('Ctrl Pts',(6.50296605215554,139.476571375183,14.6864207393261));
#83593=CARTESIAN_POINT('Ctrl Pts',(6.33564735913931,139.984553534226,12.2160336743987));
#83594=CARTESIAN_POINT('Ctrl Pts',(6.3357883151664,139.987674636155,12.2190589540515));
#83595=CARTESIAN_POINT('Ctrl Pts',(6.33592973903903,139.990781924426,12.2220984365611));
#83596=CARTESIAN_POINT('Ctrl Pts',(6.33621393093556,139.996976184895,12.2282131236378));
#83597=CARTESIAN_POINT('Ctrl Pts',(6.33635670003917,140.000063059071,12.2312883679801));
#83598=CARTESIAN_POINT('Ctrl Pts',(6.33650000000001,140.003135769676,12.2343777040635));
#83599=CARTESIAN_POINT('',(2.06296787020315,138.314392290401,12.3412366180523));
#83600=CARTESIAN_POINT('Ctrl Pts',(2.06350000000003,138.31381039713,12.3405101317741));
#83601=CARTESIAN_POINT('Ctrl Pts',(2.06349999999999,138.285458471108,12.3559164614661));
#83602=CARTESIAN_POINT('Ctrl Pts',(2.06349999999991,138.257842156157,12.372524187337));
#83603=CARTESIAN_POINT('Ctrl Pts',(2.06349999999993,138.231048120938,12.3903151986867));
#83604=CARTESIAN_POINT('Ctrl Pts',(2.06349999999997,138.190824387068,12.4170234156452));
#83605=CARTESIAN_POINT('Ctrl Pts',(2.06350000000012,138.15245237466,12.4463958230688));
#83606=CARTESIAN_POINT('Ctrl Pts',(2.0635,138.116003297166,12.4781362863144));
#83607=CARTESIAN_POINT('Ctrl Pts',(2.06349999999994,138.097947361144,12.4938596958785));
#83608=CARTESIAN_POINT('Ctrl Pts',(2.06350000000003,138.080363580768,12.5101649876866));
#83609=CARTESIAN_POINT('Ctrl Pts',(2.06349999999992,138.063262566106,12.5270202810066));
#83610=CARTESIAN_POINT('Ctrl Pts',(2.06349999999987,138.055307674324,12.5348608704087));
#83611=CARTESIAN_POINT('Ctrl Pts',(2.06350000000001,138.047460879066,12.542817048106));
#83612=CARTESIAN_POINT('Ctrl Pts',(2.06350000000004,138.039728403076,12.5508795988707));
#83613=CARTESIAN_POINT('Ctrl Pts',(2.06350000000019,138.004683647871,12.5874203030686));
#83614=CARTESIAN_POINT('Ctrl Pts',(2.06350000000007,137.97195072146,12.6261758296458));
#83615=CARTESIAN_POINT('Ctrl Pts',(2.06350000000008,137.941609469643,12.6668229112449));
#83616=CARTESIAN_POINT('Ctrl Pts',(2.06350000000009,137.920229233239,12.6954652434387));
#83617=CARTESIAN_POINT('Ctrl Pts',(2.06350000000024,137.900036955561,12.725047988167));
#83618=CARTESIAN_POINT('Ctrl Pts',(2.06349999999998,137.881068772353,12.7554710709598));
#83619=CARTESIAN_POINT('Ctrl Pts',(2.06349999999989,137.874172837461,12.766531465931));
#83620=CARTESIAN_POINT('Ctrl Pts',(2.06349999999995,137.867438766385,12.777703018237));
#83621=CARTESIAN_POINT('Ctrl Pts',(2.06349999999992,137.860868566423,12.7889812037336));
#83622=CARTESIAN_POINT('Ctrl Pts',(2.0634999999999,137.855417684603,12.7983380051462));
#83623=CARTESIAN_POINT('Ctrl Pts',(2.06350000000018,137.850083786557,12.8077610883057));
#83624=CARTESIAN_POINT('Ctrl Pts',(2.06350000000015,137.844869690817,12.8172435416598));
#83625=CARTESIAN_POINT('Ctrl Pts',(2.06349999999998,137.819549238928,12.863291795451));
#83626=CARTESIAN_POINT('Ctrl Pts',(2.06350000000024,137.797034877009,12.9107653736245));
#83627=CARTESIAN_POINT('Ctrl Pts',(2.06350000000017,137.777411572447,12.9593365650308));
#83628=CARTESIAN_POINT('Ctrl Pts',(2.06350000000009,137.757448351045,13.0087491114608));
#83629=CARTESIAN_POINT('Ctrl Pts',(2.06350000000017,137.740476446572,13.0592985264396));
#83630=CARTESIAN_POINT('Ctrl Pts',(2.06350000000001,137.72662193392,13.1106779323383));
#83631=CARTESIAN_POINT('Ctrl Pts',(2.06349999999992,137.718765064424,13.1398151020845));
#83632=CARTESIAN_POINT('Ctrl Pts',(2.06350000000036,137.711911474736,13.1692198144023));
#83633=CARTESIAN_POINT('Ctrl Pts',(2.06350000000024,137.706090714823,13.1988396596195));
#83634=CARTESIAN_POINT('Ctrl Pts',(2.06350000000017,137.702885402907,13.2151503895351));
#83635=CARTESIAN_POINT('Ctrl Pts',(2.06350000000025,137.699993372106,13.2315263917338));
#83636=CARTESIAN_POINT('Ctrl Pts',(2.06350000000008,137.697420260214,13.2479591140196));
#83637=CARTESIAN_POINT('Ctrl Pts',(2.06349999999997,137.695935004121,13.2574444383731));
#83638=CARTESIAN_POINT('Ctrl Pts',(2.06350000000016,137.694556261355,13.2669477366054));
#83639=CARTESIAN_POINT('Ctrl Pts',(2.06350000000011,137.693286568647,13.2764543915575));
#83640=CARTESIAN_POINT('Ctrl Pts',(2.06349999999986,137.686032340524,13.3307694579084));
#83641=CARTESIAN_POINT('Ctrl Pts',(2.0635000000002,137.682316399564,13.3853020607817));
#83642=CARTESIAN_POINT('Ctrl Pts',(2.06349999999998,137.682252389277,13.4397235925187));
#83643=CARTESIAN_POINT('Ctrl Pts',(2.06349999999994,137.682241271235,13.4491761492556));
#83644=CARTESIAN_POINT('Ctrl Pts',(2.06349999999988,137.682340435788,13.4586254213502));
#83645=CARTESIAN_POINT('Ctrl Pts',(2.06349999999989,137.682550620444,13.4680697618261));
#83646=CARTESIAN_POINT('Ctrl Pts',(2.06349999999994,137.683718804571,13.5205604092094));
#83647=CARTESIAN_POINT('Ctrl Pts',(2.06350000000034,137.688312171862,13.5728980536096));
#83648=CARTESIAN_POINT('Ctrl Pts',(2.0635000000001,137.696128834035,13.6248637376689));
#83649=CARTESIAN_POINT('Ctrl Pts',(2.06349999999998,137.700124807928,13.6514292348389));
#83650=CARTESIAN_POINT('Ctrl Pts',(2.06349999999988,137.704963995215,13.6778976645399));
#83651=CARTESIAN_POINT('Ctrl Pts',(2.06350000000013,137.710624501111,13.7042400680577));
#83652=CARTESIAN_POINT('Ctrl Pts',(2.06350000000029,137.714078239673,13.7203127966335));
#83653=CARTESIAN_POINT('Ctrl Pts',(2.06349999999984,137.717837803142,13.7363386079794));
#83654=CARTESIAN_POINT('Ctrl Pts',(2.0634999999999,137.721898811607,13.7523108670406));
#83655=CARTESIAN_POINT('Ctrl Pts',(2.06349999999993,137.724577776208,13.7628474411447));
#83656=CARTESIAN_POINT('Ctrl Pts',(2.0635,137.727388445803,13.7733621159339));
#83657=CARTESIAN_POINT('Ctrl Pts',(2.06350000000002,137.730324276325,13.7838350181237));
#83658=CARTESIAN_POINT('Ctrl Pts',(2.06350000000014,137.745127646236,13.8366426458083));
#83659=CARTESIAN_POINT('Ctrl Pts',(2.06350000000013,137.76313364273,13.8884900800757));
#83660=CARTESIAN_POINT('Ctrl Pts',(2.06350000000001,137.784102793348,13.9391405178824));
#83661=CARTESIAN_POINT('Ctrl Pts',(2.06349999999989,137.805528956221,13.9908948569041));
#83662=CARTESIAN_POINT('Ctrl Pts',(2.06350000000002,137.830049059367,14.0414004131965));
#83663=CARTESIAN_POINT('Ctrl Pts',(2.06349999999993,137.857462565103,14.090404990338));
#83664=CARTESIAN_POINT('Ctrl Pts',(2.06349999999988,137.8728625944,14.1179341918534));
#83665=CARTESIAN_POINT('Ctrl Pts',(2.06349999999982,137.88917669756,14.1449896367826));
#83666=CARTESIAN_POINT('Ctrl Pts',(2.06349999999995,137.906376242815,14.1715248807554));
#83667=CARTESIAN_POINT('Ctrl Pts',(2.06350000000004,137.917641306872,14.1889044811272));
#83668=CARTESIAN_POINT('Ctrl Pts',(2.06349999999991,137.929286303867,14.2060608964028));
#83669=CARTESIAN_POINT('Ctrl Pts',(2.06349999999999,137.941304251294,14.222980560379));
#83670=CARTESIAN_POINT('Ctrl Pts',(2.06350000000003,137.947363355696,14.2315109696768));
#83671=CARTESIAN_POINT('Ctrl Pts',(2.06350000000009,137.953518778308,14.2399832102723));
#83672=CARTESIAN_POINT('Ctrl Pts',(2.06350000000006,137.959764791964,14.2483889110011));
#83673=CARTESIAN_POINT('Ctrl Pts',(2.0634999999999,137.994493741366,14.2951261055335));
#83674=CARTESIAN_POINT('Ctrl Pts',(2.06350000000023,138.031910482614,14.3396636613191));
#83675=CARTESIAN_POINT('Ctrl Pts',(2.0635000000002,138.071787386868,14.3817421533142));
#83676=CARTESIAN_POINT('Ctrl Pts',(2.06350000000016,138.111761295662,14.42392300543));
#83677=CARTESIAN_POINT('Ctrl Pts',(2.06349999999991,138.154207834877,14.46363388879));
#83678=CARTESIAN_POINT('Ctrl Pts',(2.06350000000003,138.198946759824,14.500595934106));
#83679=CARTESIAN_POINT('Ctrl Pts',(2.06350000000015,138.24264340849,14.536696879984));
#83680=CARTESIAN_POINT('Ctrl Pts',(2.06349999999996,138.288527497966,14.5701764701555));
#83681=CARTESIAN_POINT('Ctrl Pts',(2.06349999999993,138.336469361946,14.6007438022739));
#83682=CARTESIAN_POINT('Ctrl Pts',(2.06349999999992,138.346225523483,14.606964249398));
#83683=CARTESIAN_POINT('Ctrl Pts',(2.06350000000002,138.356067013842,14.6130639630822));
#83684=CARTESIAN_POINT('Ctrl Pts',(2.06350000000003,138.365992905425,14.6190402776369));
#83685=CARTESIAN_POINT('Ctrl Pts',(2.06296787020315,138.314932905069,12.3419926211435));
#83686=CARTESIAN_POINT('Ctrl Pts',(2.06314524680209,138.318975915862,12.3391014809294));
#83687=CARTESIAN_POINT('Ctrl Pts',(2.06332262340104,138.323037228809,12.3362359347072));
#83688=CARTESIAN_POINT('Ctrl Pts',(2.06349999999998,138.327116518419,12.3333962121349));
#83689=CARTESIAN_POINT('Origin',(2.0635,139.,13.3));
#83690=CARTESIAN_POINT('',(2.0635,137.5365,13.3));
#83691=CARTESIAN_POINT('Origin',(2.0635,139.,13.3));
#83692=CARTESIAN_POINT('',(2.0635,139.657803339705,14.6073358467787));
#83693=CARTESIAN_POINT('Origin',(2.0635,139.,13.3));
#83694=CARTESIAN_POINT('Ctrl Pts',(2.06350000000018,139.657803339705,14.6073358467788));
#83695=CARTESIAN_POINT('Ctrl Pts',(2.06349989428253,139.684079946574,14.591010615939));
#83696=CARTESIAN_POINT('Ctrl Pts',(2.06350000000023,139.709768001976,14.5738092016242));
#83697=CARTESIAN_POINT('Ctrl Pts',(2.06350000000016,139.73481752449,14.5557291197204));
#83698=CARTESIAN_POINT('Ctrl Pts',(2.06350000000004,139.781451017712,14.5220702994189));
#83699=CARTESIAN_POINT('Ctrl Pts',(2.06350000000018,139.82587360943,14.4853672608473));
#83700=CARTESIAN_POINT('Ctrl Pts',(2.06350000000009,139.867935641536,14.4459285506673));
#83701=CARTESIAN_POINT('Ctrl Pts',(2.06350000000007,139.882253364624,14.4325037943481));
#83702=CARTESIAN_POINT('Ctrl Pts',(2.06349999999999,139.896297210705,14.4187618210828));
#83703=CARTESIAN_POINT('Ctrl Pts',(2.0635,139.910060112663,14.4047141853808));
#83704=CARTESIAN_POINT('Ctrl Pts',(2.0635,139.919224857191,14.3953598360718));
#83705=CARTESIAN_POINT('Ctrl Pts',(2.06350000000004,139.928266229555,14.3858686242349));
#83706=CARTESIAN_POINT('Ctrl Pts',(2.06350000000003,139.937178156248,14.3762480582926));
#83707=CARTESIAN_POINT('Ctrl Pts',(2.0635,139.976265965014,14.3340521499645));
#83708=CARTESIAN_POINT('Ctrl Pts',(2.06350000000006,140.012758651286,14.289488762563));
#83709=CARTESIAN_POINT('Ctrl Pts',(2.06349999999999,140.046512923681,14.2428726644843));
#83710=CARTESIAN_POINT('Ctrl Pts',(2.06349999999994,140.069594989694,14.2109953412078));
#83711=CARTESIAN_POINT('Ctrl Pts',(2.06349999999989,140.091395632075,14.1781574148101));
#83712=CARTESIAN_POINT('Ctrl Pts',(2.06350000000002,140.111855976246,14.1444544521514));
#83713=CARTESIAN_POINT('Ctrl Pts',(2.06350000000009,140.124030465247,14.124400227025));
#83714=CARTESIAN_POINT('Ctrl Pts',(2.06350000000023,140.135730200644,14.1040396688165));
#83715=CARTESIAN_POINT('Ctrl Pts',(2.06350000000009,140.146940838788,14.0833926592231));
#83716=CARTESIAN_POINT('Ctrl Pts',(2.06350000000002,140.152630135659,14.0729144896885));
#83717=CARTESIAN_POINT('Ctrl Pts',(2.0635000000001,140.158194033354,14.062361138362));
#83718=CARTESIAN_POINT('Ctrl Pts',(2.06350000000009,140.163622324462,14.051751955927));
#83719=CARTESIAN_POINT('Ctrl Pts',(2.06350000000008,140.189238203462,14.0016876671563));
#83720=CARTESIAN_POINT('Ctrl Pts',(2.06350000000014,140.21188389594,13.9502997058246));
#83721=CARTESIAN_POINT('Ctrl Pts',(2.06350000000001,140.231416910877,13.8978764178243));
#83722=CARTESIAN_POINT('Ctrl Pts',(2.06349999999989,140.250468168828,13.846746083592));
#83723=CARTESIAN_POINT('Ctrl Pts',(2.06350000000013,140.266558520148,13.7946298218694));
#83724=CARTESIAN_POINT('Ctrl Pts',(2.06350000000017,140.279507455499,13.7417894949803));
#83725=CARTESIAN_POINT('Ctrl Pts',(2.06350000000019,140.287166257202,13.7105364556663));
#83726=CARTESIAN_POINT('Ctrl Pts',(2.06349999999981,140.29372517824,13.6790300876173));
#83727=CARTESIAN_POINT('Ctrl Pts',(2.06349999999983,140.299138330151,13.6473257620931));
#83728=CARTESIAN_POINT('Ctrl Pts',(2.06349999999983,140.302878403847,13.6254204995194));
#83729=CARTESIAN_POINT('Ctrl Pts',(2.06350000000023,140.306071382412,13.6034207594909));
#83730=CARTESIAN_POINT('Ctrl Pts',(2.0635000000002,140.308700255454,13.5813453715114));
#83731=CARTESIAN_POINT('Ctrl Pts',(2.06350000000018,140.309953510264,13.5708214375904));
#83732=CARTESIAN_POINT('Ctrl Pts',(2.06349999999984,140.3110785436,13.5602790505158));
#83733=CARTESIAN_POINT('Ctrl Pts',(2.06349999999987,140.312072069745,13.5497379143829));
#83734=CARTESIAN_POINT('Ctrl Pts',(2.06350000000001,140.317021324794,13.497227196353));
#83735=CARTESIAN_POINT('Ctrl Pts',(2.06350000000023,140.318724308353,13.4446473264495));
#83736=CARTESIAN_POINT('Ctrl Pts',(2.0635000000002,140.31702314186,13.3922422893445));
#83737=CARTESIAN_POINT('Ctrl Pts',(2.0635000000002,140.316671800718,13.3814191008754));
#83738=CARTESIAN_POINT('Ctrl Pts',(2.06350000000014,140.316175081863,13.37060339188));
#83739=CARTESIAN_POINT('Ctrl Pts',(2.06350000000011,140.315531316653,13.3597973595764));
#83740=CARTESIAN_POINT('Ctrl Pts',(2.06349999999993,140.312184859518,13.3036248244557));
#83741=CARTESIAN_POINT('Ctrl Pts',(2.06349999999996,140.304869503365,13.2477115081018));
#83742=CARTESIAN_POINT('Ctrl Pts',(2.0635,140.293769535929,13.1923868892441));
#83743=CARTESIAN_POINT('Ctrl Pts',(2.06350000000001,140.289037860702,13.168803204878));
#83744=CARTESIAN_POINT('Ctrl Pts',(2.06350000000024,140.283617773,13.1453268573598));
#83745=CARTESIAN_POINT('Ctrl Pts',(2.06350000000001,140.277520714535,13.1219853586564));
#83746=CARTESIAN_POINT('Ctrl Pts',(2.06349999999984,140.273131016534,13.1051801843606));
#83747=CARTESIAN_POINT('Ctrl Pts',(2.06350000000026,140.268390372215,13.088444936072));
#83748=CARTESIAN_POINT('Ctrl Pts',(2.06350000000014,140.263302593258,13.0717903762639));
#83749=CARTESIAN_POINT('Ctrl Pts',(2.06350000000007,140.260354166497,13.0621388661973));
#83750=CARTESIAN_POINT('Ctrl Pts',(2.06349999999997,140.257291730647,13.0525230050277));
#83751=CARTESIAN_POINT('Ctrl Pts',(2.06349999999996,140.25411792868,13.0429485488959));
#83752=CARTESIAN_POINT('Ctrl Pts',(2.0634999999999,140.237589408932,12.9930867147718));
#83753=CARTESIAN_POINT('Ctrl Pts',(2.06349999999985,140.21803357519,12.9443107641048));
#83754=CARTESIAN_POINT('Ctrl Pts',(2.06350000000003,140.195622000842,12.8968802651591));
#83755=CARTESIAN_POINT('Ctrl Pts',(2.06350000000021,140.173326992335,12.849696459103));
#83756=CARTESIAN_POINT('Ctrl Pts',(2.06350000000015,140.148205079085,12.8038432496687));
#83757=CARTESIAN_POINT('Ctrl Pts',(2.06350000000018,140.120386075282,12.7596089388244));
#83758=CARTESIAN_POINT('Ctrl Pts',(2.06350000000019,140.106465222191,12.7374737341553));
#83759=CARTESIAN_POINT('Ctrl Pts',(2.06349999999988,140.091868456507,12.7157445125586));
#83760=CARTESIAN_POINT('Ctrl Pts',(2.06349999999998,140.076609269789,12.6944615591124));
#83761=CARTESIAN_POINT('Ctrl Pts',(2.06350000000006,140.06536335881,12.678776175334));
#83762=CARTESIAN_POINT('Ctrl Pts',(2.06349999999983,140.053757610563,12.6633332439248));
#83763=CARTESIAN_POINT('Ctrl Pts',(2.06349999999981,140.041796927407,12.6481500329652));
#83764=CARTESIAN_POINT('Ctrl Pts',(2.0634999999998,140.036011601584,12.6408059856978));
#83765=CARTESIAN_POINT('Ctrl Pts',(2.06349999999992,140.030143780519,12.6335235707603));
#83766=CARTESIAN_POINT('Ctrl Pts',(2.06349999999991,140.024202397352,12.62631448201));
#83767=CARTESIAN_POINT('Ctrl Pts',(2.06349999999989,139.992132527971,12.5874019042322));
#83768=CARTESIAN_POINT('Ctrl Pts',(2.06350000000001,139.957860281516,12.5505432833733));
#83769=CARTESIAN_POINT('Ctrl Pts',(2.06350000000002,139.921515012406,12.5159914507611));
#83770=CARTESIAN_POINT('Ctrl Pts',(2.06350000000004,139.885895513455,12.4821295755946));
#83771=CARTESIAN_POINT('Ctrl Pts',(2.06350000000002,139.84828421327,12.4504826970841));
#83772=CARTESIAN_POINT('Ctrl Pts',(2.06349999999996,139.808779096866,12.4213324380416));
#83773=CARTESIAN_POINT('Ctrl Pts',(2.0634999999999,139.769273980462,12.392182178999));
#83774=CARTESIAN_POINT('Ctrl Pts',(2.06349999999984,139.727874423062,12.3655278554708));
#83775=CARTESIAN_POINT('Ctrl Pts',(2.06349999999994,139.684664424539,12.3417048010816));
#83776=CARTESIAN_POINT('Ctrl Pts',(1.89596885983369,139.853032748447,12.1054162410973));
#83777=CARTESIAN_POINT('Ctrl Pts',(1.92239202009947,140.249693546547,12.3886532696619));
#83778=CARTESIAN_POINT('Ctrl Pts',(1.97523171512371,140.731457227216,13.376929657557));
#83779=CARTESIAN_POINT('Ctrl Pts',(2.05448794490642,139.876218985649,14.7974726129258));
#83780=CARTESIAN_POINT('Ctrl Pts',(2.13373754918179,138.220031131084,14.8484165931406));
#83781=CARTESIAN_POINT('Ctrl Pts',(2.21298715345717,137.276245446404,13.4879812017709));
#83782=CARTESIAN_POINT('Ctrl Pts',(2.29223675773254,137.904992849519,11.9552937639631));
#83783=CARTESIAN_POINT('Ctrl Pts',(2.37148636200791,139.533067892115,11.6499624106074));
#83784=CARTESIAN_POINT('Ctrl Pts',(2.45073596628329,140.674653851833,12.8500720032827));
#83785=CARTESIAN_POINT('Ctrl Pts',(2.52998557055866,140.28820612476,14.4608100243095));
#83786=CARTESIAN_POINT('Ctrl Pts',(2.60923517483404,138.72628924818,15.0123030597136));
#83787=CARTESIAN_POINT('Ctrl Pts',(2.68848477910941,137.414134523873,14.0013890496938));
#83788=CARTESIAN_POINT('Ctrl Pts',(2.76773438338479,137.549031147364,12.3504687424606));
#83789=CARTESIAN_POINT('Ctrl Pts',(2.84698398766016,139.00789645503,11.5659724020108));
#83790=CARTESIAN_POINT('Ctrl Pts',(2.92623359193554,140.459555443865,12.3637232239451));
#83791=CARTESIAN_POINT('Ctrl Pts',(3.0054831962109,140.579413374398,14.0158002212712));
#83792=CARTESIAN_POINT('Ctrl Pts',(3.08473280048628,139.258102654343,15.0147299843183));
#83793=CARTESIAN_POINT('Ctrl Pts',(3.16398240476165,137.701280945341,14.4490191483896));
#83794=CARTESIAN_POINT('Ctrl Pts',(3.24323200903703,137.329502248306,12.8348618994128));
#83795=CARTESIAN_POINT('Ctrl Pts',(3.3224816133124,138.482003811076,11.6451295913287));
#83796=CARTESIAN_POINT('Ctrl Pts',(3.40173121758777,140.107161699214,11.9654179947715));
#83797=CARTESIAN_POINT('Ctrl Pts',(3.48098082186315,140.722066996773,13.5034733719682));
#83798=CARTESIAN_POINT('Ctrl Pts',(3.56023042613852,139.765636634447,14.8558652548918));
#83799=CARTESIAN_POINT('Ctrl Pts',(3.6394800304139,138.110585287296,14.7885757019759));
#83800=CARTESIAN_POINT('Ctrl Pts',(3.71872963468927,137.267098793937,13.363004453076));
#83801=CARTESIAN_POINT('Ctrl Pts',(3.79797923896465,138.00483385609,11.8799434883052));
#83802=CARTESIAN_POINT('Ctrl Pts',(3.87722884324002,139.650628853749,11.6926424649233));
#83803=CARTESIAN_POINT('Ctrl Pts',(3.95647844751539,140.702744093894,12.9720080770802));
#83804=CARTESIAN_POINT('Ctrl Pts',(4.03572805179077,140.201155259721,14.5506567046047));
#83805=CARTESIAN_POINT('Ctrl Pts',(4.11497765606614,138.603547459727,14.9881177488894));
#83806=CARTESIAN_POINT('Ctrl Pts',(4.19422726034152,137.36769098179,13.8852208299455));
#83807=CARTESIAN_POINT('Ctrl Pts',(4.27347686461689,137.621268636156,12.2483270579015));
#83808=CARTESIAN_POINT('Ctrl Pts',(4.35272646889227,139.13289824627,11.5710540184731));
#83809=CARTESIAN_POINT('Ctrl Pts',(4.43197607316764,140.523262102069,12.4713935078738));
#83810=CARTESIAN_POINT('Ctrl Pts',(4.51122567744301,140.523693940408,14.1278121327004));
#83811=CARTESIAN_POINT('Ctrl Pts',(4.59047528171839,139.133799720494,15.0288764520582));
#83812=CARTESIAN_POINT('Ctrl Pts',(4.66972488599376,137.621817178961,14.3523916852465));
#83813=CARTESIAN_POINT('Ctrl Pts',(4.74897449026913,137.367386061086,12.715630355902));
#83814=CARTESIAN_POINT('Ctrl Pts',(4.82822409454451,138.602667312506,11.612089193016));
#83815=CARTESIAN_POINT('Ctrl Pts',(4.90747369881989,140.200502982632,12.0487171742856));
#83816=CARTESIAN_POINT('Ctrl Pts',(4.98672330309525,140.702914895189,13.6271040366256));
#83817=CARTESIAN_POINT('Ctrl Pts',(5.06597290737063,139.651466831615,14.9070180937402));
#83818=CARTESIAN_POINT('Ctrl Pts',(5.14522251164601,138.005574484851,14.7205751631362));
#83819=CARTESIAN_POINT('Ctrl Pts',(5.22447211592137,137.267066055636,13.2378992071656));
#83820=CARTESIAN_POINT('Ctrl Pts',(5.30372172019676,138.109809500551,11.8118880519989));
#83821=CARTESIAN_POINT('Ctrl Pts',(5.38297132447213,139.764824761192,11.7437361569266));
#83822=CARTESIAN_POINT('Ctrl Pts',(5.4622209287475,140.721961748847,13.0956278985068));
#83823=CARTESIAN_POINT('Ctrl Pts',(5.54147053302288,140.107855186128,14.6340062945752));
#83824=CARTESIAN_POINT('Ctrl Pts',(5.62072013729825,138.482871353761,14.9551366430618));
#83825=CARTESIAN_POINT('Ctrl Pts',(5.69996974157362,137.329735497801,13.7660165502442));
#83826=CARTESIAN_POINT('Ctrl Pts',(5.779219345849,137.700701639676,12.1516426964784));
#83827=CARTESIAN_POINT('Ctrl Pts',(5.85846895012437,139.257168003577,11.585167634447));
#83828=CARTESIAN_POINT('Ctrl Pts',(5.93771855439974,140.579123638415,12.5833103492865));
#83829=CARTESIAN_POINT('Ctrl Pts',(6.01696815867512,140.45987057973,14.2356519565008));
#83830=CARTESIAN_POINT('Ctrl Pts',(6.09621776295049,139.009157629426,15.0337420570016));
#83831=CARTESIAN_POINT('Ctrl Pts',(6.17546736722587,137.54878859506,14.2508782232481));
#83832=CARTESIAN_POINT('Ctrl Pts',(6.25472476122387,137.415305990955,12.5981114806508));
#83833=CARTESIAN_POINT('Ctrl Pts',(6.30756562046341,138.286672883565,11.9276015280158));
#83834=CARTESIAN_POINT('Ctrl Pts',(6.33398994494448,138.767973032967,11.8505660727666));
#83835=CARTESIAN_POINT('Ctrl Pts',(1.95222224061816,139.796411161913,12.1847088917025));
#83836=CARTESIAN_POINT('Ctrl Pts',(1.97864540088395,140.166742884434,12.4491455518734));
#83837=CARTESIAN_POINT('Ctrl Pts',(2.03148509590819,140.61652863227,13.371823312847));
#83838=CARTESIAN_POINT('Ctrl Pts',(2.1107413256909,139.818058370819,14.6980751685837));
#83839=CARTESIAN_POINT('Ctrl Pts',(2.18999092996627,138.271802970893,14.7456376502693));
#83840=CARTESIAN_POINT('Ctrl Pts',(2.26924053424165,137.390662762501,13.4755036106089));
#83841=CARTESIAN_POINT('Ctrl Pts',(2.34849013851702,137.977675923223,12.0445510646305));
#83842=CARTESIAN_POINT('Ctrl Pts',(2.42773974279239,139.497684549755,11.7594866303082));
#83843=CARTESIAN_POINT('Ctrl Pts',(2.50698934706777,140.563495683334,12.8799367851997));
#83844=CARTESIAN_POINT('Ctrl Pts',(2.58623895134316,140.202699120838,14.3837591662256));
#83845=CARTESIAN_POINT('Ctrl Pts',(2.66548855561852,138.744457292782,14.8986458571674));
#83846=CARTESIAN_POINT('Ctrl Pts',(2.74473815989389,137.519399203867,13.954833087049));
#83847=CARTESIAN_POINT('Ctrl Pts',(2.82398776416927,137.645341820781,12.4134955915047));
#83848=CARTESIAN_POINT('Ctrl Pts',(2.90323736844464,139.007372313592,11.6810716099503));
#83849=CARTESIAN_POINT('Ctrl Pts',(2.98248697272001,140.362674819976,12.4258702828854));
#83850=CARTESIAN_POINT('Ctrl Pts',(3.06173657699539,140.47457696429,13.9682876911322));
#83851=CARTESIAN_POINT('Ctrl Pts',(3.14098618127076,139.24097062535,14.9009116902761));
#83852=CARTESIAN_POINT('Ctrl Pts',(3.22023578554614,137.787485763937,14.3727509309516));
#83853=CARTESIAN_POINT('Ctrl Pts',(3.29948538982151,137.440384548166,12.8657362793951));
#83854=CARTESIAN_POINT('Ctrl Pts',(3.37873499409688,138.516386741965,11.754974598122));
#83855=CARTESIAN_POINT('Ctrl Pts',(3.45798459837226,140.033671845426,12.054003281367));
#83856=CARTESIAN_POINT('Ctrl Pts',(3.53723420264763,140.607761695303,13.48996746008));
#83857=CARTESIAN_POINT('Ctrl Pts',(3.616483806923,139.714816122536,14.7525918936683));
#83858=CARTESIAN_POINT('Ctrl Pts',(3.69573341119839,138.169621792299,14.6897688061374));
#83859=CARTESIAN_POINT('Ctrl Pts',(3.77498301547375,137.382123235581,13.3588224189182));
#83860=CARTESIAN_POINT('Ctrl Pts',(3.85423261974913,138.070889802988,11.9742022993617));
#83861=CARTESIAN_POINT('Ctrl Pts',(3.9334822240245,139.607442190621,11.799333719075));
#83862=CARTESIAN_POINT('Ctrl Pts',(4.01273182829988,140.589721384936,12.9937791322712));
#83863=CARTESIAN_POINT('Ctrl Pts',(4.09198143257525,140.121426413903,14.4676421111397));
#83864=CARTESIAN_POINT('Ctrl Pts',(4.17123103685062,138.629862711817,14.8760658899505));
#83865=CARTESIAN_POINT('Ctrl Pts',(4.250480641126,137.476038435618,13.8463757423157));
#83866=CARTESIAN_POINT('Ctrl Pts',(4.32973024540137,137.712784416022,12.3181337454002));
#83867=CARTESIAN_POINT('Ctrl Pts',(4.40897984967675,139.124076885584,11.6858159249589));
#83868=CARTESIAN_POINT('Ctrl Pts',(4.48822945395212,140.422152833892,12.5263937576091));
#83869=CARTESIAN_POINT('Ctrl Pts',(4.5674790582275,140.422556008183,14.0728646100041));
#83870=CARTESIAN_POINT('Ctrl Pts',(4.64672866250288,139.124918522831,14.9141191607164));
#83871=CARTESIAN_POINT('Ctrl Pts',(4.72597826677826,137.713296548309,14.2825372898755));
#83872=CARTESIAN_POINT('Ctrl Pts',(4.80522787105361,137.475753754575,12.7544189445367));
#83873=CARTESIAN_POINT('Ctrl Pts',(4.88447747532899,138.629040985953,11.7241273158127));
#83874=CARTESIAN_POINT('Ctrl Pts',(4.96372707960436,140.120817432881,12.1317733276681));
#83875=CARTESIAN_POINT('Ctrl Pts',(5.04297668387974,140.589880848987,13.6053919164879));
#83876=CARTESIAN_POINT('Ctrl Pts',(5.12222628815512,139.608224546196,14.8003493706192));
#83877=CARTESIAN_POINT('Ctrl Pts',(5.2014758924305,138.07158127118,14.6262819256554));
#83878=CARTESIAN_POINT('Ctrl Pts',(5.28072549670586,137.382092670345,13.2420212592459));
#83879=CARTESIAN_POINT('Ctrl Pts',(5.35997510098123,138.168897499796,11.9106641653312));
#83880=CARTESIAN_POINT('Ctrl Pts',(5.43922470525661,139.714058138834,11.8470359751594));
#83881=CARTESIAN_POINT('Ctrl Pts',(5.51847430953198,140.607663433396,13.1091934651874));
#83882=CARTESIAN_POINT('Ctrl Pts',(5.59772391380736,140.034319300897,14.5454592218123));
#83883=CARTESIAN_POINT('Ctrl Pts',(5.67697351808273,138.51719669994,14.845273964481));
#83884=CARTESIAN_POINT('Ctrl Pts',(5.75622312235812,137.440602315305,13.7350838615822));
#83885=CARTESIAN_POINT('Ctrl Pts',(5.83547272663349,137.786944910733,12.2278669827701));
#83886=CARTESIAN_POINT('Ctrl Pts',(5.91472233090886,139.240098013714,11.6989927242281));
#83887=CARTESIAN_POINT('Ctrl Pts',(5.99397193518423,140.474306460055,12.6308819169081));
#83888=CARTESIAN_POINT('Ctrl Pts',(6.0732215394596,140.36296903813,14.173546371085));
#83889=CARTESIAN_POINT('Ctrl Pts',(6.15247114373499,139.008549775264,14.91866180236));
#83890=CARTESIAN_POINT('Ctrl Pts',(6.23172074801035,137.645115368322,14.187761966927));
#83891=CARTESIAN_POINT('Ctrl Pts',(6.31097814200836,137.520492912708,12.6447005964944));
#83892=CARTESIAN_POINT('Ctrl Pts',(6.36381900124789,138.334021256911,12.018696950768));
#83893=CARTESIAN_POINT('Ctrl Pts',(6.39024332572898,138.783374241205,11.9467748627412));
#83894=CARTESIAN_POINT('Ctrl Pts',(2.00847562140265,139.739789575378,12.2640015423077));
#83895=CARTESIAN_POINT('Ctrl Pts',(2.03489878166844,140.083792222322,12.509637834085));
#83896=CARTESIAN_POINT('Ctrl Pts',(2.08773847669269,140.501600037324,13.3667169681371));
#83897=CARTESIAN_POINT('Ctrl Pts',(2.16699470647539,139.759897755991,14.5986777242415));
#83898=CARTESIAN_POINT('Ctrl Pts',(2.24624431075077,138.323574810704,14.6428587073981));
#83899=CARTESIAN_POINT('Ctrl Pts',(2.32549391502614,137.505080078599,13.4630260194469));
#83900=CARTESIAN_POINT('Ctrl Pts',(2.40474351930151,138.050358996926,12.1338083652978));
#83901=CARTESIAN_POINT('Ctrl Pts',(2.48399312357689,139.462301207396,11.8690108500091));
#83902=CARTESIAN_POINT('Ctrl Pts',(2.56324272785226,140.452337514835,12.9098015671167));
#83903=CARTESIAN_POINT('Ctrl Pts',(2.64249233212764,140.117192116915,14.3067083081417));
#83904=CARTESIAN_POINT('Ctrl Pts',(2.72174193640301,138.762625337382,14.7849886546212));
#83905=CARTESIAN_POINT('Ctrl Pts',(2.80099154067839,137.624663883859,13.908277124404));
#83906=CARTESIAN_POINT('Ctrl Pts',(2.88024114495376,137.741652494196,12.4765224405487));
#83907=CARTESIAN_POINT('Ctrl Pts',(2.95949074922913,139.006848172153,11.7961708178899));
#83908=CARTESIAN_POINT('Ctrl Pts',(3.03874035350451,140.265794196088,12.4880173418254));
#83909=CARTESIAN_POINT('Ctrl Pts',(3.11798995777988,140.369740554181,13.9207751609933));
#83910=CARTESIAN_POINT('Ctrl Pts',(3.19723956205525,139.223838596359,14.7870933962339));
#83911=CARTESIAN_POINT('Ctrl Pts',(3.27648916633063,137.873690582534,14.2964827135134));
#83912=CARTESIAN_POINT('Ctrl Pts',(3.355738770606,137.551266848025,12.8966106593774));
#83913=CARTESIAN_POINT('Ctrl Pts',(3.43498837488138,138.550769672853,11.864819604915));
#83914=CARTESIAN_POINT('Ctrl Pts',(3.51423797915675,139.960181991637,12.1425885679623));
#83915=CARTESIAN_POINT('Ctrl Pts',(3.59348758343212,140.493456393832,13.4764615481916));
#83916=CARTESIAN_POINT('Ctrl Pts',(3.6727371877075,139.663995610628,14.6493185324447));
#83917=CARTESIAN_POINT('Ctrl Pts',(3.75198679198287,138.2286582973,14.590961910299));
#83918=CARTESIAN_POINT('Ctrl Pts',(3.83123639625824,137.497147677226,13.35464038476));
#83919=CARTESIAN_POINT('Ctrl Pts',(3.91048600053362,138.136945749885,12.0684611104179));
#83920=CARTESIAN_POINT('Ctrl Pts',(3.98973560480899,139.564255527493,11.9060249732265));
#83921=CARTESIAN_POINT('Ctrl Pts',(4.06898520908437,140.476698675979,13.0155501874623));
#83922=CARTESIAN_POINT('Ctrl Pts',(4.14823481335974,140.041697568084,14.3846275176746));
#83923=CARTESIAN_POINT('Ctrl Pts',(4.22748441763512,138.656177963905,14.7640140310118));
#83924=CARTESIAN_POINT('Ctrl Pts',(4.30673402191049,137.584385889446,13.8075306546858));
#83925=CARTESIAN_POINT('Ctrl Pts',(4.38598362618586,137.804300195889,12.3879404328989));
#83926=CARTESIAN_POINT('Ctrl Pts',(4.46523323046124,139.115255524898,11.8005778314444));
#83927=CARTESIAN_POINT('Ctrl Pts',(4.54448283473661,140.321043565714,12.5813940073443));
#83928=CARTESIAN_POINT('Ctrl Pts',(4.62373243901199,140.321418075957,14.0179170873078));
#83929=CARTESIAN_POINT('Ctrl Pts',(4.70298204328736,139.116037325168,14.7993618693745));
#83930=CARTESIAN_POINT('Ctrl Pts',(4.78223164756273,137.804775917658,14.2126828945046));
#83931=CARTESIAN_POINT('Ctrl Pts',(4.86148125183811,137.584121448064,12.7932075331713));
#83932=CARTESIAN_POINT('Ctrl Pts',(4.94073085611348,138.655414659402,11.8361654386095));
#83933=CARTESIAN_POINT('Ctrl Pts',(5.01998046038886,140.041131883128,12.2148294810507));
#83934=CARTESIAN_POINT('Ctrl Pts',(5.09923006466423,140.476846802786,13.5836797963504));
#83935=CARTESIAN_POINT('Ctrl Pts',(5.17847966893961,139.564982260777,14.6936806474984));
#83936=CARTESIAN_POINT('Ctrl Pts',(5.25772927321498,138.137588057508,14.5319886881745));
#83937=CARTESIAN_POINT('Ctrl Pts',(5.33697887749035,137.497119285054,13.2461433113263));
#83938=CARTESIAN_POINT('Ctrl Pts',(5.41622848176573,138.227985499041,12.0094402786633));
#83939=CARTESIAN_POINT('Ctrl Pts',(5.4954780860411,139.663291516476,11.950335793392));
#83940=CARTESIAN_POINT('Ctrl Pts',(5.57472769031648,140.493365117947,13.1227590318682));
#83941=CARTESIAN_POINT('Ctrl Pts',(5.65397729459185,139.960783415665,14.4569121490495));
#83942=CARTESIAN_POINT('Ctrl Pts',(5.73322689886722,138.551522046119,14.7354112859003));
#83943=CARTESIAN_POINT('Ctrl Pts',(5.8124765031426,137.551469132808,13.7041511729202));
#83944=CARTESIAN_POINT('Ctrl Pts',(5.89172610741797,137.873188181787,12.3040912690618));
#83945=CARTESIAN_POINT('Ctrl Pts',(5.97097571169335,139.223028023853,11.8128178140093));
#83946=CARTESIAN_POINT('Ctrl Pts',(6.05022531596872,140.369489281695,12.6784534845299));
#83947=CARTESIAN_POINT('Ctrl Pts',(6.1294749202441,140.266067496531,14.1114407856692));
#83948=CARTESIAN_POINT('Ctrl Pts',(6.20872452451946,139.0079419211,14.8035815477182));
#83949=CARTESIAN_POINT('Ctrl Pts',(6.28797412879484,137.741442141584,14.1246457106057));
#83950=CARTESIAN_POINT('Ctrl Pts',(6.36723152279283,137.625679834461,12.6912897123383));
#83951=CARTESIAN_POINT('Ctrl Pts',(6.42007238203238,138.381369630258,12.1097923735202));
#83952=CARTESIAN_POINT('Ctrl Pts',(6.44649670651346,138.798775449443,12.0429836527158));
#83953=CARTESIAN_POINT('Ctrl Pts',(2.06472900218714,139.683167988843,12.3432941929129));
#83954=CARTESIAN_POINT('Ctrl Pts',(2.09115216245292,140.000841560209,12.5701301162965));
#83955=CARTESIAN_POINT('Ctrl Pts',(2.14399185747717,140.386671442379,13.3616106234272));
#83956=CARTESIAN_POINT('Ctrl Pts',(2.22324808725986,139.701737141161,14.4992802798993));
#83957=CARTESIAN_POINT('Ctrl Pts',(2.30249769153524,138.375346650514,14.5400797645268));
#83958=CARTESIAN_POINT('Ctrl Pts',(2.38174729581061,137.619497394696,13.4505484282849));
#83959=CARTESIAN_POINT('Ctrl Pts',(2.46099690008598,138.123042070629,12.2230656659651));
#83960=CARTESIAN_POINT('Ctrl Pts',(2.54024650436136,139.426917865036,11.97853506971));
#83961=CARTESIAN_POINT('Ctrl Pts',(2.61949610863673,140.341179346336,12.9396663490336));
#83962=CARTESIAN_POINT('Ctrl Pts',(2.69874571291211,140.031685112994,14.2296574500578));
#83963=CARTESIAN_POINT('Ctrl Pts',(2.77799531718748,138.780793381982,14.6713314520748));
#83964=CARTESIAN_POINT('Ctrl Pts',(2.85724492146286,137.729928563852,13.8617211617591));
#83965=CARTESIAN_POINT('Ctrl Pts',(2.93649452573823,137.837963167611,12.5395492895927));
#83966=CARTESIAN_POINT('Ctrl Pts',(3.0157441300136,139.006324030715,11.9112700258293));
#83967=CARTESIAN_POINT('Ctrl Pts',(3.09499373428898,140.1689135722,12.5501644007656));
#83968=CARTESIAN_POINT('Ctrl Pts',(3.17424333856435,140.264904144072,13.8732626308543));
#83969=CARTESIAN_POINT('Ctrl Pts',(3.25349294283972,139.206706567366,14.6732751021918));
#83970=CARTESIAN_POINT('Ctrl Pts',(3.3327425471151,137.959895401132,14.2202144960755));
#83971=CARTESIAN_POINT('Ctrl Pts',(3.41199215139047,137.662149147884,12.9274850393596));
#83972=CARTESIAN_POINT('Ctrl Pts',(3.49124175566585,138.585152603743,11.9746646117082));
#83973=CARTESIAN_POINT('Ctrl Pts',(3.57049135994122,139.88669213785,12.2311738545576));
#83974=CARTESIAN_POINT('Ctrl Pts',(3.6497409642166,140.37915109236,13.4629556363033));
#83975=CARTESIAN_POINT('Ctrl Pts',(3.72899056849197,139.613175098719,14.5460451712212));
#83976=CARTESIAN_POINT('Ctrl Pts',(3.80824017276735,138.287694802302,14.4921550144606));
#83977=CARTESIAN_POINT('Ctrl Pts',(3.88748977704271,137.612172118871,13.350458350602));
#83978=CARTESIAN_POINT('Ctrl Pts',(3.9667393813181,138.203001696784,12.1627199214744));
#83979=CARTESIAN_POINT('Ctrl Pts',(4.04598898559346,139.521068864365,12.0127162273781));
#83980=CARTESIAN_POINT('Ctrl Pts',(4.12523858986884,140.363675967023,13.0373212426534));
#83981=CARTESIAN_POINT('Ctrl Pts',(4.20448819414421,139.961968722265,14.3016129242096));
#83982=CARTESIAN_POINT('Ctrl Pts',(4.28373779841958,138.682493215994,14.651962172073));
#83983=CARTESIAN_POINT('Ctrl Pts',(4.36298740269496,137.692733343272,13.768685567056));
#83984=CARTESIAN_POINT('Ctrl Pts',(4.44223700697033,137.895815975755,12.4577471203976));
#83985=CARTESIAN_POINT('Ctrl Pts',(4.52148661124571,139.106434164211,11.9153397379301));
#83986=CARTESIAN_POINT('Ctrl Pts',(4.60073621552108,140.219934297536,12.6363942570796));
#83987=CARTESIAN_POINT('Ctrl Pts',(4.67998581979646,140.220280143731,13.9629695646115));
#83988=CARTESIAN_POINT('Ctrl Pts',(4.75923542407183,139.107156127504,14.6846045780327));
#83989=CARTESIAN_POINT('Ctrl Pts',(4.8384850283472,137.896255287007,14.1428284991337));
#83990=CARTESIAN_POINT('Ctrl Pts',(4.91773463262258,137.692489141553,12.831996121806));
#83991=CARTESIAN_POINT('Ctrl Pts',(4.99698423689795,138.681788332849,11.9482035614062));
#83992=CARTESIAN_POINT('Ctrl Pts',(5.07623384117334,139.961446333378,12.2978856344331));
#83993=CARTESIAN_POINT('Ctrl Pts',(5.1554834454487,140.363812756586,13.5619676762128));
#83994=CARTESIAN_POINT('Ctrl Pts',(5.23473304972408,139.521739975356,14.5870119243775));
#83995=CARTESIAN_POINT('Ctrl Pts',(5.31398265399944,138.203594843837,14.4376954506937));
#83996=CARTESIAN_POINT('Ctrl Pts',(5.39323225827483,137.612145899761,13.2502653634066));
#83997=CARTESIAN_POINT('Ctrl Pts',(5.4724818625502,138.287073498288,12.1082163919956));
#83998=CARTESIAN_POINT('Ctrl Pts',(5.55173146682557,139.612524894117,12.0536356116246));
#83999=CARTESIAN_POINT('Ctrl Pts',(5.63098107110095,140.379066802497,13.136324598549));
#84000=CARTESIAN_POINT('Ctrl Pts',(5.71023067537633,139.887247530433,14.3683650762867));
#84001=CARTESIAN_POINT('Ctrl Pts',(5.78948027965169,138.585847392298,14.6255486073194));
#84002=CARTESIAN_POINT('Ctrl Pts',(5.86872988392707,137.662335950312,13.6732184842583));
#84003=CARTESIAN_POINT('Ctrl Pts',(5.94797948820244,137.959431452842,12.3803155553536));
#84004=CARTESIAN_POINT('Ctrl Pts',(6.02722909247781,139.205958033989,11.9266429037905));
#84005=CARTESIAN_POINT('Ctrl Pts',(6.10647869675319,140.264672103334,12.7260250521515));
#84006=CARTESIAN_POINT('Ctrl Pts',(6.18572830102857,140.169165954932,14.0493352002535));
#84007=CARTESIAN_POINT('Ctrl Pts',(6.26497790530394,139.007334066938,14.6885012930766));
#84008=CARTESIAN_POINT('Ctrl Pts',(6.34422750957932,137.837768914846,14.0615294542845));
#84009=CARTESIAN_POINT('Ctrl Pts',(6.42348490357732,137.730866756214,12.7378788281818));
#84010=CARTESIAN_POINT('Ctrl Pts',(6.47632576281685,138.428718003605,12.2008877962723));
#84011=CARTESIAN_POINT('Ctrl Pts',(6.50275008729793,138.814176657679,12.1391924426906));
#84012=CARTESIAN_POINT('Ctrl Pts',(2.06350000000012,139.657803339705,14.6073358467789));
#84013=CARTESIAN_POINT('Ctrl Pts',(2.06364329234591,139.653977763695,14.6094211449295));
#84014=CARTESIAN_POINT('Ctrl Pts',(2.06378605389376,139.650142629059,14.6114889008338));
#84015=CARTESIAN_POINT('Ctrl Pts',(2.06407023080022,139.642462904297,14.6155842536617));
#84016=CARTESIAN_POINT('Ctrl Pts',(2.06421164723845,139.638618396783,14.6176119166426));
#84017=CARTESIAN_POINT('Ctrl Pts',(2.06435259587952,139.634764697661,14.6196220306061));
#84018=CARTESIAN_POINT('Origin',(6.5,139.,13.3));
#84019=CARTESIAN_POINT('',(6.4,138.189703570316,13.3965254145956));
#84020=CARTESIAN_POINT('',(6.45000000000003,138.133974596216,13.3));
#84021=CARTESIAN_POINT('Ctrl Pts',(6.4,138.189703570316,13.3965254145956));
#84022=CARTESIAN_POINT('Ctrl Pts',(6.42130722384788,138.162667372368,13.3496973461057));
#84023=CARTESIAN_POINT('Ctrl Pts',(6.45000000000003,138.133974596216,13.3));
#84024=CARTESIAN_POINT('',(6.4,138.511258324007,13.9534745854044));
#84025=CARTESIAN_POINT('Origin',(6.4,139.,13.3));
#84026=CARTESIAN_POINT('',(6.45000000000001,138.566987298108,14.05));
#84027=CARTESIAN_POINT('Ctrl Pts',(6.45000000000001,138.566987298108,14.05));
#84028=CARTESIAN_POINT('Ctrl Pts',(6.42130722384786,138.538294521956,14.0003026538943));
#84029=CARTESIAN_POINT('Ctrl Pts',(6.4,138.511258324007,13.9534745854044));
#84030=CARTESIAN_POINT('',(6.4,138.678445246309,14.05));
#84031=CARTESIAN_POINT('Ctrl Pts',(6.4,138.678445246309,14.05));
#84032=CARTESIAN_POINT('Ctrl Pts',(6.42130722384789,138.624372850412,14.05));
#84033=CARTESIAN_POINT('Ctrl Pts',(6.45000000000001,138.566987298108,14.05));
#84034=CARTESIAN_POINT('',(6.4,139.321554753691,14.05));
#84035=CARTESIAN_POINT('Origin',(6.4,139.,13.3));
#84036=CARTESIAN_POINT('',(6.45,139.433012701892,14.05));
#84037=CARTESIAN_POINT('Ctrl Pts',(6.45,139.433012701892,14.05));
#84038=CARTESIAN_POINT('Ctrl Pts',(6.42130722384791,139.375627149588,14.05));
#84039=CARTESIAN_POINT('Ctrl Pts',(6.4,139.321554753691,14.05));
#84040=CARTESIAN_POINT('',(6.4,139.488741675993,13.9534745854044));
#84041=CARTESIAN_POINT('Ctrl Pts',(6.4,139.488741675993,13.9534745854044));
#84042=CARTESIAN_POINT('Ctrl Pts',(6.4213072238479,139.461705478044,14.0003026538944));
#84043=CARTESIAN_POINT('Ctrl Pts',(6.45,139.433012701892,14.05));
#84044=CARTESIAN_POINT('',(6.4,139.810296429684,13.3965254145956));
#84045=CARTESIAN_POINT('Origin',(6.4,139.,13.3));
#84046=CARTESIAN_POINT('',(6.45000000000003,139.866025403784,13.3));
#84047=CARTESIAN_POINT('Ctrl Pts',(6.45000000000003,139.866025403784,13.3));
#84048=CARTESIAN_POINT('Ctrl Pts',(6.42130722384793,139.837332627632,13.3496973461056));
#84049=CARTESIAN_POINT('Ctrl Pts',(6.4,139.810296429684,13.3965254145956));
#84050=CARTESIAN_POINT('',(6.4,139.810296429684,13.2034745854044));
#84051=CARTESIAN_POINT('Ctrl Pts',(6.4,139.810296429684,13.2034745854044));
#84052=CARTESIAN_POINT('Ctrl Pts',(6.42130722384792,139.837332627632,13.2503026538944));
#84053=CARTESIAN_POINT('Ctrl Pts',(6.45000000000003,139.866025403784,13.3));
#84054=CARTESIAN_POINT('',(6.4,139.488741675993,12.6465254145956));
#84055=CARTESIAN_POINT('Origin',(6.4,139.,13.3));
#84056=CARTESIAN_POINT('',(6.45,139.433012701892,12.55));
#84057=CARTESIAN_POINT('Ctrl Pts',(6.45,139.433012701892,12.55));
#84058=CARTESIAN_POINT('Ctrl Pts',(6.42130722384787,139.461705478044,12.5996973461056));
#84059=CARTESIAN_POINT('Ctrl Pts',(6.4,139.488741675993,12.6465254145956));
#84060=CARTESIAN_POINT('',(6.4,139.321554753691,12.55));
#84061=CARTESIAN_POINT('Ctrl Pts',(6.4,139.321554753691,12.55));
#84062=CARTESIAN_POINT('Ctrl Pts',(6.4213072238479,139.375627149588,12.55));
#84063=CARTESIAN_POINT('Ctrl Pts',(6.45,139.433012701892,12.55));
#84064=CARTESIAN_POINT('',(6.4,138.678445246309,12.55));
#84065=CARTESIAN_POINT('Origin',(6.4,139.,13.3));
#84066=CARTESIAN_POINT('',(6.45000000000001,138.566987298108,12.55));
#84067=CARTESIAN_POINT('Ctrl Pts',(6.45000000000001,138.566987298108,12.55));
#84068=CARTESIAN_POINT('Ctrl Pts',(6.4213072238479,138.624372850412,12.55));
#84069=CARTESIAN_POINT('Ctrl Pts',(6.4,138.678445246309,12.55));
#84070=CARTESIAN_POINT('',(6.4,138.511258324007,12.6465254145956));
#84071=CARTESIAN_POINT('Ctrl Pts',(6.39999999999999,138.511258324007,12.6465254145956));
#84072=CARTESIAN_POINT('Ctrl Pts',(6.42130722384788,138.538294521956,12.5996973461056));
#84073=CARTESIAN_POINT('Ctrl Pts',(6.45000000000001,138.566987298108,12.55));
#84074=CARTESIAN_POINT('',(6.4,138.189703570316,13.2034745854044));
#84075=CARTESIAN_POINT('Origin',(6.4,139.,13.3));
#84076=CARTESIAN_POINT('Ctrl Pts',(6.45000000000003,138.133974596216,13.3));
#84077=CARTESIAN_POINT('Ctrl Pts',(6.42130722384786,138.162667372368,13.2503026538943));
#84078=CARTESIAN_POINT('Ctrl Pts',(6.4,138.189703570316,13.2034745854043));
#84079=CARTESIAN_POINT('',(6.6,137.983974596216,13.3));
#84080=CARTESIAN_POINT('',(6.5,138.083974596216,13.3));
#84081=CARTESIAN_POINT('Origin',(6.6,139.,13.3));
#84082=CARTESIAN_POINT('Origin',(6.5,139.,13.3));
#84083=CARTESIAN_POINT('',(6.6,138.678445246309,12.55));
#84084=CARTESIAN_POINT('',(6.5,138.678445246309,12.55));
#84085=CARTESIAN_POINT('',(6.6,139.321554753691,12.55));
#84086=CARTESIAN_POINT('',(6.5,139.321554753691,12.55));
#84087=CARTESIAN_POINT('Origin',(6.6,139.,13.3));
#84088=CARTESIAN_POINT('Origin',(6.5,139.,13.3));
#84089=CARTESIAN_POINT('',(6.6,139.810296429684,13.2034745854044));
#84090=CARTESIAN_POINT('',(6.5,139.810296429684,13.2034745854044));
#84091=CARTESIAN_POINT('',(6.6,139.488741675993,12.6465254145956));
#84092=CARTESIAN_POINT('Origin',(6.6,139.,13.3));
#84093=CARTESIAN_POINT('',(6.5,139.488741675993,12.6465254145956));
#84094=CARTESIAN_POINT('Origin',(6.5,139.,13.3));
#84095=CARTESIAN_POINT('',(6.6,138.189703570316,13.2034745854044));
#84096=CARTESIAN_POINT('',(6.5,138.189703570316,13.2034745854044));
#84097=CARTESIAN_POINT('',(6.6,138.511258324007,12.6465254145956));
#84098=CARTESIAN_POINT('',(6.5,138.511258324007,12.6465254145956));
#84099=CARTESIAN_POINT('Origin',(6.6,139.,13.3));
#84100=CARTESIAN_POINT('Origin',(6.5,139.,13.3));
#84101=CARTESIAN_POINT('',(6.6,139.488741675993,13.9534745854044));
#84102=CARTESIAN_POINT('',(6.5,139.488741675993,13.9534745854044));
#84103=CARTESIAN_POINT('',(6.6,139.810296429684,13.3965254145956));
#84104=CARTESIAN_POINT('Origin',(6.6,139.,13.3));
#84105=CARTESIAN_POINT('',(6.5,139.810296429684,13.3965254145956));
#84106=CARTESIAN_POINT('Origin',(6.5,139.,13.3));
#84107=CARTESIAN_POINT('',(6.6,138.511258324007,13.9534745854044));
#84108=CARTESIAN_POINT('',(6.5,138.511258324007,13.9534745854044));
#84109=CARTESIAN_POINT('',(6.6,138.189703570316,13.3965254145956));
#84110=CARTESIAN_POINT('',(6.5,138.189703570316,13.3965254145956));
#84111=CARTESIAN_POINT('Origin',(6.6,139.,13.3));
#84112=CARTESIAN_POINT('Origin',(6.5,139.,13.3));
#84113=CARTESIAN_POINT('',(6.6,138.678445246309,14.05));
#84114=CARTESIAN_POINT('',(6.5,138.678445246309,14.05));
#84115=CARTESIAN_POINT('',(6.6,139.321554753691,14.05));
#84116=CARTESIAN_POINT('Origin',(6.6,139.,13.3));
#84117=CARTESIAN_POINT('',(6.5,139.321554753691,14.05));
#84118=CARTESIAN_POINT('Origin',(6.6,138.133974596216,13.3));
#84119=CARTESIAN_POINT('',(6.6,138.242227771689,13.4875));
#84120=CARTESIAN_POINT('',(5.1,138.133974596216,13.3));
#84121=CARTESIAN_POINT('',(6.6,138.133974596216,13.3));
#84122=CARTESIAN_POINT('',(5.1,138.566987298108,14.05));
#84123=CARTESIAN_POINT('',(5.1,138.566987298108,14.05));
#84124=CARTESIAN_POINT('',(6.6,138.566987298108,14.05));
#84125=CARTESIAN_POINT('Origin',(6.6,138.566987298108,12.55));
#84126=CARTESIAN_POINT('',(6.6,138.458734122635,12.7375));
#84127=CARTESIAN_POINT('',(5.1,138.566987298108,12.55));
#84128=CARTESIAN_POINT('',(6.6,138.566987298108,12.55));
#84129=CARTESIAN_POINT('',(5.1,138.133974596216,13.3));
#84130=CARTESIAN_POINT('Origin',(6.6,139.433012701892,12.55));
#84131=CARTESIAN_POINT('',(6.6,139.216506350946,12.55));
#84132=CARTESIAN_POINT('',(5.1,139.433012701892,12.55));
#84133=CARTESIAN_POINT('',(6.6,139.433012701892,12.55));
#84134=CARTESIAN_POINT('',(5.1,138.566987298108,12.55));
#84135=CARTESIAN_POINT('Origin',(6.6,139.,13.3));
#84136=CARTESIAN_POINT('Origin',(6.6,139.,13.3));
#84137=CARTESIAN_POINT('Origin',(6.6,139.,13.3));
#84138=CARTESIAN_POINT('',(6.6,139.757772228311,13.1125));
#84139=CARTESIAN_POINT('Origin',(6.6,139.,13.3));
#84140=CARTESIAN_POINT('Origin',(6.6,139.,13.3));
#84141=CARTESIAN_POINT('',(6.6,139.541265877365,13.8625));
#84142=CARTESIAN_POINT('Origin',(6.6,139.,13.3));
#84143=CARTESIAN_POINT('',(6.6,138.783493649054,14.05));
#84144=CARTESIAN_POINT('Origin',(5.1,139.,13.3));
#84145=CARTESIAN_POINT('',(5.1,139.433012701892,14.05));
#84146=CARTESIAN_POINT('',(5.1,139.866025403784,13.3));
#84147=CARTESIAN_POINT('',(5.1,139.866025403784,13.3));
#84148=CARTESIAN_POINT('Origin',(5.1,139.,13.3));
#84149=CARTESIAN_POINT('Origin',(5.1,139.,13.3));
#84150=CARTESIAN_POINT('',(5.1,139.433012701892,12.55));
#84151=CARTESIAN_POINT('Origin',(5.1,139.,13.3));
#84152=CARTESIAN_POINT('Origin',(5.1,139.,13.3));
#84153=CARTESIAN_POINT('Origin',(5.1,139.,13.3));
#84154=CARTESIAN_POINT('Origin',(5.1,139.,13.3));
#84155=CARTESIAN_POINT('Origin',(5.1,139.,13.3));
#84156=CARTESIAN_POINT('Origin',(5.1,139.,13.3));
#84157=CARTESIAN_POINT('Origin',(5.1,139.,13.3));
#84158=CARTESIAN_POINT('Origin',(5.1,139.,13.3));
#84159=CARTESIAN_POINT('',(5.1,139.433012701892,14.05));
#84160=CARTESIAN_POINT('Origin',(5.1,139.,13.3));
#84161=CARTESIAN_POINT('Origin',(4.83981971989424,139.,13.3));
#84162=CARTESIAN_POINT('',(4.57963943978849,139.,13.3));
#84163=CARTESIAN_POINT('',(4.83981971989424,138.566987298108,13.3));
#84164=CARTESIAN_POINT('Origin',(6.6,139.433012701892,14.05));
#84165=CARTESIAN_POINT('',(6.6,139.433012701892,14.05));
#84166=CARTESIAN_POINT('',(6.6,139.866025403784,13.3));
#84167=CARTESIAN_POINT('Origin',(6.6,138.566987298108,14.05));
#84168=CARTESIAN_POINT('Origin',(6.6,139.866025403784,13.3));
#84169=CARTESIAN_POINT('Origin',(1.6,140.,13.3));
#84170=CARTESIAN_POINT('',(1.6,138.,13.3));
#84171=CARTESIAN_POINT('Origin',(1.6,139.,13.3));
#84172=CARTESIAN_POINT('Origin',(1.85,139.,13.3));
#84173=CARTESIAN_POINT('',(1.85,137.75,13.3));
#84174=CARTESIAN_POINT('Origin',(6.45,139.,13.3));
#84175=CARTESIAN_POINT('',(6.6,137.8,13.3));
#84176=CARTESIAN_POINT('',(6.45,137.65,13.3));
#84177=CARTESIAN_POINT('Origin',(6.6,139.,13.3));
#84178=CARTESIAN_POINT('Origin',(6.6,139.,13.3));
#84179=CARTESIAN_POINT('',(0.,0.,0.));
#84180=CARTESIAN_POINT('Origin',(-17.425,15.,5.5));
#84181=CARTESIAN_POINT('',(-17.35,15.,6.55));
#84182=CARTESIAN_POINT('Origin',(-17.35,15.,5.5));
#84183=CARTESIAN_POINT('',(-17.5,15.,6.7));
#84184=CARTESIAN_POINT('',(-17.425,15.,6.625));
#84185=CARTESIAN_POINT('Origin',(-17.5,15.,5.5));
#84186=CARTESIAN_POINT('Origin',(-17.5,15.,5.5));
#84187=CARTESIAN_POINT('',(-13.5,15.,6.55));
#84188=CARTESIAN_POINT('',(-17.5,15.,6.55));
#84189=CARTESIAN_POINT('',(-13.5,13.95,5.5));
#84190=CARTESIAN_POINT('Origin',(-13.5,15.,5.5));
#84191=CARTESIAN_POINT('Origin',(-13.5,15.,5.5));
#84192=CARTESIAN_POINT('Origin',(-17.5,10.,0.));
#84193=CARTESIAN_POINT('',(-17.5,10.,0.5));
#84194=CARTESIAN_POINT('',(-17.5,20.,0.5));
#84195=CARTESIAN_POINT('',(-17.5,10.,0.5));
#84196=CARTESIAN_POINT('',(-17.5,10.,15.5));
#84197=CARTESIAN_POINT('',(-17.5,10.,16.));
#84198=CARTESIAN_POINT('',(-17.5,20.,15.5));
#84199=CARTESIAN_POINT('',(-17.5,10.,15.5));
#84200=CARTESIAN_POINT('',(-17.5,20.,16.));
#84201=CARTESIAN_POINT('Origin',(-13.5,15.,5.5));
#84202=CARTESIAN_POINT('',(-12.8690963500211,15.,5.5));
#84203=CARTESIAN_POINT('',(-13.5,13.95,5.5));
#84204=CARTESIAN_POINT('Origin',(17.425,15.,5.5));
#84205=CARTESIAN_POINT('',(17.35,15.,6.55));
#84206=CARTESIAN_POINT('Origin',(17.35,15.,5.5));
#84207=CARTESIAN_POINT('',(17.5,15.,6.7));
#84208=CARTESIAN_POINT('',(17.425,15.,6.625));
#84209=CARTESIAN_POINT('Origin',(17.5,15.,5.5));
#84210=CARTESIAN_POINT('Origin',(17.5,15.,5.5));
#84211=CARTESIAN_POINT('',(13.5,15.,6.55));
#84212=CARTESIAN_POINT('',(17.5,15.,6.55));
#84213=CARTESIAN_POINT('',(13.5,13.95,5.5));
#84214=CARTESIAN_POINT('Origin',(13.5,15.,5.5));
#84215=CARTESIAN_POINT('Origin',(13.5,15.,5.5));
#84216=CARTESIAN_POINT('Origin',(17.5,10.,16.));
#84217=CARTESIAN_POINT('',(17.5,10.,15.5));
#84218=CARTESIAN_POINT('',(17.5,20.,15.5));
#84219=CARTESIAN_POINT('',(17.5,10.,15.5));
#84220=CARTESIAN_POINT('',(17.5,10.,0.5));
#84221=CARTESIAN_POINT('',(17.5,10.,0.));
#84222=CARTESIAN_POINT('',(17.5,20.,0.5));
#84223=CARTESIAN_POINT('',(17.5,10.,0.5));
#84224=CARTESIAN_POINT('',(17.5,20.,0.));
#84225=CARTESIAN_POINT('Origin',(13.1845481750105,15.,5.5));
#84226=CARTESIAN_POINT('',(12.8690963500211,15.,5.5));
#84227=CARTESIAN_POINT('',(13.1845481750105,14.475,5.5));
#84228=CARTESIAN_POINT('Origin',(10.,10.1,11.));
#84229=CARTESIAN_POINT('',(8.45,10.2,11.));
#84230=CARTESIAN_POINT('Origin',(10.,10.2,11.));
#84231=CARTESIAN_POINT('',(8.25,10.,11.));
#84232=CARTESIAN_POINT('',(8.35,10.1,11.));
#84233=CARTESIAN_POINT('Origin',(10.,10.,11.));
#84234=CARTESIAN_POINT('Origin',(0.,10.,8.));
#84235=CARTESIAN_POINT('',(17.,10.,16.));
#84236=CARTESIAN_POINT('',(14.875,10.,18.125));
#84237=CARTESIAN_POINT('',(-17.,10.,16.));
#84238=CARTESIAN_POINT('',(17.5,10.,16.));
#84239=CARTESIAN_POINT('',(-14.875,10.,18.125));
#84240=CARTESIAN_POINT('',(-17.,10.,0.));
#84241=CARTESIAN_POINT('',(-14.875,10.,-2.12499999999999));
#84242=CARTESIAN_POINT('',(17.,10.,0.));
#84243=CARTESIAN_POINT('',(-17.5,10.,0.));
#84244=CARTESIAN_POINT('',(14.875,10.,-2.12499999999999));
#84245=CARTESIAN_POINT('',(-11.75,10.,11.));
#84246=CARTESIAN_POINT('Origin',(-10.,10.,11.));
#84247=CARTESIAN_POINT('',(-13.3,10.,3.5));
#84248=CARTESIAN_POINT('Origin',(-10.,10.,3.5));
#84249=CARTESIAN_POINT('',(-2.315,10.,13.3));
#84250=CARTESIAN_POINT('Origin',(0.,10.,13.3));
#84251=CARTESIAN_POINT('',(6.7,10.,3.5));
#84252=CARTESIAN_POINT('Origin',(10.,10.,3.5));
#84253=CARTESIAN_POINT('Origin',(10.,10.,11.));
#84254=CARTESIAN_POINT('',(8.45,16.,11.));
#84255=CARTESIAN_POINT('',(8.45,10.,11.));
#84256=CARTESIAN_POINT('Origin',(10.,16.,11.));
#84257=CARTESIAN_POINT('Origin',(-10.,10.1,11.));
#84258=CARTESIAN_POINT('',(-11.55,10.2,11.));
#84259=CARTESIAN_POINT('Origin',(-10.,10.2,11.));
#84260=CARTESIAN_POINT('',(-11.65,10.1,11.));
#84261=CARTESIAN_POINT('Origin',(-10.,10.,11.));
#84262=CARTESIAN_POINT('',(-11.55,16.,11.));
#84263=CARTESIAN_POINT('',(-11.55,10.,11.));
#84264=CARTESIAN_POINT('Origin',(-10.,16.,11.));
#84265=CARTESIAN_POINT('Origin',(10.,16.4656669797464,11.));
#84266=CARTESIAN_POINT('',(10.,16.9313339594927,11.));
#84267=CARTESIAN_POINT('',(9.225,16.4656669797464,11.));
#84268=CARTESIAN_POINT('Origin',(-10.,16.4656669797464,11.));
#84269=CARTESIAN_POINT('',(-10.,16.9313339594927,11.));
#84270=CARTESIAN_POINT('',(-10.775,16.4656669797464,11.));
#84271=CARTESIAN_POINT('Origin',(10.,10.15,3.5));
#84272=CARTESIAN_POINT('',(7.,10.3,3.5));
#84273=CARTESIAN_POINT('Origin',(10.,10.3,3.5));
#84274=CARTESIAN_POINT('',(6.85,10.15,3.5));
#84275=CARTESIAN_POINT('Origin',(10.,10.,3.5));
#84276=CARTESIAN_POINT('',(7.,13.2,3.5));
#84277=CARTESIAN_POINT('',(7.,10.,3.5));
#84278=CARTESIAN_POINT('Origin',(10.,13.2,3.5));
#84279=CARTESIAN_POINT('Origin',(-10.,10.15,3.5));
#84280=CARTESIAN_POINT('',(-13.,10.3,3.5));
#84281=CARTESIAN_POINT('Origin',(-10.,10.3,3.5));
#84282=CARTESIAN_POINT('',(-13.15,10.15,3.5));
#84283=CARTESIAN_POINT('Origin',(-10.,10.,3.5));
#84284=CARTESIAN_POINT('',(-13.,13.2,3.5));
#84285=CARTESIAN_POINT('',(-13.,10.,3.5));
#84286=CARTESIAN_POINT('Origin',(-10.,13.2,3.5));
#84287=CARTESIAN_POINT('Origin',(-10.,13.2,3.5));
#84288=CARTESIAN_POINT('',(-11.7,13.2,3.5));
#84289=CARTESIAN_POINT('Origin',(-10.,13.2,3.5));
#84290=CARTESIAN_POINT('Origin',(10.,13.2,3.5));
#84291=CARTESIAN_POINT('',(8.3,13.2,3.5));
#84292=CARTESIAN_POINT('Origin',(10.,13.2,3.5));
#84293=CARTESIAN_POINT('Origin',(-10.,10.,3.5));
#84294=CARTESIAN_POINT('',(-11.7,20.,3.5));
#84295=CARTESIAN_POINT('',(-11.7,10.,3.5));
#84296=CARTESIAN_POINT('Origin',(-10.,20.,3.5));
#84297=CARTESIAN_POINT('Origin',(10.,10.,3.5));
#84298=CARTESIAN_POINT('',(8.3,20.,3.5));
#84299=CARTESIAN_POINT('',(8.3,10.,3.5));
#84300=CARTESIAN_POINT('Origin',(10.,20.,3.5));
#84301=CARTESIAN_POINT('Origin',(0.,19.85,13.3));
#84302=CARTESIAN_POINT('',(-2.015,19.7,13.3));
#84303=CARTESIAN_POINT('Origin',(0.,19.7,13.3));
#84304=CARTESIAN_POINT('',(-2.315,20.,13.3));
#84305=CARTESIAN_POINT('',(-2.165,19.85,13.3));
#84306=CARTESIAN_POINT('Origin',(0.,20.,13.3));
#84307=CARTESIAN_POINT('Origin',(0.,10.,13.3));
#84308=CARTESIAN_POINT('',(-2.015,10.3,13.3));
#84309=CARTESIAN_POINT('Origin',(0.,10.3,13.3));
#84310=CARTESIAN_POINT('',(-2.015,10.,13.3));
#84311=CARTESIAN_POINT('Origin',(0.,20.,8.));
#84312=CARTESIAN_POINT('',(17.,20.,16.));
#84313=CARTESIAN_POINT('',(14.875,20.,18.125));
#84314=CARTESIAN_POINT('',(17.,20.,0.));
#84315=CARTESIAN_POINT('',(14.875,20.,-2.12499999999999));
#84316=CARTESIAN_POINT('',(-17.,20.,0.));
#84317=CARTESIAN_POINT('',(-17.5,20.,0.));
#84318=CARTESIAN_POINT('',(-14.875,20.,-2.12499999999999));
#84319=CARTESIAN_POINT('',(-17.,20.,16.));
#84320=CARTESIAN_POINT('',(-14.875,20.,18.125));
#84321=CARTESIAN_POINT('',(17.5,20.,16.));
#84322=CARTESIAN_POINT('Origin',(0.,10.15,13.3));
#84323=CARTESIAN_POINT('',(-2.165,10.15,13.3));
#84324=CARTESIAN_POINT('Origin',(17.25,10.,15.75));
#84325=CARTESIAN_POINT('',(17.,10.,16.));
#84326=CARTESIAN_POINT('Origin',(-17.5,10.,16.));
#84327=CARTESIAN_POINT('',(-17.,10.,16.));
#84328=CARTESIAN_POINT('Origin',(17.25,10.,0.25));
#84329=CARTESIAN_POINT('',(17.,10.,0.));
#84330=CARTESIAN_POINT('Origin',(17.5,10.,0.));
#84331=CARTESIAN_POINT('',(-17.,10.,0.));
#84332=CARTESIAN_POINT('Origin',(-17.25,10.,0.25));
#84333=CARTESIAN_POINT('Origin',(-17.25,10.,15.75));
#84334=CARTESIAN_POINT('',(0.,0.,0.));
#84335=CARTESIAN_POINT('Origin',(-10.,13.2,3.5));
#84336=CARTESIAN_POINT('',(-11.4635,13.4616367005047,3.50000000259583));
#84337=CARTESIAN_POINT('',(-11.4634991472179,13.3893449541571,3.49842009727736));
#84338=CARTESIAN_POINT('',(-11.4635,13.2,3.5));
#84339=CARTESIAN_POINT('',(-9.36566843221574,13.3006902612923,2.18111573215603));
#84340=CARTESIAN_POINT('Ctrl Pts',(-11.4635,13.4616367005047,3.50000000259583));
#84341=CARTESIAN_POINT('Ctrl Pts',(-11.4635000000769,13.4594692264253,3.45664071964579));
#84342=CARTESIAN_POINT('Ctrl Pts',(-11.4615730750431,13.4572524781583,3.41330134333718));
#84343=CARTESIAN_POINT('Ctrl Pts',(-11.4570944001824,13.4545591997314,3.36303805100765));
#84344=CARTESIAN_POINT('Ctrl Pts',(-11.4564127667556,13.4541776568914,3.35597043620558));
#84345=CARTESIAN_POINT('Ctrl Pts',(-11.4553183718019,13.4536038460783,3.34542659047019));
#84346=CARTESIAN_POINT('Ctrl Pts',(-11.4549445129957,13.4534136947061,3.34194631982525));
#84347=CARTESIAN_POINT('Ctrl Pts',(-11.4542514885814,13.4530713334346,3.33570581660528));
#84348=CARTESIAN_POINT('Ctrl Pts',(-11.4539369444619,13.4529193833867,3.33294512288282));
#84349=CARTESIAN_POINT('Ctrl Pts',(-11.4532344551081,13.4525873268,3.32693181026965));
#84350=CARTESIAN_POINT('Ctrl Pts',(-11.4528434538211,13.4524070545936,3.32367961528733));
#84351=CARTESIAN_POINT('Ctrl Pts',(-11.4517110420546,13.4518974628054,3.31452022986426));
#84352=CARTESIAN_POINT('Ctrl Pts',(-11.4509445077889,13.451566787266,3.3086162818247));
#84353=CARTESIAN_POINT('Ctrl Pts',(-11.4460147637586,13.4495243520316,3.27237981472014));
#84354=CARTESIAN_POINT('Ctrl Pts',(-11.4409368346681,13.4477669423748,3.24218143057608));
#84355=CARTESIAN_POINT('Ctrl Pts',(-11.4054411893259,13.4372267871199,3.06522729157856));
#84356=CARTESIAN_POINT('Ctrl Pts',(-11.3535717993129,13.4279212793678,2.92367650435652));
#84357=CARTESIAN_POINT('Ctrl Pts',(-11.2636712071939,13.4172531649537,2.76090173424482));
#84358=CARTESIAN_POINT('Ctrl Pts',(-11.2450865575485,13.4152229539322,2.73000587678491));
#84359=CARTESIAN_POINT('Ctrl Pts',(-11.2201031001592,13.4127009082363,2.69174646122165));
#84360=CARTESIAN_POINT('Ctrl Pts',(-11.2147474778138,13.4121712784354,2.68371945425952));
#84361=CARTESIAN_POINT('Ctrl Pts',(-11.2060868213118,13.4113319597054,2.67101288472951));
#84362=CARTESIAN_POINT('Ctrl Pts',(-11.2028330858424,13.4110203716262,2.66629883847623));
#84363=CARTESIAN_POINT('Ctrl Pts',(-11.1966858210542,13.4104385885131,2.65750351763395));
#84364=CARTESIAN_POINT('Ctrl Pts',(-11.193798885466,13.4101681513858,2.65341775412679));
#84365=CARTESIAN_POINT('Ctrl Pts',(-11.1872944466276,13.4095649864841,2.64431171863613));
#84366=CARTESIAN_POINT('Ctrl Pts',(-11.1836659282499,13.4092326826582,2.63929940760112));
#84367=CARTESIAN_POINT('Ctrl Pts',(-11.1728692343824,13.4082560013332,2.62458263455339));
#84368=CARTESIAN_POINT('Ctrl Pts',(-11.1656126291685,13.4076150133666,2.61494349620032));
#84369=CARTESIAN_POINT('Ctrl Pts',(-11.092662928475,13.401318311072,2.52049613728245));
#84370=CARTESIAN_POINT('Ctrl Pts',(-11.0179522223292,13.3960590647726,2.44306260042212));
#84371=CARTESIAN_POINT('Ctrl Pts',(-10.8622094018413,13.3861975082971,2.31362134557764));
#84372=CARTESIAN_POINT('Ctrl Pts',(-10.7832221702084,13.3815991271004,2.26005726325232));
#84373=CARTESIAN_POINT('Ctrl Pts',(-10.6899904553064,13.3759949982724,2.20931597205417));
#84374=CARTESIAN_POINT('Ctrl Pts',(-10.6803170670352,13.3754114274331,2.20419107785057));
#84375=CARTESIAN_POINT('Ctrl Pts',(-10.6667905505303,13.3745912607967,2.19721803101913));
#84376=CARTESIAN_POINT('Ctrl Pts',(-10.6629852137812,13.3743600764605,2.19527738489373));
#84377=CARTESIAN_POINT('Ctrl Pts',(-10.6565718222941,13.3739695991742,2.19204198448465));
#84378=CARTESIAN_POINT('Ctrl Pts',(-10.6539683131556,13.3738108502423,2.19073830977841));
#84379=CARTESIAN_POINT('Ctrl Pts',(-10.6487281495498,13.3734908373348,2.18813389347963));
#84380=CARTESIAN_POINT('Ctrl Pts',(-10.6460915013723,13.3733295733911,2.18683334454379));
#84381=CARTESIAN_POINT('Ctrl Pts',(-10.6407323454947,13.3730013235739,2.18420994324195));
#84382=CARTESIAN_POINT('Ctrl Pts',(-10.6380096170278,13.3728343102812,2.18288757492739));
#84383=CARTESIAN_POINT('Ctrl Pts',(-10.6276778956324,13.3721996856272,2.17790924198447));
#84384=CARTESIAN_POINT('Ctrl Pts',(-10.6200415730722,13.3717288373096,2.17431076261737));
#84385=CARTESIAN_POINT('Ctrl Pts',(-10.6019316987249,13.370608738785,2.16596751020181));
#84386=CARTESIAN_POINT('Ctrl Pts',(-10.5914326228172,13.3699566628213,2.1612797560522));
#84387=CARTESIAN_POINT('Ctrl Pts',(-10.5533537362692,13.367584748646,2.14481320251804));
#84388=CARTESIAN_POINT('Ctrl Pts',(-10.5254697749396,13.3658350196347,2.13375955971625));
#84389=CARTESIAN_POINT('Ctrl Pts',(-10.4349209780345,13.3601532833078,2.1010466672274));
#84390=CARTESIAN_POINT('Ctrl Pts',(-10.3711169814764,13.3561537800153,2.08278486941994));
#84391=CARTESIAN_POINT('Ctrl Pts',(-10.2146204612242,13.3466022489873,2.04928995599158));
#84392=CARTESIAN_POINT('Ctrl Pts',(-10.1212603883285,13.3411269864733,2.03852046886337));
#84393=CARTESIAN_POINT('Ctrl Pts',(-10.0168214938582,13.3353405102178,2.03655770780648));
#84394=CARTESIAN_POINT('Ctrl Pts',(-10.0061416505944,13.3347524372917,2.03647391765776));
#84395=CARTESIAN_POINT('Ctrl Pts',(-9.98894652604875,13.3338113372643,2.03652724045638));
#84396=CARTESIAN_POINT('Ctrl Pts',(-9.98243154168301,13.3334560913878,2.03659094974347));
#84397=CARTESIAN_POINT('Ctrl Pts',(-9.9708169785602,13.3328250872998,2.03678210104788));
#84398=CARTESIAN_POINT('Ctrl Pts',(-9.9657172610516,13.3325488200792,2.03689270275051));
#84399=CARTESIAN_POINT('Ctrl Pts',(-9.95503956958434,13.3319720055825,2.03718013646321));
#84400=CARTESIAN_POINT('Ctrl Pts',(-9.94946181114394,13.3316716231658,2.03736221637199));
#84401=CARTESIAN_POINT('Ctrl Pts',(-9.93484842948733,13.3308870162885,2.03792294802465));
#84402=CARTESIAN_POINT('Ctrl Pts',(-9.92581495916483,13.3304043833784,2.03835345666247));
#84403=CARTESIAN_POINT('Ctrl Pts',(-9.8849919337385,13.328233552819,2.04067840038425));
#84404=CARTESIAN_POINT('Ctrl Pts',(-9.85326419092452,13.326574703922,2.04352645668856));
#84405=CARTESIAN_POINT('Ctrl Pts',(-9.76637832118243,13.3220893944813,2.05419416590938));
#84406=CARTESIAN_POINT('Ctrl Pts',(-9.71153349824011,13.3193238498333,2.06413046537932));
#84407=CARTESIAN_POINT('Ctrl Pts',(-9.55673011949273,13.3115244326859,2.10140675421736));
#84408=CARTESIAN_POINT('Ctrl Pts',(-9.45894154015568,13.3066184055781,2.13625411982279));
#84409=CARTESIAN_POINT('Ctrl Pts',(-9.36565800289699,13.3013233430428,2.18112074824442));
#84410=CARTESIAN_POINT('',(-10.6340070945752,13.3,2.18095972236315));
#84411=CARTESIAN_POINT('Origin',(-10.,13.3,3.5));
#84412=CARTESIAN_POINT('Ctrl Pts',(-10.6340070945752,13.3,2.18095972236315));
#84413=CARTESIAN_POINT('Ctrl Pts',(-10.6850438328051,13.3030790375799,2.20549093241817));
#84414=CARTESIAN_POINT('Ctrl Pts',(-10.7346958992828,13.3061580751599,2.23300784107455));
#84415=CARTESIAN_POINT('Ctrl Pts',(-10.7826083532765,13.3092371127398,2.26332849334117));
#84416=CARTESIAN_POINT('Ctrl Pts',(-10.8304973178774,13.3123146408015,2.29363428071045));
#84417=CARTESIAN_POINT('Ctrl Pts',(-10.8766479449887,13.3153921688632,2.32674082310971));
#84418=CARTESIAN_POINT('Ctrl Pts',(-10.9207316621788,13.3184696969249,2.36242123074426));
#84419=CARTESIAN_POINT('Ctrl Pts',(-10.964804673546,13.3215464776025,2.39809297331719));
#84420=CARTESIAN_POINT('Ctrl Pts',(-11.0068113885096,13.32462325828,2.43633702988196));
#84421=CARTESIAN_POINT('Ctrl Pts',(-11.046455477424,13.3277000389576,2.47688554708218));
#84422=CARTESIAN_POINT('Ctrl Pts',(-11.0861023040175,13.3307770321066,2.51743686441816));
#84423=CARTESIAN_POINT('Ctrl Pts',(-11.1233858362807,13.3338540252557,2.5602926053304));
#84424=CARTESIAN_POINT('Ctrl Pts',(-11.1580471976943,13.3369310184047,2.60514865038241));
#84425=CARTESIAN_POINT('Ctrl Pts',(-11.1927217650378,13.3400091838839,2.6500217855244));
#84426=CARTESIAN_POINT('Ctrl Pts',(-11.2247718768695,13.343087349363,2.69689634758693));
#84427=CARTESIAN_POINT('Ctrl Pts',(-11.2539806258271,13.3461655148421,2.7454373186738));
#84428=CARTESIAN_POINT('Ctrl Pts',(-11.2832337604374,13.3492483579054,2.79405205268298));
#84429=CARTESIAN_POINT('Ctrl Pts',(-11.3096366589622,13.3523312009688,2.84433782677361));
#84430=CARTESIAN_POINT('Ctrl Pts',(-11.3330177139849,13.3554140440321,2.89593375843158));
#84431=CARTESIAN_POINT('Ctrl Pts',(-11.3564177009697,13.3584993833159,2.9475714680258));
#84432=CARTESIAN_POINT('Ctrl Pts',(-11.3767907926723,13.3615847225997,3.0005209880128));
#84433=CARTESIAN_POINT('Ctrl Pts',(-11.3940142001552,13.3646700618836,3.05440302989634));
#84434=CARTESIAN_POINT('Ctrl Pts',(-11.4112733415321,13.3677618024086,3.10839686238641));
#84435=CARTESIAN_POINT('Ctrl Pts',(-11.4253696219277,13.3708535429337,3.16332660322355));
#84436=CARTESIAN_POINT('Ctrl Pts',(-11.4362308040338,13.3739452834588,3.21880019995678));
#84437=CARTESIAN_POINT('Ctrl Pts',(-11.4423316239996,13.3756819408631,3.24996019922882));
#84438=CARTESIAN_POINT('Ctrl Pts',(-11.4474126501818,13.3774185982674,3.28129164813557));
#84439=CARTESIAN_POINT('Ctrl Pts',(-11.4514682711404,13.3791552556717,3.31272451342262));
#84440=CARTESIAN_POINT('Ctrl Pts',(-11.459400281725,13.3825518218335,3.37420112149529));
#84441=CARTESIAN_POINT('Ctrl Pts',(-11.4634320084862,13.3859483879953,3.43622799192429));
#84442=CARTESIAN_POINT('Ctrl Pts',(-11.4634991472179,13.3893449541571,3.49842009727736));
#84443=CARTESIAN_POINT('Origin',(-10.,13.2,3.5));
#84444=CARTESIAN_POINT('',(-11.4635,13.9594225818479,3.50000000603013));
#84445=CARTESIAN_POINT('',(-11.4629363565808,13.890319544931,3.49951158075118));
#84446=CARTESIAN_POINT('',(-11.4635,13.2,3.5));
#84447=CARTESIAN_POINT('Ctrl Pts',(-11.4635,13.9594225818479,3.50000000603013));
#84448=CARTESIAN_POINT('Ctrl Pts',(-11.4635000000932,13.9582466062511,3.47738503015688));
#84449=CARTESIAN_POINT('Ctrl Pts',(-11.4629758096419,13.9570856371282,3.45477011473293));
#84450=CARTESIAN_POINT('Ctrl Pts',(-11.4551533251145,13.9485175930481,3.28616518543354));
#84451=CARTESIAN_POINT('Ctrl Pts',(-11.4265472801892,13.9417767639844,3.14201777790797));
#84452=CARTESIAN_POINT('Ctrl Pts',(-11.3670356613366,13.9328211398458,2.97662230864313));
#84453=CARTESIAN_POINT('Ctrl Pts',(-11.3561568005029,13.9312807746578,2.9490470039185));
#84454=CARTESIAN_POINT('Ctrl Pts',(-11.3422380561025,13.9293950845638,2.91668141253647));
#84455=CARTESIAN_POINT('Ctrl Pts',(-11.3399975341956,13.9290939131093,2.91155273807459));
#84456=CARTESIAN_POINT('Ctrl Pts',(-11.3362970383369,13.9286001099927,2.9032128368399));
#84457=CARTESIAN_POINT('Ctrl Pts',(-11.3348547534459,13.9284085183133,2.89999376715706));
#84458=CARTESIAN_POINT('Ctrl Pts',(-11.3322524321439,13.928064319768,2.8942414092527));
#84459=CARTESIAN_POINT('Ctrl Pts',(-11.3310967859915,13.9279119802224,2.89170618992729));
#84460=CARTESIAN_POINT('Ctrl Pts',(-11.3285700688749,13.9275799993336,2.8862048391398));
#84461=CARTESIAN_POINT('Ctrl Pts',(-11.3271963201307,13.9274001996067,2.88324003469209));
#84462=CARTESIAN_POINT('Ctrl Pts',(-11.3233026177517,13.9268925753011,2.87490995177149));
#84463=CARTESIAN_POINT('Ctrl Pts',(-11.3207600096875,13.9265634084605,2.86955541012884));
#84464=CARTESIAN_POINT('Ctrl Pts',(-11.3050471655727,13.9245438356597,2.83697759536428));
#84465=CARTESIAN_POINT('Ctrl Pts',(-11.291069095096,13.9228089061138,2.81015425998862));
#84466=CARTESIAN_POINT('Ctrl Pts',(-11.2052562762834,13.9125753020144,2.65723863443827));
#84467=CARTESIAN_POINT('Ctrl Pts',(-11.1158132283642,13.9035763970159,2.54194922444878));
#84468=CARTESIAN_POINT('Ctrl Pts',(-10.9823275852265,13.8929469874535,2.41444915989708));
#84469=CARTESIAN_POINT('Ctrl Pts',(-10.9527125558145,13.8907196795358,2.38836727534984));
#84470=CARTESIAN_POINT('Ctrl Pts',(-10.9143802523893,13.8879940245031,2.35726675995235));
#84471=CARTESIAN_POINT('Ctrl Pts',(-10.9066194226553,13.8874498136532,2.35109977233512));
#84472=CARTESIAN_POINT('Ctrl Pts',(-10.89424240565,13.8865937367087,2.34146814125312));
#84473=CARTESIAN_POINT('Ctrl Pts',(-10.8896674470801,13.886279815974,2.33795121327366));
#84474=CARTESIAN_POINT('Ctrl Pts',(-10.8811126233196,13.8856974242563,2.33145496087006));
#84475=CARTESIAN_POINT('Ctrl Pts',(-10.8771381595618,13.8854286844339,2.32846868870981));
#84476=CARTESIAN_POINT('Ctrl Pts',(-10.8682837061934,13.8848339895568,2.32188608279294));
#84477=CARTESIAN_POINT('Ctrl Pts',(-10.863396417653,13.8845084214412,2.31829968949218));
#84478=CARTESIAN_POINT('Ctrl Pts',(-10.8491360596189,13.8835661086115,2.30797084216438));
#84479=CARTESIAN_POINT('Ctrl Pts',(-10.8397051896972,13.8829524328757,2.3013087280542));
#84480=CARTESIAN_POINT('Ctrl Pts',(-10.75794967512,13.877711150996,2.24499375678881));
#84481=CARTESIAN_POINT('Ctrl Pts',(-10.6813718847936,13.8733405340097,2.20182308177545));
#84482=CARTESIAN_POINT('Ctrl Pts',(-10.5356758122848,13.8655304543736,2.13615333959942));
#84483=CARTESIAN_POINT('Ctrl Pts',(-10.4678765224952,13.8620703494366,2.11143339811311));
#84484=CARTESIAN_POINT('Ctrl Pts',(-10.3812138451641,13.8575964485435,2.08690683275938));
#84485=CARTESIAN_POINT('Ctrl Pts',(-10.3638043571153,13.8566949105505,2.08232491307433));
#84486=CARTESIAN_POINT('Ctrl Pts',(-10.3139648081243,13.8540953389334,2.07018638305261));
#84487=CARTESIAN_POINT('Ctrl Pts',(-10.2813572106567,13.8523722979068,2.06341422949068));
#84488=CARTESIAN_POINT('Ctrl Pts',(-10.2428440253955,13.8502820368155,2.05677702700672));
#84489=CARTESIAN_POINT('Ctrl Pts',(-10.2371327576853,13.8499706495551,2.05582763374375));
#84490=CARTESIAN_POINT('Ctrl Pts',(-10.2278749273723,13.8494633946948,2.05434508648266));
#84491=CARTESIAN_POINT('Ctrl Pts',(-10.2243317186376,13.8492686626496,2.05379102790929));
#84492=CARTESIAN_POINT('Ctrl Pts',(-10.2180262116206,13.8489210071784,2.05282875306515));
#84493=CARTESIAN_POINT('Ctrl Pts',(-10.2152647443401,13.8487683727909,2.05241541296835));
#84494=CARTESIAN_POINT('Ctrl Pts',(-10.2093072205452,13.8484382488928,2.05154110713939));
#84495=CARTESIAN_POINT('Ctrl Pts',(-10.2061108626171,13.8482606174844,2.05108282197535));
#84496=CARTESIAN_POINT('Ctrl Pts',(-10.1972250165376,13.8477654325336,2.04983879148628));
#84497=CARTESIAN_POINT('Ctrl Pts',(-10.1915324441188,13.8474466398496,2.04907596393223));
#84498=CARTESIAN_POINT('Ctrl Pts',(-10.1590337832059,13.8456183464952,2.04491559801112));
#84499=CARTESIAN_POINT('Ctrl Pts',(-10.1321437466162,13.8440733896872,2.04222765816543));
#84500=CARTESIAN_POINT('Ctrl Pts',(-10.0444080224075,13.8389609006446,2.03590484615251));
#84501=CARTESIAN_POINT('Ctrl Pts',(-9.9834083088122,13.8352969350701,2.03532576228975));
#84502=CARTESIAN_POINT('Ctrl Pts',(-9.80664840950789,13.8246386580238,2.04469273879405));
#84503=CARTESIAN_POINT('Ctrl Pts',(-9.69186441666404,13.8177042430711,2.0646026870416));
#84504=CARTESIAN_POINT('Ctrl Pts',(-9.56473590207054,13.8102871618157,2.10262656021611));
#84505=CARTESIAN_POINT('Ctrl Pts',(-9.54892640258902,13.8093686328021,2.10764946702432));
#84506=CARTESIAN_POINT('Ctrl Pts',(-9.52705109525389,13.8081026449642,2.11501128296192));
#84507=CARTESIAN_POINT('Ctrl Pts',(-9.52091074011626,13.8077478316051,2.11712332589203));
#84508=CARTESIAN_POINT('Ctrl Pts',(-9.5103317775379,13.8071374353213,2.12084099613906));
#84509=CARTESIAN_POINT('Ctrl Pts',(-9.50588654070424,13.8068812242043,2.12242734634818));
#84510=CARTESIAN_POINT('Ctrl Pts',(-9.49669009329876,13.8063517101734,2.12575947942917));
#84511=CARTESIAN_POINT('Ctrl Pts',(-9.49194010454745,13.8060785170797,2.12750846484077));
#84512=CARTESIAN_POINT('Ctrl Pts',(-9.48081921475893,13.8054395726164,2.13166891287029));
#84513=CARTESIAN_POINT('Ctrl Pts',(-9.47445585660575,13.8050744861701,2.13410029385447));
#84514=CARTESIAN_POINT('Ctrl Pts',(-9.45373388380511,13.8038871255502,2.14218421939232));
#84515=CARTESIAN_POINT('Ctrl Pts',(-9.4394473933587,13.8030709326886,2.14801954051584));
#84516=CARTESIAN_POINT('Ctrl Pts',(-9.36511376197395,13.7988331598728,2.17976202314754));
#84517=CARTESIAN_POINT('Ctrl Pts',(-9.30675796476374,13.7955416671563,2.20944756530999));
#84518=CARTESIAN_POINT('Ctrl Pts',(-9.1772978469926,13.7881127463837,2.28662779009391));
#84519=CARTESIAN_POINT('Ctrl Pts',(-9.10798034530001,13.7840406018752,2.33663799170221));
#84520=CARTESIAN_POINT('Ctrl Pts',(-9.00311977632505,13.7771772823459,2.4272013350867));
#84521=CARTESIAN_POINT('Ctrl Pts',(-8.96475704843755,13.7744821341029,2.46417276740201));
#84522=CARTESIAN_POINT('Ctrl Pts',(-8.92363169648773,13.7712600813543,2.50837781449751));
#84523=CARTESIAN_POINT('Ctrl Pts',(-8.91880422234596,13.7708762607193,2.51364358884478));
#84524=CARTESIAN_POINT('Ctrl Pts',(-8.91165492421536,13.7702990355094,2.52155754009971));
#84525=CARTESIAN_POINT('Ctrl Pts',(-8.9093037212749,13.7701077579779,2.52417917712055));
#84526=CARTESIAN_POINT('Ctrl Pts',(-8.90510997094335,13.7697639329295,2.52888938253385));
#84527=CARTESIAN_POINT('Ctrl Pts',(-8.90326390156836,13.7696116507789,2.5309747488697));
#84528=CARTESIAN_POINT('Ctrl Pts',(-8.89926360226851,13.7692796205003,2.53551966199074));
#84529=CARTESIAN_POINT('Ctrl Pts',(-8.89711168865999,13.7690997129631,2.53798112701712));
#84530=CARTESIAN_POINT('Ctrl Pts',(-8.89107011014472,13.7685910028816,2.54493869621058));
#84531=CARTESIAN_POINT('Ctrl Pts',(-8.88719961420015,13.7682608462765,2.54945126716448));
#84532=CARTESIAN_POINT('Ctrl Pts',(-8.8635497141802,13.766217808896,2.57736685216161));
#84533=CARTESIAN_POINT('Ctrl Pts',(-8.84448315881396,13.7644591635936,2.60136117517366));
#84534=CARTESIAN_POINT('Ctrl Pts',(-8.73554217686856,13.7538079833206,2.74766201824499));
#84535=CARTESIAN_POINT('Ctrl Pts',(-8.66437662775479,13.744385681221,2.88275561968854));
#84536=CARTESIAN_POINT('Ctrl Pts',(-8.60442310346896,13.7337897297474,3.05805391710281));
#84537=CARTESIAN_POINT('Ctrl Pts',(-8.59468597150639,13.7319093371147,3.09006835616096));
#84538=CARTESIAN_POINT('Ctrl Pts',(-8.58360833507799,13.7295414318251,3.13154817302867));
#84539=CARTESIAN_POINT('Ctrl Pts',(-8.58125162591186,13.7290215125677,3.14072969197802));
#84540=CARTESIAN_POINT('Ctrl Pts',(-8.57764152850863,13.7281982488104,3.1553840703986));
#84541=CARTESIAN_POINT('Ctrl Pts',(-8.57633016892955,13.7278930570218,3.16084225840401));
#84542=CARTESIAN_POINT('Ctrl Pts',(-8.5740278861272,13.7273458954099,3.17067358926938));
#84543=CARTESIAN_POINT('Ctrl Pts',(-8.57302560010035,13.72710356593,3.17504397682378));
#84544=CARTESIAN_POINT('Ctrl Pts',(-8.57072262296208,13.7265368628499,3.18530207299097));
#84545=CARTESIAN_POINT('Ctrl Pts',(-8.56943819569798,13.7262130100459,3.19119337549489));
#84546=CARTESIAN_POINT('Ctrl Pts',(-8.56582892874529,13.7252797152414,3.20825397631357));
#84547=CARTESIAN_POINT('Ctrl Pts',(-8.56359820630299,13.7246732572833,3.21944287418016));
#84548=CARTESIAN_POINT('Ctrl Pts',(-8.5465582654733,13.7197838869832,3.31044941212668));
#84549=CARTESIAN_POINT('Ctrl Pts',(-8.53828190275751,13.7157184060523,3.39135046083801));
#84550=CARTESIAN_POINT('Ctrl Pts',(-8.53509529062912,13.7073972452405,3.56108490611073));
#84551=CARTESIAN_POINT('Ctrl Pts',(-8.54147527872705,13.7031744766665,3.64960375252398));
#84552=CARTESIAN_POINT('Ctrl Pts',(-8.56246164039444,13.6966733533247,3.77748744368947));
#84553=CARTESIAN_POINT('Ctrl Pts',(-8.57080550919317,13.6945687004384,3.81767649339344));
#84554=CARTESIAN_POINT('Ctrl Pts',(-8.58246251612846,13.6920189662021,3.86395692465306));
#84555=CARTESIAN_POINT('Ctrl Pts',(-8.58414395658109,13.6916586415886,3.87044408762766));
#84556=CARTESIAN_POINT('Ctrl Pts',(-8.58676456801308,13.6911077640926,3.88027612630479));
#84557=CARTESIAN_POINT('Ctrl Pts',(-8.58767121655815,13.6909190241075,3.88362967222534));
#84558=CARTESIAN_POINT('Ctrl Pts',(-8.58932536283157,13.69057790384,3.88966274734633));
#84559=CARTESIAN_POINT('Ctrl Pts',(-8.59006856730329,13.6904257711126,3.89234339997065));
#84560=CARTESIAN_POINT('Ctrl Pts',(-8.59171206152173,13.690091794407,3.89820631503039));
#84561=CARTESIAN_POINT('Ctrl Pts',(-8.59261548591959,13.6899097753758,3.90138761325441));
#84562=CARTESIAN_POINT('Ctrl Pts',(-8.59521934268837,13.6893896238694,3.91043990430011));
#84563=CARTESIAN_POINT('Ctrl Pts',(-8.59694576235166,13.6890500432456,3.91630327134095));
#84564=CARTESIAN_POINT('Ctrl Pts',(-8.60849927347496,13.6868122429452,3.95465366924297));
#84565=CARTESIAN_POINT('Ctrl Pts',(-8.61941656009519,13.6848578935218,3.98679897354983));
#84566=CARTESIAN_POINT('Ctrl Pts',(-8.66499946123898,13.6773169190869,4.10710551010846));
#84567=CARTESIAN_POINT('Ctrl Pts',(-8.70707712835278,13.6715271629977,4.19220958991921));
#84568=CARTESIAN_POINT('Ctrl Pts',(-8.80072929427249,13.6609514406805,4.34286216015206));
#84569=CARTESIAN_POINT('Ctrl Pts',(-8.85025105331755,13.6561484314662,4.40925671616065));
#84570=CARTESIAN_POINT('Ctrl Pts',(-8.91223078849635,13.6509717821927,4.47913488835436));
#84571=CARTESIAN_POINT('Ctrl Pts',(-8.91942643893409,13.6503817623822,4.48707029880919));
#84572=CARTESIAN_POINT('Ctrl Pts',(-8.93110771747107,13.6494411612357,4.49967165085258));
#84573=CARTESIAN_POINT('Ctrl Pts',(-8.93553820752311,13.6490882799397,4.50438798051702));
#84574=CARTESIAN_POINT('Ctrl Pts',(-8.94346542384514,13.6484636659082,4.51271526213057));
#84575=CARTESIAN_POINT('Ctrl Pts',(-8.94694972544813,13.6481914098162,4.51633785371999));
#84576=CARTESIAN_POINT('Ctrl Pts',(-8.95425630603311,13.6476251940673,4.52385651543028));
#84577=CARTESIAN_POINT('Ctrl Pts',(-8.9580818611004,13.6473313823767,4.52774930338147));
#84578=CARTESIAN_POINT('Ctrl Pts',(-8.96809807728009,13.6465688991416,4.53782814611052));
#84579=CARTESIAN_POINT('Ctrl Pts',(-8.97432265855781,13.6461017182843,4.5439802846348));
#84580=CARTESIAN_POINT('Ctrl Pts',(-9.00200868570563,13.6440523804781,4.5708574520043));
#84581=CARTESIAN_POINT('Ctrl Pts',(-9.02404653451883,13.6424960837332,4.59097999108372));
#84582=CARTESIAN_POINT('Ctrl Pts',(-9.0853633609575,13.6383462068342,4.64362175013917));
#84583=CARTESIAN_POINT('Ctrl Pts',(-9.1257518097775,13.6358029756795,4.67478573593734));
#84584=CARTESIAN_POINT('Ctrl Pts',(-9.24114667256317,13.6289054313731,4.75457167589954));
#84585=CARTESIAN_POINT('Ctrl Pts',(-9.31909810842037,13.624649504223,4.79852985739633));
#84586=CARTESIAN_POINT('Ctrl Pts',(-9.41064137953276,13.6196378831124,4.8396307855888));
#84587=CARTESIAN_POINT('Ctrl Pts',(-9.42076743193361,13.6190831709443,4.84404012198047));
#84588=CARTESIAN_POINT('Ctrl Pts',(-9.4629288745006,13.6167684568911,4.86183414723024));
#84589=CARTESIAN_POINT('Ctrl Pts',(-9.4953834119252,13.6149746874378,4.87419044353775));
#84590=CARTESIAN_POINT('Ctrl Pts',(-9.53379444185724,13.612804973922,4.88727034426828));
#84591=CARTESIAN_POINT('Ctrl Pts',(-9.53935616335689,13.6124896817394,4.88912702226633));
#84592=CARTESIAN_POINT('Ctrl Pts',(-9.54836048889752,13.611977186569,4.89207292877823));
#84593=CARTESIAN_POINT('Ctrl Pts',(-9.55179628516663,13.6117811543679,4.89318294436378));
#84594=CARTESIAN_POINT('Ctrl Pts',(-9.55790403022811,13.6114317660788,4.89513126463055));
#84595=CARTESIAN_POINT('Ctrl Pts',(-9.56057431345817,13.6112787057201,4.89597462651518));
#84596=CARTESIAN_POINT('Ctrl Pts',(-9.5663286415538,13.6109481914429,4.89777388284596));
#84597=CARTESIAN_POINT('Ctrl Pts',(-9.5694133933102,13.6107705986127,4.89872722445381));
#84598=CARTESIAN_POINT('Ctrl Pts',(-9.57796055429666,13.6102774381241,4.90133776822581));
#84599=CARTESIAN_POINT('Ctrl Pts',(-9.58342948263533,13.6099606579149,4.90297321295187));
#84600=CARTESIAN_POINT('Ctrl Pts',(-9.6140959532309,13.6081780259888,4.91194869252319));
#84601=CARTESIAN_POINT('Ctrl Pts',(-9.63947636422258,13.6066789062582,4.91864145458542));
#84602=CARTESIAN_POINT('Ctrl Pts',(-9.72142668071614,13.6017923649351,4.93791050661331));
#84603=CARTESIAN_POINT('Ctrl Pts',(-9.77856697895659,13.5983175247031,4.94781089984347));
#84604=CARTESIAN_POINT('Ctrl Pts',(-9.95505635661787,13.5876327799909,4.96769647384994));
#84605=CARTESIAN_POINT('Ctrl Pts',(-10.0751896132792,13.5804711804802,4.96646142213768));
#84606=CARTESIAN_POINT('Ctrl Pts',(-10.2099635213672,13.5728752368683,4.94845160092698));
#84607=CARTESIAN_POINT('Ctrl Pts',(-10.2260461936635,13.5719749975809,4.94602899997067));
#84608=CARTESIAN_POINT('Ctrl Pts',(-10.2484436898104,13.5707295514294,4.94227235476854));
#84609=CARTESIAN_POINT('Ctrl Pts',(-10.2547947165544,13.5703773236158,4.94116392773745));
#84610=CARTESIAN_POINT('Ctrl Pts',(-10.2657772029017,13.569769799548,4.939172316186));
#84611=CARTESIAN_POINT('Ctrl Pts',(-10.2704120670037,13.5695138939623,4.93830865672145));
#84612=CARTESIAN_POINT('Ctrl Pts',(-10.280035425227,13.5689835369843,4.93646728136238));
#84613=CARTESIAN_POINT('Ctrl Pts',(-10.285023166984,13.5687092037159,4.93548594036558));
#84614=CARTESIAN_POINT('Ctrl Pts',(-10.296758206342,13.5680650083923,4.93311349040502));
#84615=CARTESIAN_POINT('Ctrl Pts',(-10.3035010274427,13.5676958366373,4.93170068029508));
#84616=CARTESIAN_POINT('Ctrl Pts',(-10.3256932994976,13.5664838503899,4.92688695024322));
#84617=CARTESIAN_POINT('Ctrl Pts',(-10.3410978844261,13.5656474572788,4.92328308954725));
#84618=CARTESIAN_POINT('Ctrl Pts',(-10.4228401171124,13.561231270936,4.90275631766725));
#84619=CARTESIAN_POINT('Ctrl Pts',(-10.4879903292252,13.5577946123582,4.88144340446504));
#84620=CARTESIAN_POINT('Ctrl Pts',(-10.6308570509259,13.5502089456224,4.82333173734331));
#84621=CARTESIAN_POINT('Ctrl Pts',(-10.7073017897354,13.5461166784398,4.7840991962932));
#84622=CARTESIAN_POINT('Ctrl Pts',(-10.7921411472125,13.5411329603865,4.73067257558485));
#84623=CARTESIAN_POINT('Ctrl Pts',(-10.8042976167603,13.5404071780409,4.72276241043271));
#84624=CARTESIAN_POINT('Ctrl Pts',(-10.8460586041076,13.5378661800646,4.69469648358011));
#84625=CARTESIAN_POINT('Ctrl Pts',(-10.8750374289745,13.5360182903242,4.67363706176502));
#84626=CARTESIAN_POINT('Ctrl Pts',(-10.9078697001915,13.5337875407603,4.64788496434825));
#84627=CARTESIAN_POINT('Ctrl Pts',(-10.9125046703904,13.5334693134436,4.64420387521335));
#84628=CARTESIAN_POINT('Ctrl Pts',(-10.9199122754855,13.5329551542494,4.63824712632199));
#84629=CARTESIAN_POINT('Ctrl Pts',(-10.9226991433255,13.5327604391648,4.63598917491196));
#84630=CARTESIAN_POINT('Ctrl Pts',(-10.9276408041016,13.532412832639,4.63195520490714));
#84631=CARTESIAN_POINT('Ctrl Pts',(-10.9297988855222,13.5322602287105,4.63018320628363));
#84632=CARTESIAN_POINT('Ctrl Pts',(-10.934388960798,13.5319339148781,4.62639225431527));
#84633=CARTESIAN_POINT('Ctrl Pts',(-10.9368194853879,13.531760083796,4.62437159873695));
#84634=CARTESIAN_POINT('Ctrl Pts',(-10.9434705181101,13.5312815814992,4.61880561922792));
#84635=CARTESIAN_POINT('Ctrl Pts',(-10.9476775274277,13.5309757776052,4.61524433832486));
#84636=CARTESIAN_POINT('Ctrl Pts',(-10.9701241157657,13.5293277513058,4.5960243288098));
#84637=CARTESIAN_POINT('Ctrl Pts',(-10.98799491515,13.5279572386478,4.57994260845164));
#84638=CARTESIAN_POINT('Ctrl Pts',(-11.0419494396188,13.5236572263307,4.52892920382205));
#84639=CARTESIAN_POINT('Ctrl Pts',(-11.076636453377,13.5206592227322,4.49257608025498));
#84640=CARTESIAN_POINT('Ctrl Pts',(-11.1923353415791,13.5099902721221,4.35810511989452));
#84641=CARTESIAN_POINT('Ctrl Pts',(-11.2623822355807,13.5023051830361,4.25127249846792));
#84642=CARTESIAN_POINT('Ctrl Pts',(-11.3262086327459,13.4940676108242,4.11917871858112));
#84643=CARTESIAN_POINT('Ctrl Pts',(-11.3343319135663,13.4929858020648,4.101473207523));
#84644=CARTESIAN_POINT('Ctrl Pts',(-11.3451579691168,13.4914948834813,4.07657706026865));
#84645=CARTESIAN_POINT('Ctrl Pts',(-11.3481610218037,13.4910755909108,4.0695199125207));
#84646=CARTESIAN_POINT('Ctrl Pts',(-11.3529060979015,13.4904036106651,4.058121150634));
#84647=CARTESIAN_POINT('Ctrl Pts',(-11.354682995527,13.4901497452288,4.05379428569315));
#84648=CARTESIAN_POINT('Ctrl Pts',(-11.3583266831376,13.4896244685637,4.04479918142102));
#84649=CARTESIAN_POINT('Ctrl Pts',(-11.3601902250354,13.4893531695293,4.04012968701556));
#84650=CARTESIAN_POINT('Ctrl Pts',(-11.3645121780949,13.488717620863,4.02913590363951));
#84651=CARTESIAN_POINT('Ctrl Pts',(-11.3669507546732,13.4883540400027,4.02280390694054));
#84652=CARTESIAN_POINT('Ctrl Pts',(-11.3747978217616,13.487167279424,4.00199794760603));
#84653=CARTESIAN_POINT('Ctrl Pts',(-11.3800212443667,13.4863502529278,3.98745500236345));
#84654=CARTESIAN_POINT('Ctrl Pts',(-11.406319013975,13.4820841955652,3.91042385655824));
#84655=CARTESIAN_POINT('Ctrl Pts',(-11.4233832728651,13.4787684450086,3.84664427799868));
#84656=CARTESIAN_POINT('Ctrl Pts',(-11.4523955575071,13.4713531112475,3.69885980015698));
#84657=CARTESIAN_POINT('Ctrl Pts',(-11.4614643780711,13.4673149955992,3.61453917439005));
#84658=CARTESIAN_POINT('Ctrl Pts',(-11.4633981313327,13.462630799978,3.51993994582104));
#84659=CARTESIAN_POINT('Ctrl Pts',(-11.4634999999823,13.4621350600777,3.50996944764625));
#84660=CARTESIAN_POINT('Ctrl Pts',(-11.4635,13.4616367005047,3.50000000259583));
#84661=CARTESIAN_POINT('Ctrl Pts',(-11.4638034778342,13.3888174556321,3.49845133854934));
#84662=CARTESIAN_POINT('Ctrl Pts',(-11.4637389471014,13.3919645434129,3.55221748613726));
#84663=CARTESIAN_POINT('Ctrl Pts',(-11.4606820604459,13.3951565851578,3.60609881299289));
#84664=CARTESIAN_POINT('Ctrl Pts',(-11.4546528039997,13.3983331287172,3.65973463770758));
#84665=CARTESIAN_POINT('Ctrl Pts',(-11.4486311466748,13.4015056686419,3.71330286119413));
#84666=CARTESIAN_POINT('Ctrl Pts',(-11.4396448753746,13.4046624601302,3.76662621772362));
#84667=CARTESIAN_POINT('Ctrl Pts',(-11.427751489726,13.4077628611718,3.81935395290464));
#84668=CARTESIAN_POINT('Ctrl Pts',(-11.4158679180049,13.4108607038912,3.87203817935049));
#84669=CARTESIAN_POINT('Ctrl Pts',(-11.4010370563809,13.4138754519379,3.92411692140531));
#84670=CARTESIAN_POINT('Ctrl Pts',(-11.3833734100942,13.4168000700608,3.97524255973066));
#84671=CARTESIAN_POINT('Ctrl Pts',(-11.365716659341,13.4197235464714,4.02634823963184));
#84672=CARTESIAN_POINT('Ctrl Pts',(-11.3453758482529,13.422647278177,4.07655708571848));
#84673=CARTESIAN_POINT('Ctrl Pts',(-11.3223609188837,13.4255094599703,4.12551597861373));
#84674=CARTESIAN_POINT('Ctrl Pts',(-11.2993281844628,13.4283738560348,4.17451274760263));
#84675=CARTESIAN_POINT('Ctrl Pts',(-11.2735457975972,13.4311296631554,4.22221618697834));
#84676=CARTESIAN_POINT('Ctrl Pts',(-11.2452411977534,13.4338443445426,4.2683285929259));
#84677=CARTESIAN_POINT('Ctrl Pts',(-11.2169266033059,13.4365599845077,4.31445728157045));
#84678=CARTESIAN_POINT('Ctrl Pts',(-11.1860867348378,13.4392347488967,4.35899583250288));
#84679=CARTESIAN_POINT('Ctrl Pts',(-11.1529218371365,13.4419159292845,4.4016390119544));
#84680=CARTESIAN_POINT('Ctrl Pts',(-11.119693539766,13.4446022351502,4.44436371023027));
#84681=CARTESIAN_POINT('Ctrl Pts',(-11.0841310338689,13.4472954693768,4.48518531569453));
#84682=CARTESIAN_POINT('Ctrl Pts',(-11.0464774039781,13.4500570205331,4.52381765057115));
#84683=CARTESIAN_POINT('Ctrl Pts',(-11.0149929368743,13.4523661197298,4.55612047184215));
#84684=CARTESIAN_POINT('Ctrl Pts',(-10.9820471053411,13.4547234711996,4.58689275186817));
#84685=CARTESIAN_POINT('Ctrl Pts',(-10.947806378907,13.457167717929,4.61598287146918));
#84686=CARTESIAN_POINT('Ctrl Pts',(-10.9477906510602,13.4571688406487,4.61599623347969));
#84687=CARTESIAN_POINT('Ctrl Pts',(-10.94777492294,13.4571699633867,4.61600959513598));
#84688=CARTESIAN_POINT('Ctrl Pts',(-10.9477591945465,13.4571710861431,4.61602295643805));
#84689=CARTESIAN_POINT('Ctrl Pts',(-10.9094872476417,13.4599030925948,4.64853505276661));
#84690=CARTESIAN_POINT('Ctrl Pts',(-10.869431407601,13.4627519499741,4.67908033928225));
#84691=CARTESIAN_POINT('Ctrl Pts',(-10.8278340982856,13.4656578568494,4.70748720938998));
#84692=CARTESIAN_POINT('Ctrl Pts',(-10.8237759029398,13.465941354459,4.71025855758433));
#84693=CARTESIAN_POINT('Ctrl Pts',(-10.8197030771707,13.4662253950528,4.71300955229469));
#84694=CARTESIAN_POINT('Ctrl Pts',(-10.815615872548,13.4665099231026,4.71574003452877));
#84695=CARTESIAN_POINT('Ctrl Pts',(-10.7697160879684,13.4697052062841,4.74640366845739));
#84696=CARTESIAN_POINT('Ctrl Pts',(-10.7219970544357,13.4729613189875,4.77448093742227));
#84697=CARTESIAN_POINT('Ctrl Pts',(-10.6727944195478,13.4762124530802,4.79979131982366));
#84698=CARTESIAN_POINT('Ctrl Pts',(-10.6236407645761,13.4794603507553,4.82507650641162));
#84699=CARTESIAN_POINT('Ctrl Pts',(-10.5730065714788,13.4827029317654,4.84760067203343));
#84700=CARTESIAN_POINT('Ctrl Pts',(-10.5212366024711,13.4858947597026,4.86722193790353));
#84701=CARTESIAN_POINT('Ctrl Pts',(-10.469497861905,13.48908466228,4.88683136792424));
#84702=CARTESIAN_POINT('Ctrl Pts',(-10.4166247401001,13.4922237292158,4.90354154255135));
#84703=CARTESIAN_POINT('Ctrl Pts',(-10.3629705797557,13.4952903731062,4.91724518846785));
#84704=CARTESIAN_POINT('Ctrl Pts',(-10.309327739629,13.498356369981,4.93094594312197));
#84705=CARTESIAN_POINT('Ctrl Pts',(-10.254904202352,13.5013499723776,4.94164140890122));
#84706=CARTESIAN_POINT('Ctrl Pts',(-10.2000620512057,13.504274428245,4.94925790984549));
#84707=CARTESIAN_POINT('Ctrl Pts',(-10.1451707659611,13.5072015041865,4.95688123455394));
#84708=CARTESIAN_POINT('Ctrl Pts',(-10.0898601359871,13.5100594326265,4.96141989310606));
#84709=CARTESIAN_POINT('Ctrl Pts',(-10.0345019800102,13.5128754485554,4.96283519573269));
#84710=CARTESIAN_POINT('Ctrl Pts',(-9.97911943547413,13.5156927051067,4.96425112188427));
#84711=CARTESIAN_POINT('Ctrl Pts',(-9.92368938023504,13.5184682986004,4.96254059815874));
#84712=CARTESIAN_POINT('Ctrl Pts',(-9.86859235972315,13.5212504641971,4.95770397676074));
#84713=CARTESIAN_POINT('Ctrl Pts',(-9.81339269079736,13.5240378131028,4.95285834450317));
#84714=CARTESIAN_POINT('Ctrl Pts',(-9.75852748088284,13.5268322697061,4.94487441448456));
#84715=CARTESIAN_POINT('Ctrl Pts',(-9.7043860069233,13.5296974670412,4.93379840192616));
#84716=CARTESIAN_POINT('Ctrl Pts',(-9.66259727071438,13.5319089505282,4.92524945537559));
#84717=CARTESIAN_POINT('Ctrl Pts',(-9.62123992915594,13.5341630234317,4.9148592385162));
#84718=CARTESIAN_POINT('Ctrl Pts',(-9.58049393286608,13.5364914585468,4.90267111986085));
#84719=CARTESIAN_POINT('Ctrl Pts',(-9.58047693404163,13.5364924299468,4.90266603509895));
#84720=CARTESIAN_POINT('Ctrl Pts',(-9.58045993532319,13.5364934013597,4.90266095002429));
#84721=CARTESIAN_POINT('Ctrl Pts',(-9.58044293671079,13.5364943727856,4.90265586463689));
#84722=CARTESIAN_POINT('Ctrl Pts',(-9.53202383501105,13.5392613967326,4.88817057112994));
#84723=CARTESIAN_POINT('Ctrl Pts',(-9.48429284608302,13.5421405845651,4.87108885568505));
#84724=CARTESIAN_POINT('Ctrl Pts',(-9.43753012185968,13.5450718499842,4.85152258524947));
#84725=CARTESIAN_POINT('Ctrl Pts',(-9.43327565767751,13.5453385359813,4.84974244950825));
#84726=CARTESIAN_POINT('Ctrl Pts',(-9.42902922831058,13.5456056530415,4.84794177767954));
#84727=CARTESIAN_POINT('Ctrl Pts',(-9.42479105634956,13.5458731559159,4.84612067190963));
#84728=CARTESIAN_POINT('Ctrl Pts',(-9.37405702481399,13.5490753618169,4.82432069814493));
#84729=CARTESIAN_POINT('Ctrl Pts',(-9.32450261137027,13.5523322309487,4.79958811715058));
#84730=CARTESIAN_POINT('Ctrl Pts',(-9.27646151112173,13.5555794400524,4.77210561834639));
#84731=CARTESIAN_POINT('Ctrl Pts',(-9.22846654423733,13.5588235308954,4.74464951069724));
#84732=CARTESIAN_POINT('Ctrl Pts',(-9.18198175759054,13.5620576470011,4.71444904085066));
#84733=CARTESIAN_POINT('Ctrl Pts',(-9.13731388703022,13.5652380057577,4.6817155957195));
#84734=CARTESIAN_POINT('Ctrl Pts',(-9.09267141884258,13.5684165558619,4.64900076591882));
#84735=CARTESIAN_POINT('Ctrl Pts',(-9.04984370571082,13.5715412748565,4.61375593455757));
#84736=CARTESIAN_POINT('Ctrl Pts',(-9.00911342310494,13.5745922292323,4.57621866854711));
#84737=CARTESIAN_POINT('Ctrl Pts',(-8.96839035491113,13.5776426432032,4.5386880513809));
#84738=CARTESIAN_POINT('Ctrl Pts',(-8.92976401327719,13.5806193232223,4.49886580285893));
#84739=CARTESIAN_POINT('Ctrl Pts',(-8.89349379236424,13.5835270645262,4.45701531701962));
#84740=CARTESIAN_POINT('Ctrl Pts',(-8.85718929406797,13.586437553808,4.41512528013517));
#84741=CARTESIAN_POINT('Ctrl Pts',(-8.82324554259782,13.5892791041831,4.37120308457584));
#84742=CARTESIAN_POINT('Ctrl Pts',(-8.79189791977439,13.5920803007864,4.32553960581249));
#84743=CARTESIAN_POINT('Ctrl Pts',(-8.76053561004683,13.5948828097989,4.2798547329186));
#84744=CARTESIAN_POINT('Ctrl Pts',(-8.73177218894977,13.597645223792,4.2324268041065));
#84745=CARTESIAN_POINT('Ctrl Pts',(-8.70581493137394,13.6004168019331,4.18357557404067));
#84746=CARTESIAN_POINT('Ctrl Pts',(-8.67980828609894,13.6031936534305,4.13463139695039));
#84747=CARTESIAN_POINT('Ctrl Pts',(-8.65661905923465,13.6059802289843,4.08425835729951));
#84748=CARTESIAN_POINT('Ctrl Pts',(-8.63642053376971,13.6088406852103,4.03280883998907));
#84749=CARTESIAN_POINT('Ctrl Pts',(-8.62090319297247,13.6110382057259,3.99328319761756));
#84750=CARTESIAN_POINT('Ctrl Pts',(-8.6071503804057,13.613279763713,3.9531228751966));
#84751=CARTESIAN_POINT('Ctrl Pts',(-8.59522272434344,13.6155966400574,3.91250036744496));
#84752=CARTESIAN_POINT('Ctrl Pts',(-8.59521747235296,13.6155976602254,3.91248248052545));
#84753=CARTESIAN_POINT('Ctrl Pts',(-8.59521222071596,13.6155986804079,3.91246459351607));
#84754=CARTESIAN_POINT('Ctrl Pts',(-8.59520696943243,13.6155997006051,3.91244670641683));
#84755=CARTESIAN_POINT('Ctrl Pts',(-8.58103522202286,13.6183529277781,3.86417442201071));
#84756=CARTESIAN_POINT('Ctrl Pts',(-8.56939194522168,13.6212198794063,3.81506537742746));
#84757=CARTESIAN_POINT('Ctrl Pts',(-8.56033681483484,13.6241402746798,3.76541254431727));
#84758=CARTESIAN_POINT('Ctrl Pts',(-8.55950142175534,13.6244096996241,3.76083175625723));
#84759=CARTESIAN_POINT('Ctrl Pts',(-8.55868804299287,13.6246795794397,3.75624637375511));
#84760=CARTESIAN_POINT('Ctrl Pts',(-8.55789671636854,13.624949866793,3.75165664722065));
#84761=CARTESIAN_POINT('Ctrl Pts',(-8.5485449206615,13.6281440877793,3.69741585260893));
#84762=CARTESIAN_POINT('Ctrl Pts',(-8.54227472254286,13.6313946029861,3.64256284387078));
#84763=CARTESIAN_POINT('Ctrl Pts',(-8.53911607976639,13.6346365187915,3.58747478516665));
#84764=CARTESIAN_POINT('Ctrl Pts',(-8.53596063262516,13.6378751547133,3.53244245968546));
#84765=CARTESIAN_POINT('Ctrl Pts',(-8.53591009395743,13.6411048750132,3.47717552279635));
#84766=CARTESIAN_POINT('Ctrl Pts',(-8.5389556392251,13.6442812733838,3.42204434808979));
#84767=CARTESIAN_POINT('Ctrl Pts',(-8.54199931682544,13.647455723842,3.36694698233559));
#84768=CARTESIAN_POINT('Ctrl Pts',(-8.54813515207398,13.6505767818087,3.31198518841675));
#84769=CARTESIAN_POINT('Ctrl Pts',(-8.55731922032615,13.6536238408607,3.25752355090235));
#84770=CARTESIAN_POINT('Ctrl Pts',(-8.5665013158374,13.6566702454034,3.20307361176588));
#84771=CARTESIAN_POINT('Ctrl Pts',(-8.57873036085231,13.6596426850592,3.14912364743867));
#84772=CARTESIAN_POINT('Ctrl Pts',(-8.59392807648934,13.6625452517985,3.09603284314746));
#84773=CARTESIAN_POINT('Ctrl Pts',(-8.60913971754387,13.6654504781121,3.0428933926233));
#84774=CARTESIAN_POINT('Ctrl Pts',(-8.62732563089968,13.6682858291034,2.99061477778822));
#84775=CARTESIAN_POINT('Ctrl Pts',(-8.6483714712423,13.6710792000015,2.93955100388496));
#84776=CARTESIAN_POINT('Ctrl Pts',(-8.66942672598226,13.6738738204532,2.88846438771693));
#84777=CARTESIAN_POINT('Ctrl Pts',(-8.69334475356521,13.6766267119448,2.83859389722841));
#84778=CARTESIAN_POINT('Ctrl Pts',(-8.71997185679439,13.6793865475947,2.79028566021711));
#84779=CARTESIAN_POINT('Ctrl Pts',(-8.74664989035071,13.6821516620514,2.74188502283116));
#84780=CARTESIAN_POINT('Ctrl Pts',(-8.77604778932435,13.6849242600086,2.6950530123612));
#84781=CARTESIAN_POINT('Ctrl Pts',(-8.80796629411427,13.6877681689548,2.65012506096888));
#84782=CARTESIAN_POINT('Ctrl Pts',(-8.83337919098557,13.6900324343155,2.61435429404583));
#84783=CARTESIAN_POINT('Ctrl Pts',(-8.86038912178864,13.6923423747132,2.57979044471691));
#84784=CARTESIAN_POINT('Ctrl Pts',(-8.88887257476405,13.6947328382195,2.54659367539854));
#84785=CARTESIAN_POINT('Ctrl Pts',(-8.88888491832562,13.6947338741484,2.54657928927878));
#84786=CARTESIAN_POINT('Ctrl Pts',(-8.88889726216392,13.6947349100925,2.54656490341523));
#84787=CARTESIAN_POINT('Ctrl Pts',(-8.88890960627894,13.6947359460517,2.54655051780791));
#84788=CARTESIAN_POINT('Ctrl Pts',(-8.92169834615637,13.6974876861723,2.50833911620758));
#84789=CARTESIAN_POINT('Ctrl Pts',(-8.9565677002468,13.7003535294571,2.4717973217811));
#84790=CARTESIAN_POINT('Ctrl Pts',(-8.99330384693746,13.7032733772355,2.43713445424665));
#84791=CARTESIAN_POINT('Ctrl Pts',(-8.99673080379003,13.703545757255,2.43390090467414));
#84792=CARTESIAN_POINT('Ctrl Pts',(-9.00017396903045,13.7038186072335,2.43068371265036));
#84793=CARTESIAN_POINT('Ctrl Pts',(-9.00363314629963,13.7040918783833,2.42748305164184));
#84794=CARTESIAN_POINT('Ctrl Pts',(-9.04410156576257,13.7072888384287,2.39003897688877));
#84795=CARTESIAN_POINT('Ctrl Pts',(-9.08676704561797,13.7105428120646,2.35485586819792));
#84796=CARTESIAN_POINT('Ctrl Pts',(-9.13132804186191,13.7137888296548,2.32216441714941));
#84797=CARTESIAN_POINT('Ctrl Pts',(-9.1758447733736,13.7170316228086,2.28950544020269));
#84798=CARTESIAN_POINT('Ctrl Pts',(-9.22225309481509,13.7202661384793,2.25933284974102));
#84799=CARTESIAN_POINT('Ctrl Pts',(-9.27023617413474,13.7234478790248,2.23184096100257));
#84800=CARTESIAN_POINT('Ctrl Pts',(-9.31819053906954,13.72662771553,2.20436552416102));
#84801=CARTESIAN_POINT('Ctrl Pts',(-9.36771772897977,13.7297547023749,2.17956745466027));
#84802=CARTESIAN_POINT('Ctrl Pts',(-9.41848677567056,13.7328081680564,2.15760840596674));
#84803=CARTESIAN_POINT('Ctrl Pts',(-9.46924548951519,13.7358610122767,2.13565382652143));
#84804=CARTESIAN_POINT('Ctrl Pts',(-9.52124554430092,13.7388403670468,2.11653714951301));
#84805=CARTESIAN_POINT('Ctrl Pts',(-9.57414187350395,13.7417503029817,2.10038825685897));
#84806=CARTESIAN_POINT('Ctrl Pts',(-9.62708678578948,13.7446629115721,2.08422453211741));
#84807=CARTESIAN_POINT('Ctrl Pts',(-9.68092962567542,13.7475061000111,2.07103423323377));
#84808=CARTESIAN_POINT('Ctrl Pts',(-9.7353100624131,13.7503077856434,2.06091417345501));
#84809=CARTESIAN_POINT('Ctrl Pts',(-9.78971504058485,13.753110735653,2.05078954657831));
#84810=CARTESIAN_POINT('Ctrl Pts',(-9.84465809458332,13.7558724357173,2.04373828028838));
#84811=CARTESIAN_POINT('Ctrl Pts',(-9.89976404808854,13.7586416089291,2.03981988639053));
#84812=CARTESIAN_POINT('Ctrl Pts',(-9.95497449508993,13.7614160331269,2.03589406232132));
#84813=CARTESIAN_POINT('Ctrl Pts',(-10.0103483599692,13.7641984746339,2.03511356918302));
#84814=CARTESIAN_POINT('Ctrl Pts',(-10.0654945829337,13.7670528007821,2.03749383091482));
#84815=CARTESIAN_POINT('Ctrl Pts',(-10.1086033050148,13.7692840751295,2.03935452120257));
#84816=CARTESIAN_POINT('Ctrl Pts',(-10.1515725545089,13.7715597302384,2.0431459448033));
#84817=CARTESIAN_POINT('Ctrl Pts',(-10.1942109485973,13.7739127461963,2.0488527094524));
#84818=CARTESIAN_POINT('Ctrl Pts',(-10.1942293142312,13.7739137597107,2.04885516752692));
#84819=CARTESIAN_POINT('Ctrl Pts',(-10.1942476798041,13.7739147732396,2.04885762595655));
#84820=CARTESIAN_POINT('Ctrl Pts',(-10.194266045316,13.7739157867827,2.04886008474125));
#84821=CARTESIAN_POINT('Ctrl Pts',(-10.2442097744667,13.7766720468016,2.05554657832052));
#84822=CARTESIAN_POINT('Ctrl Pts',(-10.2938863219672,13.7795417787078,2.06489100340673));
#84823=CARTESIAN_POINT('Ctrl Pts',(-10.3430031029192,13.7824648329367,2.07682795496787));
#84824=CARTESIAN_POINT('Ctrl Pts',(-10.3475396640703,13.7827348142751,2.07793048468714));
#84825=CARTESIAN_POINT('Ctrl Pts',(-10.3520714246654,13.7830052504997,2.07905510426859));
#84826=CARTESIAN_POINT('Ctrl Pts',(-10.3565981392177,13.7832760942166,2.08020174555158));
#84827=CARTESIAN_POINT('Ctrl Pts',(-10.4100398314226,13.7864736332674,2.09373881527563));
#84828=CARTESIAN_POINT('Ctrl Pts',(-10.4627825400434,13.7897273418425,2.11034907458777));
#84829=CARTESIAN_POINT('Ctrl Pts',(-10.5144686863502,13.7929724463404,2.12990545839473));
#84830=CARTESIAN_POINT('Ctrl Pts',(-10.5661036608873,13.7962143380289,2.14944248044155));
#84831=CARTESIAN_POINT('Ctrl Pts',(-10.6166843450709,13.7994473075797,2.17191948587805));
#84832=CARTESIAN_POINT('Ctrl Pts',(-10.6658752612794,13.8026270766391,2.19717677960584));
#84833=CARTESIAN_POINT('Ctrl Pts',(-10.7150369120028,13.805804953937,2.22241904684071));
#84834=CARTESIAN_POINT('Ctrl Pts',(-10.7628105260939,13.8089295576144,2.25043818611738));
#84835=CARTESIAN_POINT('Ctrl Pts',(-10.8088802671553,13.8119804340562,2.28104483930439));
#84836=CARTESIAN_POINT('Ctrl Pts',(-10.8549408012514,13.8150307007851,2.31164537579989));
#84837=CARTESIAN_POINT('Ctrl Pts',(-10.8992981051754,13.8180072724059,2.34483240405891));
#84838=CARTESIAN_POINT('Ctrl Pts',(-10.9416552807271,13.8209144210495,2.38038740919537));
#84839=CARTESIAN_POINT('Ctrl Pts',(-10.9840516323039,13.8238242585062,2.41597529904989));
#84840=CARTESIAN_POINT('Ctrl Pts',(-11.0244439990362,13.8266646716509,2.45393565561274));
#84841=CARTESIAN_POINT('Ctrl Pts',(-11.0625548888345,13.829463751375,2.49401911485619));
#84842=CARTESIAN_POINT('Ctrl Pts',(-11.1006831095188,13.8322641039775,2.53412080200948));
#84843=CARTESIAN_POINT('Ctrl Pts',(-11.1365274799243,13.8350233770792,2.57634770869379));
#84844=CARTESIAN_POINT('Ctrl Pts',(-11.1698337107885,13.8377904239016,2.62041766331957));
#84845=CARTESIAN_POINT('Ctrl Pts',(-11.2032033178711,13.840562735954,2.66457147573996));
#84846=CARTESIAN_POINT('Ctrl Pts',(-11.2340245862339,13.8433433687054,2.71057558109447));
#84847=CARTESIAN_POINT('Ctrl Pts',(-11.2620715734637,13.8461962565836,2.75811042793408));
#84848=CARTESIAN_POINT('Ctrl Pts',(-11.2840139973899,13.8484281995272,2.795299083959));
#84849=CARTESIAN_POINT('Ctrl Pts',(-11.3042588076683,13.8507048203907,2.83342394002852));
#84850=CARTESIAN_POINT('Ctrl Pts',(-11.3227144771106,13.8530591735347,2.87231568712075));
#84851=CARTESIAN_POINT('Ctrl Pts',(-11.3227224883573,13.8530601955135,2.87233256927086));
#84852=CARTESIAN_POINT('Ctrl Pts',(-11.3227304992674,13.853061217507,2.87234945156567));
#84853=CARTESIAN_POINT('Ctrl Pts',(-11.3227385098408,13.8530622395152,2.87236633400517));
#84854=CARTESIAN_POINT('Ctrl Pts',(-11.3451309243512,13.8559191174301,2.91955878397471));
#84855=CARTESIAN_POINT('Ctrl Pts',(-11.3649563316523,13.8588965713256,2.96803084211943));
#84856=CARTESIAN_POINT('Ctrl Pts',(-11.3821167642417,13.8619287665913,3.01749211161235));
#84857=CARTESIAN_POINT('Ctrl Pts',(-11.3844554623751,13.8623420073048,3.02423290780344));
#84858=CARTESIAN_POINT('Ctrl Pts',(-11.3867446659438,13.8627562647528,3.03099199785369));
#84859=CARTESIAN_POINT('Ctrl Pts',(-11.3889841324662,13.8631713722903,3.03776857201318));
#84860=CARTESIAN_POINT('Ctrl Pts',(-11.4076065058816,13.8666232156173,3.09411944540883));
#84861=CARTESIAN_POINT('Ctrl Pts',(-11.4227902001525,13.8701330513621,3.15168650924206));
#84862=CARTESIAN_POINT('Ctrl Pts',(-11.4344372945637,13.8736242312343,3.21004616268316));
#84863=CARTESIAN_POINT('Ctrl Pts',(-11.4460380654213,13.8771015257672,3.26817370445484));
#84864=CARTESIAN_POINT('Ctrl Pts',(-11.4541308043979,13.8805599316602,3.32708788606901));
#84865=CARTESIAN_POINT('Ctrl Pts',(-11.4586520317584,13.8839512986877,3.38637061734034));
#84866=CARTESIAN_POINT('Ctrl Pts',(-11.4615197102294,13.886102340747,3.42397186996851));
#84867=CARTESIAN_POINT('Ctrl Pts',(-11.4629511893303,13.8882270014167,3.46172138259162));
#84868=CARTESIAN_POINT('Ctrl Pts',(-11.4629363565808,13.890319544931,3.49951158075118));
#84869=CARTESIAN_POINT('Origin',(-10.,13.2,3.5));
#84870=CARTESIAN_POINT('',(-11.4635,14.4604121156607,3.50000000573507));
#84871=CARTESIAN_POINT('',(-11.4635,14.3893209889657,3.49999999993469));
#84872=CARTESIAN_POINT('',(-11.4635,13.2,3.5));
#84873=CARTESIAN_POINT('Ctrl Pts',(-11.4635,14.4604121156607,3.50000000573456));
#84874=CARTESIAN_POINT('Ctrl Pts',(-11.4635000000723,14.4593041116426,3.48153842462835));
#84875=CARTESIAN_POINT('Ctrl Pts',(-11.4631506697053,14.458199281557,3.46307658818486));
#84876=CARTESIAN_POINT('Ctrl Pts',(-11.4593750689781,14.4522573821589,3.36336413420576));
#84877=CARTESIAN_POINT('Ctrl Pts',(-11.4495305890919,14.4475406793002,3.28249266876787));
#84878=CARTESIAN_POINT('Ctrl Pts',(-11.4306966054332,14.4424045849979,3.19166596886317));
#84879=CARTESIAN_POINT('Ctrl Pts',(-11.4282471587374,14.4417764267522,3.18051179128755));
#84880=CARTESIAN_POINT('Ctrl Pts',(-11.4243039418189,14.4408226099513,3.16350786520779));
#84881=CARTESIAN_POINT('Ctrl Pts',(-11.4229041527754,14.4404939788765,3.15763696315542));
#84882=CARTESIAN_POINT('Ctrl Pts',(-11.4202855199202,14.4398968440649,3.14694760675266));
#84883=CARTESIAN_POINT('Ctrl Pts',(-11.4190783767436,14.4396279717479,3.14212640223678));
#84884=CARTESIAN_POINT('Ctrl Pts',(-11.4164112600126,14.4390474464297,3.13169993002671));
#84885=CARTESIAN_POINT('Ctrl Pts',(-11.4149425184964,14.4387360790542,3.12609697820713));
#84886=CARTESIAN_POINT('Ctrl Pts',(-11.4108455316339,14.4378896327043,3.11083771440092));
#84887=CARTESIAN_POINT('Ctrl Pts',(-11.4081514169898,14.437356672603,3.10119930773066));
#84888=CARTESIAN_POINT('Ctrl Pts',(-11.3940034093553,14.4346723632037,3.05251543149943));
#84889=CARTESIAN_POINT('Ctrl Pts',(-11.381023052222,14.4325707387485,3.01393039613512));
#84890=CARTESIAN_POINT('Ctrl Pts',(-11.3614207471332,14.429798355418,2.96281930929373));
#84891=CARTESIAN_POINT('Ctrl Pts',(-11.3562023154256,14.4290918920926,2.9497774653871));
#84892=CARTESIAN_POINT('Ctrl Pts',(-11.312271596917,14.4233842111193,2.84441027958009));
#84893=CARTESIAN_POINT('Ctrl Pts',(-11.2643688016554,14.4186275547095,2.75620865429596));
#84894=CARTESIAN_POINT('Ctrl Pts',(-11.1779740760711,14.4110757507415,2.62993879687574));
#84895=CARTESIAN_POINT('Ctrl Pts',(-11.1457674738151,14.4084146233724,2.58794447189866));
#84896=CARTESIAN_POINT('Ctrl Pts',(-11.1046319578082,14.4050700608973,2.53993359604392));
#84897=CARTESIAN_POINT('Ctrl Pts',(-11.0978183953659,14.404517680338,2.53214979417164));
#84898=CARTESIAN_POINT('Ctrl Pts',(-11.0881965508677,14.4037387819038,2.52139014577647));
#84899=CARTESIAN_POINT('Ctrl Pts',(-11.0854572798457,14.4035171625098,2.5183526738616));
#84900=CARTESIAN_POINT('Ctrl Pts',(-11.0807757792988,14.4031385439883,2.51320509243872));
#84901=CARTESIAN_POINT('Ctrl Pts',(-11.0788399906273,14.4029820250326,2.51108910956974));
#84902=CARTESIAN_POINT('Ctrl Pts',(-11.0751141359171,14.4026808144987,2.50704039131262));
#84903=CARTESIAN_POINT('Ctrl Pts',(-11.0733250565243,14.4025362010696,2.50510678334688));
#84904=CARTESIAN_POINT('Ctrl Pts',(-11.0685520457656,14.4021504766622,2.49997604976387));
#84905=CARTESIAN_POINT('Ctrl Pts',(-11.065559012149,14.4019086852552,2.49678747706412));
#84906=CARTESIAN_POINT('Ctrl Pts',(-11.0547640675646,14.4010370882455,2.48539009139971));
#84907=CARTESIAN_POINT('Ctrl Pts',(-11.046881426683,14.4004015089416,2.4772586997586));
#84908=CARTESIAN_POINT('Ctrl Pts',(-10.9849167805197,14.3954179257212,2.41480560462796));
#84909=CARTESIAN_POINT('Ctrl Pts',(-10.9267410402003,14.390818790509,2.3647216474997));
#84910=CARTESIAN_POINT('Ctrl Pts',(-10.813409908893,14.382359907193,2.28169232073399));
#84911=CARTESIAN_POINT('Ctrl Pts',(-10.7594852277375,14.3785129710107,2.24736587046793));
#84912=CARTESIAN_POINT('Ctrl Pts',(-10.6522677466764,14.3713144477356,2.18859197029449));
#84913=CARTESIAN_POINT('Ctrl Pts',(-10.5994074769879,14.3679545248946,2.16360327873566));
#84914=CARTESIAN_POINT('Ctrl Pts',(-10.5316946259927,14.3638918354729,2.13642215873947));
#84915=CARTESIAN_POINT('Ctrl Pts',(-10.5181195003967,14.3630888227772,2.1312064037073));
#84916=CARTESIAN_POINT('Ctrl Pts',(-10.4982265693755,14.3619283884958,2.12390162001956));
#84917=CARTESIAN_POINT('Ctrl Pts',(-10.4919689813092,14.3615656815066,2.12165207973847));
#84918=CARTESIAN_POINT('Ctrl Pts',(-10.4809471897867,14.3609308432514,2.11777447743404));
#84919=CARTESIAN_POINT('Ctrl Pts',(-10.4761895443317,14.3606581166207,2.11612821643571));
#84920=CARTESIAN_POINT('Ctrl Pts',(-10.4662884453787,14.3600932220642,2.11275930104501));
#84921=CARTESIAN_POINT('Ctrl Pts',(-10.4611437132677,14.3598011878942,2.11104062408813));
#84922=CARTESIAN_POINT('Ctrl Pts',(-10.4478121336516,14.3590482286469,2.10666924179509));
#84923=CARTESIAN_POINT('Ctrl Pts',(-10.439611165235,14.3585887263669,2.10406005269817));
#84924=CARTESIAN_POINT('Ctrl Pts',(-10.4067988717358,14.3567644649578,2.09393845776422));
#84925=CARTESIAN_POINT('Ctrl Pts',(-10.382013560085,14.3554183583217,2.08700313939953));
#84926=CARTESIAN_POINT('Ctrl Pts',(-10.2012158785516,14.3458001169739,2.04151857700132));
#84927=CARTESIAN_POINT('Ctrl Pts',(-10.040010019301,14.3384410370629,2.02825113933093));
#84928=CARTESIAN_POINT('Ctrl Pts',(-9.84889906581922,14.328685004098,2.04398917552953));
#84929=CARTESIAN_POINT('Ctrl Pts',(-9.81800246202222,14.3270703464246,2.04752774949459));
#84930=CARTESIAN_POINT('Ctrl Pts',(-9.78133457163267,14.3250851291321,2.05291556606619));
#84931=CARTESIAN_POINT('Ctrl Pts',(-9.7754303517248,14.3247633253456,2.05382006682907));
#84932=CARTESIAN_POINT('Ctrl Pts',(-9.76629517217275,14.3242618679235,2.05527682703097));
#84933=CARTESIAN_POINT('Ctrl Pts',(-9.76306018316681,14.3240835981042,2.05580385133066));
#84934=CARTESIAN_POINT('Ctrl Pts',(-9.75707903677028,14.323752671754,2.05679889964672));
#84935=CARTESIAN_POINT('Ctrl Pts',(-9.75433243001706,14.3236001854758,2.05726389969384));
#84936=CARTESIAN_POINT('Ctrl Pts',(-9.74812293381212,14.3232542711549,2.05833341218179));
#84937=CARTESIAN_POINT('Ctrl Pts',(-9.74466090271375,14.3230605871653,2.0589425577836));
#84938=CARTESIAN_POINT('Ctrl Pts',(-9.73419980421892,14.3224729178724,2.06082207252783));
#84939=CARTESIAN_POINT('Ctrl Pts',(-9.72720787881597,14.3220768539564,2.06213098460307));
#84940=CARTESIAN_POINT('Ctrl Pts',(-9.63917112801196,14.3170509184235,2.07927699437777));
#84941=CARTESIAN_POINT('Ctrl Pts',(-9.55960573488289,14.3120988818137,2.1018936082228));
#84942=CARTESIAN_POINT('Ctrl Pts',(-9.43248107653116,14.3039162305376,2.14996276278858));
#84943=CARTESIAN_POINT('Ctrl Pts',(-9.38364848795247,14.3007006231604,2.17154621806499));
#84944=CARTESIAN_POINT('Ctrl Pts',(-9.27582037802258,14.2935248006285,2.22643350815974));
#84945=CARTESIAN_POINT('Ctrl Pts',(-9.21773281225691,14.289606747387,2.2612636563679));
#84946=CARTESIAN_POINT('Ctrl Pts',(-9.14938252960827,14.284956436793,2.308979971233));
#84947=CARTESIAN_POINT('Ctrl Pts',(-9.13665303863318,14.2840882342111,2.31817478400478));
#84948=CARTESIAN_POINT('Ctrl Pts',(-9.11857968692033,14.2828520658595,2.33167747931422));
#84949=CARTESIAN_POINT('Ctrl Pts',(-9.1131146053878,14.2824777971522,2.3358206410879));
#84950=CARTESIAN_POINT('Ctrl Pts',(-9.1036620244799,14.2818295638375,2.34309198064149));
#84951=CARTESIAN_POINT('Ctrl Pts',(-9.0996613084195,14.281554925281,2.3462027158307));
#84952=CARTESIAN_POINT('Ctrl Pts',(-9.09197729478612,14.2810268637449,2.35224168197554));
#84953=CARTESIAN_POINT('Ctrl Pts',(-9.08829180814358,14.2807733315566,2.35516701506633));
#84954=CARTESIAN_POINT('Ctrl Pts',(-9.07959407567654,14.2801743476316,2.36213942657337));
#84955=CARTESIAN_POINT('Ctrl Pts',(-9.07459429367989,14.2798295139788,2.36620194452444));
#84956=CARTESIAN_POINT('Ctrl Pts',(-9.05704701702705,14.2786172998891,2.38065319013408));
#84957=CARTESIAN_POINT('Ctrl Pts',(-9.0446460575153,14.2777570112564,2.3912184699568));
#84958=CARTESIAN_POINT('Ctrl Pts',(-8.94219975033353,14.2706121335422,2.48149498262767));
#84959=CARTESIAN_POINT('Ctrl Pts',(-8.8621202607452,14.2648278457553,2.57181574140944));
#84960=CARTESIAN_POINT('Ctrl Pts',(-8.76104575217004,14.2561345912015,2.71884301775442));
#84961=CARTESIAN_POINT('Ctrl Pts',(-8.73099024637538,14.2532817982974,2.76868119677067));
#84962=CARTESIAN_POINT('Ctrl Pts',(-8.691768093299,14.2489538794105,2.8434539025698));
#84963=CARTESIAN_POINT('Ctrl Pts',(-8.68018540558855,14.2475807272606,2.86706021964633));
#84964=CARTESIAN_POINT('Ctrl Pts',(-8.66687557727843,14.2458658947284,2.89614243831849));
#84965=CARTESIAN_POINT('Ctrl Pts',(-8.66453595075689,14.245558865472,2.90133444036668));
#84966=CARTESIAN_POINT('Ctrl Pts',(-8.66092215901931,14.2450755645916,2.90948062211416));
#84967=CARTESIAN_POINT('Ctrl Pts',(-8.65962730586755,14.2449005210417,2.91242563000101));
#84968=CARTESIAN_POINT('Ctrl Pts',(-8.65722659710088,14.2445724165034,2.9179350229826));
#84969=CARTESIAN_POINT('Ctrl Pts',(-8.65611836551723,14.2444195009755,2.9204983165843));
#84970=CARTESIAN_POINT('Ctrl Pts',(-8.65359824961482,14.244068431326,2.92637334657593));
#84971=CARTESIAN_POINT('Ctrl Pts',(-8.65219124804487,14.2438699886391,2.92968712223823));
#84972=CARTESIAN_POINT('Ctrl Pts',(-8.64853515355139,14.2433479558743,2.93838706551633));
#84973=CARTESIAN_POINT('Ctrl Pts',(-8.64630605418791,14.2430232221022,2.94378150145911));
#84974=CARTESIAN_POINT('Ctrl Pts',(-8.63120570142131,14.2407791398923,2.98095292475122));
#84975=CARTESIAN_POINT('Ctrl Pts',(-8.61942319928684,14.2388028061162,3.01315810216131));
#84976=CARTESIAN_POINT('Ctrl Pts',(-8.57994651878173,14.2313411382223,3.13406060561002));
#84977=CARTESIAN_POINT('Ctrl Pts',(-8.55958516690778,14.2256660998844,3.22492048356303));
#84978=CARTESIAN_POINT('Ctrl Pts',(-8.53747870968423,14.2151179001388,3.40041897465775));
#84979=CARTESIAN_POINT('Ctrl Pts',(-8.53417314536208,14.2102385235977,3.4844989329429));
#84980=CARTESIAN_POINT('Ctrl Pts',(-8.53863613806729,14.2049513135456,3.57987238998724));
#84981=CARTESIAN_POINT('Ctrl Pts',(-8.5393073571228,14.2043200220066,3.5913287974092));
#84982=CARTESIAN_POINT('Ctrl Pts',(-8.54053792892943,14.2033624602404,3.60880845367943));
#84983=CARTESIAN_POINT('Ctrl Pts',(-8.54099997587137,14.2030331813313,3.61483791887953));
#84984=CARTESIAN_POINT('Ctrl Pts',(-8.5419098691852,14.2024353712951,3.62581782556946));
#84985=CARTESIAN_POINT('Ctrl Pts',(-8.54234558864907,14.2021664672428,3.63076915815563));
#84986=CARTESIAN_POINT('Ctrl Pts',(-8.54334274581042,14.2015864358263,3.64147553885085));
#84987=CARTESIAN_POINT('Ctrl Pts',(-8.54391308471256,14.2012755903013,3.64722968695282));
#84988=CARTESIAN_POINT('Ctrl Pts',(-8.54555909817605,14.2004319464622,3.66289015307856));
#84989=CARTESIAN_POINT('Ctrl Pts',(-8.54670187663079,14.1999012434357,3.67278920700273));
#84990=CARTESIAN_POINT('Ctrl Pts',(-8.55295386310655,14.1972490157889,3.72248497802612));
#84991=CARTESIAN_POINT('Ctrl Pts',(-8.5595972268523,14.1951757575384,3.76207310117166));
#84992=CARTESIAN_POINT('Ctrl Pts',(-8.57074962514721,14.1924309214968,3.81507557120897));
#84993=CARTESIAN_POINT('Ctrl Pts',(-8.57383710547414,14.1917245635973,3.82876839979471));
#84994=CARTESIAN_POINT('Ctrl Pts',(-8.60074421906827,14.1859714656528,3.94057884016097));
#84995=CARTESIAN_POINT('Ctrl Pts',(-8.63446083964771,14.1811758330106,4.03603044944025));
#84996=CARTESIAN_POINT('Ctrl Pts',(-8.70032732407648,14.173589203107,4.17487939151635));
#84997=CARTESIAN_POINT('Ctrl Pts',(-8.7254762972443,14.1709362075542,4.22124861622847));
#84998=CARTESIAN_POINT('Ctrl Pts',(-8.75847528992601,14.1676015012024,4.27495503357835));
#84999=CARTESIAN_POINT('Ctrl Pts',(-8.76397473460302,14.1670500146294,4.28369665117282));
#85000=CARTESIAN_POINT('Ctrl Pts',(-8.77177917179701,14.1662721731516,4.29581565388331));
#85001=CARTESIAN_POINT('Ctrl Pts',(-8.77400662646717,14.1660506992169,4.29924289489074));
#85002=CARTESIAN_POINT('Ctrl Pts',(-8.7778209710577,14.1656722564136,4.3050583163535));
#85003=CARTESIAN_POINT('Ctrl Pts',(-8.77940059498354,14.1655157666566,4.30745127646895));
#85004=CARTESIAN_POINT('Ctrl Pts',(-8.78244527250804,14.165214554503,4.31203428387048));
#85005=CARTESIAN_POINT('Ctrl Pts',(-8.78390921989145,14.165069909931,4.31422503457328));
#85006=CARTESIAN_POINT('Ctrl Pts',(-8.78782036820243,14.16468398684,4.32004386596956));
#85007=CARTESIAN_POINT('Ctrl Pts',(-8.79027792011034,14.1644420265999,4.32366491383094));
#85008=CARTESIAN_POINT('Ctrl Pts',(-8.79916403914265,14.1635691984649,4.33663249379929));
#85009=CARTESIAN_POINT('Ctrl Pts',(-8.80568481958957,14.1629325359026,4.34591498877244));
#85010=CARTESIAN_POINT('Ctrl Pts',(-8.85927799269935,14.157736591395,4.42035120979246));
#85011=CARTESIAN_POINT('Ctrl Pts',(-8.91153357123456,14.1529018032807,4.48159650099979));
#85012=CARTESIAN_POINT('Ctrl Pts',(-9.02020076115273,14.1436770663582,4.58955370693775));
#85013=CARTESIAN_POINT('Ctrl Pts',(-9.07561640786214,14.139300727543,4.63694779045571));
#85014=CARTESIAN_POINT('Ctrl Pts',(-9.16222252812138,14.1330397108026,4.70048223279547));
#85015=CARTESIAN_POINT('Ctrl Pts',(-9.19083006085732,14.1310538033954,4.71994793299115));
#85016=CARTESIAN_POINT('Ctrl Pts',(-9.23887587363222,14.1278533088287,4.75020580317848));
#85017=CARTESIAN_POINT('Ctrl Pts',(-9.25791662228319,14.1266178564323,4.76160089664236));
#85018=CARTESIAN_POINT('Ctrl Pts',(-9.28426967129974,14.1249515490318,4.77656894295486));
#85019=CARTESIAN_POINT('Ctrl Pts',(-9.29136281270442,14.124507258797,4.7805200154813));
#85020=CARTESIAN_POINT('Ctrl Pts',(-9.30268925421853,14.1238043842731,4.7867062148745));
#85021=CARTESIAN_POINT('Ctrl Pts',(-9.30690120376539,14.1235444379114,4.78897991411648));
#85022=CARTESIAN_POINT('Ctrl Pts',(-9.31555654150454,14.1230131585737,4.79359755667895));
#85023=CARTESIAN_POINT('Ctrl Pts',(-9.32000099905483,14.122741903112,4.79593936822146));
#85024=CARTESIAN_POINT('Ctrl Pts',(-9.3302909592772,14.1221174183178,4.80129370023385));
#85025=CARTESIAN_POINT('Ctrl Pts',(-9.33614490914258,14.1217647659493,4.80428981202847));
#85026=CARTESIAN_POINT('Ctrl Pts',(-9.35465419980878,14.1206578072834,4.81360616054434));
#85027=CARTESIAN_POINT('Ctrl Pts',(-9.36738129726038,14.1199084800202,4.81978253598129));
#85028=CARTESIAN_POINT('Ctrl Pts',(-9.43041675037628,14.1162522247754,4.84925182961821));
#85029=CARTESIAN_POINT('Ctrl Pts',(-9.48193329907797,14.1134371534019,4.86985886809654));
#85030=CARTESIAN_POINT('Ctrl Pts',(-9.63117826927043,14.1056128422882,4.91993018253081));
#85031=CARTESIAN_POINT('Ctrl Pts',(-9.73097715768316,14.1007816779589,4.94217076653062));
#85032=CARTESIAN_POINT('Ctrl Pts',(-9.84580858331721,14.0950306734715,4.95541845802973));
#85033=CARTESIAN_POINT('Ctrl Pts',(-9.85936435064441,14.094348422177,4.95679081582959));
#85034=CARTESIAN_POINT('Ctrl Pts',(-9.90854990123835,14.0918548999297,4.96107735538652));
#85035=CARTESIAN_POINT('Ctrl Pts',(-9.94426186570979,14.0900102745399,4.96287491830589));
#85036=CARTESIAN_POINT('Ctrl Pts',(-9.9859160960748,14.0877831684182,4.96344418748409));
#85037=CARTESIAN_POINT('Ctrl Pts',(-9.99183164097463,14.0874651081145,4.96348916011669));
#85038=CARTESIAN_POINT('Ctrl Pts',(-10.0013323907847,14.0869512015507,4.96350378489108));
#85039=CARTESIAN_POINT('Ctrl Pts',(-10.0049175553373,14.0867565712009,4.96349612939262));
#85040=CARTESIAN_POINT('Ctrl Pts',(-10.011300111432,14.086408766205,4.96345904750473));
#85041=CARTESIAN_POINT('Ctrl Pts',(-10.0140974866146,14.0862558784797,4.96343477374512));
#85042=CARTESIAN_POINT('Ctrl Pts',(-10.0200833735656,14.0859277446791,4.96336566732801));
#85043=CARTESIAN_POINT('Ctrl Pts',(-10.0232717637088,14.0857523731999,4.96331843520849));
#85044=CARTESIAN_POINT('Ctrl Pts',(-10.0320239643193,14.0852694011451,4.96316017037511));
#85045=CARTESIAN_POINT('Ctrl Pts',(-10.0375872760037,14.0849606554884,4.96302782376296));
#85046=CARTESIAN_POINT('Ctrl Pts',(-10.0674965618524,14.0832918933654,4.96214559951987));
#85047=CARTESIAN_POINT('Ctrl Pts',(-10.0918203738008,14.0819031115467,4.96081977528727));
#85048=CARTESIAN_POINT('Ctrl Pts',(-10.1671359390982,14.0775276505674,4.95482616566594));
#85049=CARTESIAN_POINT('Ctrl Pts',(-10.217922462486,14.0744708450747,4.94808935210492));
#85050=CARTESIAN_POINT('Ctrl Pts',(-10.3969462058607,14.0635248014939,4.91471019988736));
#85051=CARTESIAN_POINT('Ctrl Pts',(-10.5218715913884,14.0556387861717,4.87354798843426));
#85052=CARTESIAN_POINT('Ctrl Pts',(-10.6533726533742,14.0474842713034,4.80964450075971));
#85053=CARTESIAN_POINT('Ctrl Pts',(-10.6669763424547,14.0466415041869,4.80276902244779));
#85054=CARTESIAN_POINT('Ctrl Pts',(-10.6860154999664,14.0454628042309,4.79276997609644));
#85055=CARTESIAN_POINT('Ctrl Pts',(-10.6915417865954,14.0451207705642,4.78982224992127));
#85056=CARTESIAN_POINT('Ctrl Pts',(-10.7011469979569,14.0445264032371,4.78461934356134));
#85057=CARTESIAN_POINT('Ctrl Pts',(-10.7052343606598,14.0442735165954,4.78238000134131));
#85058=CARTESIAN_POINT('Ctrl Pts',(-10.7137746384088,14.0437451797012,4.77764786107218));
#85059=CARTESIAN_POINT('Ctrl Pts',(-10.7182253585414,14.0434698703348,4.77515121714888));
#85060=CARTESIAN_POINT('Ctrl Pts',(-10.7288002525965,14.0428157644681,4.76914626961165));
#85061=CARTESIAN_POINT('Ctrl Pts',(-10.7349123175732,14.042437728101,4.7656168257832));
#85062=CARTESIAN_POINT('Ctrl Pts',(-10.7555463406542,14.0411613810557,4.75350172289471));
#85063=CARTESIAN_POINT('Ctrl Pts',(-10.7699455910349,14.040270518108,4.74470906642126));
#85064=CARTESIAN_POINT('Ctrl Pts',(-10.8040071821918,14.0381604219844,4.7230926336885));
#85065=CARTESIAN_POINT('Ctrl Pts',(-10.823519553052,14.0369494307768,4.71004080914583));
#85066=CARTESIAN_POINT('Ctrl Pts',(-10.9373481063402,14.0298510092092,4.62987156839359));
#85067=CARTESIAN_POINT('Ctrl Pts',(-11.023739952332,14.024361667009,4.552229863221));
#85068=CARTESIAN_POINT('Ctrl Pts',(-11.1413359322687,14.0155933574891,4.41820311469097));
#85069=CARTESIAN_POINT('Ctrl Pts',(-11.1795280376052,14.0124578945094,4.36859459021663));
#85070=CARTESIAN_POINT('Ctrl Pts',(-11.2184677304692,14.0087352368312,4.31069174116087));
#85071=CARTESIAN_POINT('Ctrl Pts',(-11.2224648458871,14.0083461749696,4.30465172940805));
#85072=CARTESIAN_POINT('Ctrl Pts',(-11.2283491213237,14.0077625971509,4.29561499816345));
#85073=CARTESIAN_POINT('Ctrl Pts',(-11.2302705649923,14.007570278141,4.29264060300603));
#85074=CARTESIAN_POINT('Ctrl Pts',(-11.2336851923166,14.007225290817,4.28731243232751));
#85075=CARTESIAN_POINT('Ctrl Pts',(-11.2351824645837,14.0070728948977,4.2849613359059));
#85076=CARTESIAN_POINT('Ctrl Pts',(-11.2384151521333,14.0067414044978,4.27985304665037));
#85077=CARTESIAN_POINT('Ctrl Pts',(-11.2401480564084,14.0065621557493,4.27709437082169));
#85078=CARTESIAN_POINT('Ctrl Pts',(-11.2449842294291,14.0060575873514,4.26933810823639));
#85079=CARTESIAN_POINT('Ctrl Pts',(-11.2480665611999,14.0057309504855,4.26432762132821));
#85080=CARTESIAN_POINT('Ctrl Pts',(-11.2663870047416,14.003759559667,4.2341404967701));
#85081=CARTESIAN_POINT('Ctrl Pts',(-11.2808921145457,14.0020726540537,4.20852908496264));
#85082=CARTESIAN_POINT('Ctrl Pts',(-11.3570099687491,13.9925563484428,4.06414330473809));
#85083=CARTESIAN_POINT('Ctrl Pts',(-11.4028839154276,13.9842775844866,3.93778639184374));
#85084=CARTESIAN_POINT('Ctrl Pts',(-11.4414821788112,13.9735635673457,3.7578430097127));
#85085=CARTESIAN_POINT('Ctrl Pts',(-11.4494808128266,13.9707064496622,3.70823090366372));
#85086=CARTESIAN_POINT('Ctrl Pts',(-11.4559646310173,13.9673914050103,3.64863948814271));
#85087=CARTESIAN_POINT('Ctrl Pts',(-11.4569196210957,13.9668569242536,3.63896736410953));
#85088=CARTESIAN_POINT('Ctrl Pts',(-11.4583294345449,13.9659842211894,3.62307089487082));
#85089=CARTESIAN_POINT('Ctrl Pts',(-11.4588409097876,13.9656442457038,3.61685198518387));
#85090=CARTESIAN_POINT('Ctrl Pts',(-11.4596892954621,13.9650349902647,3.60566098155111));
#85091=CARTESIAN_POINT('Ctrl Pts',(-11.4600406111535,13.9647652662042,3.60069010350523));
#85092=CARTESIAN_POINT('Ctrl Pts',(-11.4607353402448,13.9641920063239,3.59009058643531));
#85093=CARTESIAN_POINT('Ctrl Pts',(-11.4610716257979,13.9638886962335,3.58446155050797));
#85094=CARTESIAN_POINT('Ctrl Pts',(-11.4618914662117,13.9630727341222,3.56926321728734));
#85095=CARTESIAN_POINT('Ctrl Pts',(-11.4623136008877,13.9625619925752,3.55969079303546));
#85096=CARTESIAN_POINT('Ctrl Pts',(-11.4632139046721,13.9611683106935,3.53341466330243));
#85097=CARTESIAN_POINT('Ctrl Pts',(-11.4634999999312,13.9602913597298,3.51670731772259));
#85098=CARTESIAN_POINT('Ctrl Pts',(-11.4635,13.9594225818479,3.50000000603013));
#85099=CARTESIAN_POINT('Ctrl Pts',(-11.4634999124217,13.8906444325997,3.49949369805951));
#85100=CARTESIAN_POINT('Ctrl Pts',(-11.4635032710664,13.8911858909132,3.50920208713336));
#85101=CARTESIAN_POINT('Ctrl Pts',(-11.4634100262615,13.8917243994204,3.51891046394916));
#85102=CARTESIAN_POINT('Ctrl Pts',(-11.4630599651482,13.8927118813261,3.5368092430745));
#85103=CARTESIAN_POINT('Ctrl Pts',(-11.4628309580255,13.8931616918135,3.54499971198327));
#85104=CARTESIAN_POINT('Ctrl Pts',(-11.4623552135967,13.8938769137533,3.55808147343423));
#85105=CARTESIAN_POINT('Ctrl Pts',(-11.4621526902116,13.8941436923484,3.56297411859369));
#85106=CARTESIAN_POINT('Ctrl Pts',(-11.4617040830429,13.8946692244319,3.57263776807771));
#85107=CARTESIAN_POINT('Ctrl Pts',(-11.4614591871489,13.894928011513,3.57740876427155));
#85108=CARTESIAN_POINT('Ctrl Pts',(-11.4608882362896,13.8954772699635,3.58756066605114));
#85109=CARTESIAN_POINT('Ctrl Pts',(-11.4605558026249,13.8957675389846,3.59294115158493));
#85110=CARTESIAN_POINT('Ctrl Pts',(-11.4596250734639,13.8965111611674,3.60676385876572));
#85111=CARTESIAN_POINT('Ctrl Pts',(-11.4589832576214,13.8969631558713,3.61520301501556));
#85112=CARTESIAN_POINT('Ctrl Pts',(-11.456177683201,13.8987280206099,3.64829428153379));
#85113=CARTESIAN_POINT('Ctrl Pts',(-11.4534619514906,13.9000237246107,3.67289617978589));
#85114=CARTESIAN_POINT('Ctrl Pts',(-11.4336082383893,13.9076269398112,3.81873030306006));
#85115=CARTESIAN_POINT('Ctrl Pts',(-11.4019376940631,13.9134477571552,3.93748498438483));
#85116=CARTESIAN_POINT('Ctrl Pts',(-11.3377899299475,13.9217963971866,4.09535860170369));
#85117=CARTESIAN_POINT('Ctrl Pts',(-11.3175574215204,13.9241757404651,4.1388862213477));
#85118=CARTESIAN_POINT('Ctrl Pts',(-11.284335208419,13.9278510626477,4.20204169542735));
#85119=CARTESIAN_POINT('Ctrl Pts',(-11.2729504157475,13.9290771281436,4.2224794705723));
#85120=CARTESIAN_POINT('Ctrl Pts',(-11.2582943219294,13.9306267833715,4.24736725694616));
#85121=CARTESIAN_POINT('Ctrl Pts',(-11.2554806555111,13.9309230561008,4.25208426327092));
#85122=CARTESIAN_POINT('Ctrl Pts',(-11.2510007026186,13.9313930442305,4.25949953820821));
#85123=CARTESIAN_POINT('Ctrl Pts',(-11.249352054374,13.9315656380569,4.26220846907503));
#85124=CARTESIAN_POINT('Ctrl Pts',(-11.2462308447665,13.931891750029,4.26729966453415));
#85125=CARTESIAN_POINT('Ctrl Pts',(-11.2447602418358,13.9320451420336,4.26968307342567));
#85126=CARTESIAN_POINT('Ctrl Pts',(-11.2413778284302,13.9323973386053,4.27512990957486));
#85127=CARTESIAN_POINT('Ctrl Pts',(-11.2394615138154,13.9325964344036,4.27819049392208));
#85128=CARTESIAN_POINT('Ctrl Pts',(-11.2343305451963,13.9331282804365,4.28631823418877));
#85129=CARTESIAN_POINT('Ctrl Pts',(-11.2310960534466,13.9334622731247,4.2913727092182));
#85130=CARTESIAN_POINT('Ctrl Pts',(-11.2072295451169,13.9359166505887,4.32816800062603));
#85131=CARTESIAN_POINT('Ctrl Pts',(-11.185405460241,13.9381063904024,4.35911514716666));
#85132=CARTESIAN_POINT('Ctrl Pts',(-11.1061530438012,13.9457875977111,4.46272048388466));
#85133=CARTESIAN_POINT('Ctrl Pts',(-11.0430462057516,13.9514431051591,4.53075715632658));
#85134=CARTESIAN_POINT('Ctrl Pts',(-10.9231761460071,13.9610020037966,4.6376301220376));
#85135=CARTESIAN_POINT('Ctrl Pts',(-10.8693218313548,13.9649640960408,4.67929553407391));
#85136=CARTESIAN_POINT('Ctrl Pts',(-10.8015697887803,13.9695387882705,4.72454038346953));
#85137=CARTESIAN_POINT('Ctrl Pts',(-10.7902779621024,13.9702887020011,4.73185796119353));
#85138=CARTESIAN_POINT('Ctrl Pts',(-10.7723084958512,13.971462694586,4.74315413680451));
#85139=CARTESIAN_POINT('Ctrl Pts',(-10.7656975193451,13.9718905446668,4.74723691925821));
#85140=CARTESIAN_POINT('Ctrl Pts',(-10.753138277802,13.9726957864608,4.75485571390308));
#85141=CARTESIAN_POINT('Ctrl Pts',(-10.7471968583926,13.9730735640408,4.75840255296829));
#85142=CARTESIAN_POINT('Ctrl Pts',(-10.7369039082363,13.9737226624015,4.76444851905635));
#85143=CARTESIAN_POINT('Ctrl Pts',(-10.7325643033987,13.9739946998868,4.76696762767455));
#85144=CARTESIAN_POINT('Ctrl Pts',(-10.7241787170347,13.9745172714312,4.77177791058589));
#85145=CARTESIAN_POINT('Ctrl Pts',(-10.7201346097001,13.9747679153383,4.77407221642244));
#85146=CARTESIAN_POINT('Ctrl Pts',(-10.7106646635601,13.9753516683393,4.77938521835069));
#85147=CARTESIAN_POINT('Ctrl Pts',(-10.7052303885801,13.9756842366191,4.78238874823704));
#85148=CARTESIAN_POINT('Ctrl Pts',(-10.6863698495434,13.9768302803127,4.79265684254898));
#85149=CARTESIAN_POINT('Ctrl Pts',(-10.6728488964784,13.9776375945381,4.79974600155214));
#85150=CARTESIAN_POINT('Ctrl Pts',(-10.5422131558147,13.9853087273094,4.86565454267108));
#85151=CARTESIAN_POINT('Ctrl Pts',(-10.4178144227959,13.9915594092099,4.90870166175729));
#85152=CARTESIAN_POINT('Ctrl Pts',(-10.2392156905274,14.0004685511921,4.94472238624106));
#85153=CARTESIAN_POINT('Ctrl Pts',(-10.1885989004517,14.0029960243115,4.95219719251997));
#85154=CARTESIAN_POINT('Ctrl Pts',(-10.1134650391501,14.0068770226795,4.95929792903287));
#85155=CARTESIAN_POINT('Ctrl Pts',(-10.0891794962779,14.0081513906661,4.9609831075946));
#85156=CARTESIAN_POINT('Ctrl Pts',(-10.0593030301201,14.0097555814205,4.9623085835812));
#85157=CARTESIAN_POINT('Ctrl Pts',(-10.0537400927606,14.0100558291128,4.96252358730388));
#85158=CARTESIAN_POINT('Ctrl Pts',(-10.044986850254,14.0105308914473,4.96281188674444));
#85159=CARTESIAN_POINT('Ctrl Pts',(-10.0417972420909,14.0107045482622,4.96290649832834));
#85160=CARTESIAN_POINT('Ctrl Pts',(-10.0358088613235,14.0110316536179,4.96306452783837));
#85161=CARTESIAN_POINT('Ctrl Pts',(-10.033010203,14.011184968555,4.9631303473121));
#85162=CARTESIAN_POINT('Ctrl Pts',(-10.0266238685112,14.0115358213642,4.96326221005647));
#85163=CARTESIAN_POINT('Ctrl Pts',(-10.0230361319911,14.0117336408742,4.96332308866219));
#85164=CARTESIAN_POINT('Ctrl Pts',(-10.0135256133057,14.0122598616147,4.96344948377995));
#85165=CARTESIAN_POINT('Ctrl Pts',(-10.0076026573392,14.0125894649278,4.96349223809736));
#85166=CARTESIAN_POINT('Ctrl Pts',(-9.96568245246635,14.0149348095153,4.96354035136587));
#85167=CARTESIAN_POINT('Ctrl Pts',(-9.92969865646566,14.0170133029548,4.96225352223029));
#85168=CARTESIAN_POINT('Ctrl Pts',(-9.88394151331369,14.0197097919931,4.95892440558378));
#85169=CARTESIAN_POINT('Ctrl Pts',(-9.87408870873401,14.0202936117471,4.95810710666906));
#85170=CARTESIAN_POINT('Ctrl Pts',(-9.77548719422565,14.0261637115097,4.94892118096201));
#85171=CARTESIAN_POINT('Ctrl Pts',(-9.687670053473,14.0316009288096,4.9325604251217));
#85172=CARTESIAN_POINT('Ctrl Pts',(-9.53535740836338,14.0409980668464,4.88950320621494));
#85173=CARTESIAN_POINT('Ctrl Pts',(-9.47023960214507,14.0450070400785,4.86600435201072));
#85174=CARTESIAN_POINT('Ctrl Pts',(-9.39250012515686,14.0497521247001,4.83155112284302));
#85175=CARTESIAN_POINT('Ctrl Pts',(-9.37808546408041,14.0506304836527,4.82487992989306));
#85176=CARTESIAN_POINT('Ctrl Pts',(-9.35757621043408,14.0518784705054,4.81497962268128));
#85177=CARTESIAN_POINT('Ctrl Pts',(-9.35139174446376,14.0522545665639,4.81194019169793));
#85178=CARTESIAN_POINT('Ctrl Pts',(-9.34069043955313,14.0529050090987,4.806586738772));
#85179=CARTESIAN_POINT('Ctrl Pts',(-9.33616377888516,14.0531800416248,4.80429271057883));
#85180=CARTESIAN_POINT('Ctrl Pts',(-9.32746828180742,14.0537081951419,4.79982899771809));
#85181=CARTESIAN_POINT('Ctrl Pts',(-9.32329779055664,14.0539614293269,4.79766268950284));
#85182=CARTESIAN_POINT('Ctrl Pts',(-9.31345917862181,14.0545586894861,4.79249181978395));
#85183=CARTESIAN_POINT('Ctrl Pts',(-9.30780020957477,14.0549021066307,4.78946999016714));
#85184=CARTESIAN_POINT('Ctrl Pts',(-9.28798913417361,14.0561040985067,4.77872308555758));
#85185=CARTESIAN_POINT('Ctrl Pts',(-9.27394470261818,14.0569557413303,4.77080129636367));
#85186=CARTESIAN_POINT('Ctrl Pts',(-9.15456093815374,14.0641982457844,4.70083729320009));
#85187=CARTESIAN_POINT('Ctrl Pts',(-9.05725069768205,14.0700690851717,4.62605664361488));
#85188=CARTESIAN_POINT('Ctrl Pts',(-8.92997519251147,14.0787997333249,4.50005475628076));
#85189=CARTESIAN_POINT('Ctrl Pts',(-8.89195061040829,14.081591714299,4.45775168258011));
#85190=CARTESIAN_POINT('Ctrl Pts',(-8.84029492113772,14.0858366818902,4.39307858175174));
#85191=CARTESIAN_POINT('Ctrl Pts',(-8.82464786221086,14.0871921305771,4.37238317896592));
#85192=CARTESIAN_POINT('Ctrl Pts',(-8.80626008658573,14.0888871728448,4.3466696246112));
#85193=CARTESIAN_POINT('Ctrl Pts',(-8.80298708656365,14.08919304817,4.34203593573131));
#85194=CARTESIAN_POINT('Ctrl Pts',(-8.79790284446138,14.08967495651,4.33474846570885));
#85195=CARTESIAN_POINT('Ctrl Pts',(-8.79607322454802,14.0898497733384,4.33210749984603));
#85196=CARTESIAN_POINT('Ctrl Pts',(-8.79266873726176,14.0901777323262,4.3271585573484));
#85197=CARTESIAN_POINT('Ctrl Pts',(-8.79109177519245,14.0903307310507,4.32485208404071));
#85198=CARTESIAN_POINT('Ctrl Pts',(-8.78749317068819,14.0906823651433,4.31955625925411));
#85199=CARTESIAN_POINT('Ctrl Pts',(-8.7854759788767,14.0908812922157,4.3165639440667));
#85200=CARTESIAN_POINT('Ctrl Pts',(-8.78020990389279,14.0914053458062,4.30868953355507));
#85201=CARTESIAN_POINT('Ctrl Pts',(-8.77697929491117,14.0917316298276,4.30379536750177));
#85202=CARTESIAN_POINT('Ctrl Pts',(-8.75476657696193,14.0940078564958,4.26970057258097));
#85203=CARTESIAN_POINT('Ctrl Pts',(-8.73680406952355,14.0960165956496,4.23985195342664));
#85204=CARTESIAN_POINT('Ctrl Pts',(-8.6976050923087,14.1007638637677,4.16911880973339));
#85205=CARTESIAN_POINT('Ctrl Pts',(-8.67719957349552,14.1035259533372,4.12781459708676));
#85206=CARTESIAN_POINT('Ctrl Pts',(-8.60931610861705,14.1137367789869,3.97234335341583));
#85207=CARTESIAN_POINT('Ctrl Pts',(-8.57439636355503,14.1211479511917,3.85323508322942));
#85208=CARTESIAN_POINT('Ctrl Pts',(-8.55237215857691,14.1289287233202,3.71553564884653));
#85209=CARTESIAN_POINT('Ctrl Pts',(-8.55012914148257,14.129802627925,3.69989123127804));
#85210=CARTESIAN_POINT('Ctrl Pts',(-8.54727434022999,14.1310454328642,3.67739135523392));
#85211=CARTESIAN_POINT('Ctrl Pts',(-8.54645687123336,14.1314207296773,3.67056350882363));
#85212=CARTESIAN_POINT('Ctrl Pts',(-8.54512015145841,14.1320702057688,3.65869025793949));
#85213=CARTESIAN_POINT('Ctrl Pts',(-8.54457895347306,14.1323450659023,3.65364748577135));
#85214=CARTESIAN_POINT('Ctrl Pts',(-8.54358653583629,14.132873178244,3.64392421824097));
#85215=CARTESIAN_POINT('Ctrl Pts',(-8.54313163891788,14.1331265419234,3.6392441682159));
#85216=CARTESIAN_POINT('Ctrl Pts',(-8.54210838049684,14.1337245519092,3.62816232078356));
#85217=CARTESIAN_POINT('Ctrl Pts',(-8.54155961536221,14.1340685852731,3.62175878174878));
#85218=CARTESIAN_POINT('Ctrl Pts',(-8.53977649447696,14.1352750360525,3.5992062115059));
#85219=CARTESIAN_POINT('Ctrl Pts',(-8.53876801501689,14.1361304509997,3.58304018311448));
#85220=CARTESIAN_POINT('Ctrl Pts',(-8.53248259780247,14.1433304939431,3.44560282877686));
#85221=CARTESIAN_POINT('Ctrl Pts',(-8.54204308505491,14.1491636747077,3.32412945788826));
#85222=CARTESIAN_POINT('Ctrl Pts',(-8.57805434608823,14.15787729412,3.1490059559888));
#85223=CARTESIAN_POINT('Ctrl Pts',(-8.59291071834515,14.1606950199935,3.09352106106201));
#85224=CARTESIAN_POINT('Ctrl Pts',(-8.61920250345888,14.1649751413803,3.01429303644262));
#85225=CARTESIAN_POINT('Ctrl Pts',(-8.62808030387407,14.1663381251565,2.98975578271803));
#85226=CARTESIAN_POINT('Ctrl Pts',(-8.63968409872609,14.1680416071993,2.96018040847446));
#85227=CARTESIAN_POINT('Ctrl Pts',(-8.64179039701179,14.1683479887029,2.95490256387294));
#85228=CARTESIAN_POINT('Ctrl Pts',(-8.64513632337104,14.168830515243,2.94665833060462));
#85229=CARTESIAN_POINT('Ctrl Pts',(-8.64635510246021,14.1690054388122,2.94368347472463));
#85230=CARTESIAN_POINT('Ctrl Pts',(-8.64865142077304,14.1693334992296,2.93813073226279));
#85231=CARTESIAN_POINT('Ctrl Pts',(-8.64972654561636,14.1694864918822,2.93555190268197));
#85232=CARTESIAN_POINT('Ctrl Pts',(-8.65220620303712,14.1698379696396,2.92965174255666));
#85233=CARTESIAN_POINT('Ctrl Pts',(-8.65361562770511,14.1700367453811,2.92633252195491));
#85234=CARTESIAN_POINT('Ctrl Pts',(-8.65734537343156,14.1705600907946,2.91763836169766));
#85235=CARTESIAN_POINT('Ctrl Pts',(-8.65968568084542,14.1708858126703,2.91227213138819));
#85236=CARTESIAN_POINT('Ctrl Pts',(-8.67608519559245,14.1731493982531,2.8752761024063));
#85237=CARTESIAN_POINT('Ctrl Pts',(-8.69122949671118,14.1751453328076,2.84414196965002));
#85238=CARTESIAN_POINT('Ctrl Pts',(-8.71494682760646,14.178113061807,2.7994821412635));
#85239=CARTESIAN_POINT('Ctrl Pts',(-8.72266172865886,14.1790569898152,2.78551148116026));
#85240=CARTESIAN_POINT('Ctrl Pts',(-8.77642708612927,14.1854820287117,2.69180454241418));
#85241=CARTESIAN_POINT('Ctrl Pts',(-8.82968620171524,14.1910977721433,2.61644040014841));
#85242=CARTESIAN_POINT('Ctrl Pts',(-8.93058345149162,14.2002493353626,2.49893892311125));
#85243=CARTESIAN_POINT('Ctrl Pts',(-8.9745170527604,14.2038732225143,2.45397832813544));
#85244=CARTESIAN_POINT('Ctrl Pts',(-9.03243913592683,14.2082154081896,2.4018713935886));
#85245=CARTESIAN_POINT('Ctrl Pts',(-9.04382609879661,14.2090501680802,2.39194225934966));
#85246=CARTESIAN_POINT('Ctrl Pts',(-9.06052367029214,14.2102476589927,2.37783152260777));
#85247=CARTESIAN_POINT('Ctrl Pts',(-9.06571244959343,14.2106161593746,2.3735078158146));
#85248=CARTESIAN_POINT('Ctrl Pts',(-9.0748346356763,14.2112577718285,2.36601286457413));
#85249=CARTESIAN_POINT('Ctrl Pts',(-9.0787548505221,14.2115315179099,2.36282580485295));
#85250=CARTESIAN_POINT('Ctrl Pts',(-9.0863811381315,14.2120602621776,2.35669109711661));
#85251=CARTESIAN_POINT('Ctrl Pts',(-9.09008516347825,14.2123153555749,2.35374101391647));
#85252=CARTESIAN_POINT('Ctrl Pts',(-9.0989491470618,14.2129217796122,2.34675130489529));
#85253=CARTESIAN_POINT('Ctrl Pts',(-9.10412207261081,14.2132724554158,2.34272823699314));
#85254=CARTESIAN_POINT('Ctrl Pts',(-9.12277459649179,14.2145255735667,2.32842188481019));
#85255=CARTESIAN_POINT('Ctrl Pts',(-9.13640591385913,14.2154202717952,2.31833804566199));
#85256=CARTESIAN_POINT('Ctrl Pts',(-9.23892428091119,14.2220019485415,2.24522130191374));
#85257=CARTESIAN_POINT('Ctrl Pts',(-9.33442725608668,14.2272907522713,2.19205449586917));
#85258=CARTESIAN_POINT('Ctrl Pts',(-9.4960128214411,14.2358090642966,2.12442366659073));
#85259=CARTESIAN_POINT('Ctrl Pts',(-9.558729519278,14.2390309998275,2.10304169936223));
#85260=CARTESIAN_POINT('Ctrl Pts',(-9.65002929994171,14.2438589385648,2.0786786318));
#85261=CARTESIAN_POINT('Ctrl Pts',(-9.67759021020195,14.2453341119206,2.07217450623295));
#85262=CARTESIAN_POINT('Ctrl Pts',(-9.7110222790235,14.2471633097302,2.06530211867285));
#85263=CARTESIAN_POINT('Ctrl Pts',(-9.71673089268684,14.2474770376255,2.06416409556601));
#85264=CARTESIAN_POINT('Ctrl Pts',(-9.72563267694309,14.2479686213699,2.0624446600172));
#85265=CARTESIAN_POINT('Ctrl Pts',(-9.72882131420717,14.2481451799787,2.06183975043562));
#85266=CARTESIAN_POINT('Ctrl Pts',(-9.73475495769333,14.2484746541843,2.0607345266009));
#85267=CARTESIAN_POINT('Ctrl Pts',(-9.73749939668629,14.2486274130061,2.06023145323678));
#85268=CARTESIAN_POINT('Ctrl Pts',(-9.74375075003085,14.2489762053549,2.05910400788803));
#85269=CARTESIAN_POINT('Ctrl Pts',(-9.74725850233021,14.2491725124807,2.05848459148154));
#85270=CARTESIAN_POINT('Ctrl Pts',(-9.75639311946363,14.2496851998631,2.05690592140658));
#85271=CARTESIAN_POINT('Ctrl Pts',(-9.76202334215519,14.2500026593933,2.0559667801384));
#85272=CARTESIAN_POINT('Ctrl Pts',(-9.79892082977262,14.252092015672,2.05003379366724));
#85273=CARTESIAN_POINT('Ctrl Pts',(-9.8303355587873,14.2539125479754,2.04602320605826));
#85274=CARTESIAN_POINT('Ctrl Pts',(-9.87327476152129,14.2564355497007,2.04195178757122));
#85275=CARTESIAN_POINT('Ctrl Pts',(-9.88470849612051,14.257110708452,2.04100317505609));
#85276=CARTESIAN_POINT('Ctrl Pts',(-9.98805535957383,14.2632370996351,2.03365128649823));
#85277=CARTESIAN_POINT('Ctrl Pts',(-10.0803708557154,14.2688627528796,2.03580652673169));
#85278=CARTESIAN_POINT('Ctrl Pts',(-10.2226423370278,14.2773691824545,2.05263128331906));
#85279=CARTESIAN_POINT('Ctrl Pts',(-10.2730654554302,14.2803548821478,2.06129160435795));
#85280=CARTESIAN_POINT('Ctrl Pts',(-10.3520953055363,14.2849657170242,2.07917103588605));
#85281=CARTESIAN_POINT('Ctrl Pts',(-10.3810472216457,14.2866402884213,2.08666025011202));
#85282=CARTESIAN_POINT('Ctrl Pts',(-10.4181580309301,14.2887688950394,2.09748340421269));
#85283=CARTESIAN_POINT('Ctrl Pts',(-10.4265430364494,14.2892486649193,2.10001072038826));
#85284=CARTESIAN_POINT('Ctrl Pts',(-10.4401170826114,14.2900235277542,2.10423533468347));
#85285=CARTESIAN_POINT('Ctrl Pts',(-10.445320114575,14.290320104036,2.10588664591674));
#85286=CARTESIAN_POINT('Ctrl Pts',(-10.4552950013835,14.2908878815622,2.10911396433005));
#85287=CARTESIAN_POINT('Ctrl Pts',(-10.46006820856,14.2911592232891,2.11068551189828));
#85288=CARTESIAN_POINT('Ctrl Pts',(-10.4709653296392,14.2917779229859,2.11433563609061));
#85289=CARTESIAN_POINT('Ctrl Pts',(-10.4770837747838,14.2921247498063,2.11643028914363));
#85290=CARTESIAN_POINT('Ctrl Pts',(-10.4932879215678,14.2930419221006,2.1220980586177));
#85291=CARTESIAN_POINT('Ctrl Pts',(-10.5033487668819,14.2936099615852,2.12574137784267));
#85292=CARTESIAN_POINT('Ctrl Pts',(-10.5898977075677,14.2984862620739,2.15816120114442));
#85293=CARTESIAN_POINT('Ctrl Pts',(-10.6638946856737,14.3025741231933,2.19318833173846));
#85294=CARTESIAN_POINT('Ctrl Pts',(-10.7883826980132,14.3096251898686,2.26543387012209));
#85295=CARTESIAN_POINT('Ctrl Pts',(-10.8401319481357,14.3126196953081,2.30005043258246));
#85296=CARTESIAN_POINT('Ctrl Pts',(-10.9370757284407,14.3186125422779,2.37425242145927));
#85297=CARTESIAN_POINT('Ctrl Pts',(-10.9823467030928,14.3216019416517,2.4135322903232));
#85298=CARTESIAN_POINT('Ctrl Pts',(-11.0329370496065,14.3253455418522,2.46318058809871));
#85299=CARTESIAN_POINT('Ctrl Pts',(-11.0407066954874,14.3259327124718,2.47097959162656));
#85300=CARTESIAN_POINT('Ctrl Pts',(-11.0513131777703,14.3267526058414,2.48186914603582));
#85301=CARTESIAN_POINT('Ctrl Pts',(-11.0542260102086,14.3269797202769,2.48488554730696));
#85302=CARTESIAN_POINT('Ctrl Pts',(-11.0591235563383,14.3273649751488,2.49000104575627));
#85303=CARTESIAN_POINT('Ctrl Pts',(-11.0611151159603,14.3275225944139,2.49209360272408));
#85304=CARTESIAN_POINT('Ctrl Pts',(-11.0648971291998,14.3278237772223,2.49609104571092));
#85305=CARTESIAN_POINT('Ctrl Pts',(-11.0666886947265,14.3279672506064,2.4979948540056));
#85306=CARTESIAN_POINT('Ctrl Pts',(-11.0713889883588,14.3283457509564,2.50301651597053));
#85307=CARTESIAN_POINT('Ctrl Pts',(-11.0742891851997,14.3285814125397,2.50614227505617));
#85308=CARTESIAN_POINT('Ctrl Pts',(-11.0843897913738,14.329409457747,2.51712432224812));
#85309=CARTESIAN_POINT('Ctrl Pts',(-11.091517839206,14.3300069039825,2.52504635456808));
#85310=CARTESIAN_POINT('Ctrl Pts',(-11.1665083321774,14.3364266309579,2.6102431518381));
#85311=CARTESIAN_POINT('Ctrl Pts',(-11.2261270538426,14.3426982024485,2.69438294245455));
#85312=CARTESIAN_POINT('Ctrl Pts',(-11.3199836244461,14.3542205076847,2.86171960095103));
#85313=CARTESIAN_POINT('Ctrl Pts',(-11.3563652307633,14.3594728738015,2.94319116259341));
#85314=CARTESIAN_POINT('Ctrl Pts',(-11.3916613937173,14.3656142093642,3.04665519222934));
#85315=CARTESIAN_POINT('Ctrl Pts',(-11.3978057672359,14.3667399744873,3.06596999585366));
#85316=CARTESIAN_POINT('Ctrl Pts',(-11.4056964885964,14.3682693235905,3.0926829342911));
#85317=CARTESIAN_POINT('Ctrl Pts',(-11.4077891700488,14.3686840492858,3.09997566848611));
#85318=CARTESIAN_POINT('Ctrl Pts',(-11.4112223426029,14.3693803230517,3.11230055014877));
#85319=CARTESIAN_POINT('Ctrl Pts',(-11.4125928418872,14.3696628335035,3.11732412187163));
#85320=CARTESIAN_POINT('Ctrl Pts',(-11.4152529747908,14.3702204300546,3.12728389497237));
#85321=CARTESIAN_POINT('Ctrl Pts',(-11.4165436652269,14.3704955467296,3.13221973541871));
#85322=CARTESIAN_POINT('Ctrl Pts',(-11.4196226872878,14.3711632534436,3.14425118461895));
#85323=CARTESIAN_POINT('Ctrl Pts',(-11.4213836741099,14.3715549643808,3.15135369280404));
#85324=CARTESIAN_POINT('Ctrl Pts',(-11.4270978726473,14.3728601218171,3.1751636286099));
#85325=CARTESIAN_POINT('Ctrl Pts',(-11.4308104332278,14.3737659223643,3.1919276983659));
#85326=CARTESIAN_POINT('Ctrl Pts',(-11.4536926321944,14.3797737405633,3.30460989540102));
#85327=CARTESIAN_POINT('Ctrl Pts',(-11.4634999999956,14.3845638431022,3.40217672343184));
#85328=CARTESIAN_POINT('Ctrl Pts',(-11.4635,14.3893209889657,3.49999999993469));
#85329=CARTESIAN_POINT('Origin',(-10.,13.2,3.5));
#85330=CARTESIAN_POINT('',(-11.4635,14.961903098074,3.50000000001399));
#85331=CARTESIAN_POINT('',(-11.4635,14.8882344353249,3.49999999998375));
#85332=CARTESIAN_POINT('',(-11.4635,13.2,3.5));
#85333=CARTESIAN_POINT('',(-11.4634998863947,14.9618714498257,3.49938784807456));
#85334=CARTESIAN_POINT('Ctrl Pts',(-11.4635,14.961903098074,3.50000000001399));
#85335=CARTESIAN_POINT('Ctrl Pts',(-11.4635,14.9618925647885,3.49979609515158));
#85336=CARTESIAN_POINT('Ctrl Pts',(-11.4634999573859,14.961882029762,3.49959218904603));
#85337=CARTESIAN_POINT('Ctrl Pts',(-11.463499872156,14.9618714929895,3.49938828171059));
#85338=CARTESIAN_POINT('Ctrl Pts',(-11.4634998719743,14.9618714705267,3.4993878470109));
#85339=CARTESIAN_POINT('Ctrl Pts',(-11.4634941562415,14.9611653489416,3.48572300442809));
#85340=CARTESIAN_POINT('Ctrl Pts',(-11.463297055919,14.9604517338739,3.47205933875743));
#85341=CARTESIAN_POINT('Ctrl Pts',(-11.462675813711,14.9592958685541,3.45021222867011));
#85342=CARTESIAN_POINT('Ctrl Pts',(-11.462374217243,14.9588594130255,3.44202585900509));
#85343=CARTESIAN_POINT('Ctrl Pts',(-11.4618314016375,14.9582144209366,3.43003024009514));
#85344=CARTESIAN_POINT('Ctrl Pts',(-11.4616439768593,14.9580086649302,3.42621857699805));
#85345=CARTESIAN_POINT('Ctrl Pts',(-11.4612918956356,14.9576492267382,3.41958716663405));
#85346=CARTESIAN_POINT('Ctrl Pts',(-11.4611339795133,14.9574959074667,3.41676706385665));
#85347=CARTESIAN_POINT('Ctrl Pts',(-11.4608126232754,14.9571983649139,3.41131119760458));
#85348=CARTESIAN_POINT('Ctrl Pts',(-11.4606502101068,14.9570541982038,3.408675372308));
#85349=CARTESIAN_POINT('Ctrl Pts',(-11.460311369411,14.9567652687256,3.40340855334878));
#85350=CARTESIAN_POINT('Ctrl Pts',(-11.4601349648237,14.9566205107315,3.40077758585935));
#85351=CARTESIAN_POINT('Ctrl Pts',(-11.4596963723103,14.9562736108224,3.39449083336596));
#85352=CARTESIAN_POINT('Ctrl Pts',(-11.4594275607889,14.9560711072967,3.39083554702266));
#85353=CARTESIAN_POINT('Ctrl Pts',(-11.4584155458281,14.955343182091,3.37774660656628));
#85354=CARTESIAN_POINT('Ctrl Pts',(-11.4575945969423,14.9548136966491,3.36831940949505));
#85355=CARTESIAN_POINT('Ctrl Pts',(-11.4546921843024,14.953115600815,3.33835537049578));
#85356=CARTESIAN_POINT('Ctrl Pts',(-11.4522676952669,14.9519311692878,3.31785501242865));
#85357=CARTESIAN_POINT('Ctrl Pts',(-11.4324365182466,14.94360707134,3.17597209312809));
#85358=CARTESIAN_POINT('Ctrl Pts',(-11.40026788733,14.9360397509419,3.05714430200627));
#85359=CARTESIAN_POINT('Ctrl Pts',(-11.3314871629945,14.9253872985827,2.88977453303682));
#85360=CARTESIAN_POINT('Ctrl Pts',(-11.3061142940837,14.9220330636867,2.83720295945621));
#85361=CARTESIAN_POINT('Ctrl Pts',(-11.2705831372885,14.9179764225479,2.77359664460495));
#85362=CARTESIAN_POINT('Ctrl Pts',(-11.2633089494245,14.9171741070723,2.76101836071715));
#85363=CARTESIAN_POINT('Ctrl Pts',(-11.2524353858916,14.9160144861728,2.74284609249837));
#85364=CARTESIAN_POINT('Ctrl Pts',(-11.2489834406885,14.9156519057848,2.7371652850024));
#85365=CARTESIAN_POINT('Ctrl Pts',(-11.242849486914,14.9150172127121,2.72722400135307));
#85366=CARTESIAN_POINT('Ctrl Pts',(-11.2401839941528,14.9147445055185,2.7229535067101));
#85367=CARTESIAN_POINT('Ctrl Pts',(-11.2346002556836,14.9141795787947,2.71410949211253));
#85368=CARTESIAN_POINT('Ctrl Pts',(-11.2316785034138,14.9138874934652,2.70953826971854));
#85369=CARTESIAN_POINT('Ctrl Pts',(-11.2240540772426,14.913134248671,2.69775440114759));
#85370=CARTESIAN_POINT('Ctrl Pts',(-11.2193130126363,14.9126745140809,2.69056676224568));
#85371=CARTESIAN_POINT('Ctrl Pts',(-11.2001320945518,14.9108482125492,2.662038719991));
#85372=CARTESIAN_POINT('Ctrl Pts',(-11.1851927706987,14.9095003519492,2.64103879399989));
#85373=CARTESIAN_POINT('Ctrl Pts',(-11.097529470527,14.9019754130674,2.52445698764153));
#85374=CARTESIAN_POINT('Ctrl Pts',(-11.0138163647713,14.8962586810473,2.43772302821349));
#85375=CARTESIAN_POINT('Ctrl Pts',(-10.882616825591,14.8879939319066,2.33158776942962));
#85376=CARTESIAN_POINT('Ctrl Pts',(-10.8432890537668,14.8855824008541,2.30289409147578));
#85377=CARTESIAN_POINT('Ctrl Pts',(-10.7894771440365,14.882268982896,2.26760205810116));
#85378=CARTESIAN_POINT('Ctrl Pts',(-10.7762085480918,14.8814508715331,2.25920223126527));
#85379=CARTESIAN_POINT('Ctrl Pts',(-10.7565976213906,14.8802362588672,2.24722498349501));
#85380=CARTESIAN_POINT('Ctrl Pts',(-10.7503593125465,14.8798490938724,2.24347857135356));
#85381=CARTESIAN_POINT('Ctrl Pts',(-10.7404526528811,14.8792325985728,2.23762921635464));
#85382=CARTESIAN_POINT('Ctrl Pts',(-10.736802605289,14.8790051010416,2.23549533550374));
#85383=CARTESIAN_POINT('Ctrl Pts',(-10.7298979823834,14.8785739913863,2.23149881872907));
#85384=CARTESIAN_POINT('Ctrl Pts',(-10.7266453868623,14.8783705889706,2.22963281186522));
#85385=CARTESIAN_POINT('Ctrl Pts',(-10.7209755863483,14.8780154118914,2.22640895870506));
#85386=CARTESIAN_POINT('Ctrl Pts',(-10.7185616064974,14.8778639980089,2.22504543054102));
#85387=CARTESIAN_POINT('Ctrl Pts',(-10.7134640906307,14.8775438308677,2.2221851923121));
#85388=CARTESIAN_POINT('Ctrl Pts',(-10.7107797177237,14.8773749825155,2.22069007512704));
#85389=CARTESIAN_POINT('Ctrl Pts',(-10.7036775305322,14.8769276414606,2.21676361817231));
#85390=CARTESIAN_POINT('Ctrl Pts',(-10.699251864399,14.8766482637709,2.21434666133254));
#85391=CARTESIAN_POINT('Ctrl Pts',(-10.6805588544942,14.8754659157775,2.20426305490482));
#85392=CARTESIAN_POINT('Ctrl Pts',(-10.6661777738268,14.8745506408534,2.19681094465549));
#85393=CARTESIAN_POINT('Ctrl Pts',(-10.5079179185524,14.8644412056483,2.11810658127842));
#85394=CARTESIAN_POINT('Ctrl Pts',(-10.353367839915,14.8543869381076,2.0707500682976));
#85395=CARTESIAN_POINT('Ctrl Pts',(-10.1541503836348,14.8428101526799,2.04408044742302));
#85396=CARTESIAN_POINT('Ctrl Pts',(-10.1139044482114,14.8405295819394,2.04038008045864));
#85397=CARTESIAN_POINT('Ctrl Pts',(-10.0639048801985,14.8377673890358,2.03786397441423));
#85398=CARTESIAN_POINT('Ctrl Pts',(-10.0542510453968,14.8372373001573,2.03747395873035));
#85399=CARTESIAN_POINT('Ctrl Pts',(-10.038939492813,14.836401534841,2.03700718804892));
#85400=CARTESIAN_POINT('Ctrl Pts',(-10.0332840893871,14.8360939178519,2.03686759909809));
#85401=CARTESIAN_POINT('Ctrl Pts',(-10.0226473009366,14.8355173312904,2.03666676194556));
#85402=CARTESIAN_POINT('Ctrl Pts',(-10.0176661497447,14.8352481372942,2.03659815025506));
#85403=CARTESIAN_POINT('Ctrl Pts',(-10.0064704090983,14.8346448923091,2.0365011089357));
#85404=CARTESIAN_POINT('Ctrl Pts',(-10.0002557719555,14.834311284629,2.03648682734015));
#85405=CARTESIAN_POINT('Ctrl Pts',(-9.98440626561432,14.8334635532542,2.03655136123908));
#85406=CARTESIAN_POINT('Ctrl Pts',(-9.97477183965166,14.83295115272,2.03668573823459));
#85407=CARTESIAN_POINT('Ctrl Pts',(-9.91651883599945,14.8298696133236,2.03807372433107));
#85408=CARTESIAN_POINT('Ctrl Pts',(-9.86798379163357,14.827373575416,2.04165508579084));
#85409=CARTESIAN_POINT('Ctrl Pts',(-9.68532041755657,14.8181295829508,2.06432982740108));
#85410=CARTESIAN_POINT('Ctrl Pts',(-9.55391115244006,14.8118460513211,2.0995821566756));
#85411=CARTESIAN_POINT('Ctrl Pts',(-9.40201905512112,14.8034343129593,2.16391449073052));
#85412=CARTESIAN_POINT('Ctrl Pts',(-9.37516234655413,14.801896781624,2.1762615931939));
#85413=CARTESIAN_POINT('Ctrl Pts',(-9.34342490366024,14.7999978699034,2.19203360609857));
#85414=CARTESIAN_POINT('Ctrl Pts',(-9.33816607903672,14.7996804672609,2.1946867029691));
#85415=CARTESIAN_POINT('Ctrl Pts',(-9.33002211141636,14.7991844151925,2.19885723131609));
#85416=CARTESIAN_POINT('Ctrl Pts',(-9.32712572041076,14.7990071023433,2.20035270971994));
#85417=CARTESIAN_POINT('Ctrl Pts',(-9.32176191953072,14.7986770355272,2.20314490947861));
#85418=CARTESIAN_POINT('Ctrl Pts',(-9.31929320483483,14.7985244445488,2.20443901021965));
#85419=CARTESIAN_POINT('Ctrl Pts',(-9.31369845472581,14.7981771027566,2.20739218497442));
#85420=CARTESIAN_POINT('Ctrl Pts',(-9.31057474484624,14.7979820868382,2.20905554281994));
#85421=CARTESIAN_POINT('Ctrl Pts',(-9.30108543529763,14.7973864246472,2.21415281076305));
#85422=CARTESIAN_POINT('Ctrl Pts',(-9.29473933011607,14.7969836176409,2.21762254154762));
#85423=CARTESIAN_POINT('Ctrl Pts',(-9.23588990555423,14.7932085338717,2.25036739460156));
#85424=CARTESIAN_POINT('Ctrl Pts',(-9.18521625643155,14.7896639527778,2.28280163359406));
#85425=CARTESIAN_POINT('Ctrl Pts',(-9.13221996427978,14.7857368314953,2.32151765106432));
#85426=CARTESIAN_POINT('Ctrl Pts',(-9.12777269944645,14.7854054802587,2.32480538938953));
#85427=CARTESIAN_POINT('Ctrl Pts',(-9.03275776395706,14.7782888873674,2.39588371630588));
#85428=CARTESIAN_POINT('Ctrl Pts',(-8.95031998660529,14.7714252403453,2.47393537866975));
#85429=CARTESIAN_POINT('Ctrl Pts',(-8.85512799931429,14.7629320992061,2.58767513568424));
#85430=CARTESIAN_POINT('Ctrl Pts',(-8.83353907418968,14.7609546478014,2.61544487879821));
#85431=CARTESIAN_POINT('Ctrl Pts',(-8.80756116954138,14.7585064027503,2.65146750378906));
#85432=CARTESIAN_POINT('Ctrl Pts',(-8.80222338109642,14.7579993708997,2.65901906190863));
#85433=CARTESIAN_POINT('Ctrl Pts',(-8.79378808640856,14.7571915267414,2.67119601435724));
#85434=CARTESIAN_POINT('Ctrl Pts',(-8.79064483046342,14.7568889892139,2.67578928530601));
#85435=CARTESIAN_POINT('Ctrl Pts',(-8.78472983009452,14.7563167443723,2.68453962333893));
#85436=CARTESIAN_POINT('Ctrl Pts',(-8.78195302762407,14.7560468498355,2.6886931618011));
#85437=CARTESIAN_POINT('Ctrl Pts',(-8.77568902705632,14.7554351020333,2.69816749795127));
#85438=CARTESIAN_POINT('Ctrl Pts',(-8.77221512965469,14.7550937462624,2.7034969970504));
#85439=CARTESIAN_POINT('Ctrl Pts',(-8.76330652822853,14.7542127817259,2.71736095461726));
#85440=CARTESIAN_POINT('Ctrl Pts',(-8.75792532962948,14.7536751391083,2.72592950027572));
#85441=CARTESIAN_POINT('Ctrl Pts',(-8.72212342038124,14.750059002665,2.78427204559509));
#85442=CARTESIAN_POINT('Ctrl Pts',(-8.69461165083842,14.7470877696307,2.83577313663909));
#85443=CARTESIAN_POINT('Ctrl Pts',(-8.63112667196301,14.7395221303334,2.97389023531073));
#85444=CARTESIAN_POINT('Ctrl Pts',(-8.60026970582796,14.7350612777493,3.06255254069402));
#85445=CARTESIAN_POINT('Ctrl Pts',(-8.56538816939235,14.727793208853,3.20571536017011));
#85446=CARTESIAN_POINT('Ctrl Pts',(-8.55556012721204,14.7250943646727,3.25853170470827));
#85447=CARTESIAN_POINT('Ctrl Pts',(-8.54731548323043,14.7217040720922,3.32209950573827));
#85448=CARTESIAN_POINT('Ctrl Pts',(-8.54608535369498,14.7211475789637,3.33244976865544));
#85449=CARTESIAN_POINT('Ctrl Pts',(-8.54452527851898,14.7203638287484,3.3468908354331));
#85450=CARTESIAN_POINT('Ctrl Pts',(-8.54410179740904,14.7201415515894,3.35097146578372));
#85451=CARTESIAN_POINT('Ctrl Pts',(-8.54341121256805,14.7197621457897,3.35790991350719));
#85452=CARTESIAN_POINT('Ctrl Pts',(-8.54313534472277,14.7196055022068,3.36076687021167));
#85453=CARTESIAN_POINT('Ctrl Pts',(-8.54262265748319,14.7193043191511,3.3662447871321));
#85454=CARTESIAN_POINT('Ctrl Pts',(-8.54238450078552,14.7191598593208,3.3688655969126));
#85455=CARTESIAN_POINT('Ctrl Pts',(-8.54177063406256,14.7187750777326,3.37582927838293));
#85456=CARTESIAN_POINT('Ctrl Pts',(-8.54140725941812,14.7185340815292,3.38017317532311));
#85457=CARTESIAN_POINT('Ctrl Pts',(-8.54017657920275,14.717668181767,3.39572099613764));
#85458=CARTESIAN_POINT('Ctrl Pts',(-8.5394189400394,14.7170376001372,3.40693291616243));
#85459=CARTESIAN_POINT('Ctrl Pts',(-8.53387118612173,14.7114194994315,3.50597552797113));
#85460=CARTESIAN_POINT('Ctrl Pts',(-8.53687993494716,14.7061029330103,3.59405664850519));
#85461=CARTESIAN_POINT('Ctrl Pts',(-8.56047688999091,14.6946357609698,3.78304220603267));
#85462=CARTESIAN_POINT('Ctrl Pts',(-8.58383037462774,14.6885362444489,3.8831570149342));
#85463=CARTESIAN_POINT('Ctrl Pts',(-8.62425892384568,14.6816071550057,3.99959809355428));
#85464=CARTESIAN_POINT('Ctrl Pts',(-8.63147184563165,14.6804553979283,4.01903036166328));
#85465=CARTESIAN_POINT('Ctrl Pts',(-8.64190962845576,14.6788970395135,4.04541849489856));
#85466=CARTESIAN_POINT('Ctrl Pts',(-8.64477970049039,14.6784787354355,4.05251129832242));
#85467=CARTESIAN_POINT('Ctrl Pts',(-8.64970087862084,14.6777782311501,4.0644039086174));
#85468=CARTESIAN_POINT('Ctrl Pts',(-8.65172225469562,14.6774950414398,4.06921578663917));
#85469=CARTESIAN_POINT('Ctrl Pts',(-8.6557652324437,14.6769374529482,4.07869770536841));
#85470=CARTESIAN_POINT('Ctrl Pts',(-8.65778553535971,14.6766630153595,4.08336821675354));
#85471=CARTESIAN_POINT('Ctrl Pts',(-8.66228946418074,14.676060286359,4.09363308185138));
#85472=CARTESIAN_POINT('Ctrl Pts',(-8.66478391611111,14.675732366568,4.09922260002691));
#85473=CARTESIAN_POINT('Ctrl Pts',(-8.67366700950775,14.6745848799438,4.11879675816106));
#85474=CARTESIAN_POINT('Ctrl Pts',(-8.68024100620505,14.6737716208157,4.13269649240202));
#85475=CARTESIAN_POINT('Ctrl Pts',(-8.745295869381,14.6660497120382,4.2648173837534));
#85476=CARTESIAN_POINT('Ctrl Pts',(-8.81928232218055,14.6597637678889,4.37472030649176));
#85477=CARTESIAN_POINT('Ctrl Pts',(-8.94071397065072,14.6508331496625,4.51109654883778));
#85478=CARTESIAN_POINT('Ctrl Pts',(-8.97637506673069,14.6483259141703,4.54718405369752));
#85479=CARTESIAN_POINT('Ctrl Pts',(-9.03172376523995,14.6444729715065,4.5976609731145));
#85480=CARTESIAN_POINT('Ctrl Pts',(-9.05001466538014,14.6432051955157,4.6135287185643));
#85481=CARTESIAN_POINT('Ctrl Pts',(-9.0729741613783,14.6416085773171,4.63246907011735));
#85482=CARTESIAN_POINT('Ctrl Pts',(-9.07727873014917,14.6413090137971,4.63597911794853));
#85483=CARTESIAN_POINT('Ctrl Pts',(-9.08408386574832,14.6408348998374,4.64146398850898));
#85484=CARTESIAN_POINT('Ctrl Pts',(-9.08657112509848,14.6406615018767,4.64345533019182));
#85485=CARTESIAN_POINT('Ctrl Pts',(-9.09125463080724,14.6403347450532,4.64717999105758));
#85486=CARTESIAN_POINT('Ctrl Pts',(-9.09344935536209,14.6401815186307,4.64891514315538));
#85487=CARTESIAN_POINT('Ctrl Pts',(-9.09847051712793,14.6398307332045,4.65286153541031));
#85488=CARTESIAN_POINT('Ctrl Pts',(-9.10130011847474,14.6396328916599,4.65506867791382));
#85489=CARTESIAN_POINT('Ctrl Pts',(-9.10882500576555,14.6391064010243,4.66089384338185));
#85490=CARTESIAN_POINT('Ctrl Pts',(-9.11353415460382,14.6387765470279,4.66449374771605));
#85491=CARTESIAN_POINT('Ctrl Pts',(-9.14690316320284,14.6364373787969,4.68968295130505));
#85492=CARTESIAN_POINT('Ctrl Pts',(-9.17632455243358,14.6343657221275,4.71023885503368));
#85493=CARTESIAN_POINT('Ctrl Pts',(-9.21777709636512,14.6314663595144,4.73698856277608));
#85494=CARTESIAN_POINT('Ctrl Pts',(-9.22918519330165,14.6306703442032,4.74412937238147));
#85495=CARTESIAN_POINT('Ctrl Pts',(-9.32786375717238,14.6238106622919,4.8040182128677));
#85496=CARTESIAN_POINT('Ctrl Pts',(-9.42033762718389,14.6175790371933,4.84767379449155));
#85497=CARTESIAN_POINT('Ctrl Pts',(-9.56892749650163,14.6083352996318,4.899672259121));
#85498=CARTESIAN_POINT('Ctrl Pts',(-9.62225897527975,14.6051535840508,4.91499779604537));
#85499=CARTESIAN_POINT('Ctrl Pts',(-9.69013264525586,14.6012810005489,4.93038966265702));
#85500=CARTESIAN_POINT('Ctrl Pts',(-9.70397350472048,14.600500173755,4.93331807301127));
#85501=CARTESIAN_POINT('Ctrl Pts',(-9.72430774509668,14.5993656696688,4.93731321423341));
#85502=CARTESIAN_POINT('Ctrl Pts',(-9.73076903411243,14.5990070340954,4.93853751574538));
#85503=CARTESIAN_POINT('Ctrl Pts',(-9.74218042512871,14.5983768589851,4.94062019757165));
#85504=CARTESIAN_POINT('Ctrl Pts',(-9.74712707289918,14.5981047514563,4.94149671191149));
#85505=CARTESIAN_POINT('Ctrl Pts',(-9.75745562822386,14.5975387741943,4.94327206341733));
#85506=CARTESIAN_POINT('Ctrl Pts',(-9.7628382534342,14.5972450527911,4.94416630911928));
#85507=CARTESIAN_POINT('Ctrl Pts',(-9.77686728426921,14.5964826533297,4.94641648132642));
#85508=CARTESIAN_POINT('Ctrl Pts',(-9.78552114552896,14.5960154674733,4.94772499866229));
#85509=CARTESIAN_POINT('Ctrl Pts',(-9.82081154011209,14.5941224376476,4.95273774277879));
#85510=CARTESIAN_POINT('Ctrl Pts',(-9.84753689645598,14.5927171097038,4.95578520920637));
#85511=CARTESIAN_POINT('Ctrl Pts',(-10.0330484797189,14.5831260044657,4.97177376483858));
#85512=CARTESIAN_POINT('Ctrl Pts',(-10.1929050688574,14.5758260786432,4.95944774436787));
#85513=CARTESIAN_POINT('Ctrl Pts',(-10.3777597628051,14.5661432464801,4.91424628419051));
#85514=CARTESIAN_POINT('Ctrl Pts',(-10.4076557724205,14.5645318296078,4.90592015866132));
#85515=CARTESIAN_POINT('Ctrl Pts',(-10.4429594830149,14.5625502388016,4.89486729993801));
#85516=CARTESIAN_POINT('Ctrl Pts',(-10.4486454937222,14.5622286148242,4.89304885288785));
#85517=CARTESIAN_POINT('Ctrl Pts',(-10.4574351501718,14.5617273783574,4.8901784315798));
#85518=CARTESIAN_POINT('Ctrl Pts',(-10.4605467225262,14.5615491477444,4.88915071327117));
#85519=CARTESIAN_POINT('Ctrl Pts',(-10.4662970800943,14.5612182581444,4.88722998949425));
#85520=CARTESIAN_POINT('Ctrl Pts',(-10.4689367818223,14.5610657691221,4.88633989517037));
#85521=CARTESIAN_POINT('Ctrl Pts',(-10.4749025318789,14.5607198018598,4.88430928569167));
#85522=CARTESIAN_POINT('Ctrl Pts',(-10.4782270037585,14.5605260673192,4.88316432341943));
#85523=CARTESIAN_POINT('Ctrl Pts',(-10.4882689873286,14.5599380892001,4.87966529015015));
#85524=CARTESIAN_POINT('Ctrl Pts',(-10.4949733790469,14.5595417638173,4.87727421622463));
#85525=CARTESIAN_POINT('Ctrl Pts',(-10.5503824953309,14.5562365618224,4.85705612065294));
#85526=CARTESIAN_POINT('Ctrl Pts',(-10.5981211042744,14.5531989649412,4.83670202615643));
#85527=CARTESIAN_POINT('Ctrl Pts',(-10.7190833218266,14.5451739064173,4.77734929979471));
#85528=CARTESIAN_POINT('Ctrl Pts',(-10.7902575079625,14.5401292070343,4.73458328875718));
#85529=CARTESIAN_POINT('Ctrl Pts',(-10.8984476366941,14.5322059267931,4.6563674968305));
#85530=CARTESIAN_POINT('Ctrl Pts',(-10.9379013757492,14.5292514279283,4.62460469095677));
#85531=CARTESIAN_POINT('Ctrl Pts',(-10.9977635808065,14.5246825017653,4.57106564858843));
#85532=CARTESIAN_POINT('Ctrl Pts',(-11.0192878954463,14.5230197356274,4.55060275724091));
#85533=CARTESIAN_POINT('Ctrl Pts',(-11.0463201506024,14.5209038332795,4.52329012630722));
#85534=CARTESIAN_POINT('Ctrl Pts',(-11.0524087671256,14.5204253354726,4.51702720301684));
#85535=CARTESIAN_POINT('Ctrl Pts',(-11.0622065758544,14.5196520797133,4.50676669070671));
#85536=CARTESIAN_POINT('Ctrl Pts',(-11.0659500750907,14.5193558489495,4.5028022825268));
#85537=CARTESIAN_POINT('Ctrl Pts',(-11.0731007537442,14.5187884381013,4.4951443470398));
#85538=CARTESIAN_POINT('Ctrl Pts',(-11.0765112316097,14.5185171195869,4.49145401719912));
#85539=CARTESIAN_POINT('Ctrl Pts',(-11.0842721149211,14.5178980674495,4.48296904516542));
#85540=CARTESIAN_POINT('Ctrl Pts',(-11.0886098646393,14.5175508679945,4.47816293499361));
#85541=CARTESIAN_POINT('Ctrl Pts',(-11.1000503119783,14.5166318433307,4.46531686273832));
#85542=CARTESIAN_POINT('Ctrl Pts',(-11.1070968146649,14.5160623401602,4.45722723815051));
#85543=CARTESIAN_POINT('Ctrl Pts',(-11.170713829191,14.5108867113263,4.3825504771167));
#85544=CARTESIAN_POINT('Ctrl Pts',(-11.2213066435107,14.506535428348,4.31109729997014));
#85545=CARTESIAN_POINT('Ctrl Pts',(-11.3242138073556,14.49653038765,4.1340854782053));
#85546=CARTESIAN_POINT('Ctrl Pts',(-11.3707728072551,14.4909846397861,4.02590946919204));
#85547=CARTESIAN_POINT('Ctrl Pts',(-11.40684118657,14.4842295579097,3.90340756888663));
#85548=CARTESIAN_POINT('Ctrl Pts',(-11.409664275351,14.4836758391506,3.89342903996408));
#85549=CARTESIAN_POINT('Ctrl Pts',(-11.4134536590065,14.4828953613382,3.87947037684506));
#85550=CARTESIAN_POINT('Ctrl Pts',(-11.4145097163728,14.4826735271771,3.87551467950928));
#85551=CARTESIAN_POINT('Ctrl Pts',(-11.4162774447946,14.4822946514273,3.86877998664128));
#85552=CARTESIAN_POINT('Ctrl Pts',(-11.4169975781294,14.4821380916016,3.86600320030713));
#85553=CARTESIAN_POINT('Ctrl Pts',(-11.4183631342146,14.4818368898653,3.86067326567109));
#85554=CARTESIAN_POINT('Ctrl Pts',(-11.4190098353259,14.481692326592,3.85812047147511));
#85555=CARTESIAN_POINT('Ctrl Pts',(-11.4207110255185,14.4813069103332,3.85132821837439));
#85556=CARTESIAN_POINT('Ctrl Pts',(-11.4217534193583,14.4810653788785,3.84708579428408));
#85557=CARTESIAN_POINT('Ctrl Pts',(-11.4254230419094,14.480195650896,3.83185690700463));
#85558=CARTESIAN_POINT('Ctrl Pts',(-11.4279419759509,14.4795617121576,3.82084505990614));
#85559=CARTESIAN_POINT('Ctrl Pts',(-11.4483457461069,14.4741021535261,3.72664341749088));
#85560=CARTESIAN_POINT('Ctrl Pts',(-11.4590698476733,14.4689683731578,3.642075580809));
#85561=CARTESIAN_POINT('Ctrl Pts',(-11.4631290190957,14.4626991343197,3.53804989860196));
#85562=CARTESIAN_POINT('Ctrl Pts',(-11.4634999999255,14.4615539391712,3.51902508777929));
#85563=CARTESIAN_POINT('Ctrl Pts',(-11.4635,14.4604121156607,3.50000000573456));
#85564=CARTESIAN_POINT('',(-11.4634998779574,14.8881996490159,3.4994023223159));
#85565=CARTESIAN_POINT('Ctrl Pts',(-11.4635,14.3893209889657,3.49999999993469));
#85566=CARTESIAN_POINT('Ctrl Pts',(-11.4635,14.389342318194,3.5004386022108));
#85567=CARTESIAN_POINT('Ctrl Pts',(-11.4634998028312,14.3893636472093,3.50087720962041));
#85568=CARTESIAN_POINT('Ctrl Pts',(-11.4634121584128,14.394103948603,3.59835813830859));
#85569=CARTESIAN_POINT('Ctrl Pts',(-11.4536730819326,14.3987763817662,3.69513925308056));
#85570=CARTESIAN_POINT('Ctrl Pts',(-11.4322738321971,14.4044740470969,3.80090277700886));
#85571=CARTESIAN_POINT('Ctrl Pts',(-11.4299955115346,14.4050546072532,3.81155037255397));
#85572=CARTESIAN_POINT('Ctrl Pts',(-11.4266513225759,14.4058735549096,3.82636907495734));
#85573=CARTESIAN_POINT('Ctrl Pts',(-11.4256854829067,14.4061065411713,3.83056265998381));
#85574=CARTESIAN_POINT('Ctrl Pts',(-11.4241015176665,14.4064831443729,3.83730400286495));
#85575=CARTESIAN_POINT('Ctrl Pts',(-11.4234950096157,14.4066261048282,3.83985449878406));
#85576=CARTESIAN_POINT('Ctrl Pts',(-11.4222075191619,14.4069270270035,3.84520475792863));
#85577=CARTESIAN_POINT('Ctrl Pts',(-11.4215251191904,14.4070850717748,3.8480041487153));
#85578=CARTESIAN_POINT('Ctrl Pts',(-11.419838318364,14.407472206315,3.8548361176531));
#85579=CARTESIAN_POINT('Ctrl Pts',(-11.4188250028883,14.4077017985899,3.85886645287101));
#85580=CARTESIAN_POINT('Ctrl Pts',(-11.4151261661451,14.4085292398004,3.87331754375532));
#85581=CARTESIAN_POINT('Ctrl Pts',(-11.4123429586264,14.4091323342623,3.88371266315544));
#85582=CARTESIAN_POINT('Ctrl Pts',(-11.394041990626,14.4129756672591,3.94916762015689));
#85583=CARTESIAN_POINT('Ctrl Pts',(-11.3754229631227,14.4163584040188,4.0033041915881));
#85584=CARTESIAN_POINT('Ctrl Pts',(-11.3269812635271,14.423992657982,4.12120070912478));
#85585=CARTESIAN_POINT('Ctrl Pts',(-11.2956291761927,14.4282537359137,4.18418942620265));
#85586=CARTESIAN_POINT('Ctrl Pts',(-11.2207994271709,14.4369918740804,4.31078836588991));
#85587=CARTESIAN_POINT('Ctrl Pts',(-11.1765794246168,14.4414367664753,4.37372350413566));
#85588=CARTESIAN_POINT('Ctrl Pts',(-11.120844864374,14.4462815274992,4.44109081668099));
#85589=CARTESIAN_POINT('Ctrl Pts',(-11.1139830792076,14.4468666758097,4.449203267402));
#85590=CARTESIAN_POINT('Ctrl Pts',(-11.1028179259459,14.4478010115508,4.46211559070526));
#85591=CARTESIAN_POINT('Ctrl Pts',(-11.0985702194774,14.4481524517087,4.46696290642563));
#85592=CARTESIAN_POINT('Ctrl Pts',(-11.0909558831337,14.4487753865979,4.47553715049023));
#85593=CARTESIAN_POINT('Ctrl Pts',(-11.0876018488371,14.4490473956288,4.47927508403406));
#85594=CARTESIAN_POINT('Ctrl Pts',(-11.0805550178097,14.449613963184,4.487047626402));
#85595=CARTESIAN_POINT('Ctrl Pts',(-11.0768587060985,14.4499083683507,4.49107895321984));
#85596=CARTESIAN_POINT('Ctrl Pts',(-11.0671528554002,14.4506742767163,4.50154608719232));
#85597=CARTESIAN_POINT('Ctrl Pts',(-11.0611076307184,14.4511442625555,4.5079486009497));
#85598=CARTESIAN_POINT('Ctrl Pts',(-11.0339565160482,14.4532245601372,4.53618942178855));
#85599=CARTESIAN_POINT('Ctrl Pts',(-11.0122309001124,14.4548079929299,4.55742298544379));
#85600=CARTESIAN_POINT('Ctrl Pts',(-10.9513225714017,14.4590511195217,4.61335300566082));
#85601=CARTESIAN_POINT('Ctrl Pts',(-10.9109143426204,14.4616573752491,4.64664954367225));
#85602=CARTESIAN_POINT('Ctrl Pts',(-10.8129423107516,14.4676355668168,4.71892428685838));
#85603=CARTESIAN_POINT('Ctrl Pts',(-10.7542167048291,14.4709700364914,4.75610849349001));
#85604=CARTESIAN_POINT('Ctrl Pts',(-10.637943889477,14.4774618487418,4.81862731034578));
#85605=CARTESIAN_POINT('Ctrl Pts',(-10.5809737447922,14.480599439223,4.84470003270051));
#85606=CARTESIAN_POINT('Ctrl Pts',(-10.5157496791872,14.4843246169107,4.86963024443279));
#85607=CARTESIAN_POINT('Ctrl Pts',(-10.5089633353008,14.4847137833371,4.87216655587092));
#85608=CARTESIAN_POINT('Ctrl Pts',(-10.4988314715312,14.4852975254021,4.87586771160278));
#85609=CARTESIAN_POINT('Ctrl Pts',(-10.4954999970626,14.4854899029261,4.8770710036859));
#85610=CARTESIAN_POINT('Ctrl Pts',(-10.4895381110456,14.4858350080482,4.8791999360828));
#85611=CARTESIAN_POINT('Ctrl Pts',(-10.4869093906532,14.4859874631704,4.88013016451039));
#85612=CARTESIAN_POINT('Ctrl Pts',(-10.4812020876988,14.4863191069529,4.88213147902669));
#85613=CARTESIAN_POINT('Ctrl Pts',(-10.4781226231971,14.486498450168,4.88319977996017));
#85614=CARTESIAN_POINT('Ctrl Pts',(-10.4694721152723,14.4870033100668,4.8861683991773));
#85615=CARTESIAN_POINT('Ctrl Pts',(-10.4638932035743,14.4873301454291,4.88804538512558));
#85616=CARTESIAN_POINT('Ctrl Pts',(-10.4303269589742,14.4893033684728,4.8991135510081));
#85617=CARTESIAN_POINT('Ctrl Pts',(-10.402080427348,14.4909919828032,4.90749106858268));
#85618=CARTESIAN_POINT('Ctrl Pts',(-10.2439044071077,14.5005304652491,4.94925399066714));
#85619=CARTESIAN_POINT('Ctrl Pts',(-10.11011020097,14.5088311459879,4.96550634083251));
#85620=CARTESIAN_POINT('Ctrl Pts',(-9.92610919725075,14.5195409137585,4.96248360021393));
#85621=CARTESIAN_POINT('Ctrl Pts',(-9.87632817384542,14.5223770220857,4.95911762376294));
#85622=CARTESIAN_POINT('Ctrl Pts',(-9.81717708968965,14.525671299234,4.95206824098857));
#85623=CARTESIAN_POINT('Ctrl Pts',(-9.8075540342621,14.5262048853686,4.95082423114348));
#85624=CARTESIAN_POINT('Ctrl Pts',(-9.79176722072903,14.5270765139875,4.94862357163731));
#85625=CARTESIAN_POINT('Ctrl Pts',(-9.78559604731992,14.5274163009371,4.9477230706959));
#85626=CARTESIAN_POINT('Ctrl Pts',(-9.77450270460006,14.528025463329,4.94603183570263));
#85627=CARTESIAN_POINT('Ctrl Pts',(-9.7695784877446,14.5282952809169,4.94525535032436));
#85628=CARTESIAN_POINT('Ctrl Pts',(-9.75908595454679,14.528868999375,4.94354582466448));
#85629=CARTESIAN_POINT('Ctrl Pts',(-9.75351886525646,14.5291726726454,4.9426056899389));
#85630=CARTESIAN_POINT('Ctrl Pts',(-9.73849591853881,14.5299902478676,4.93997920795611));
#85631=CARTESIAN_POINT('Ctrl Pts',(-9.72905090307435,14.5305022276834,4.93823193426739));
#85632=CARTESIAN_POINT('Ctrl Pts',(-9.68075406032457,14.5331105805803,4.92880463579633));
#85633=CARTESIAN_POINT('Ctrl Pts',(-9.64220661203632,14.5351597143119,4.9196425286188));
#85634=CARTESIAN_POINT('Ctrl Pts',(-9.46031577036151,14.5447476923221,4.86852919701771));
#85635=CARTESIAN_POINT('Ctrl Pts',(-9.32360851419405,14.5516141937201,4.80637523549079));
#85636=CARTESIAN_POINT('Ctrl Pts',(-9.17648226743139,14.5606161694766,4.71010516029549));
#85637=CARTESIAN_POINT('Ctrl Pts',(-9.15468495970759,14.5620000084049,4.69498044499086));
#85638=CARTESIAN_POINT('Ctrl Pts',(-9.12895134599161,14.5637104750145,4.67606793141302));
#85639=CARTESIAN_POINT('Ctrl Pts',(-9.12460849974417,14.5640018424251,4.67283897292114));
#85640=CARTESIAN_POINT('Ctrl Pts',(-9.11750917138189,14.5644827846558,4.66749913952317));
#85641=CARTESIAN_POINT('Ctrl Pts',(-9.11474207678029,14.5646714087241,4.66540238211958));
#85642=CARTESIAN_POINT('Ctrl Pts',(-9.10976940707364,14.5650125416893,4.6616064278575));
#85643=CARTESIAN_POINT('Ctrl Pts',(-9.10756119813874,14.5651648048303,4.6599107666315));
#85644=CARTESIAN_POINT('Ctrl Pts',(-9.10273451029718,14.565499334031,4.65618245910433));
#85645=CARTESIAN_POINT('Ctrl Pts',(-9.10011812531457,14.5656817770791,4.65414723883737));
#85646=CARTESIAN_POINT('Ctrl Pts',(-9.09267302128851,14.5662040394351,4.64831517295536));
#85647=CARTESIAN_POINT('Ctrl Pts',(-9.08786132198781,14.5665453235079,4.64449683795408));
#85648=CARTESIAN_POINT('Ctrl Pts',(-9.05614154474927,14.5688192997372,4.61899845294539));
#85649=CARTESIAN_POINT('Ctrl Pts',(-9.02998643967149,14.5708101362053,4.59640304686016));
#85650=CARTESIAN_POINT('Ctrl Pts',(-8.93229728227649,14.5786255458622,4.50577606571329));
#85651=CARTESIAN_POINT('Ctrl Pts',(-8.86691415133092,14.5846662181041,4.431499639084));
#85652=CARTESIAN_POINT('Ctrl Pts',(-8.76419674668663,14.5951667291323,4.28783929512394));
#85653=CARTESIAN_POINT('Ctrl Pts',(-8.72401580447861,14.5996789223421,4.22094922021483));
#85654=CARTESIAN_POINT('Ctrl Pts',(-8.68461007668905,14.6045865336568,4.14163458794331));
#85655=CARTESIAN_POINT('Ctrl Pts',(-8.67997718897416,14.6051728912806,4.13204855951779));
#85656=CARTESIAN_POINT('Ctrl Pts',(-8.67270556135671,14.6061087742783,4.11657387403076));
#85657=CARTESIAN_POINT('Ctrl Pts',(-8.67000050096529,14.6064605643365,4.11071695851973));
#85658=CARTESIAN_POINT('Ctrl Pts',(-8.66525833512971,14.6070838970414,4.10026841300552));
#85659=CARTESIAN_POINT('Ctrl Pts',(-8.66320598738009,14.6073559562996,4.09568384927746));
#85660=CARTESIAN_POINT('Ctrl Pts',(-8.65896955319943,14.6079224076401,4.08608827804928));
#85661=CARTESIAN_POINT('Ctrl Pts',(-8.65678985375869,14.6082166477332,4.0810754108215));
#85662=CARTESIAN_POINT('Ctrl Pts',(-8.65117797699607,14.6089816451301,4.06796891145177));
#85663=CARTESIAN_POINT('Ctrl Pts',(-8.64779052234515,14.6094508918143,4.05985629156161));
#85664=CARTESIAN_POINT('Ctrl Pts',(-8.63307985704552,14.6115231092877,4.02371315852638));
#85665=CARTESIAN_POINT('Ctrl Pts',(-8.62255324408652,14.6130994633753,3.99536527170792));
#85666=CARTESIAN_POINT('Ctrl Pts',(-8.59633988427138,14.6173180459498,3.91745774302727));
#85667=CARTESIAN_POINT('Ctrl Pts',(-8.58240226533197,14.6199076461924,3.86735528846226));
#85668=CARTESIAN_POINT('Ctrl Pts',(-8.54827221938631,14.6276564855475,3.71333093641444));
#85669=CARTESIAN_POINT('Ctrl Pts',(-8.53665383458155,14.6326599237121,3.60787967298341));
#85670=CARTESIAN_POINT('Ctrl Pts',(-8.5364603238373,14.6395172610135,3.47350180698756));
#85671=CARTESIAN_POINT('Ctrl Pts',(-8.53725783843772,14.6410057726106,3.44490287714756));
#85672=CARTESIAN_POINT('Ctrl Pts',(-8.53920929031795,14.6428334658408,3.41081799661619));
#85673=CARTESIAN_POINT('Ctrl Pts',(-8.53955726092556,14.6431315613034,3.40529027951902));
#85674=CARTESIAN_POINT('Ctrl Pts',(-8.54017703797334,14.6436213635055,3.39626237895485));
#85675=CARTESIAN_POINT('Ctrl Pts',(-8.54043007975871,14.643812058964,3.39276091252988));
#85676=CARTESIAN_POINT('Ctrl Pts',(-8.54090654845293,14.6441553686145,3.38648210185648));
#85677=CARTESIAN_POINT('Ctrl Pts',(-8.5411253105693,14.6443077222738,3.3837044544901));
#85678=CARTESIAN_POINT('Ctrl Pts',(-8.54161914373234,14.6446405906303,3.37765496188581));
#85679=CARTESIAN_POINT('Ctrl Pts',(-8.54189728981065,14.6448212696088,3.37438345498683));
#85680=CARTESIAN_POINT('Ctrl Pts',(-8.54271451798922,14.6453336015689,3.36513996407526));
#85681=CARTESIAN_POINT('Ctrl Pts',(-8.54327929111791,14.6456666350909,3.35917038967585));
#85682=CARTESIAN_POINT('Ctrl Pts',(-8.5470416019305,14.6477614652763,3.32185061091354));
#85683=CARTESIAN_POINT('Ctrl Pts',(-8.55121413370243,14.6495716108706,3.29060913552611));
#85684=CARTESIAN_POINT('Ctrl Pts',(-8.58450789119584,14.6614149673323,3.09073812546877));
#85685=CARTESIAN_POINT('Ctrl Pts',(-8.64200738318631,14.6720532122382,2.92816398274606));
#85686=CARTESIAN_POINT('Ctrl Pts',(-8.73496465313359,14.6826184803685,2.76391215063134));
#85687=CARTESIAN_POINT('Ctrl Pts',(-8.74387545889991,14.6835905392957,2.74880699841342));
#85688=CARTESIAN_POINT('Ctrl Pts',(-8.75691862071611,14.6849577868378,2.72757823647388));
#85689=CARTESIAN_POINT('Ctrl Pts',(-8.76082891077137,14.6853609614944,2.72132053404061));
#85690=CARTESIAN_POINT('Ctrl Pts',(-8.76727969667483,14.6860153229084,2.71116889282431));
#85691=CARTESIAN_POINT('Ctrl Pts',(-8.76979168302489,14.6862675491686,2.70725706599327));
#85692=CARTESIAN_POINT('Ctrl Pts',(-8.77510744121103,14.6867959317582,2.6990651408183));
#85693=CARTESIAN_POINT('Ctrl Pts',(-8.777915109139,14.6870719393491,2.69478763690839));
#85694=CARTESIAN_POINT('Ctrl Pts',(-8.78468621927589,14.687730325603,2.68458879476031));
#85695=CARTESIAN_POINT('Ctrl Pts',(-8.78867060660366,14.6881119180431,2.67868147325002));
#85696=CARTESIAN_POINT('Ctrl Pts',(-8.80246001185854,14.6894130192345,2.65855569364177));
#85697=CARTESIAN_POINT('Ctrl Pts',(-8.81247369874298,14.6903246759255,2.64448152507192));
#85698=CARTESIAN_POINT('Ctrl Pts',(-8.83710747201905,14.6924921958117,2.61112510054536));
#85699=CARTESIAN_POINT('Ctrl Pts',(-8.85196134733785,14.693739186876,2.59202150273576));
#85700=CARTESIAN_POINT('Ctrl Pts',(-8.91167032814787,14.6985404741856,2.51903889311095));
#85701=CARTESIAN_POINT('Ctrl Pts',(-8.95990081226546,14.7019723429171,2.46804033037075));
#85702=CARTESIAN_POINT('Ctrl Pts',(-9.08653934581786,14.7103271899521,2.35206849377786));
#85703=CARTESIAN_POINT('Ctrl Pts',(-9.16840958621896,14.7151992592941,2.29144334789854));
#85704=CARTESIAN_POINT('Ctrl Pts',(-9.2650789484952,14.7211301026905,2.23436287598538));
#85705=CARTESIAN_POINT('Ctrl Pts',(-9.27433305141891,14.7216996731456,2.22903432455242));
#85706=CARTESIAN_POINT('Ctrl Pts',(-9.28736587405346,14.722505504595,2.22171870624835));
#85707=CARTESIAN_POINT('Ctrl Pts',(-9.29109645596594,14.7227365883625,2.21964605372261));
#85708=CARTESIAN_POINT('Ctrl Pts',(-9.29712740604751,14.7231109231526,2.21632979127867));
#85709=CARTESIAN_POINT('Ctrl Pts',(-9.29942216390929,14.7232535326876,2.21507596199455));
#85710=CARTESIAN_POINT('Ctrl Pts',(-9.30425847568518,14.7235544853693,2.21245026390786));
#85711=CARTESIAN_POINT('Ctrl Pts',(-9.30680073996476,14.7237129157286,2.21107976312565));
#85712=CARTESIAN_POINT('Ctrl Pts',(-9.31304096385428,14.7241023321206,2.20773954346345));
#85713=CARTESIAN_POINT('Ctrl Pts',(-9.31674334226656,14.724333834119,2.20577817062005));
#85714=CARTESIAN_POINT('Ctrl Pts',(-9.33018360487602,14.7251757378988,2.19873179903315));
#85715=CARTESIAN_POINT('Ctrl Pts',(-9.3399699972636,14.725791624287,2.19374071688748));
#85716=CARTESIAN_POINT('Ctrl Pts',(-9.40323453775983,14.7297868550527,2.16236809436687));
#85717=CARTESIAN_POINT('Ctrl Pts',(-9.45822239713232,14.7333203086661,2.13916794981007));
#85718=CARTESIAN_POINT('Ctrl Pts',(-9.57533236702496,14.7407639914435,2.0979826844455));
#85719=CARTESIAN_POINT('Ctrl Pts',(-9.637549589396,14.7446721582833,2.08062505308544));
#85720=CARTESIAN_POINT('Ctrl Pts',(-9.7787372410444,14.7532570106408,2.05112833336713));
#85721=CARTESIAN_POINT('Ctrl Pts',(-9.85797479411013,14.7578795224073,2.04122710117559));
#85722=CARTESIAN_POINT('Ctrl Pts',(-9.9483013197222,14.7628896489768,2.03737445817805));
#85723=CARTESIAN_POINT('Ctrl Pts',(-9.95897257273528,14.7634776719302,2.03703623153573));
#85724=CARTESIAN_POINT('Ctrl Pts',(-9.97610540086514,14.7644156886124,2.03668081748006));
#85725=CARTESIAN_POINT('Ctrl Pts',(-9.98256491375617,14.7647679634693,2.03658959910783));
#85726=CARTESIAN_POINT('Ctrl Pts',(-9.99404893751969,14.7653918519988,2.03650347547258));
#85727=CARTESIAN_POINT('Ctrl Pts',(-9.99907318599637,14.7656639854529,2.03649166919401));
#85728=CARTESIAN_POINT('Ctrl Pts',(-10.0095594164535,14.7662302908705,2.03652102817245));
#85729=CARTESIAN_POINT('Ctrl Pts',(-10.015021314684,14.7665243127017,2.03656689779099));
#85730=CARTESIAN_POINT('Ctrl Pts',(-10.0292542554504,14.7672880893945,2.03676611895257));
#85731=CARTESIAN_POINT('Ctrl Pts',(-10.0380244745551,14.7677563427297,2.03696775635065));
#85732=CARTESIAN_POINT('Ctrl Pts',(-10.0768206162417,14.7698177023062,2.0382088198072));
#85733=CARTESIAN_POINT('Ctrl Pts',(-10.1068132628365,14.7713845428022,2.04009385450433));
#85734=CARTESIAN_POINT('Ctrl Pts',(-10.1879956941611,14.7755702437649,2.04771167493886));
#85735=CARTESIAN_POINT('Ctrl Pts',(-10.2389760149104,14.7781375505845,2.05522501010984));
#85736=CARTESIAN_POINT('Ctrl Pts',(-10.3938242997306,14.7858996734032,2.08646871710028));
#85737=CARTESIAN_POINT('Ctrl Pts',(-10.4955722327321,14.7909329752407,2.11885092764405));
#85738=CARTESIAN_POINT('Ctrl Pts',(-10.6190668988083,14.7978257449656,2.17357334855364));
#85739=CARTESIAN_POINT('Ctrl Pts',(-10.6448877105855,14.7993150899003,2.18593336794324));
#85740=CARTESIAN_POINT('Ctrl Pts',(-10.67525222424,14.8011437163814,2.20157889277397));
#85741=CARTESIAN_POINT('Ctrl Pts',(-10.6801621210611,14.8014418635582,2.2041441341138));
#85742=CARTESIAN_POINT('Ctrl Pts',(-10.6881597827738,14.8019317339091,2.20838059400114));
#85743=CARTESIAN_POINT('Ctrl Pts',(-10.6912563513537,14.8021224453322,2.21003518157764));
#85744=CARTESIAN_POINT('Ctrl Pts',(-10.6966618203515,14.8024572339183,2.21294853500151));
#85745=CARTESIAN_POINT('Ctrl Pts',(-10.6989733159429,14.8026010018738,2.21420239968839));
#85746=CARTESIAN_POINT('Ctrl Pts',(-10.701290635301,14.802745745833,2.21546751892041));
#85747=CARTESIAN_POINT('Ctrl Pts',(-10.7012998170609,14.802746319352,2.2154725317457));
#85748=CARTESIAN_POINT('Ctrl Pts',(-10.7013179991876,14.8027474550787,2.21548245861698));
#85749=CARTESIAN_POINT('Ctrl Pts',(-10.7013269995107,14.8027480172833,2.21548737263408));
#85750=CARTESIAN_POINT('Ctrl Pts',(-10.7013442395075,14.8027490941964,2.21549678560237));
#85751=CARTESIAN_POINT('Ctrl Pts',(-10.7013524792389,14.8027496089069,2.21550128456522));
#85752=CARTESIAN_POINT('Ctrl Pts',(-10.7013689210014,14.8027506359884,2.2155102621116));
#85753=CARTESIAN_POINT('Ctrl Pts',(-10.7013771231267,14.8027511483653,2.2155147407456));
#85754=CARTESIAN_POINT('Ctrl Pts',(-10.7013934902058,14.8027521708122,2.21552367792028));
#85755=CARTESIAN_POINT('Ctrl Pts',(-10.7014016550708,14.8027526808767,2.21552813641152));
#85756=CARTESIAN_POINT('Ctrl Pts',(-10.7014179476104,14.8027536986975,2.21553703328753));
#85757=CARTESIAN_POINT('Ctrl Pts',(-10.7014260753742,14.8027542064594,2.21554147172013));
#85758=CARTESIAN_POINT('Ctrl Pts',(-10.7014422938674,14.8027552196846,2.21555032856131));
#85759=CARTESIAN_POINT('Ctrl Pts',(-10.701450384669,14.8027557251524,2.21555474700838));
#85760=CARTESIAN_POINT('Ctrl Pts',(-10.701466529898,14.8027567338304,2.21556356423642));
#85761=CARTESIAN_POINT('Ctrl Pts',(-10.701474584129,14.8027572370283,2.21556796290921));
#85762=CARTESIAN_POINT('Ctrl Pts',(-10.7014906560814,14.8027582411579,2.21557674051193));
#85763=CARTESIAN_POINT('Ctrl Pts',(-10.7014986738488,14.8027587420924,2.21558111946614));
#85764=CARTESIAN_POINT('Ctrl Pts',(-10.70151467328,14.8027597417204,2.21558985785088));
#85765=CARTESIAN_POINT('Ctrl Pts',(-10.7015226548932,14.8027602404107,2.21559421725288));
#85766=CARTESIAN_POINT('Ctrl Pts',(-10.7043322685578,14.8029357873097,2.21712880762796));
#85767=CARTESIAN_POINT('Ctrl Pts',(-10.707128858977,14.8031114175166,2.2186681861633));
#85768=CARTESIAN_POINT('Ctrl Pts',(-10.7148740617645,14.8036002729374,2.22296459877992));
#85769=CARTESIAN_POINT('Ctrl Pts',(-10.7198116819565,14.8039147013131,2.22574120347394));
#85770=CARTESIAN_POINT('Ctrl Pts',(-10.7308711094175,14.8046250161681,2.23204511538023));
#85771=CARTESIAN_POINT('Ctrl Pts',(-10.7369837093925,14.8050218117944,2.23558820939854));
#85772=CARTESIAN_POINT('Ctrl Pts',(-10.7560473149775,14.8062719456654,2.24682339508197));
#85773=CARTESIAN_POINT('Ctrl Pts',(-10.7689050272972,14.8071335218242,2.25467105880305));
#85774=CARTESIAN_POINT('Ctrl Pts',(-10.820134098984,14.8106340253724,2.28703437677541));
#85775=CARTESIAN_POINT('Ctrl Pts',(-10.8574712183705,14.8133399085539,2.31313516009308));
#85776=CARTESIAN_POINT('Ctrl Pts',(-10.9439649612743,14.8198886711239,2.37981340534427));
#85777=CARTESIAN_POINT('Ctrl Pts',(-10.9918112571779,14.8237457275513,2.42194682535507));
#85778=CARTESIAN_POINT('Ctrl Pts',(-11.0935244932582,14.8323265126232,2.52403663086385));
#85779=CARTESIAN_POINT('Ctrl Pts',(-11.1455012830883,14.8369923758831,2.58559832503061));
#85780=CARTESIAN_POINT('Ctrl Pts',(-11.1983594793626,14.8420425957085,2.6598327609473));
#85781=CARTESIAN_POINT('Ctrl Pts',(-11.2044620066647,14.8426311485935,2.66860495889492));
#85782=CARTESIAN_POINT('Ctrl Pts',(-11.2141004248147,14.843569844042,2.68278878118939));
#85783=CARTESIAN_POINT('Ctrl Pts',(-11.2176974137151,14.8439222729796,2.6881582492922));
#85784=CARTESIAN_POINT('Ctrl Pts',(-11.2240275146196,14.8445463381623,2.6977443425));
#85785=CARTESIAN_POINT('Ctrl Pts',(-11.2267746837641,14.8448184951978,2.70195152234554));
#85786=CARTESIAN_POINT('Ctrl Pts',(-11.2324621204086,14.8453847544427,2.71076037176514));
#85787=CARTESIAN_POINT('Ctrl Pts',(-11.2353984131859,14.8456787071084,2.71536452359918));
#85788=CARTESIAN_POINT('Ctrl Pts',(-11.2429811246269,14.8464420973229,2.72740241976261));
#85789=CARTESIAN_POINT('Ctrl Pts',(-11.2475866815155,14.8469100362181,2.73486172898027));
#85790=CARTESIAN_POINT('Ctrl Pts',(-11.2676476485209,14.8489679732402,2.76801587532363));
#85791=CARTESIAN_POINT('Ctrl Pts',(-11.282378854405,14.8505318156998,2.79414168728199));
#85792=CARTESIAN_POINT('Ctrl Pts',(-11.3201296659054,14.8547071820405,2.86618128859346));
#85793=CARTESIAN_POINT('Ctrl Pts',(-11.3415529291829,14.8572674871752,2.91288435927259));
#85794=CARTESIAN_POINT('Ctrl Pts',(-11.3975992591731,14.8647407067194,3.05424982825733));
#85795=CARTESIAN_POINT('Ctrl Pts',(-11.4249527831082,14.869514882211,3.15145474985847));
#85796=CARTESIAN_POINT('Ctrl Pts',(-11.4456619666599,14.8756690960264,3.2712449825051));
#85797=CARTESIAN_POINT('Ctrl Pts',(-11.4487754533726,14.8767390071556,3.29187264875632));
#85798=CARTESIAN_POINT('Ctrl Pts',(-11.4534716577475,14.878653668477,3.32823763046049));
#85799=CARTESIAN_POINT('Ctrl Pts',(-11.4552421594919,14.8794901011025,3.34394748275528));
#85800=CARTESIAN_POINT('Ctrl Pts',(-11.4572368589926,14.8806084314415,3.36465615721395));
#85801=CARTESIAN_POINT('Ctrl Pts',(-11.4576904684699,14.880878356399,3.36963238265516));
#85802=CARTESIAN_POINT('Ctrl Pts',(-11.4583810221683,14.881316004209,3.37766265046703));
#85803=CARTESIAN_POINT('Ctrl Pts',(-11.4586338812994,14.8814828548404,3.380715328387));
#85804=CARTESIAN_POINT('Ctrl Pts',(-11.459089437443,14.8817963158792,3.38643324368223));
#85805=CARTESIAN_POINT('Ctrl Pts',(-11.4592944182874,14.8819427981857,3.38909826453622));
#85806=CARTESIAN_POINT('Ctrl Pts',(-11.4596981435806,14.8822427915594,3.39454222776246));
#85807=CARTESIAN_POINT('Ctrl Pts',(-11.4598962559606,14.8823963365641,3.39732121121951));
#85808=CARTESIAN_POINT('Ctrl Pts',(-11.4603396224605,14.8827552963578,3.40380127201299));
#85809=CARTESIAN_POINT('Ctrl Pts',(-11.4605787425555,14.8829610378778,3.40750273309786));
#85810=CARTESIAN_POINT('Ctrl Pts',(-11.4614403784447,14.8837515254349,3.42167787003378));
#85811=CARTESIAN_POINT('Ctrl Pts',(-11.4619643106131,14.8843412870754,3.43215696343751));
#85812=CARTESIAN_POINT('Ctrl Pts',(-11.4631173255255,14.8860090843852,3.46155296687572));
#85813=CARTESIAN_POINT('Ctrl Pts',(-11.4634921491228,14.887098285449,3.48047715784938));
#85814=CARTESIAN_POINT('Ctrl Pts',(-11.4634998779574,14.8881996490159,3.4994023223159));
#85815=CARTESIAN_POINT('Ctrl Pts',(-11.4634998771631,14.8881995360101,3.49940038049047));
#85816=CARTESIAN_POINT('Ctrl Pts',(-11.4634999590548,14.8882111678261,3.49960025472328));
#85817=CARTESIAN_POINT('Ctrl Pts',(-11.4635,14.8882228009326,3.49980012789184));
#85818=CARTESIAN_POINT('Ctrl Pts',(-11.4635,14.8882344353249,3.49999999998375));
#85819=CARTESIAN_POINT('Origin',(-10.,13.2,3.5));
#85820=CARTESIAN_POINT('',(-11.4635,15.4596442608852,3.50000000000481));
#85821=CARTESIAN_POINT('',(-11.4635,15.3905155741067,3.49999999999573));
#85822=CARTESIAN_POINT('',(-11.4635,13.2,3.5));
#85823=CARTESIAN_POINT('Ctrl Pts',(-11.4635,15.4596442608852,3.50000000000481));
#85824=CARTESIAN_POINT('Ctrl Pts',(-11.4635,15.4596305239997,3.49972896597656));
#85825=CARTESIAN_POINT('Ctrl Pts',(-11.4634999247368,15.4596167888801,3.49945793106095));
#85826=CARTESIAN_POINT('Ctrl Pts',(-11.4634551756689,15.4555356919543,3.41891492979269));
#85827=CARTESIAN_POINT('Ctrl Pts',(-11.4568063299427,15.4516448954757,3.33877945007402));
#85828=CARTESIAN_POINT('Ctrl Pts',(-11.429541796671,15.4435734829384,3.1750591932718));
#85829=CARTESIAN_POINT('Ctrl Pts',(-11.4080682176578,15.4394039263173,3.09193536609401));
#85830=CARTESIAN_POINT('Ctrl Pts',(-11.37568177232,15.434289074522,3.00054101620579));
#85831=CARTESIAN_POINT('Ctrl Pts',(-11.3717894747857,15.4336877512384,2.98994780994598));
#85832=CARTESIAN_POINT('Ctrl Pts',(-11.3662217651065,15.4328442173318,2.97531970819412));
#85833=CARTESIAN_POINT('Ctrl Pts',(-11.3646501139149,15.4326078451764,2.97124543911044));
#85834=CARTESIAN_POINT('Ctrl Pts',(-11.3621016207484,15.4322272241544,2.96472590376175));
#85835=CARTESIAN_POINT('Ctrl Pts',(-11.3611363604048,15.4320836588598,2.9622761010461));
#85836=CARTESIAN_POINT('Ctrl Pts',(-11.3591055783895,15.4317828303336,2.9571625401835));
#85837=CARTESIAN_POINT('Ctrl Pts',(-11.3580388329525,15.4316254914923,2.95449930457078));
#85838=CARTESIAN_POINT('Ctrl Pts',(-11.3554301908,15.4312424058033,2.94804164728486));
#85839=CARTESIAN_POINT('Ctrl Pts',(-11.3538801878438,15.4310161798071,2.94425054080497));
#85840=CARTESIAN_POINT('Ctrl Pts',(-11.3483458887013,15.4302134501606,2.93087492388027));
#85841=CARTESIAN_POINT('Ctrl Pts',(-11.3442756572806,15.4296320953399,2.92132657522915));
#85842=CARTESIAN_POINT('Ctrl Pts',(-11.3187058276955,15.4260374273143,2.86306823339446));
#85843=CARTESIAN_POINT('Ctrl Pts',(-11.2946644573736,15.4228997181584,2.81552205115584));
#85844=CARTESIAN_POINT('Ctrl Pts',(-11.2192978538469,15.4138764482001,2.68471034206742));
#85845=CARTESIAN_POINT('Ctrl Pts',(-11.1621408427373,15.4079255343839,2.60511683750367));
#85846=CARTESIAN_POINT('Ctrl Pts',(-11.0851725098982,15.4011224105358,2.51787034808266));
#85847=CARTESIAN_POINT('Ctrl Pts',(-11.0726058361066,15.4000433637595,2.50416126398622));
#85848=CARTESIAN_POINT('Ctrl Pts',(-11.033286241938,15.396764042071,2.46287527300432));
#85849=CARTESIAN_POINT('Ctrl Pts',(-11.0057048751487,15.3945963352812,2.43610797192771));
#85850=CARTESIAN_POINT('Ctrl Pts',(-10.9697798968078,15.3919322525683,2.40389056994274));
#85851=CARTESIAN_POINT('Ctrl Pts',(-10.9623936073968,15.3913924841453,2.39739967259808));
#85852=CARTESIAN_POINT('Ctrl Pts',(-10.9505835215266,15.3905418282193,2.38723034516482));
#85853=CARTESIAN_POINT('Ctrl Pts',(-10.9462025773107,15.3902289291237,2.38350278991417));
#85854=CARTESIAN_POINT('Ctrl Pts',(-10.9379937718405,15.3896475099769,2.37660129152837));
#85855=CARTESIAN_POINT('Ctrl Pts',(-10.9341715026429,15.3893787281474,2.37342085111512));
#85856=CARTESIAN_POINT('Ctrl Pts',(-10.925636172017,15.3887827925637,2.36639206592505));
#85857=CARTESIAN_POINT('Ctrl Pts',(-10.9209151557293,15.3884560341586,2.36255349636957));
#85858=CARTESIAN_POINT('Ctrl Pts',(-10.9070813967356,15.387506751398,2.35144811435346));
#85859=CARTESIAN_POINT('Ctrl Pts',(-10.89790550092,15.3868873677109,2.34426048947077));
#85860=CARTESIAN_POINT('Ctrl Pts',(-10.8132001998544,15.3812600682219,2.27952725110197));
#85861=CARTESIAN_POINT('Ctrl Pts',(-10.7323215298924,15.3765576184053,2.22934803547161));
#85862=CARTESIAN_POINT('Ctrl Pts',(-10.5479634960048,15.3665388088277,2.13845841619453));
#85863=CARTESIAN_POINT('Ctrl Pts',(-10.4435765171853,15.3612785158233,2.100967244196));
#85864=CARTESIAN_POINT('Ctrl Pts',(-10.3263507817662,15.3549030713687,2.07331666067449));
#85865=CARTESIAN_POINT('Ctrl Pts',(-10.3166964270464,15.3543745127806,2.07114257325522));
#85866=CARTESIAN_POINT('Ctrl Pts',(-10.3033768970087,15.353639578052,2.06828473521485));
#85867=CARTESIAN_POINT('Ctrl Pts',(-10.2997298299482,15.3534377554188,2.06751678213002));
#85868=CARTESIAN_POINT('Ctrl Pts',(-10.2934814295339,15.3530909135124,2.06622597988029));
#85869=CARTESIAN_POINT('Ctrl Pts',(-10.2908815155282,15.3529462798142,2.06569625464344));
#85870=CARTESIAN_POINT('Ctrl Pts',(-10.2854832094401,15.3526452905358,2.06461164625534));
#85871=CARTESIAN_POINT('Ctrl Pts',(-10.2826846335496,15.3524888706417,2.06405787498233));
#85872=CARTESIAN_POINT('Ctrl Pts',(-10.2759485397135,15.35211148098,2.06274541807741));
#85873=CARTESIAN_POINT('Ctrl Pts',(-10.2720094993891,15.3518900654938,2.06199472835211));
#85874=CARTESIAN_POINT('Ctrl Pts',(-10.2583896584571,15.3511220838221,2.05945706557036));
#85875=CARTESIAN_POINT('Ctrl Pts',(-10.2486941629726,15.3505711954585,2.05775162885507));
#85876=CARTESIAN_POINT('Ctrl Pts',(-10.1916598651684,15.347308968388,2.04831149121491));
#85877=CARTESIAN_POINT('Ctrl Pts',(-10.1439846718586,15.344495683007,2.04281070402325));
#85878=CARTESIAN_POINT('Ctrl Pts',(-10.0323325874114,15.3378307286899,2.03546095386668));
#85879=CARTESIAN_POINT('Ctrl Pts',(-9.9683288415689,15.3339543821337,2.03544649937339));
#85880=CARTESIAN_POINT('Ctrl Pts',(-9.87845763787296,15.3285593939951,2.04132171322294));
#85881=CARTESIAN_POINT('Ctrl Pts',(-9.85243560626152,15.3270024443801,2.04372402732658));
#85882=CARTESIAN_POINT('Ctrl Pts',(-9.75910427968921,15.3214500859481,2.05486774481952));
#85883=CARTESIAN_POINT('Ctrl Pts',(-9.69235238273318,15.3175439678568,2.06759190439752));
#85884=CARTESIAN_POINT('Ctrl Pts',(-9.61665193514905,15.313207843049,2.08756066769791));
#85885=CARTESIAN_POINT('Ctrl Pts',(-9.60661523569978,15.3126347443779,2.09032307199516));
#85886=CARTESIAN_POINT('Ctrl Pts',(-9.59040907124544,15.3117121451861,2.09497006566845));
#85887=CARTESIAN_POINT('Ctrl Pts',(-9.5842212169069,15.3113605369858,2.09678873626285));
#85888=CARTESIAN_POINT('Ctrl Pts',(-9.5732514801817,15.3107383317008,2.10009178253024));
#85889=CARTESIAN_POINT('Ctrl Pts',(-9.56846484210033,15.3104672135685,2.10155989585975));
#85890=CARTESIAN_POINT('Ctrl Pts',(-9.55841883704447,15.309898968704,2.10469760499573));
#85891=CARTESIAN_POINT('Ctrl Pts',(-9.55316118094456,15.3096020172258,2.10637244289861));
#85892=CARTESIAN_POINT('Ctrl Pts',(-9.53932394352627,15.3088215991895,2.11086668152395));
#85893=CARTESIAN_POINT('Ctrl Pts',(-9.53076069456945,15.308339760734,2.11373585321252));
#85894=CARTESIAN_POINT('Ctrl Pts',(-9.49128545836975,15.3061232001782,2.12736998012011));
#85895=CARTESIAN_POINT('Ctrl Pts',(-9.46071237375714,15.3044200112537,2.13909121415465));
#85896=CARTESIAN_POINT('Ctrl Pts',(-9.37662266987157,15.299749904531,2.17460920139484));
#85897=CARTESIAN_POINT('Ctrl Pts',(-9.32410197594008,15.2968518055122,2.20060682245706));
#85898=CARTESIAN_POINT('Ctrl Pts',(-9.20092772125547,15.2899143146875,2.27107227533048));
#85899=CARTESIAN_POINT('Ctrl Pts',(-9.13225019822145,15.2859278471301,2.31856495182274));
#85900=CARTESIAN_POINT('Ctrl Pts',(-9.03683473424141,15.2797146079092,2.39737676550485));
#85901=CARTESIAN_POINT('Ctrl Pts',(-9.00675942091175,15.2776402540572,2.4243895072629));
#85902=CARTESIAN_POINT('Ctrl Pts',(-8.97348035787536,15.2751558438626,2.45686681993499));
#85903=CARTESIAN_POINT('Ctrl Pts',(-8.96914456549895,15.2748282671382,2.46115136925395));
#85904=CARTESIAN_POINT('Ctrl Pts',(-8.9622641443726,15.2743019371378,2.46803596080709));
#85905=CARTESIAN_POINT('Ctrl Pts',(-8.95970217885161,15.2741044955695,2.47061866785246));
#85906=CARTESIAN_POINT('Ctrl Pts',(-8.9551826617476,15.2737535400496,2.47520887897217));
#85907=CARTESIAN_POINT('Ctrl Pts',(-8.95322121749009,15.2736003325114,2.47721248910089));
#85908=CARTESIAN_POINT('Ctrl Pts',(-8.94906370896963,15.2732736631797,2.48148386010979));
#85909=CARTESIAN_POINT('Ctrl Pts',(-8.94686925549387,15.273100089598,2.48375305677801));
#85910=CARTESIAN_POINT('Ctrl Pts',(-8.94092642347853,15.2726269485331,2.48993822228083));
#85911=CARTESIAN_POINT('Ctrl Pts',(-8.93719247159222,15.2723263103039,2.4938679058073));
#85912=CARTESIAN_POINT('Ctrl Pts',(-8.91813409800759,15.2707749253096,2.51414978148589));
#85913=CARTESIAN_POINT('Ctrl Pts',(-8.90316569275912,15.2694998891367,2.53083083402208));
#85914=CARTESIAN_POINT('Ctrl Pts',(-8.8594285966054,15.2656176851472,2.5818835794357));
#85915=CARTESIAN_POINT('Ctrl Pts',(-8.83185067574945,15.2629560089545,2.61723867634104));
#85916=CARTESIAN_POINT('Ctrl Pts',(-8.76571477293374,15.2560998208935,2.7105621294741));
#85917=CARTESIAN_POINT('Ctrl Pts',(-8.72958644884635,15.2518828934182,2.77012182467499));
#85918=CARTESIAN_POINT('Ctrl Pts',(-8.66329139191361,15.2432582374766,2.89935937343006));
#85919=CARTESIAN_POINT('Ctrl Pts',(-8.63402223335021,15.2388809762397,2.96927730756257));
#85920=CARTESIAN_POINT('Ctrl Pts',(-8.60696726604364,15.2340997210999,3.0512190044596));
#85921=CARTESIAN_POINT('Ctrl Pts',(-8.60375370267395,15.2335160378211,3.06131917599875));
#85922=CARTESIAN_POINT('Ctrl Pts',(-8.59876543850539,15.2325836435224,3.07760755540805));
#85923=CARTESIAN_POINT('Ctrl Pts',(-8.59692139169167,15.2322326936642,3.08377398647471));
#85924=CARTESIAN_POINT('Ctrl Pts',(-8.59371173635364,15.2316103979543,3.09477072777387));
#85925=CARTESIAN_POINT('Ctrl Pts',(-8.59233019510439,15.231338540544,3.09959624777577));
#85926=CARTESIAN_POINT('Ctrl Pts',(-8.58949485627215,15.2307720609224,3.10969573881254));
#85927=CARTESIAN_POINT('Ctrl Pts',(-8.58804574758886,15.2304775933667,3.11497095304563));
#85928=CARTESIAN_POINT('Ctrl Pts',(-8.58433856725694,15.2297110266837,3.12876868738873));
#85929=CARTESIAN_POINT('Ctrl Pts',(-8.58212785014757,15.2292404507844,3.13730377603917));
#85930=CARTESIAN_POINT('Ctrl Pts',(-8.57261337882318,15.2271526046165,3.17545406619381));
#85931=CARTESIAN_POINT('Ctrl Pts',(-8.56615913515251,15.2255624648734,3.20527440513749));
#85932=CARTESIAN_POINT('Ctrl Pts',(-8.55111580171925,15.2212957506551,3.28706814570617));
#85933=CARTESIAN_POINT('Ctrl Pts',(-8.54439223253082,15.2186734097962,3.33933888104768));
#85934=CARTESIAN_POINT('Ctrl Pts',(-8.53271469506209,15.2109152816151,3.49694491628077));
#85935=CARTESIAN_POINT('Ctrl Pts',(-8.53630096204094,15.2059294778514,3.60255235812155));
#85936=CARTESIAN_POINT('Ctrl Pts',(-8.55515876038345,15.1991151490045,3.73463556914109));
#85937=CARTESIAN_POINT('Ctrl Pts',(-8.55992412777462,15.1976536733168,3.76230009026063));
#85938=CARTESIAN_POINT('Ctrl Pts',(-8.5665717899392,15.1958563169162,3.79520523106249));
#85939=CARTESIAN_POINT('Ctrl Pts',(-8.56769246332606,15.1955599743587,3.80059554273705));
#85940=CARTESIAN_POINT('Ctrl Pts',(-8.56957524666501,15.195072512928,3.80940188176442));
#85941=CARTESIAN_POINT('Ctrl Pts',(-8.57031925367067,15.1948823896445,3.81282177425315));
#85942=CARTESIAN_POINT('Ctrl Pts',(-8.57167725771477,15.1945397342874,3.81895791075269));
#85943=CARTESIAN_POINT('Ctrl Pts',(-8.57228674636658,15.1943874589618,3.82167510033378));
#85944=CARTESIAN_POINT('Ctrl Pts',(-8.57363314941225,15.1940543189583,3.82759835020923));
#85945=CARTESIAN_POINT('Ctrl Pts',(-8.57437310994154,15.1938732871037,3.83080362969389));
#85946=CARTESIAN_POINT('Ctrl Pts',(-8.5764997290435,15.1933588017598,3.83987581880031));
#85947=CARTESIAN_POINT('Ctrl Pts',(-8.57791182445659,15.1930239490981,3.84573662232813));
#85948=CARTESIAN_POINT('Ctrl Pts',(-8.58709103329239,15.1908898132808,3.88282643978772));
#85949=CARTESIAN_POINT('Ctrl Pts',(-8.59584967683019,15.1890401039775,3.91379873525406));
#85950=CARTESIAN_POINT('Ctrl Pts',(-8.62968671575224,15.1825226835892,4.01995498778359));
#85951=CARTESIAN_POINT('Ctrl Pts',(-8.65984367379001,15.1777083807406,4.09337346073131));
#85952=CARTESIAN_POINT('Ctrl Pts',(-8.74113151012844,15.1669527749925,4.25303920240693));
#85953=CARTESIAN_POINT('Ctrl Pts',(-8.79547653613902,15.1610858880768,4.33722594648556));
#85954=CARTESIAN_POINT('Ctrl Pts',(-8.86464691593975,15.1549567769307,4.42353614521159));
#85955=CARTESIAN_POINT('Ctrl Pts',(-8.87139665549476,15.1543703086505,4.43177257750891));
#85956=CARTESIAN_POINT('Ctrl Pts',(-8.88237880792422,15.1534343455758,4.44487921608996));
#85957=CARTESIAN_POINT('Ctrl Pts',(-8.88655449133425,15.1530825845425,4.44979627450981));
#85958=CARTESIAN_POINT('Ctrl Pts',(-8.8940382259944,15.1524593604496,4.45849153317498));
#85959=CARTESIAN_POINT('Ctrl Pts',(-8.89733344966403,15.1521873805266,4.46228059544641));
#85960=CARTESIAN_POINT('Ctrl Pts',(-8.90425456370589,15.1516211520048,4.47015670816005));
#85961=CARTESIAN_POINT('Ctrl Pts',(-8.90788397529257,15.151327054929,4.4742405705148));
#85962=CARTESIAN_POINT('Ctrl Pts',(-8.91740831308821,15.15056255699,4.48483737510305));
#85963=CARTESIAN_POINT('Ctrl Pts',(-8.92333920827098,15.1500936639218,4.4913177896407));
#85964=CARTESIAN_POINT('Ctrl Pts',(-8.94990532124871,15.148024324217,4.51982567745601));
#85965=CARTESIAN_POINT('Ctrl Pts',(-8.97116145693098,15.1464504051846,4.5412658961279));
#85966=CARTESIAN_POINT('Ctrl Pts',(-9.03069252501514,15.1422399951761,4.59770834599292));
#85967=CARTESIAN_POINT('Ctrl Pts',(-9.07018946038228,15.1396558716182,4.63135914252011));
#85968=CARTESIAN_POINT('Ctrl Pts',(-9.19486868036149,15.1319477799415,4.72663505465746));
#85969=CARTESIAN_POINT('Ctrl Pts',(-9.28496457063728,15.1269772920335,4.78124582763346));
#85970=CARTESIAN_POINT('Ctrl Pts',(-9.4067730171197,15.1201240747427,4.83820014783875));
#85971=CARTESIAN_POINT('Ctrl Pts',(-9.43379323321419,15.1185945897375,4.84985464223194));
#85972=CARTESIAN_POINT('Ctrl Pts',(-9.46633703910955,15.1167210616185,4.86274256060889));
#85973=CARTESIAN_POINT('Ctrl Pts',(-9.47154133525394,15.116420512928,4.86476916728659));
#85974=CARTESIAN_POINT('Ctrl Pts',(-9.48004818434357,15.1159275165333,4.86802586915334));
#85975=CARTESIAN_POINT('Ctrl Pts',(-9.48334385371099,15.1157361028238,4.8692739299524));
#85976=CARTESIAN_POINT('Ctrl Pts',(-9.48925323858479,15.1153920784687,4.87148742584891));
#85977=CARTESIAN_POINT('Ctrl Pts',(-9.49186523334213,15.1152397337505,4.87245731165007));
#85978=CARTESIAN_POINT('Ctrl Pts',(-9.49754953501219,15.1149075697124,4.87454955480878));
#85979=CARTESIAN_POINT('Ctrl Pts',(-9.5006227984139,15.1147275908429,4.87566905849327));
#85980=CARTESIAN_POINT('Ctrl Pts',(-9.50928928780186,15.1142190081,4.87879314969508));
#85981=CARTESIAN_POINT('Ctrl Pts',(-9.51489093931473,15.1138890543297,4.88077396755631));
#85982=CARTESIAN_POINT('Ctrl Pts',(-9.54931690174186,15.1118544377,4.8927120971759));
#85983=CARTESIAN_POINT('Ctrl Pts',(-9.57843268625854,15.1101045038807,4.90179990534415));
#85984=CARTESIAN_POINT('Ctrl Pts',(-9.75160576131538,15.0996110617689,4.94996894629137));
#85985=CARTESIAN_POINT('Ctrl Pts',(-9.90068412272485,15.0903494570182,4.96773943994467));
#85986=CARTESIAN_POINT('Ctrl Pts',(-10.0854962516892,15.0797468876945,4.96143470858105));
#85987=CARTESIAN_POINT('Ctrl Pts',(-10.1210410043669,15.0777412714519,4.9589209714033));
#85988=CARTESIAN_POINT('Ctrl Pts',(-10.1660972810273,15.075240820453,4.95407629656318));
#85989=CARTESIAN_POINT('Ctrl Pts',(-10.1757232652197,15.074709027742,4.95294443231735));
#85990=CARTESIAN_POINT('Ctrl Pts',(-10.1909556123931,15.0738712008915,4.95099975264291));
#85991=CARTESIAN_POINT('Ctrl Pts',(-10.1965696060167,15.073563209881,4.95024988168364));
#85992=CARTESIAN_POINT('Ctrl Pts',(-10.207065141767,15.0729888615243,4.94878591045955));
#85993=CARTESIAN_POINT('Ctrl Pts',(-10.2119476860737,15.0727222620452,4.94807968236347));
#85994=CARTESIAN_POINT('Ctrl Pts',(-10.2229399456884,15.072123346253,4.94643293735704));
#85995=CARTESIAN_POINT('Ctrl Pts',(-10.229047482265,15.071791475386,4.94547836861207));
#85996=CARTESIAN_POINT('Ctrl Pts',(-10.2471186793039,15.070812082335,4.942536544441));
#85997=CARTESIAN_POINT('Ctrl Pts',(-10.2590640514646,15.0701680188861,4.94043922214755));
#85998=CARTESIAN_POINT('Ctrl Pts',(-10.3686230803753,15.0642885205211,4.91979627920464));
#85999=CARTESIAN_POINT('Ctrl Pts',(-10.4641395082695,15.059389569775,4.89150352424864));
#86000=CARTESIAN_POINT('Ctrl Pts',(-10.6037619261951,15.0520418276346,4.83415254617049));
#86001=CARTESIAN_POINT('Ctrl Pts',(-10.6503924129982,15.0495482740272,4.81205219940654));
#86002=CARTESIAN_POINT('Ctrl Pts',(-10.7467881196453,15.0441421405985,4.75996199431381));
#86003=CARTESIAN_POINT('Ctrl Pts',(-10.7961285062314,15.0412206506213,4.72937980734762));
#86004=CARTESIAN_POINT('Ctrl Pts',(-10.8493986491535,15.0377424432373,4.69180785200379));
#86005=CARTESIAN_POINT('Ctrl Pts',(-10.8552477198228,15.0373559014095,4.68761751199154));
#86006=CARTESIAN_POINT('Ctrl Pts',(-10.8639211302505,15.0367753855477,4.68130648117454));
#86007=CARTESIAN_POINT('Ctrl Pts',(-10.8667691663875,15.0365835749731,4.6792183569735));
#86008=CARTESIAN_POINT('Ctrl Pts',(-10.8717822395187,15.0362437936472,4.67551489719724));
#86009=CARTESIAN_POINT('Ctrl Pts',(-10.8739503922626,15.0360961185289,4.67390385398586));
#86010=CARTESIAN_POINT('Ctrl Pts',(-10.8761257756508,15.0359472199628,4.67227807087424));
#86011=CARTESIAN_POINT('Ctrl Pts',(-10.8761374461992,15.0359464211272,4.67226934856275));
#86012=CARTESIAN_POINT('Ctrl Pts',(-10.8761606415294,15.0359448333915,4.67225201234286));
#86013=CARTESIAN_POINT('Ctrl Pts',(-10.8761721662952,15.0359440444931,4.67224339845296));
#86014=CARTESIAN_POINT('Ctrl Pts',(-10.876195072934,15.0359424764368,4.67222627694832));
#86015=CARTESIAN_POINT('Ctrl Pts',(-10.8762064547431,15.0359416972838,4.67221776938775));
#86016=CARTESIAN_POINT('Ctrl Pts',(-10.8762290780093,15.0359401485458,4.67220085866198));
#86017=CARTESIAN_POINT('Ctrl Pts',(-10.8762403195403,15.0359393789562,4.67219245544786));
#86018=CARTESIAN_POINT('Ctrl Pts',(-10.8762626646925,15.0359378491795,4.67217575160816));
#86019=CARTESIAN_POINT('Ctrl Pts',(-10.8762737684747,15.0359370889817,4.67216745086838));
#86020=CARTESIAN_POINT('Ctrl Pts',(-10.8762958409873,15.0359355777943,4.67215094985926));
#86021=CARTESIAN_POINT('Ctrl Pts',(-10.8763068096672,15.0359348268085,4.67214274963351));
#86022=CARTESIAN_POINT('Ctrl Pts',(-10.8763286144016,15.0359333338804,4.6721264478562));
#86023=CARTESIAN_POINT('Ctrl Pts',(-10.8763394504403,15.0359325919395,4.67211834632221));
#86024=CARTESIAN_POINT('Ctrl Pts',(-10.876360992492,15.0359311169245,4.67210224000176));
#86025=CARTESIAN_POINT('Ctrl Pts',(-10.8763716984013,15.0359303838578,4.67209423529848));
#86026=CARTESIAN_POINT('Ctrl Pts',(-10.8763929823846,15.0359289264425,4.67207832101846));
#86027=CARTESIAN_POINT('Ctrl Pts',(-10.8764035604791,15.0359282020929,4.67207041143181));
#86028=CARTESIAN_POINT('Ctrl Pts',(-10.87642459128,15.0359267619452,4.67205468557145));
#86029=CARTESIAN_POINT('Ctrl Pts',(-10.8764350439283,15.0359260461517,4.6720468693464));
#86030=CARTESIAN_POINT('Ctrl Pts',(-10.87645582608,15.0359246229638,4.67203132854752));
#86031=CARTESIAN_POINT('Ctrl Pts',(-10.8764661555771,15.0359239155703,4.67202360398344));
#86032=CARTESIAN_POINT('Ctrl Pts',(-10.8764866934039,15.0359225090484,4.67200824504284));
#86033=CARTESIAN_POINT('Ctrl Pts',(-10.8764969018557,15.035921809912,4.67200061057998));
#86034=CARTESIAN_POINT('Ctrl Pts',(-10.8790948178505,15.0357438848339,4.67005768780813));
#86035=CARTESIAN_POINT('Ctrl Pts',(-10.8816760830758,15.0355660632671,4.66811385390571));
#86036=CARTESIAN_POINT('Ctrl Pts',(-10.8870281543534,15.0351952399179,4.66405560500789));
#86037=CARTESIAN_POINT('Ctrl Pts',(-10.8897978843546,15.0350021453055,4.66193981025642));
#86038=CARTESIAN_POINT('Ctrl Pts',(-10.8968822653561,15.0345052447549,4.65648787208356));
#86039=CARTESIAN_POINT('Ctrl Pts',(-10.9011858352736,15.0342005137745,4.65313749598288));
#86040=CARTESIAN_POINT('Ctrl Pts',(-10.9136945416134,15.0333066007085,4.64328654167272));
#86041=CARTESIAN_POINT('Ctrl Pts',(-10.9218486271412,15.0327135089199,4.63672201020118));
#86042=CARTESIAN_POINT('Ctrl Pts',(-10.9502818532888,15.0306106923727,4.61332440552044));
#86043=CARTESIAN_POINT('Ctrl Pts',(-10.9701752541397,15.0290764114008,4.59603223683043));
#86044=CARTESIAN_POINT('Ctrl Pts',(-11.0934145911177,15.0192189751559,4.48292253295863));
#86045=CARTESIAN_POINT('Ctrl Pts',(-11.1829560351067,15.0105232002911,4.37310861173191));
#86046=CARTESIAN_POINT('Ctrl Pts',(-11.2732444225819,15.0004615697204,4.22241629916845));
#86047=CARTESIAN_POINT('Ctrl Pts',(-11.2900177844434,14.9985088288786,4.19201955965918));
#86048=CARTESIAN_POINT('Ctrl Pts',(-11.310034610839,14.9960640539962,4.15248283331175));
#86049=CARTESIAN_POINT('Ctrl Pts',(-11.3142892568767,14.9955370342598,4.14386977317137));
#86050=CARTESIAN_POINT('Ctrl Pts',(-11.320908966445,14.9947049830729,4.1301298415765));
#86051=CARTESIAN_POINT('Ctrl Pts',(-11.3233296496965,14.9943980403267,4.12503020275846));
#86052=CARTESIAN_POINT('Ctrl Pts',(-11.327620482344,14.9938490564419,4.1158540559587));
#86053=CARTESIAN_POINT('Ctrl Pts',(-11.3295015040351,14.9936066450047,4.11178273493822));
#86054=CARTESIAN_POINT('Ctrl Pts',(-11.3338552306561,14.9930414167458,4.10224452974898));
#86055=CARTESIAN_POINT('Ctrl Pts',(-11.3363131003484,14.9927191086675,4.09677093533924));
#86056=CARTESIAN_POINT('Ctrl Pts',(-11.3432828386302,14.9917956881457,4.08099057461121));
#86057=CARTESIAN_POINT('Ctrl Pts',(-11.3477096635691,14.9911974552448,4.07064656705221));
#86058=CARTESIAN_POINT('Ctrl Pts',(-11.3805409257206,14.9866669468822,3.99141723359833));
#86059=CARTESIAN_POINT('Ctrl Pts',(-11.4037681826831,14.9829153079701,3.92050074532737));
#86060=CARTESIAN_POINT('Ctrl Pts',(-11.4494005048327,14.97347487253,3.7341661659573));
#86061=CARTESIAN_POINT('Ctrl Pts',(-11.4634999999989,14.9679620217355,3.6172895195206));
#86062=CARTESIAN_POINT('Ctrl Pts',(-11.4635,14.961903098074,3.50000000001399));
#86063=CARTESIAN_POINT('Ctrl Pts',(-11.4635,14.8882344353249,3.49999999998375));
#86064=CARTESIAN_POINT('Ctrl Pts',(-11.4635000000011,14.8942398463545,3.60316946844975));
#86065=CARTESIAN_POINT('Ctrl Pts',(-11.4525909842708,14.9005631074229,3.70605351707629));
#86066=CARTESIAN_POINT('Ctrl Pts',(-11.4139418140341,14.9115352747244,3.88623554115491));
#86067=CARTESIAN_POINT('Ctrl Pts',(-11.3903693881249,14.9162386267349,3.96398890181075));
#86068=CARTESIAN_POINT('Ctrl Pts',(-11.3562631000691,14.9213624430335,4.05001182474101));
#86069=CARTESIAN_POINT('Ctrl Pts',(-11.3519309330338,14.9219904851051,4.06057592407899));
#86070=CARTESIAN_POINT('Ctrl Pts',(-11.3451200584314,14.9229442315386,4.07664609054269));
#86071=CARTESIAN_POINT('Ctrl Pts',(-11.3427302335125,14.9232729065917,4.08218915042296));
#86072=CARTESIAN_POINT('Ctrl Pts',(-11.3383096329501,14.9238701753104,4.09227045635291));
#86073=CARTESIAN_POINT('Ctrl Pts',(-11.3362899035378,14.9241391373364,4.09681342282491));
#86074=CARTESIAN_POINT('Ctrl Pts',(-11.3318657990193,14.9247199180101,4.1066294819829));
#86075=CARTESIAN_POINT('Ctrl Pts',(-11.3294531674705,14.9250314504131,4.11189877580763));
#86076=CARTESIAN_POINT('Ctrl Pts',(-11.3227856777081,14.9258785004376,4.12623527163765));
#86077=CARTESIAN_POINT('Ctrl Pts',(-11.3184688953993,14.9264118950679,4.13527343965763));
#86078=CARTESIAN_POINT('Ctrl Pts',(-11.2961109676347,14.9291009078496,4.18087512597888));
#86079=CARTESIAN_POINT('Ctrl Pts',(-11.276639515071,14.9312065918726,4.21671927176488));
#86080=CARTESIAN_POINT('Ctrl Pts',(-11.2485836215971,14.9339726899913,4.26358555172696));
#86081=CARTESIAN_POINT('Ctrl Pts',(-11.2413036116069,14.9346690809629,4.27536398611937));
#86082=CARTESIAN_POINT('Ctrl Pts',(-11.1799430085759,14.9403743632802,4.37156046142418));
#86083=CARTESIAN_POINT('Ctrl Pts',(-11.1174888547309,14.9451375093534,4.45031637052945));
#86084=CARTESIAN_POINT('Ctrl Pts',(-11.0196089356964,14.9520556001033,4.55062939020628));
#86085=CARTESIAN_POINT('Ctrl Pts',(-10.9905869972881,14.954054528487,4.57803594963648));
#86086=CARTESIAN_POINT('Ctrl Pts',(-10.9500432617639,14.9568351377534,4.61330208036142));
#86087=CARTESIAN_POINT('Ctrl Pts',(-10.9394749762753,14.9575589466431,4.6222345857603));
#86088=CARTESIAN_POINT('Ctrl Pts',(-10.9236417963749,14.9586445506031,4.63523668057777));
#86089=CARTESIAN_POINT('Ctrl Pts',(-10.9184729937097,14.9589991370126,4.63942259306721));
#86090=CARTESIAN_POINT('Ctrl Pts',(-10.9091064979989,14.959642388092,4.64690282800226));
#86091=CARTESIAN_POINT('Ctrl Pts',(-10.9049189505992,14.9599302188324,4.65020972551071));
#86092=CARTESIAN_POINT('Ctrl Pts',(-10.898231985169,14.9603904047423,4.65543128885926));
#86093=CARTESIAN_POINT('Ctrl Pts',(-10.8957442696172,14.9605617268526,4.65736094867607));
#86094=CARTESIAN_POINT('Ctrl Pts',(-10.8911614439799,14.9608775956956,4.66089210741686));
#86095=CARTESIAN_POINT('Ctrl Pts',(-10.8890682196649,14.961021973266,4.66249598052491));
#86096=CARTESIAN_POINT('Ctrl Pts',(-10.8841668262038,14.9613602744784,4.66623055142004));
#86097=CARTESIAN_POINT('Ctrl Pts',(-10.8813552987281,14.9615545049822,4.66835675736992));
#86098=CARTESIAN_POINT('Ctrl Pts',(-10.8729956394954,14.9621324679079,4.67463136969499));
#86099=CARTESIAN_POINT('Ctrl Pts',(-10.8674257840841,14.9625181327696,4.67875050222272));
#86100=CARTESIAN_POINT('Ctrl Pts',(-10.8230534053649,14.965593722231,4.71108086177603));
#86101=CARTESIAN_POINT('Ctrl Pts',(-10.7829175560504,14.9683940614871,4.73740575378498));
#86102=CARTESIAN_POINT('Ctrl Pts',(-10.6648471168658,14.9765290500929,4.80680127348856));
#86103=CARTESIAN_POINT('Ctrl Pts',(-10.5841749258098,14.9819549150823,4.84480179992673));
#86104=CARTESIAN_POINT('Ctrl Pts',(-10.4376851436043,14.9911954356943,4.89811987002947));
#86105=CARTESIAN_POINT('Ctrl Pts',(-10.3733221161449,14.9950681815391,4.91666507748371));
#86106=CARTESIAN_POINT('Ctrl Pts',(-10.2926446318109,14.9996713321233,4.9340275980174));
#86107=CARTESIAN_POINT('Ctrl Pts',(-10.2773285912516,15.0005345839328,4.9370681651998));
#86108=CARTESIAN_POINT('Ctrl Pts',(-10.2552331436454,15.0017650987034,4.94108817557133));
#86109=CARTESIAN_POINT('Ctrl Pts',(-10.2484913042628,15.0021385838179,4.9422659814753));
#86110=CARTESIAN_POINT('Ctrl Pts',(-10.236744327441,15.0027859739623,4.94423337597208));
#86111=CARTESIAN_POINT('Ctrl Pts',(-10.2317429300737,15.0030605471564,4.94504433707251));
#86112=CARTESIAN_POINT('Ctrl Pts',(-10.222083272515,15.0035888442992,4.94655918076951));
#86113=CARTESIAN_POINT('Ctrl Pts',(-10.2174256332924,15.0038426754045,4.94726657465079));
#86114=CARTESIAN_POINT('Ctrl Pts',(-10.2063729698559,15.0044429241842,4.94889067310962));
#86115=CARTESIAN_POINT('Ctrl Pts',(-10.1999751014081,15.0047887180051,4.94978755200362));
#86116=CARTESIAN_POINT('Ctrl Pts',(-10.1773247131694,15.0060072159816,4.95280998481098));
#86117=CARTESIAN_POINT('Ctrl Pts',(-10.1610423161494,15.0068727314364,4.9547048864692));
#86118=CARTESIAN_POINT('Ctrl Pts',(-10.0263100253444,15.0139561778449,4.96809471160317));
#86119=CARTESIAN_POINT('Ctrl Pts',(-9.90689796821671,15.0196859228711,4.96537668725338));
#86120=CARTESIAN_POINT('Ctrl Pts',(-9.73074272871516,15.0283567719625,4.93972689016283));
#86121=CARTESIAN_POINT('Ctrl Pts',(-9.67293178081447,15.0312485904662,4.92770390335595));
#86122=CARTESIAN_POINT('Ctrl Pts',(-9.59042092525551,15.0356297987794,4.90526878823164));
#86123=CARTESIAN_POINT('Ctrl Pts',(-9.56502861172117,15.0370143228863,4.89761765242205));
#86124=CARTESIAN_POINT('Ctrl Pts',(-9.53443880959041,15.0387419692196,4.88748608588831));
#86125=CARTESIAN_POINT('Ctrl Pts',(-9.52902848969315,15.0390498334634,4.88565893886861));
#86126=CARTESIAN_POINT('Ctrl Pts',(-9.52058328674959,15.0395341974786,4.88275169186861));
#86127=CARTESIAN_POINT('Ctrl Pts',(-9.5175409817214,15.03970946082,4.88169313582316));
#86128=CARTESIAN_POINT('Ctrl Pts',(-9.51186717425911,15.0400378145127,4.87969793670759));
#86129=CARTESIAN_POINT('Ctrl Pts',(-9.50923484536701,15.0401907580668,4.87876379945913));
#86130=CARTESIAN_POINT('Ctrl Pts',(-9.50321882364958,15.0405416790484,4.87660947657419));
#86131=CARTESIAN_POINT('Ctrl Pts',(-9.49983695386807,15.0407399435442,4.8753843516939));
#86132=CARTESIAN_POINT('Ctrl Pts',(-9.49099111631437,15.0412610848098,4.872142895987));
#86133=CARTESIAN_POINT('Ctrl Pts',(-9.48553466333627,15.0415850985818,4.87010641402269));
#86134=CARTESIAN_POINT('Ctrl Pts',(-9.44831571681395,15.0438120040533,4.85596171357128));
#86135=CARTESIAN_POINT('Ctrl Pts',(-9.41697351941511,15.0457709147941,4.84278348446731));
#86136=CARTESIAN_POINT('Ctrl Pts',(-9.29484981178013,15.053661090066,4.786353200698));
#86137=CARTESIAN_POINT('Ctrl Pts',(-9.2081681221159,15.0598180118331,4.73488636195495));
#86138=CARTESIAN_POINT('Ctrl Pts',(-9.08610674666367,15.0688484644349,4.64423894864798));
#86139=CARTESIAN_POINT('Ctrl Pts',(-9.04641399966737,15.0718567349263,4.61137670636658));
#86140=CARTESIAN_POINT('Ctrl Pts',(-8.98643462371903,15.0764977565217,4.55613449917588));
#86141=CARTESIAN_POINT('Ctrl Pts',(-8.96496696949253,15.0781807497666,4.53510466383559));
#86142=CARTESIAN_POINT('Ctrl Pts',(-8.93808624996012,15.0803183400619,4.50709899690486));
#86143=CARTESIAN_POINT('Ctrl Pts',(-8.93206868824645,15.0807989404787,4.50071570396994));
#86144=CARTESIAN_POINT('Ctrl Pts',(-8.92239799450001,15.081574810741,4.49027067066547));
#86145=CARTESIAN_POINT('Ctrl Pts',(-8.91870963101484,15.0818715710564,4.48624196955192));
#86146=CARTESIAN_POINT('Ctrl Pts',(-8.91167201039257,15.0824394809647,4.47846802681584));
#86147=CARTESIAN_POINT('Ctrl Pts',(-8.90831932194101,15.0827107725056,4.47472600790505));
#86148=CARTESIAN_POINT('Ctrl Pts',(-8.90070000759502,15.0833290554933,4.46613327679684));
#86149=CARTESIAN_POINT('Ctrl Pts',(-8.89644607895447,15.0836755183138,4.461271411728));
#86150=CARTESIAN_POINT('Ctrl Pts',(-8.88524770984574,15.0845910819654,4.44830035377643));
#86151=CARTESIAN_POINT('Ctrl Pts',(-8.87835950325239,15.0851578899332,4.44014298563865));
#86152=CARTESIAN_POINT('Ctrl Pts',(-8.81071966705183,15.0907626790732,4.35823876962812));
#86153=CARTESIAN_POINT('Ctrl Pts',(-8.75723664950791,15.0954906074507,4.27878347640379));
#86154=CARTESIAN_POINT('Ctrl Pts',(-8.67257484173989,15.1041820835112,4.12179602815909));
#86155=CARTESIAN_POINT('Ctrl Pts',(-8.63953134981396,15.1081543712008,4.04572072778805));
#86156=CARTESIAN_POINT('Ctrl Pts',(-8.60259495352467,15.1140247168365,3.93608911931097));
#86157=CARTESIAN_POINT('Ctrl Pts',(-8.59314601981413,15.1157295742275,3.90456908694282));
#86158=CARTESIAN_POINT('Ctrl Pts',(-8.58322291074366,15.1178157959694,3.86689469457777));
#86159=CARTESIAN_POINT('Ctrl Pts',(-8.5817145619884,15.1181424879712,3.8610200150951));
#86160=CARTESIAN_POINT('Ctrl Pts',(-8.57944245509655,15.118649981678,3.8519366273158));
#86161=CARTESIAN_POINT('Ctrl Pts',(-8.57865293632641,15.1188293464862,3.84873435760762));
#86162=CARTESIAN_POINT('Ctrl Pts',(-8.57721666971745,15.1191613315591,3.84282299014518));
#86163=CARTESIAN_POINT('Ctrl Pts',(-8.57656682681676,15.1193137736565,3.84011469922855));
#86164=CARTESIAN_POINT('Ctrl Pts',(-8.57511966607134,15.1196583456021,3.83400670283099));
#86165=CARTESIAN_POINT('Ctrl Pts',(-8.57432678731008,15.1198507221023,3.83060600969835));
#86166=CARTESIAN_POINT('Ctrl Pts',(-8.57232147347091,15.1203465770944,3.82186375578899));
#86167=CARTESIAN_POINT('Ctrl Pts',(-8.57112685318125,15.1206510241418,3.81651821555197));
#86168=CARTESIAN_POINT('Ctrl Pts',(-8.56409799375259,15.1224977955142,3.78421543125748));
#86169=CARTESIAN_POINT('Ctrl Pts',(-8.55899712432177,15.1240770293036,3.75710599878659));
#86170=CARTESIAN_POINT('Ctrl Pts',(-8.53796603708125,15.1318701327016,3.62487089865659));
#86171=CARTESIAN_POINT('Ctrl Pts',(-8.53275795637476,15.1383937334468,3.51836579631194));
#86172=CARTESIAN_POINT('Ctrl Pts',(-8.5422747562762,15.1478266647474,3.35995562693801));
#86173=CARTESIAN_POINT('Ctrl Pts',(-8.54821990518427,15.1508889964035,3.30787842699104));
#86174=CARTESIAN_POINT('Ctrl Pts',(-8.56200742495591,15.1556021272015,3.22626056100973));
#86175=CARTESIAN_POINT('Ctrl Pts',(-8.56800225099869,15.1573051241657,3.19645664774875));
#86176=CARTESIAN_POINT('Ctrl Pts',(-8.57692604473056,15.1594640281688,3.15828324986426));
#86177=CARTESIAN_POINT('Ctrl Pts',(-8.57900829327314,15.1599465821011,3.14972525973881));
#86178=CARTESIAN_POINT('Ctrl Pts',(-8.58250874671746,15.1607248206277,3.13588365186717));
#86179=CARTESIAN_POINT('Ctrl Pts',(-8.58387952145032,15.1610220125585,3.13058836039581));
#86180=CARTESIAN_POINT('Ctrl Pts',(-8.5865657045988,15.1615902331718,3.12044636543015));
#86181=CARTESIAN_POINT('Ctrl Pts',(-8.58787643387499,15.161861407242,3.11559851223665));
#86182=CARTESIAN_POINT('Ctrl Pts',(-8.59092596060797,15.1624787167359,3.10454567252207));
#86183=CARTESIAN_POINT('Ctrl Pts',(-8.5926808455952,15.1628243294063,3.09834520659373));
#86184=CARTESIAN_POINT('Ctrl Pts',(-8.59743651468287,15.1637361433772,3.08195606861809));
#86185=CARTESIAN_POINT('Ctrl Pts',(-8.60050738803506,15.1643000822078,3.07178802462116));
#86186=CARTESIAN_POINT('Ctrl Pts',(-8.62663584487003,15.1689034814842,2.98855818020661));
#86187=CARTESIAN_POINT('Ctrl Pts',(-8.65528821930903,15.1727511726298,2.91737318651635));
#86188=CARTESIAN_POINT('Ctrl Pts',(-8.71979843770249,15.1798725818493,2.78754861217136));
#86189=CARTESIAN_POINT('Ctrl Pts',(-8.75445983502587,15.183156754937,2.72855166315073));
#86190=CARTESIAN_POINT('Ctrl Pts',(-8.81857046839752,15.1887237550825,2.6350828894891));
#86191=CARTESIAN_POINT('Ctrl Pts',(-8.84572121775919,15.190963756061,2.59916853803295));
#86192=CARTESIAN_POINT('Ctrl Pts',(-8.88884382868792,15.1944443208247,2.54728328637657));
#86193=CARTESIAN_POINT('Ctrl Pts',(-8.90360178069876,15.1956234681499,2.5303361365475));
#86194=CARTESIAN_POINT('Ctrl Pts',(-8.92240025110593,15.1971205180982,2.50972706789437));
#86195=CARTESIAN_POINT('Ctrl Pts',(-8.92607954657268,15.1974133001321,2.50573818502168));
#86196=CARTESIAN_POINT('Ctrl Pts',(-8.931935389935,15.1978791013175,2.49946003768659));
#86197=CARTESIAN_POINT('Ctrl Pts',(-8.93409734858696,15.1980510351194,2.49715715848275));
#86198=CARTESIAN_POINT('Ctrl Pts',(-8.93819303292104,15.1983767204283,2.49282271608833));
#86199=CARTESIAN_POINT('Ctrl Pts',(-8.94012515282852,15.1985303517351,2.49078970257424));
#86200=CARTESIAN_POINT('Ctrl Pts',(-8.94457665313866,15.1988842745235,2.48613263101965));
#86201=CARTESIAN_POINT('Ctrl Pts',(-8.94709998197698,15.1990848666479,2.48351240320294));
#86202=CARTESIAN_POINT('Ctrl Pts',(-8.95387576549448,15.1996233624182,2.47652872085102));
#86203=CARTESIAN_POINT('Ctrl Pts',(-8.95814569798557,15.1999625572352,2.47218241695962));
#86204=CARTESIAN_POINT('Ctrl Pts',(-8.99086001091462,15.2025592526505,2.43929630025795));
#86205=CARTESIAN_POINT('Ctrl Pts',(-9.02044280829839,15.2048952455832,2.41191773726276));
#86206=CARTESIAN_POINT('Ctrl Pts',(-9.12762148620842,15.2132045294412,2.32064147821887));
#86207=CARTESIAN_POINT('Ctrl Pts',(-9.21063609141853,15.2193546353876,2.26353858448475));
#86208=CARTESIAN_POINT('Ctrl Pts',(-9.35504210098213,15.2290851614235,2.18472066462419));
#86209=CARTESIAN_POINT('Ctrl Pts',(-9.41319061678508,15.2327831895614,2.1577679644304));
#86210=CARTESIAN_POINT('Ctrl Pts',(-9.48715955031423,15.2372033364255,2.12921198571385));
#86211=CARTESIAN_POINT('Ctrl Pts',(-9.50148064875236,15.2380466929788,2.12393910448444));
#86212=CARTESIAN_POINT('Ctrl Pts',(-9.52228131036886,15.2392541508225,2.11664788048163));
#86213=CARTESIAN_POINT('Ctrl Pts',(-9.52869621747294,15.239624156737,2.11444921430426));
#86214=CARTESIAN_POINT('Ctrl Pts',(-9.53992068113804,15.2402675002265,2.11068907853604));
#86215=CARTESIAN_POINT('Ctrl Pts',(-9.54472344343061,15.2405414821885,2.10910781364137));
#86216=CARTESIAN_POINT('Ctrl Pts',(-9.55403218860354,15.2410700484772,2.10609637742144));
#86217=CARTESIAN_POINT('Ctrl Pts',(-9.55853709014672,15.2413247317102,2.10466308807332));
#86218=CARTESIAN_POINT('Ctrl Pts',(-9.56927498891296,15.2419291881029,2.10130390264339));
#86219=CARTESIAN_POINT('Ctrl Pts',(-9.57551410401955,15.2422783162133,2.09939779597486));
#86220=CARTESIAN_POINT('Ctrl Pts',(-9.5978395194634,15.2435203394882,2.0927400602162));
#86221=CARTESIAN_POINT('Ctrl Pts',(-9.61399483812844,15.2444056707068,2.08822323447989));
#86222=CARTESIAN_POINT('Ctrl Pts',(-9.73956200821279,15.251190923548,2.05543287596522));
#86223=CARTESIAN_POINT('Ctrl Pts',(-9.85183739388462,15.2566579178559,2.03963955576761));
#86224=CARTESIAN_POINT('Ctrl Pts',(-10.0507956081288,15.2663404534831,2.03485561460626));
#86225=CARTESIAN_POINT('Ctrl Pts',(-10.136775493678,15.2705381222922,2.0403709239744));
#86226=CARTESIAN_POINT('Ctrl Pts',(-10.2305116623212,15.2755742466312,2.05474051074436));
#86227=CARTESIAN_POINT('Ctrl Pts',(-10.239249431601,15.2760482308405,2.05616125570871));
#86228=CARTESIAN_POINT('Ctrl Pts',(-10.2517606175828,15.276734097112,2.05831223658529));
#86229=CARTESIAN_POINT('Ctrl Pts',(-10.2555450554805,15.2769425073409,2.05897823067048));
#86230=CARTESIAN_POINT('Ctrl Pts',(-10.2621071076818,15.2773055924583,2.06015969812805));
#86231=CARTESIAN_POINT('Ctrl Pts',(-10.2648859575046,15.2774598833904,2.06066832861743));
#86232=CARTESIAN_POINT('Ctrl Pts',(-10.270320301903,15.2777626858669,2.06167928186661));
#86233=CARTESIAN_POINT('Ctrl Pts',(-10.2729758814471,15.2779111523883,2.0621809148104));
#86234=CARTESIAN_POINT('Ctrl Pts',(-10.2802635831982,15.2783199255853,2.06357846254583));
#86235=CARTESIAN_POINT('Ctrl Pts',(-10.2848927434349,15.2785810635875,2.06448941738199));
#86236=CARTESIAN_POINT('Ctrl Pts',(-10.3029047561696,15.2796027175856,2.06812448837272));
#86237=CARTESIAN_POINT('Ctrl Pts',(-10.3162531984437,15.2803718408089,2.07101341540137));
#86238=CARTESIAN_POINT('Ctrl Pts',(-10.3548769649107,15.2826283341168,2.07994019741264));
#86239=CARTESIAN_POINT('Ctrl Pts',(-10.380033541817,15.2841368213591,2.08646476304541));
#86240=CARTESIAN_POINT('Ctrl Pts',(-10.4146769176456,15.2862563404977,2.09644142347499));
#86241=CARTESIAN_POINT('Ctrl Pts',(-10.4243230089417,15.2868511053106,2.0993274466112));
#86242=CARTESIAN_POINT('Ctrl Pts',(-10.5125573669318,15.2923296385583,2.12672146906737));
#86243=CARTESIAN_POINT('Ctrl Pts',(-10.5889765547282,15.2973426361053,2.15771986660788));
#86244=CARTESIAN_POINT('Ctrl Pts',(-10.7117423426112,15.3055455699722,2.22003170265305));
#86245=CARTESIAN_POINT('Ctrl Pts',(-10.7596421104052,15.308790722422,2.24786549118916));
#86246=CARTESIAN_POINT('Ctrl Pts',(-10.832183641133,15.3137458524652,2.29571698768956));
#86247=CARTESIAN_POINT('Ctrl Pts',(-10.8579466149676,15.315514915319,2.31393296639621));
#86248=CARTESIAN_POINT('Ctrl Pts',(-10.8902155388229,15.3177439931508,2.33835112129689));
#86249=CARTESIAN_POINT('Ctrl Pts',(-10.8972796084536,15.3182328340307,2.3437988357749));
#86250=CARTESIAN_POINT('Ctrl Pts',(-10.9086137858932,15.3190186944345,2.35270604041413));
#86251=CARTESIAN_POINT('Ctrl Pts',(-10.9129149172011,15.319317276063,2.35612553279761));
#86252=CARTESIAN_POINT('Ctrl Pts',(-10.9211044943868,15.3198865224981,2.36271203801644));
#86253=CARTESIAN_POINT('Ctrl Pts',(-10.9249961123888,15.3201573436389,2.36587496677694));
#86254=CARTESIAN_POINT('Ctrl Pts',(-10.9338122744345,15.3207716391897,2.37311590402879));
#86255=CARTESIAN_POINT('Ctrl Pts',(-10.9387265249153,15.3211146090705,2.37720632223563));
#86256=CARTESIAN_POINT('Ctrl Pts',(-10.9516023477294,15.3220147981336,2.38806724864338));
#86257=CARTESIAN_POINT('Ctrl Pts',(-10.9595185540679,15.3225698478196,2.39489112587574));
#86258=CARTESIAN_POINT('Ctrl Pts',(-11.0193993321717,15.3267824026093,2.44763771282057));
#86259=CARTESIAN_POINT('Ctrl Pts',(-11.0681165806546,15.3302849749552,2.49711919994953));
#86260=CARTESIAN_POINT('Ctrl Pts',(-11.1288964898801,15.3349052785255,2.56832753106945));
#86261=CARTESIAN_POINT('Ctrl Pts',(-11.1441863649272,15.3360927912822,2.58717007640934));
#86262=CARTESIAN_POINT('Ctrl Pts',(-11.1978185158371,15.3403758920866,2.65672985655768));
#86263=CARTESIAN_POINT('Ctrl Pts',(-11.2333132507234,15.3434382683448,2.70954967388866));
#86264=CARTESIAN_POINT('Ctrl Pts',(-11.2896613205186,15.3489951677788,2.80648476672443));
#86265=CARTESIAN_POINT('Ctrl Pts',(-11.3119561216286,15.3514505166937,2.84964624668677));
#86266=CARTESIAN_POINT('Ctrl Pts',(-11.3361664199632,15.3545460996965,2.90284868204695));
#86267=CARTESIAN_POINT('Ctrl Pts',(-11.3401780258813,15.3550755149608,2.91190711053269));
#86268=CARTESIAN_POINT('Ctrl Pts',(-11.345688046681,15.3558273118416,2.92469825358599));
#86269=CARTESIAN_POINT('Ctrl Pts',(-11.3472636007124,15.3560452380944,2.92839768385424));
#86270=CARTESIAN_POINT('Ctrl Pts',(-11.3499319561595,15.3564194958149,2.9347353556276));
#86271=CARTESIAN_POINT('Ctrl Pts',(-11.3510323313652,15.3565753745971,2.93737042030137));
#86272=CARTESIAN_POINT('Ctrl Pts',(-11.3531397029463,15.3568769281393,2.94245876668105));
#86273=CARTESIAN_POINT('Ctrl Pts',(-11.3541477497147,15.3570225335151,2.94491157979048));
#86274=CARTESIAN_POINT('Ctrl Pts',(-11.3565536419067,15.3573733112104,2.95081123337625));
#86275=CARTESIAN_POINT('Ctrl Pts',(-11.3579450170331,15.3575788627272,2.95426067133729));
#86276=CARTESIAN_POINT('Ctrl Pts',(-11.3629671215119,15.3583305848348,2.96684937917546));
#86277=CARTESIAN_POINT('Ctrl Pts',(-11.3665187740726,15.3588811721961,2.97601966810231));
#86278=CARTESIAN_POINT('Ctrl Pts',(-11.4090758996143,15.3657117135496,3.08927747424932));
#86279=CARTESIAN_POINT('Ctrl Pts',(-11.4361902494202,15.3725209920055,3.1974391301335));
#86280=CARTESIAN_POINT('Ctrl Pts',(-11.4592203408166,15.3830179682979,3.37111649555571));
#86281=CARTESIAN_POINT('Ctrl Pts',(-11.4634632343829,15.3868013572218,3.43510224584699));
#86282=CARTESIAN_POINT('Ctrl Pts',(-11.463499920781,15.390483742019,3.49944368928866));
#86283=CARTESIAN_POINT('Ctrl Pts',(-11.4635,15.390499659156,3.49972184492555));
#86284=CARTESIAN_POINT('Ctrl Pts',(-11.4635,15.3905155741067,3.49999999999573));
#86285=CARTESIAN_POINT('Origin',(-10.,13.2,3.5));
#86286=CARTESIAN_POINT('',(-11.4635,15.960023863236,3.50000000002449));
#86287=CARTESIAN_POINT('',(-11.4635,15.8897282898296,3.49999999995642));
#86288=CARTESIAN_POINT('',(-11.4635,13.2,3.5));
#86289=CARTESIAN_POINT('Ctrl Pts',(-11.4635,15.960023863236,3.50000000002449));
#86290=CARTESIAN_POINT('Ctrl Pts',(-11.4635000000009,15.9568962036078,3.4473044483025));
#86291=CARTESIAN_POINT('Ctrl Pts',(-11.4606539605496,15.9538221865891,3.39464321866628));
#86292=CARTESIAN_POINT('Ctrl Pts',(-11.4524341116655,15.949492807175,3.31883138145111));
#86293=CARTESIAN_POINT('Ctrl Pts',(-11.4493305376893,15.94817231534,3.29548105321944));
#86294=CARTESIAN_POINT('Ctrl Pts',(-11.4444430278596,15.9464349894388,3.26446191623883));
#86295=CARTESIAN_POINT('Ctrl Pts',(-11.4431590851417,15.9460027149928,3.2567188704753));
#86296=CARTESIAN_POINT('Ctrl Pts',(-11.4408759777639,15.9452728985708,3.24360478451572));
#86297=CARTESIAN_POINT('Ctrl Pts',(-11.4399089253907,15.9449743550825,3.23822838668932));
#86298=CARTESIAN_POINT('Ctrl Pts',(-11.4380600356207,15.9444225574881,3.22826969776994));
#86299=CARTESIAN_POINT('Ctrl Pts',(-11.4371863438578,15.9441690501085,3.22368598129795));
#86300=CARTESIAN_POINT('Ctrl Pts',(-11.4353318059959,15.9436455428288,3.21420318655391));
#86301=CARTESIAN_POINT('Ctrl Pts',(-11.4343477638558,15.9433756477469,3.20930479010235));
#86302=CARTESIAN_POINT('Ctrl Pts',(-11.4320537526297,15.9427638936236,3.19818089726335));
#86303=CARTESIAN_POINT('Ctrl Pts',(-11.4307282314604,15.9424225321171,3.19195868678954));
#86304=CARTESIAN_POINT('Ctrl Pts',(-11.4271895258137,15.9415415427226,3.17586317207036));
#86305=CARTESIAN_POINT('Ctrl Pts',(-11.424914427742,15.9410038811709,3.16600373315612));
#86306=CARTESIAN_POINT('Ctrl Pts',(-11.4088297519592,15.9373871195153,3.09945645373874));
#86307=CARTESIAN_POINT('Ctrl Pts',(-11.3917424850724,15.9344153251949,3.04361171257661));
#86308=CARTESIAN_POINT('Ctrl Pts',(-11.3578169515657,15.9295801403371,2.95257833349419));
#86309=CARTESIAN_POINT('Ctrl Pts',(-11.3428286530943,15.9276802664013,2.91677730844212));
#86310=CARTESIAN_POINT('Ctrl Pts',(-11.3093019978364,15.9238144313663,2.8448628590834));
#86311=CARTESIAN_POINT('Ctrl Pts',(-11.2906490496529,15.9218510559634,2.80884055088164));
#86312=CARTESIAN_POINT('Ctrl Pts',(-11.2451776863909,15.9173713458771,2.72930361279366));
#86313=CARTESIAN_POINT('Ctrl Pts',(-11.2175290223151,15.9148470324123,2.686327594106));
#86314=CARTESIAN_POINT('Ctrl Pts',(-11.1734834653787,15.9109704456013,2.62515130329857));
#86315=CARTESIAN_POINT('Ctrl Pts',(-11.1587848611077,15.9096972211357,2.60577341015681));
#86316=CARTESIAN_POINT('Ctrl Pts',(-11.1401405818136,15.9080944848471,2.58242567694317));
#86317=CARTESIAN_POINT('Ctrl Pts',(-11.136645254541,15.9077945179989,2.57809938281918));
#86318=CARTESIAN_POINT('Ctrl Pts',(-11.1311078783804,15.9073199075609,2.57132493294089));
#86319=CARTESIAN_POINT('Ctrl Pts',(-11.1290823085488,15.9071464204813,2.56886330067195));
#86320=CARTESIAN_POINT('Ctrl Pts',(-11.1252641384612,15.9068195922635,2.56425393675488));
#86321=CARTESIAN_POINT('Ctrl Pts',(-11.1234734142915,15.9066663842771,2.56210471633554));
#86322=CARTESIAN_POINT('Ctrl Pts',(-11.1193731955624,15.9063157656869,2.55721224114234));
#86323=CARTESIAN_POINT('Ctrl Pts',(-11.1170597755381,15.9061180735414,2.55447233435166));
#86324=CARTESIAN_POINT('Ctrl Pts',(-11.1109015035602,15.9055922390507,2.54723290984417));
#86325=CARTESIAN_POINT('Ctrl Pts',(-11.1070394269122,15.905262896463,2.54274821309016));
#86326=CARTESIAN_POINT('Ctrl Pts',(-11.0796365625771,15.9029298540553,2.5113152563544));
#86327=CARTESIAN_POINT('Ctrl Pts',(-11.0551432960583,15.9008641439903,2.48521684638434));
#86328=CARTESIAN_POINT('Ctrl Pts',(-11.0286256443926,15.8986712425415,2.45896017953603));
#86329=CARTESIAN_POINT('Ctrl Pts',(-11.0275290443621,15.8985806323488,2.45787779648239));
#86330=CARTESIAN_POINT('Ctrl Pts',(-10.9598782297139,15.8929954259981,2.3913146389042));
#86331=CARTESIAN_POINT('Ctrl Pts',(-10.8872128595198,15.8872911306016,2.33235142091044));
#86332=CARTESIAN_POINT('Ctrl Pts',(-10.7528600822203,15.8776929951419,2.24316127912962));
#86333=CARTESIAN_POINT('Ctrl Pts',(-10.6937457625153,15.8737373947097,2.20958898227639));
#86334=CARTESIAN_POINT('Ctrl Pts',(-10.6203798978882,15.8691691504059,2.17442771387024));
#86335=CARTESIAN_POINT('Ctrl Pts',(-10.6081727485223,15.8684196027385,2.16878287709968));
#86336=CARTESIAN_POINT('Ctrl Pts',(-10.5860688537917,15.8670810305065,2.15892910173817));
#86337=CARTESIAN_POINT('Ctrl Pts',(-10.5762003501307,15.8664899957783,2.1546595149432));
#86338=CARTESIAN_POINT('Ctrl Pts',(-10.5608730483858,15.8655819890449,2.14822778301719));
#86339=CARTESIAN_POINT('Ctrl Pts',(-10.5554469274014,15.8652624498807,2.1459891376893));
#86340=CARTESIAN_POINT('Ctrl Pts',(-10.5454468052684,15.8646770124106,2.14193363464437));
#86341=CARTESIAN_POINT('Ctrl Pts',(-10.5408768431749,15.8644107927743,2.14010709560459));
#86342=CARTESIAN_POINT('Ctrl Pts',(-10.5308881787346,15.8638317490648,2.13617310706793));
#86343=CARTESIAN_POINT('Ctrl Pts',(-10.5254659420733,15.8635192338782,2.13407482003494));
#86344=CARTESIAN_POINT('Ctrl Pts',(-10.5105878570213,15.8626665910351,2.12841903056188));
#86345=CARTESIAN_POINT('Ctrl Pts',(-10.5011073518067,15.8621286349723,2.12492700401845));
#86346=CARTESIAN_POINT('Ctrl Pts',(-10.452098283955,15.8593742363972,2.1074493008723));
#86347=CARTESIAN_POINT('Ctrl Pts',(-10.412016324378,15.8572107798683,2.09506823084163));
#86348=CARTESIAN_POINT('Ctrl Pts',(-10.2685440591714,15.8497088616215,2.05742025816476));
#86349=CARTESIAN_POINT('Ctrl Pts',(-10.1629989675784,15.8446493263694,2.04171898007317));
#86350=CARTESIAN_POINT('Ctrl Pts',(-9.998198904247,15.8365456077858,2.03533123189213));
#86351=CARTESIAN_POINT('Ctrl Pts',(-9.93963629123927,15.8336194918298,2.03657499629506));
#86352=CARTESIAN_POINT('Ctrl Pts',(-9.87046466678711,15.8299530480189,2.04220327667502));
#86353=CARTESIAN_POINT('Ctrl Pts',(-9.85962804380893,15.8293724589847,2.04320681323338));
#86354=CARTESIAN_POINT('Ctrl Pts',(-9.84465279962538,15.828560341094,2.0447622478619));
#86355=CARTESIAN_POINT('Ctrl Pts',(-9.84050356944017,15.8283342828381,2.04521116457326));
#86356=CARTESIAN_POINT('Ctrl Pts',(-9.83349028378045,15.8279503370411,2.04600031538899));
#86357=CARTESIAN_POINT('Ctrl Pts',(-9.830625175024,15.8277929628939,2.04633128363261));
#86358=CARTESIAN_POINT('Ctrl Pts',(-9.82516233083524,15.8274918736265,2.04697870360727));
#86359=CARTESIAN_POINT('Ctrl Pts',(-9.8225644379796,15.8273482465037,2.04729365684715));
#86360=CARTESIAN_POINT('Ctrl Pts',(-9.81571838593965,15.8269686153677,2.04814226989608));
#86361=CARTESIAN_POINT('Ctrl Pts',(-9.81147173317666,15.8267319693174,2.04868760309712));
#86362=CARTESIAN_POINT('Ctrl Pts',(-9.79655585326278,15.8258968520576,2.05066959393247));
#86363=CARTESIAN_POINT('Ctrl Pts',(-9.78590040412202,15.8252932053556,2.05220529910829));
#86364=CARTESIAN_POINT('Ctrl Pts',(-9.67593669752432,15.8189972581231,2.06929414552402));
#86365=CARTESIAN_POINT('Ctrl Pts',(-9.57847180934187,15.8128756980523,2.09492075553681));
#86366=CARTESIAN_POINT('Ctrl Pts',(-9.46293814267093,15.8054576958196,2.1384115302824));
#86367=CARTESIAN_POINT('Ctrl Pts',(-9.44165941195558,15.8040832986414,2.1469979961773));
#86368=CARTESIAN_POINT('Ctrl Pts',(-9.34602539713028,15.7978822039627,2.18822906870028));
#86369=CARTESIAN_POINT('Ctrl Pts',(-9.27425634679107,15.7931727072006,2.22653020878963));
#86370=CARTESIAN_POINT('Ctrl Pts',(-9.19643616550276,15.7880433249029,2.27678793494339));
#86371=CARTESIAN_POINT('Ctrl Pts',(-9.18691820226508,15.7874153118116,2.28309384388545));
#86372=CARTESIAN_POINT('Ctrl Pts',(-9.17248329593104,15.7864616682631,2.29290233474315));
#86373=CARTESIAN_POINT('Ctrl Pts',(-9.16751275903493,15.7861330669625,2.29632493415501));
#86374=CARTESIAN_POINT('Ctrl Pts',(-9.15848761219643,15.7855359627809,2.30262209327246));
#86375=CARTESIAN_POINT('Ctrl Pts',(-9.15442622108853,15.7852670915221,2.30548673694756));
#86376=CARTESIAN_POINT('Ctrl Pts',(-9.14566292629698,15.7846865421063,2.31173489110296));
#86377=CARTESIAN_POINT('Ctrl Pts',(-9.14096634810732,15.7843751497534,2.31512574896586));
#86378=CARTESIAN_POINT('Ctrl Pts',(-9.12820952531143,15.7835285703457,2.32445169910644));
#86379=CARTESIAN_POINT('Ctrl Pts',(-9.12018975802617,15.7829955032797,2.33044179953527));
#86380=CARTESIAN_POINT('Ctrl Pts',(-9.07986165475805,15.7803096684735,2.36121311616388));
#86381=CARTESIAN_POINT('Ctrl Pts',(-9.04853465282346,15.7782066954236,2.38725374804408));
#86382=CARTESIAN_POINT('Ctrl Pts',(-9.00796215401531,15.7754362564872,2.42394764518034));
#86383=CARTESIAN_POINT('Ctrl Pts',(-8.9977266200889,15.7747329971335,2.43347487479258));
#86384=CARTESIAN_POINT('Ctrl Pts',(-8.89320424434621,15.7674961138958,2.53359804027025));
#86385=CARTESIAN_POINT('Ctrl Pts',(-8.81133853057874,15.7614121856562,2.63628283444366));
#86386=CARTESIAN_POINT('Ctrl Pts',(-8.72921938640003,15.7532528099632,2.77350127820991));
#86387=CARTESIAN_POINT('Ctrl Pts',(-8.71498772646282,15.7517340391825,2.79898146248846));
#86388=CARTESIAN_POINT('Ctrl Pts',(-8.69882054194111,15.7498561243616,2.83007558931542));
#86389=CARTESIAN_POINT('Ctrl Pts',(-8.69614437558332,15.7495398348578,2.83529916019225));
#86390=CARTESIAN_POINT('Ctrl Pts',(-8.6920329564605,15.7490451503653,2.84344454990599));
#86391=CARTESIAN_POINT('Ctrl Pts',(-8.69057587913687,15.7488680801191,2.84635535853742));
#86392=CARTESIAN_POINT('Ctrl Pts',(-8.68788894169534,15.7485382280867,2.85176810250996));
#86393=CARTESIAN_POINT('Ctrl Pts',(-8.68665651284523,15.7483856074345,2.85426870402017));
#86394=CARTESIAN_POINT('Ctrl Pts',(-8.68387306936121,15.7480378900271,2.8599572506615));
#86395=CARTESIAN_POINT('Ctrl Pts',(-8.68232649555938,15.7478425257776,2.86314730613535));
#86396=CARTESIAN_POINT('Ctrl Pts',(-8.67764637786537,15.7472447653868,2.87289082668586));
#86397=CARTESIAN_POINT('Ctrl Pts',(-8.67455007117627,15.7468401867075,2.87946192786984));
#86398=CARTESIAN_POINT('Ctrl Pts',(-8.6420825631744,15.7425014250007,2.94971746834774));
#86399=CARTESIAN_POINT('Ctrl Pts',(-8.61727924527846,15.7383338052031,3.01540542703653));
#86400=CARTESIAN_POINT('Ctrl Pts',(-8.56926998273027,15.7282226414929,3.17674960448337));
#86401=CARTESIAN_POINT('Ctrl Pts',(-8.55080292236035,15.7222761674507,3.27348119612623));
#86402=CARTESIAN_POINT('Ctrl Pts',(-8.53827691825814,15.7140364184731,3.41541070628096));
#86403=CARTESIAN_POINT('Ctrl Pts',(-8.53638758214428,15.7115318489563,3.459639220784));
#86404=CARTESIAN_POINT('Ctrl Pts',(-8.53653154490704,15.7085410112187,3.51381550444179));
#86405=CARTESIAN_POINT('Ctrl Pts',(-8.53665891683797,15.7079961426061,3.52374170104145));
#86406=CARTESIAN_POINT('Ctrl Pts',(-8.53701874578127,15.7071425046438,3.53937973832679));
#86407=CARTESIAN_POINT('Ctrl Pts',(-8.53718368776214,15.7068316512991,3.54509270374045));
#86408=CARTESIAN_POINT('Ctrl Pts',(-8.53755480722251,15.706252137337,3.5557768902552));
#86409=CARTESIAN_POINT('Ctrl Pts',(-8.53775287697131,15.7059832292774,3.56074829549104));
#86410=CARTESIAN_POINT('Ctrl Pts',(-8.53825167439652,15.7053846242354,3.57184489901904));
#86411=CARTESIAN_POINT('Ctrl Pts',(-8.53856555871815,15.7050553403103,3.57796943195846));
#86412=CARTESIAN_POINT('Ctrl Pts',(-8.53945622958422,15.7042260163666,3.59344468708322));
#86413=CARTESIAN_POINT('Ctrl Pts',(-8.54008432683518,15.7037275712682,3.60279225428986));
#86414=CARTESIAN_POINT('Ctrl Pts',(-8.54421004905313,15.7008782099779,3.6564805458821));
#86415=CARTESIAN_POINT('Ctrl Pts',(-8.54963799199644,15.6985878862357,3.70065164209107));
#86416=CARTESIAN_POINT('Ctrl Pts',(-8.58042128618632,15.6892946397258,3.88231352972219));
#86417=CARTESIAN_POINT('Ctrl Pts',(-8.62338799325155,15.6828257351684,4.01604217549472));
#86418=CARTESIAN_POINT('Ctrl Pts',(-8.69775304316821,15.67418039309,4.16848909254152));
#86419=CARTESIAN_POINT('Ctrl Pts',(-8.71166958822675,15.6726267268869,4.19493115536883));
#86420=CARTESIAN_POINT('Ctrl Pts',(-8.72929477232807,15.6707097584033,4.22606843950203));
#86421=CARTESIAN_POINT('Ctrl Pts',(-8.73223613823896,15.6703914120714,4.2311921381551));
#86422=CARTESIAN_POINT('Ctrl Pts',(-8.73685031861745,15.669894200767,4.23911824714436));
#86423=CARTESIAN_POINT('Ctrl Pts',(-8.73850165447372,15.6697166824403,4.24193316723761));
#86424=CARTESIAN_POINT('Ctrl Pts',(-8.74158062575843,15.6693864328612,4.24714168401531));
#86425=CARTESIAN_POINT('Ctrl Pts',(-8.74300569057353,15.6692338661648,4.24953673902448));
#86426=CARTESIAN_POINT('Ctrl Pts',(-8.74625320548167,15.6688868386015,4.2549594114311));
#86427=CARTESIAN_POINT('Ctrl Pts',(-8.74807977706318,15.6686921146338,4.25798449359756));
#86428=CARTESIAN_POINT('Ctrl Pts',(-8.75366458833495,15.6680982076117,4.26715854031814));
#86429=CARTESIAN_POINT('Ctrl Pts',(-8.75745724829173,15.6676968819776,4.27328629251207));
#86430=CARTESIAN_POINT('Ctrl Pts',(-8.79269555816046,15.663988039685,4.32929177949537));
#86431=CARTESIAN_POINT('Ctrl Pts',(-8.82708051377024,15.6605146009096,4.37724987258664));
#86432=CARTESIAN_POINT('Ctrl Pts',(-8.90792462825394,15.65284891439,4.47672775812324));
#86433=CARTESIAN_POINT('Ctrl Pts',(-8.9553488470132,15.6486486352057,4.52729259636271));
#86434=CARTESIAN_POINT('Ctrl Pts',(-9.06058626698526,15.6401093348475,4.62464592604532));
#86435=CARTESIAN_POINT('Ctrl Pts',(-9.11874923704675,15.6357952075521,4.67078018011592));
#86436=CARTESIAN_POINT('Ctrl Pts',(-9.19380005005272,15.6307346876338,4.72153380011897));
#86437=CARTESIAN_POINT('Ctrl Pts',(-9.20758996838148,15.6298238015158,4.73052409851194));
#86438=CARTESIAN_POINT('Ctrl Pts',(-9.22744690372434,15.628538410048,4.74299750751416));
#86439=CARTESIAN_POINT('Ctrl Pts',(-9.23339139889537,15.6281568898385,4.74667250925717));
#86440=CARTESIAN_POINT('Ctrl Pts',(-9.24371087512879,15.6275001662113,4.75295048634648));
#86441=CARTESIAN_POINT('Ctrl Pts',(-9.2480734976975,15.6272242387452,4.75557345371734));
#86442=CARTESIAN_POINT('Ctrl Pts',(-9.25646864039173,15.6266964931476,4.7605614703379));
#86443=CARTESIAN_POINT('Ctrl Pts',(-9.26049897486578,15.6264445493617,4.76293006051219));
#86444=CARTESIAN_POINT('Ctrl Pts',(-9.2710495673999,15.6257886593534,4.76906272396085));
#86445=CARTESIAN_POINT('Ctrl Pts',(-9.27758769070849,15.6253858234389,4.772795894396));
#86446=CARTESIAN_POINT('Ctrl Pts',(-9.30025764662855,15.624001229463,4.78550914255081));
#86447=CARTESIAN_POINT('Ctrl Pts',(-9.3165307659428,15.6230284784064,4.79423450852946));
#86448=CARTESIAN_POINT('Ctrl Pts',(-9.44652115950057,15.6154132737831,4.86079738618215));
#86449=CARTESIAN_POINT('Ctrl Pts',(-9.56718702467038,15.6093343751655,4.90384570117857));
#86450=CARTESIAN_POINT('Ctrl Pts',(-9.74106357654327,15.6006332533548,4.94128835746997));
#86451=CARTESIAN_POINT('Ctrl Pts',(-9.79072531439699,15.5981458523097,4.94933213674936));
#86452=CARTESIAN_POINT('Ctrl Pts',(-9.86464256444154,15.5943203931647,4.95742608584392));
#86453=CARTESIAN_POINT('Ctrl Pts',(-9.88864611261351,15.5930589774026,4.95945627174356));
#86454=CARTESIAN_POINT('Ctrl Pts',(-9.91822290140941,15.5914695019034,4.96122397583003));
#86455=CARTESIAN_POINT('Ctrl Pts',(-9.92376016404684,15.5911704115556,4.96152334460419));
#86456=CARTESIAN_POINT('Ctrl Pts',(-9.93247945188097,15.5906968799903,4.96194506228082));
#86457=CARTESIAN_POINT('Ctrl Pts',(-9.93566046174225,15.5905235865287,4.96208851064688));
#86458=CARTESIAN_POINT('Ctrl Pts',(-9.94163765026828,15.5901969129296,4.96233850941591));
#86459=CARTESIAN_POINT('Ctrl Pts',(-9.94443367996392,15.5900436643959,4.96244742251341));
#86460=CARTESIAN_POINT('Ctrl Pts',(-9.95081944450417,15.5896926813833,4.96267782642178));
#86461=CARTESIAN_POINT('Ctrl Pts',(-9.95440932271794,15.5894946631836,4.96279412103113));
#86462=CARTESIAN_POINT('Ctrl Pts',(-9.96393536875779,15.5889673968527,4.96306761816576));
#86463=CARTESIAN_POINT('Ctrl Pts',(-9.96987206483511,15.5886369382967,4.96320190610689));
#86464=CARTESIAN_POINT('Ctrl Pts',(-10.0121984731203,15.5862684104015,4.96390162932665));
#86465=CARTESIAN_POINT('Ctrl Pts',(-10.0485946349193,15.5841661930598,4.9631455567877));
#86466=CARTESIAN_POINT('Ctrl Pts',(-10.0972051187587,15.5813030802851,4.96032010489185));
#86467=CARTESIAN_POINT('Ctrl Pts',(-10.109478904138,15.5805753972936,4.95945126767905));
#86468=CARTESIAN_POINT('Ctrl Pts',(-10.2112193692979,15.574510864254,4.95095863657535));
#86469=CARTESIAN_POINT('Ctrl Pts',(-10.2998223154583,15.5690352706318,4.93527077762637));
#86470=CARTESIAN_POINT('Ctrl Pts',(-10.450266348908,15.5597943973382,4.89408490209033));
#86471=CARTESIAN_POINT('Ctrl Pts',(-10.5128477234004,15.5559650170763,4.87229790641708));
#86472=CARTESIAN_POINT('Ctrl Pts',(-10.588027787757,15.551407305756,4.84025989483278));
#86473=CARTESIAN_POINT('Ctrl Pts',(-10.6022123035343,15.5505490530019,4.8339466377807));
#86474=CARTESIAN_POINT('Ctrl Pts',(-10.622485995773,15.5493244021479,4.82453389515986));
#86475=CARTESIAN_POINT('Ctrl Pts',(-10.6286577948156,15.5489518617864,4.8216157662461));
#86476=CARTESIAN_POINT('Ctrl Pts',(-10.6393704267743,15.548305645153,4.81645863425174));
#86477=CARTESIAN_POINT('Ctrl Pts',(-10.6439204444234,15.548031306755,4.8142390728015));
#86478=CARTESIAN_POINT('Ctrl Pts',(-10.6526840809335,15.5475031353315,4.80990761268122));
#86479=CARTESIAN_POINT('Ctrl Pts',(-10.656899188971,15.5472491971318,4.80779888343309));
#86480=CARTESIAN_POINT('Ctrl Pts',(-10.6680054172211,15.5465803298333,4.80217543051707));
#86481=CARTESIAN_POINT('Ctrl Pts',(-10.6748790368415,15.5461665998545,4.79862634272655));
#86482=CARTESIAN_POINT('Ctrl Pts',(-10.6991563963623,15.5447058687563,4.78584628620261));
#86483=CARTESIAN_POINT('Ctrl Pts',(-10.7164019496999,15.5436692704866,4.77631839031584));
#86484=CARTESIAN_POINT('Ctrl Pts',(-10.8426883036775,15.5360741976743,4.70318075718056));
#86485=CARTESIAN_POINT('Ctrl Pts',(-10.9432777160316,15.5300605192592,4.62605329344906));
#86486=CARTESIAN_POINT('Ctrl Pts',(-11.0681557927213,15.5214370382806,4.50168644538353));
#86487=CARTESIAN_POINT('Ctrl Pts',(-11.1017517380528,15.5189625191717,4.46461131243999));
#86488=CARTESIAN_POINT('Ctrl Pts',(-11.1485692807684,15.5151549232385,4.40730210538272));
#86489=CARTESIAN_POINT('Ctrl Pts',(-11.1632958109638,15.5138976571113,4.38834184125282));
#86490=CARTESIAN_POINT('Ctrl Pts',(-11.1808379498359,15.5123128423391,4.36457195935395));
#86491=CARTESIAN_POINT('Ctrl Pts',(-11.184101962443,15.5120140622116,4.36009620231301));
#86492=CARTESIAN_POINT('Ctrl Pts',(-11.1892012894379,15.511540912511,4.35301973866309));
#86493=CARTESIAN_POINT('Ctrl Pts',(-11.1910536976845,15.5113676876021,4.35043134360479));
#86494=CARTESIAN_POINT('Ctrl Pts',(-11.1945188348553,15.5110410685088,4.34555593223225));
#86495=CARTESIAN_POINT('Ctrl Pts',(-11.1961334560194,15.5108878053789,4.34327032219734));
#86496=CARTESIAN_POINT('Ctrl Pts',(-11.1998066678057,15.5105366922791,4.33803885693779));
#86497=CARTESIAN_POINT('Ctrl Pts',(-11.2018609677618,15.5103385578114,4.3350900427211));
#86498=CARTESIAN_POINT('Ctrl Pts',(-11.2072848170796,15.5098107805893,4.32724299162193));
#86499=CARTESIAN_POINT('Ctrl Pts',(-11.2106353797506,15.5094799237671,4.32233178923502));
#86500=CARTESIAN_POINT('Ctrl Pts',(-11.2343754024269,15.507101677208,4.28707447836635));
#86501=CARTESIAN_POINT('Ctrl Pts',(-11.2536498382057,15.504989558406,4.25599637727083));
#86502=CARTESIAN_POINT('Ctrl Pts',(-11.3168208868424,15.4974822733556,4.14506910678062));
#86503=CARTESIAN_POINT('Ctrl Pts',(-11.3544123653171,15.4919203340701,4.06187075066631));
#86504=CARTESIAN_POINT('Ctrl Pts',(-11.4111113944972,15.4815221562677,3.8969137613648));
#86505=CARTESIAN_POINT('Ctrl Pts',(-11.4314211491093,15.4766826516192,3.81593204748348));
#86506=CARTESIAN_POINT('Ctrl Pts',(-11.4465582022554,15.4714323971834,3.7223353357576));
#86507=CARTESIAN_POINT('Ctrl Pts',(-11.4482552171472,15.470801840148,3.71099874538706));
#86508=CARTESIAN_POINT('Ctrl Pts',(-11.4506434433598,15.4698451534468,3.69365532327172));
#86509=CARTESIAN_POINT('Ctrl Pts',(-11.4514308860396,15.4695160236494,3.68766237922612));
#86510=CARTESIAN_POINT('Ctrl Pts',(-11.452798157936,15.4689183658172,3.67673275499461));
#86511=CARTESIAN_POINT('Ctrl Pts',(-11.4533900055018,15.4686494658813,3.67179769248364));
#86512=CARTESIAN_POINT('Ctrl Pts',(-11.4546162371738,15.4680693105584,3.66111273916939));
#86513=CARTESIAN_POINT('Ctrl Pts',(-11.4552416964148,15.4677583379078,3.65536189528));
#86514=CARTESIAN_POINT('Ctrl Pts',(-11.4568527151101,15.4669140224848,3.63968503918302));
#86515=CARTESIAN_POINT('Ctrl Pts',(-11.4577709306515,15.4663827805759,3.62975231805008));
#86516=CARTESIAN_POINT('Ctrl Pts',(-11.4618609702844,15.4637373491525,3.57995981190155));
#86517=CARTESIAN_POINT('Ctrl Pts',(-11.4634999999999,15.4616710633252,3.53998959100317));
#86518=CARTESIAN_POINT('Ctrl Pts',(-11.4635,15.4596442608852,3.50000000000481));
#86519=CARTESIAN_POINT('Ctrl Pts',(-11.4635,15.3905155741067,3.49999999999573));
#86520=CARTESIAN_POINT('Ctrl Pts',(-11.4635,15.3924479265974,3.53377287519692));
#86521=CARTESIAN_POINT('Ctrl Pts',(-11.4623309559757,15.3943469930721,3.56753745619958));
#86522=CARTESIAN_POINT('Ctrl Pts',(-11.4593343437384,15.3967366095462,3.61075474225848));
#86523=CARTESIAN_POINT('Ctrl Pts',(-11.4585810250861,15.3972601693145,3.62026944362245));
#86524=CARTESIAN_POINT('Ctrl Pts',(-11.4572352147539,15.3980880983137,3.63538649531933));
#86525=CARTESIAN_POINT('Ctrl Pts',(-11.4567033698223,15.3983943456444,3.64099385738379));
#86526=CARTESIAN_POINT('Ctrl Pts',(-11.4556895848887,15.398942808918,3.65106364886));
#86527=CARTESIAN_POINT('Ctrl Pts',(-11.4552194652323,15.3991853897264,3.65552717508704));
#86528=CARTESIAN_POINT('Ctrl Pts',(-11.4540705446105,15.3997519316809,3.66597397536798));
#86529=CARTESIAN_POINT('Ctrl Pts',(-11.4533753318413,15.4000753767965,3.67195538805569));
#86530=CARTESIAN_POINT('Ctrl Pts',(-11.4512635768085,15.4010050542376,3.68919579279601));
#86531=CARTESIAN_POINT('Ctrl Pts',(-11.4497529607197,15.4016083459921,3.70044295928912));
#86532=CARTESIAN_POINT('Ctrl Pts',(-11.4368121949794,15.406333954281,3.7889747726702));
#86533=CARTESIAN_POINT('Ctrl Pts',(-11.4193406955769,15.4102562796685,3.86525297622746));
#86534=CARTESIAN_POINT('Ctrl Pts',(-11.3638911721045,15.4193170126255,4.041249878645));
#86535=CARTESIAN_POINT('Ctrl Pts',(-11.3209561715124,15.4243479523232,4.13892219510135));
#86536=CARTESIAN_POINT('Ctrl Pts',(-11.2540427537917,15.4311945194401,4.25496342070717));
#86537=CARTESIAN_POINT('Ctrl Pts',(-11.239592920001,15.4326315102702,4.27846142762621));
#86538=CARTESIAN_POINT('Ctrl Pts',(-11.2214889166481,15.4344015119695,4.30611852669048));
#86539=CARTESIAN_POINT('Ctrl Pts',(-11.2184633412356,15.4346963623763,4.31068448655606));
#86540=CARTESIAN_POINT('Ctrl Pts',(-11.2134670953802,15.4351818928509,4.31813327277118));
#86541=CARTESIAN_POINT('Ctrl Pts',(-11.2115115850846,15.4353715910389,4.32102626162252));
#86542=CARTESIAN_POINT('Ctrl Pts',(-11.2079777548484,15.4357138482009,4.32621410738476));
#86543=CARTESIAN_POINT('Ctrl Pts',(-11.2064032212908,15.435866153749,4.32851148146362));
#86544=CARTESIAN_POINT('Ctrl Pts',(-11.2029497958787,15.4361998010226,4.33351959580938));
#86545=CARTESIAN_POINT('Ctrl Pts',(-11.2010683191604,15.4363813130443,4.33622844980883));
#86546=CARTESIAN_POINT('Ctrl Pts',(-11.1957008974664,15.4368983250465,4.34390070573417));
#86547=CARTESIAN_POINT('Ctrl Pts',(-11.1921932740865,15.4372352449728,4.34884876859077));
#86548=CARTESIAN_POINT('Ctrl Pts',(-11.1694627667194,15.4394117895475,4.3804949739973));
#86549=CARTESIAN_POINT('Ctrl Pts',(-11.1493763375795,15.4413041163679,4.40655847569105));
#86550=CARTESIAN_POINT('Ctrl Pts',(-11.075710044139,15.4480767624132,4.49575841135937));
#86551=CARTESIAN_POINT('Ctrl Pts',(-11.0176691443843,15.4531145791447,4.55500516851086));
#86552=CARTESIAN_POINT('Ctrl Pts',(-10.8825252638254,15.4638053838747,4.67137149085821));
#86553=CARTESIAN_POINT('Ctrl Pts',(-10.804177403668,15.469400059251,4.72648527052344));
#86554=CARTESIAN_POINT('Ctrl Pts',(-10.71171615676,15.4752880042463,4.77883003245339));
#86555=CARTESIAN_POINT('Ctrl Pts',(-10.702371809612,15.475875792682,4.78398597704378));
#86556=CARTESIAN_POINT('Ctrl Pts',(-10.6872828738873,15.4768135090254,4.79209760358683));
#86557=CARTESIAN_POINT('Ctrl Pts',(-10.6815737793313,15.4771657157405,4.79511819967667));
#86558=CARTESIAN_POINT('Ctrl Pts',(-10.6713885960845,15.4777895262364,4.80042102555505));
#86559=CARTESIAN_POINT('Ctrl Pts',(-10.6669204265679,15.4780616493522,4.80271817219173));
#86560=CARTESIAN_POINT('Ctrl Pts',(-10.6575695297175,15.4786279755011,4.80746487655657));
#86561=CARTESIAN_POINT('Ctrl Pts',(-10.6526847320212,15.4789220281408,4.80991019980008));
#86562=CARTESIAN_POINT('Ctrl Pts',(-10.6399178175918,15.4796859766753,4.81621215444183));
#86563=CARTESIAN_POINT('Ctrl Pts',(-10.6320144393242,15.4801543697673,4.82002537921713));
#86564=CARTESIAN_POINT('Ctrl Pts',(-10.5968783948047,15.4822172516288,4.83658992258273));
#86565=CARTESIAN_POINT('Ctrl Pts',(-10.5692898427104,15.4837854256293,4.84857171850007));
#86566=CARTESIAN_POINT('Ctrl Pts',(-10.4934484355024,15.4879757278688,4.87876728120516));
#86567=CARTESIAN_POINT('Ctrl Pts',(-10.444569961316,15.4905461529664,4.895295191772));
#86568=CARTESIAN_POINT('Ctrl Pts',(-10.2969866506334,15.4980769237978,4.9366541124906));
#86569=CARTESIAN_POINT('Ctrl Pts',(-10.1964688735872,15.5028957923717,4.95381334171361));
#86570=CARTESIAN_POINT('Ctrl Pts',(-10.0622136362668,15.5097181210195,4.96254597188032));
#86571=CARTESIAN_POINT('Ctrl Pts',(-10.029374494844,15.5114188551345,4.96357373684852));
#86572=CARTESIAN_POINT('Ctrl Pts',(-9.99076287140086,15.513484179312,4.9634822165618));
#86573=CARTESIAN_POINT('Ctrl Pts',(-9.98499486145552,15.5137944321807,4.96343444211142));
#86574=CARTESIAN_POINT('Ctrl Pts',(-9.97564757487826,15.5143002157791,4.96330175527143));
#86575=CARTESIAN_POINT('Ctrl Pts',(-9.97206800674776,15.5144946217253,4.96323780390823));
#86576=CARTESIAN_POINT('Ctrl Pts',(-9.96569774405163,15.5148419181339,4.96310061122072));
#86577=CARTESIAN_POINT('Ctrl Pts',(-9.96290698694573,15.5149945217354,4.96303251896967));
#86578=CARTESIAN_POINT('Ctrl Pts',(-9.95688505362365,15.5153248107346,4.96286834702902));
#86579=CARTESIAN_POINT('Ctrl Pts',(-9.95365404315212,15.5155026395728,4.96276954822251));
#86580=CARTESIAN_POINT('Ctrl Pts',(-9.94466440782513,15.5159990746492,4.96246484626167));
#86581=CARTESIAN_POINT('Ctrl Pts',(-9.93890669713507,15.516318931364,4.96223563778122));
#86582=CARTESIAN_POINT('Ctrl Pts',(-9.90583520968154,15.5181664669529,4.96072342770647));
#86583=CARTESIAN_POINT('Ctrl Pts',(-9.8785619372936,15.5197304924079,4.95870920324859));
#86584=CARTESIAN_POINT('Ctrl Pts',(-9.78946400237685,15.524938313691,4.94961314248932));
#86585=CARTESIAN_POINT('Ctrl Pts',(-9.72803416839514,15.528682294912,4.93935313746615));
#86586=CARTESIAN_POINT('Ctrl Pts',(-9.55605141058428,15.5393178488581,4.89922355911073));
#86587=CARTESIAN_POINT('Ctrl Pts',(-9.44806758836559,15.5461457541195,4.86025589123931));
#86588=CARTESIAN_POINT('Ctrl Pts',(-9.33077783421074,15.5534764736581,4.80163464799671));
#86589=CARTESIAN_POINT('Ctrl Pts',(-9.31597017330557,15.5544012729764,4.79391432973713));
#86590=CARTESIAN_POINT('Ctrl Pts',(-9.29557609920256,15.5556744198301,4.7828334323548));
#86591=CARTESIAN_POINT('Ctrl Pts',(-9.28987551343262,15.5560302344369,4.77968662674915));
#86592=CARTESIAN_POINT('Ctrl Pts',(-9.28007552885593,15.5566418724905,4.77419124288742));
#86593=CARTESIAN_POINT('Ctrl Pts',(-9.275966183373,15.5568983305095,4.77186068447477));
#86594=CARTESIAN_POINT('Ctrl Pts',(-9.26748039705959,15.5574279114339,4.76699363342391));
#86595=CARTESIAN_POINT('Ctrl Pts',(-9.26310567267965,15.5577009269031,4.7644542645264));
#86596=CARTESIAN_POINT('Ctrl Pts',(-9.25288692263474,15.5583386904326,4.75845160609522));
#86597=CARTESIAN_POINT('Ctrl Pts',(-9.24705364275756,15.5587027803744,4.75497019107539));
#86598=CARTESIAN_POINT('Ctrl Pts',(-9.22813877838497,15.5598836274135,4.74350207582798));
#86599=CARTESIAN_POINT('Ctrl Pts',(-9.21515813779132,15.5606943945906,4.73535032794443));
#86600=CARTESIAN_POINT('Ctrl Pts',(-9.14818165004608,15.5648834933773,4.69180769531754));
#86601=CARTESIAN_POINT('Ctrl Pts',(-9.09644055774671,15.5681351977014,4.65307486203232));
#86602=CARTESIAN_POINT('Ctrl Pts',(-8.97104608087096,15.5762814416564,4.54556556398651));
#86603=CARTESIAN_POINT('Ctrl Pts',(-8.90163085381228,15.5810477380525,4.47238705418304));
#86604=CARTESIAN_POINT('Ctrl Pts',(-8.8161201283604,15.588093134494,4.3612947554924));
#86605=CARTESIAN_POINT('Ctrl Pts',(-8.79325274604905,15.5901275494179,4.32895159931876));
#86606=CARTESIAN_POINT('Ctrl Pts',(-8.76842762291223,15.5925672241003,4.29063173842885));
#86607=CARTESIAN_POINT('Ctrl Pts',(-8.76516034514825,15.5928933171649,4.28551899409216));
#86608=CARTESIAN_POINT('Ctrl Pts',(-8.75998919636404,15.5934177458523,4.2773150173647));
#86609=CARTESIAN_POINT('Ctrl Pts',(-8.75806483644245,15.5936147851654,4.27423670688957));
#86610=CARTESIAN_POINT('Ctrl Pts',(-8.75467460677688,15.5939653306117,4.26876835006387));
#86611=CARTESIAN_POINT('Ctrl Pts',(-8.75320412777754,15.5941185333728,4.26638121322627));
#86612=CARTESIAN_POINT('Ctrl Pts',(-8.75008932403682,15.5944455449542,4.26129203105642));
#86613=CARTESIAN_POINT('Ctrl Pts',(-8.74844692272374,15.5946194678516,4.25858891951134));
#86614=CARTESIAN_POINT('Ctrl Pts',(-8.74400053585063,15.5950943599629,4.25121718204668));
#86615=CARTESIAN_POINT('Ctrl Pts',(-8.74121385538734,15.5953964125454,4.24653824333437));
#86616=CARTESIAN_POINT('Ctrl Pts',(-8.72693573011277,15.5969666892207,4.22225750245936));
#86617=CARTESIAN_POINT('Ctrl Pts',(-8.71587640171128,15.5982598931284,4.20240657852535));
#86618=CARTESIAN_POINT('Ctrl Pts',(-8.68393366634153,15.6022183756158,4.14179349206602));
#86619=CARTESIAN_POINT('Ctrl Pts',(-8.664497682262,15.6049404550471,4.100302032205));
#86620=CARTESIAN_POINT('Ctrl Pts',(-8.62396026863709,15.6113170174828,4.00200742882423));
#86621=CARTESIAN_POINT('Ctrl Pts',(-8.60437453957507,15.6149819432937,3.94466464749764));
#86622=CARTESIAN_POINT('Ctrl Pts',(-8.56644434643042,15.6235512380044,3.80605199561006));
#86623=CARTESIAN_POINT('Ctrl Pts',(-8.55136816441418,15.6283846408657,3.72409612057871));
#86624=CARTESIAN_POINT('Ctrl Pts',(-8.54230231722548,15.6335888365207,3.63063094936023));
#86625=CARTESIAN_POINT('Ctrl Pts',(-8.54138527165353,15.6341788230113,3.61995858504686));
#86626=CARTESIAN_POINT('Ctrl Pts',(-8.54010233182435,15.6351193544361,3.60282467234005));
#86627=CARTESIAN_POINT('Ctrl Pts',(-8.53966199526193,15.635472199962,3.59636923049541));
#86628=CARTESIAN_POINT('Ctrl Pts',(-8.53895572271467,15.6360967430292,3.5848948022735));
#86629=CARTESIAN_POINT('Ctrl Pts',(-8.53867280400491,15.6363689640888,3.57987699769955));
#86630=CARTESIAN_POINT('Ctrl Pts',(-8.53813660442161,15.6369350998103,3.56940780191909));
#86631=CARTESIAN_POINT('Ctrl Pts',(-8.53788795564795,15.6372288665142,3.56395624417164));
#86632=CARTESIAN_POINT('Ctrl Pts',(-8.53732001545623,15.6379912173924,3.54976020611194));
#86633=CARTESIAN_POINT('Ctrl Pts',(-8.53704864221797,15.6384583106285,3.54101395546865));
#86634=CARTESIAN_POINT('Ctrl Pts',(-8.53619814278807,15.6405070733441,3.50244653962598));
#86635=CARTESIAN_POINT('Ctrl Pts',(-8.53645226202916,15.642062880952,3.47261308286535));
#86636=CARTESIAN_POINT('Ctrl Pts',(-8.53960900223283,15.6462106101044,3.39189791822188));
#86637=CARTESIAN_POINT('Ctrl Pts',(-8.54425711986274,15.6487522018452,3.34112543266745));
#86638=CARTESIAN_POINT('Ctrl Pts',(-8.56406109833577,15.6555595437033,3.20407496090257));
#86639=CARTESIAN_POINT('Ctrl Pts',(-8.58432221753983,15.6597325453229,3.11875539523684));
#86640=CARTESIAN_POINT('Ctrl Pts',(-8.61552706984217,15.664635148724,3.02546354358181));
#86641=CARTESIAN_POINT('Ctrl Pts',(-8.61908574053981,15.6651791804299,3.01520525611983));
#86642=CARTESIAN_POINT('Ctrl Pts',(-8.63517257446305,15.66757819518,2.97044786416266));
#86643=CARTESIAN_POINT('Ctrl Pts',(-8.64888097643546,15.6694700723622,2.93638991456549));
#86644=CARTESIAN_POINT('Ctrl Pts',(-8.66628237545294,15.6717499116966,2.89745126097008));
#86645=CARTESIAN_POINT('Ctrl Pts',(-8.66874420616607,15.6720699277985,2.89203150253327));
#86646=CARTESIAN_POINT('Ctrl Pts',(-8.67274640548649,15.6725864221828,2.88336146576302));
#86647=CARTESIAN_POINT('Ctrl Pts',(-8.67426583702232,15.6727816653516,2.88010152879236));
#86648=CARTESIAN_POINT('Ctrl Pts',(-8.67698930800257,15.6731301932463,2.87431413907305));
#86649=CARTESIAN_POINT('Ctrl Pts',(-8.67818860014775,15.6732831870255,2.87178450287929));
#86650=CARTESIAN_POINT('Ctrl Pts',(-8.6807670514305,15.6736111148596,2.86638591400915));
#86651=CARTESIAN_POINT('Ctrl Pts',(-8.68214829265891,15.6737861716274,2.86351806025893));
#86652=CARTESIAN_POINT('Ctrl Pts',(-8.68595792046577,15.6742672926443,2.85567374288215));
#86653=CARTESIAN_POINT('Ctrl Pts',(-8.68840518630778,15.6745744875118,2.85070657243267));
#86654=CARTESIAN_POINT('Ctrl Pts',(-8.70159037638528,15.6762192293733,2.82432356741786));
#86655=CARTESIAN_POINT('Ctrl Pts',(-8.71282418329001,15.6775845926265,2.80316108573879));
#86656=CARTESIAN_POINT('Ctrl Pts',(-8.74901075838211,15.6818554277292,2.73885506361895));
#86657=CARTESIAN_POINT('Ctrl Pts',(-8.77565088384762,15.6848275664704,2.69670407498942));
#86658=CARTESIAN_POINT('Ctrl Pts',(-8.87668053444641,15.6953525156578,2.55358571325118));
#86659=CARTESIAN_POINT('Ctrl Pts',(-8.96184800919518,15.7029216242198,2.46086687780801));
#86660=CARTESIAN_POINT('Ctrl Pts',(-9.07348741503224,15.7111253482019,2.36693918181937));
#86661=CARTESIAN_POINT('Ctrl Pts',(-9.08944786051499,15.7122649183693,2.35407362846749));
#86662=CARTESIAN_POINT('Ctrl Pts',(-9.1118960180913,15.713823116112,2.3367436415362));
#86663=CARTESIAN_POINT('Ctrl Pts',(-9.11815681938413,15.7142530423524,2.33199030553167));
#86664=CARTESIAN_POINT('Ctrl Pts',(-9.12825215470888,15.7149389476004,2.3244531522515));
#86665=CARTESIAN_POINT('Ctrl Pts',(-9.13206238094477,15.7151961723969,2.32163715809377));
#86666=CARTESIAN_POINT('Ctrl Pts',(-9.13996213077413,15.7157261023629,2.31585785579372));
#86667=CARTESIAN_POINT('Ctrl Pts',(-9.14405345692767,15.7159987068053,2.3128971104097));
#86668=CARTESIAN_POINT('Ctrl Pts',(-9.15364304932451,15.7166333996662,2.30603281916753));
#86669=CARTESIAN_POINT('Ctrl Pts',(-9.15915315594597,15.716994848937,2.30214595890034));
#86670=CARTESIAN_POINT('Ctrl Pts',(-9.17704522828503,15.7181582626773,2.28970908349303));
#86671=CARTESIAN_POINT('Ctrl Pts',(-9.18953246270674,15.7189544850009,2.28131174944742));
#86672=CARTESIAN_POINT('Ctrl Pts',(-9.25439424112042,15.7230135807754,2.2391318698669));
#86673=CARTESIAN_POINT('Ctrl Pts',(-9.3087607640867,15.7261589077104,2.20852571380866));
#86674=CARTESIAN_POINT('Ctrl Pts',(-9.44100944242262,15.7334112402951,2.1448265891744));
#86675=CARTESIAN_POINT('Ctrl Pts',(-9.52012820983936,15.7374455024037,2.11483286518537));
#86676=CARTESIAN_POINT('Ctrl Pts',(-9.65683569730927,15.7444576959922,2.07613518234008));
#86677=CARTESIAN_POINT('Ctrl Pts',(-9.71315402196966,15.7473611747843,2.0637302645995));
#86678=CARTESIAN_POINT('Ctrl Pts',(-9.7771544582214,15.7508190292898,2.05354783613727));
#86679=CARTESIAN_POINT('Ctrl Pts',(-9.784266795475,15.7512054847457,2.05246997334373));
#86680=CARTESIAN_POINT('Ctrl Pts',(-9.79488250863763,15.7517859345523,2.05094115396298));
#86681=CARTESIAN_POINT('Ctrl Pts',(-9.79838014731786,15.7519777668717,2.0504503599358));
#86682=CARTESIAN_POINT('Ctrl Pts',(-9.80464157527021,15.7523222867186,2.04959484714745));
#86683=CARTESIAN_POINT('Ctrl Pts',(-9.80740466244638,15.7524747056307,2.04922535956782));
#86684=CARTESIAN_POINT('Ctrl Pts',(-9.81340828430043,15.7528067325372,2.04843999253055));
#86685=CARTESIAN_POINT('Ctrl Pts',(-9.81664911696382,15.7529864981792,2.04802707431856));
#86686=CARTESIAN_POINT('Ctrl Pts',(-9.82576724769338,15.7534937177388,2.04689633677292));
#86687=CARTESIAN_POINT('Ctrl Pts',(-9.83164748933168,15.7538225097363,2.04620333685724));
#86688=CARTESIAN_POINT('Ctrl Pts',(-9.8674332102233,15.7558330458244,2.04220592855481));
#86689=CARTESIAN_POINT('Ctrl Pts',(-9.89742860693153,15.757558849874,2.03978893259091));
#86690=CARTESIAN_POINT('Ctrl Pts',(-10.0700758681224,15.7676452210945,2.03122271221597));
#86691=CARTESIAN_POINT('Ctrl Pts',(-10.2129520125314,15.7764955200935,2.04505024830482));
#86692=CARTESIAN_POINT('Ctrl Pts',(-10.391949115939,15.7871380350668,2.08934854924332));
#86693=CARTESIAN_POINT('Ctrl Pts',(-10.4318753627286,15.7894898873021,2.10105547516521));
#86694=CARTESIAN_POINT('Ctrl Pts',(-10.4807950875598,15.7923440815215,2.11769397573293));
#86695=CARTESIAN_POINT('Ctrl Pts',(-10.4903047977213,15.7928976528069,2.12103840755994));
#86696=CARTESIAN_POINT('Ctrl Pts',(-10.5052401058005,15.793765195711,2.12646498340331));
#86697=CARTESIAN_POINT('Ctrl Pts',(-10.5106890359732,15.7940813136363,2.12848160193782));
#86698=CARTESIAN_POINT('Ctrl Pts',(-10.5207328809838,15.7946633199977,2.13226692811116));
#86699=CARTESIAN_POINT('Ctrl Pts',(-10.5253311411677,15.7949295069913,2.13402647089481));
#86700=CARTESIAN_POINT('Ctrl Pts',(-10.5353999501252,15.7955118265018,2.1379377038491));
#86701=CARTESIAN_POINT('Ctrl Pts',(-10.5408666057631,15.7958276268652,2.1400992237151));
#86702=CARTESIAN_POINT('Ctrl Pts',(-10.5563099272839,15.7967188357942,2.14631337864954));
#86703=CARTESIAN_POINT('Ctrl Pts',(-10.5662552114978,15.797291656807,2.15044331436572));
#86704=CARTESIAN_POINT('Ctrl Pts',(-10.5885494183519,15.7985737529293,2.15999117406386));
#86705=CARTESIAN_POINT('Ctrl Pts',(-10.6008709390954,15.7992809450882,2.16547079409635));
#86706=CARTESIAN_POINT('Ctrl Pts',(-10.6783705440249,15.8037235931014,2.20122736371009));
#86707=CARTESIAN_POINT('Ctrl Pts',(-10.7413235716121,15.8073011911491,2.23610216141011));
#86708=CARTESIAN_POINT('Ctrl Pts',(-10.8576563601416,15.8141059563843,2.31224239230292));
#86709=CARTESIAN_POINT('Ctrl Pts',(-10.9112497687661,15.8173341225055,2.35284434744152));
#86710=CARTESIAN_POINT('Ctrl Pts',(-11.0059088938757,15.8235288414033,2.43538991877264));
#86711=CARTESIAN_POINT('Ctrl Pts',(-11.0476087806386,15.8264708651137,2.47639767023548));
#86712=CARTESIAN_POINT('Ctrl Pts',(-11.0915652211292,15.8299725518948,2.52513103943536));
#86713=CARTESIAN_POINT('Ctrl Pts',(-11.096349464391,15.8303594643826,2.53051458497907));
#86714=CARTESIAN_POINT('Ctrl Pts',(-11.1034214378828,15.8309404690736,2.5385917271441));
#86715=CARTESIAN_POINT('Ctrl Pts',(-11.1057395363231,15.8311323931747,2.54125873460491));
#86716=CARTESIAN_POINT('Ctrl Pts',(-11.1098691707229,15.8314770111753,2.54604484062238));
#86717=CARTESIAN_POINT('Ctrl Pts',(-11.1116843322156,15.8316294358075,2.54816074489119));
#86718=CARTESIAN_POINT('Ctrl Pts',(-11.1156127399841,15.8319613968301,2.55276659178419));
#86719=CARTESIAN_POINT('Ctrl Pts',(-11.1177236723323,15.8321410903424,2.5552583913402));
#86720=CARTESIAN_POINT('Ctrl Pts',(-11.123634503141,15.8326479068886,2.56228322976308));
#86721=CARTESIAN_POINT('Ctrl Pts',(-11.1274152406231,15.8329763646806,2.56683221733516));
#86722=CARTESIAN_POINT('Ctrl Pts',(-11.1501898824591,15.8349804605761,2.59457512067511));
#86723=CARTESIAN_POINT('Ctrl Pts',(-11.1684937796426,15.8366998393674,2.61832374942014));
#86724=CARTESIAN_POINT('Ctrl Pts',(-11.2185616993983,15.8416859341888,2.68758472845355));
#86725=CARTESIAN_POINT('Ctrl Pts',(-11.2484838545116,15.845018768198,2.73436388773581));
#86726=CARTESIAN_POINT('Ctrl Pts',(-11.3027327595979,15.851683454617,2.83084593066268));
#86727=CARTESIAN_POINT('Ctrl Pts',(-11.3270457184486,15.855009783153,2.88045991990366));
#86728=CARTESIAN_POINT('Ctrl Pts',(-11.376122882885,15.8624873419584,2.99683760341718));
#86729=CARTESIAN_POINT('Ctrl Pts',(-11.3989404602103,15.8665876788832,3.06427704862729));
#86730=CARTESIAN_POINT('Ctrl Pts',(-11.4193979278188,15.8711082217035,3.14327613881463));
#86731=CARTESIAN_POINT('Ctrl Pts',(-11.421919545259,15.8716860968864,3.15346399102705));
#86732=CARTESIAN_POINT('Ctrl Pts',(-11.4258036988268,15.8726111054585,3.16991348426326));
#86733=CARTESIAN_POINT('Ctrl Pts',(-11.4272350504583,15.8729604205542,3.17615835964278));
#86734=CARTESIAN_POINT('Ctrl Pts',(-11.4297139884825,15.8735809263,3.18730953459525));
#86735=CARTESIAN_POINT('Ctrl Pts',(-11.4307774355492,15.8738526173816,3.19221217241253));
#86736=CARTESIAN_POINT('Ctrl Pts',(-11.4329514603583,15.8744198620266,3.20248952673352));
#86737=CARTESIAN_POINT('Ctrl Pts',(-11.4340570573443,15.8747152539228,3.20786522484543));
#86738=CARTESIAN_POINT('Ctrl Pts',(-11.4362376801581,15.8753123374117,3.21877873985698));
#86739=CARTESIAN_POINT('Ctrl Pts',(-11.4373109791141,15.8756139702687,3.22431680938647));
#86740=CARTESIAN_POINT('Ctrl Pts',(-11.4398810488931,15.8763560180534,3.23800111863998));
#86741=CARTESIAN_POINT('Ctrl Pts',(-11.4413407475178,15.8767952712872,3.24615417657465));
#86742=CARTESIAN_POINT('Ctrl Pts',(-11.4565520095823,15.8815777959073,3.3354805338014));
#86743=CARTESIAN_POINT('Ctrl Pts',(-11.4634999999975,15.8856953222076,3.417663599478));
#86744=CARTESIAN_POINT('Ctrl Pts',(-11.4635,15.8897282898296,3.49999999995642));
#86745=CARTESIAN_POINT('Origin',(-10.,13.2,3.5));
#86746=CARTESIAN_POINT('',(-11.4635,16.4620214545711,3.5));
#86747=CARTESIAN_POINT('',(-11.4635,16.3880240412435,3.49999999999906));
#86748=CARTESIAN_POINT('',(-11.4635,13.2,3.5));
#86749=CARTESIAN_POINT('',(-11.463499289286,15.9600992933965,3.50126593704094));
#86750=CARTESIAN_POINT('Ctrl Pts',(-11.4635,16.4620214545711,3.5));
#86751=CARTESIAN_POINT('Ctrl Pts',(-11.4635,16.4620179317433,3.49993469539802));
#86752=CARTESIAN_POINT('Ctrl Pts',(-11.4634999956977,16.462014408645,3.49986939079802));
#86753=CARTESIAN_POINT('Ctrl Pts',(-11.4634994890769,16.4618102356802,3.49608502007503));
#86754=CARTESIAN_POINT('Ctrl Pts',(-11.4634848147942,16.4616088403519,3.49236602360626));
#86755=CARTESIAN_POINT('Ctrl Pts',(-11.4634353993144,16.4612625415967,3.48599603852318));
#86756=CARTESIAN_POINT('Ctrl Pts',(-11.463407629272,16.4611180209993,3.48334499291789));
#86757=CARTESIAN_POINT('Ctrl Pts',(-11.4633350012376,16.4608170560929,3.47783985432014));
#86758=CARTESIAN_POINT('Ctrl Pts',(-11.4632889967301,16.4606605463131,3.47498581479545));
#86759=CARTESIAN_POINT('Ctrl Pts',(-11.463158122383,16.4602825890147,3.46811414699329));
#86760=CARTESIAN_POINT('Ctrl Pts',(-11.4630650538143,16.4600606924473,3.46409670993799));
#86761=CARTESIAN_POINT('Ctrl Pts',(-11.4626854793201,16.4592892876604,3.45018645982909));
#86762=CARTESIAN_POINT('Ctrl Pts',(-11.4623151756252,16.4587354065625,3.44029642890958));
#86763=CARTESIAN_POINT('Ctrl Pts',(-11.4595398677968,16.4554413791121,3.38199583243003));
#86764=CARTESIAN_POINT('Ctrl Pts',(-11.4548314994578,16.4525972279559,3.33372884426687));
#86765=CARTESIAN_POINT('Ctrl Pts',(-11.4384257364983,16.4459184976122,3.22285099501531));
#86766=CARTESIAN_POINT('Ctrl Pts',(-11.4250190844743,16.4420613096008,3.16058757473446));
#86767=CARTESIAN_POINT('Ctrl Pts',(-11.4009291195383,16.4367900833161,3.07594297823236));
#86768=CARTESIAN_POINT('Ctrl Pts',(-11.3936697060786,16.4353367821147,3.05266169272317));
#86769=CARTESIAN_POINT('Ctrl Pts',(-11.3635631087754,16.4297985780481,2.96397077459831));
#86770=CARTESIAN_POINT('Ctrl Pts',(-11.336662434992,16.4258075901989,2.90002719525077));
#86771=CARTESIAN_POINT('Ctrl Pts',(-11.3006048313447,16.4213907872111,2.82890502969825));
#86772=CARTESIAN_POINT('Ctrl Pts',(-11.2957811785397,16.4208155954075,2.81963794066478));
#86773=CARTESIAN_POINT('Ctrl Pts',(-11.287847105386,16.4198940916472,2.80478569275871));
#86774=CARTESIAN_POINT('Ctrl Pts',(-11.2847986595119,16.4195456234819,2.79916799004742));
#86775=CARTESIAN_POINT('Ctrl Pts',(-11.2792936892484,16.4189261587787,2.78918002476904));
#86776=CARTESIAN_POINT('Ctrl Pts',(-11.2768513401937,16.418654666886,2.78480209979895));
#86777=CARTESIAN_POINT('Ctrl Pts',(-11.2716858400344,16.4180873727025,2.77565371153268));
#86778=CARTESIAN_POINT('Ctrl Pts',(-11.2689582253679,16.4177917348561,2.77088584929266));
#86779=CARTESIAN_POINT('Ctrl Pts',(-11.2617321592159,16.4170186387257,2.75841808933737));
#86780=CARTESIAN_POINT('Ctrl Pts',(-11.257190023555,16.4165427527707,2.75074368789045));
#86781=CARTESIAN_POINT('Ctrl Pts',(-11.2362697761007,16.4143952990966,2.71612269784851));
#86782=CARTESIAN_POINT('Ctrl Pts',(-11.2190929269557,16.4127528550993,2.68966722315921));
#86783=CARTESIAN_POINT('Ctrl Pts',(-11.1694580243537,16.4083019652555,2.6183754425417));
#86784=CARTESIAN_POINT('Ctrl Pts',(-11.1352908501064,16.4055541438616,2.57479232064836));
#86785=CARTESIAN_POINT('Ctrl Pts',(-11.0447416938529,16.3988386025747,2.47188127322583));
#86786=CARTESIAN_POINT('Ctrl Pts',(-10.9857041528785,16.3949302280811,2.41514994773822));
#86787=CARTESIAN_POINT('Ctrl Pts',(-10.9142041731137,16.3903380178101,2.35712198631516));
#86788=CARTESIAN_POINT('Ctrl Pts',(-10.9060969531774,16.3898190609612,2.3506837991595));
#86789=CARTESIAN_POINT('Ctrl Pts',(-10.8690422571964,16.3874517000272,2.32189331356306));
#86790=CARTESIAN_POINT('Ctrl Pts',(-10.8393335014563,16.3855662582615,2.30054651405468));
#86791=CARTESIAN_POINT('Ctrl Pts',(-10.8039038317721,16.3832937003946,2.27705019215995));
#86792=CARTESIAN_POINT('Ctrl Pts',(-10.7989287268348,16.382974047527,2.27379427081977));
#86793=CARTESIAN_POINT('Ctrl Pts',(-10.7909148008438,16.3824580617593,2.26861909028466));
#86794=CARTESIAN_POINT('Ctrl Pts',(-10.7878884581149,16.3822629606058,2.26668051827097));
#86795=CARTESIAN_POINT('Ctrl Pts',(-10.7824930416615,16.3819146366548,2.26325236159538));
#86796=CARTESIAN_POINT('Ctrl Pts',(-10.7801268017806,16.3817617040863,2.26175840225348));
#86797=CARTESIAN_POINT('Ctrl Pts',(-10.7750600384494,16.381433852987,2.25857971761627));
#86798=CARTESIAN_POINT('Ctrl Pts',(-10.7723583421704,16.3812588114774,2.25689703902055));
#86799=CARTESIAN_POINT('Ctrl Pts',(-10.7649399320901,16.3807776087937,2.2523102020271));
#86800=CARTESIAN_POINT('Ctrl Pts',(-10.7602122360716,16.3804703158602,2.24942401838785));
#86801=CARTESIAN_POINT('Ctrl Pts',(-10.7349140701712,16.3788231297274,2.23417635065422));
#86802=CARTESIAN_POINT('Ctrl Pts',(-10.7140593631872,16.3774553200107,2.22229608662211));
#86803=CARTESIAN_POINT('Ctrl Pts',(-10.6488993641576,16.3731733040815,2.1872700244556));
#86804=CARTESIAN_POINT('Ctrl Pts',(-10.6036945206132,16.3701920530025,2.16587755407076));
#86805=CARTESIAN_POINT('Ctrl Pts',(-10.4408851413988,16.3596124567826,2.09880183488542));
#86806=CARTESIAN_POINT('Ctrl Pts',(-10.318538352263,16.3519998236053,2.0660264360505));
#86807=CARTESIAN_POINT('Ctrl Pts',(-10.1738690257786,16.3438014829121,2.04672998035304));
#86808=CARTESIAN_POINT('Ctrl Pts',(-10.1541936720739,16.3427015642797,2.04451088852681));
#86809=CARTESIAN_POINT('Ctrl Pts',(-10.1267614028325,16.3411883230858,2.04197947212793));
#86810=CARTESIAN_POINT('Ctrl Pts',(-10.1190385259674,16.3407645344016,2.04132863690242));
#86811=CARTESIAN_POINT('Ctrl Pts',(-10.1066085881601,16.3400859506714,2.04038049554464));
#86812=CARTESIAN_POINT('Ctrl Pts',(-10.1019046949798,16.3398299579214,2.04004454769256));
#86813=CARTESIAN_POINT('Ctrl Pts',(-10.0921496980776,16.3393007188954,2.03939523011893));
#86814=CARTESIAN_POINT('Ctrl Pts',(-10.0870984223888,16.3390275833443,2.03908531174441));
#86815=CARTESIAN_POINT('Ctrl Pts',(-10.0752401007136,16.3383884698882,2.03841947261312));
#86816=CARTESIAN_POINT('Ctrl Pts',(-10.0684319420465,16.3380231593388,2.03808489225956));
#86817=CARTESIAN_POINT('Ctrl Pts',(-10.0461702080909,16.336833773342,2.03714671553428));
#86818=CARTESIAN_POINT('Ctrl Pts',(-10.0307090852649,16.336015812855,2.03674048914706));
#86819=CARTESIAN_POINT('Ctrl Pts',(-9.94954887933745,16.3317606611936,2.03589506695001));
#86820=CARTESIAN_POINT('Ctrl Pts',(-9.88387891043051,16.3284548725228,2.03963506899745));
#86821=CARTESIAN_POINT('Ctrl Pts',(-9.73520018917126,16.321071487501,2.05819894108525));
#86822=CARTESIAN_POINT('Ctrl Pts',(-9.652780758381,16.3170541075319,2.07579939509915));
#86823=CARTESIAN_POINT('Ctrl Pts',(-9.56459615244761,16.3124896895882,2.10274513186083));
#86824=CARTESIAN_POINT('Ctrl Pts',(-9.55688032600002,16.312087933008,2.10517290351569));
#86825=CARTESIAN_POINT('Ctrl Pts',(-9.53938282946858,16.3111706480171,2.11083829965606));
#86826=CARTESIAN_POINT('Ctrl Pts',(-9.52961449251298,16.3106541154168,2.11411548977361));
#86827=CARTESIAN_POINT('Ctrl Pts',(-9.48537506647408,16.3082913394211,2.12947902541361));
#86828=CARTESIAN_POINT('Ctrl Pts',(-9.45133178171022,16.306408091368,2.14274934747207));
#86829=CARTESIAN_POINT('Ctrl Pts',(-9.41236987114795,16.3041379917954,2.15964243110291));
#86830=CARTESIAN_POINT('Ctrl Pts',(-9.40693098154697,16.3038184386072,2.16204009111253));
#86831=CARTESIAN_POINT('Ctrl Pts',(-9.39822769070095,16.3033025830735,2.16594031213614));
#86832=CARTESIAN_POINT('Ctrl Pts',(-9.39495389919815,16.3031075114832,2.16742190534092));
#86833=CARTESIAN_POINT('Ctrl Pts',(-9.38914043862299,16.3027592205662,2.17007869508921));
#86834=CARTESIAN_POINT('Ctrl Pts',(-9.38659864629389,16.3026062912644,2.17124913540923));
#86835=CARTESIAN_POINT('Ctrl Pts',(-9.38117261180963,16.3022784242984,2.17376659425047));
#86836=CARTESIAN_POINT('Ctrl Pts',(-9.37828944818641,16.3021033635097,2.17511571363189));
#86837=CARTESIAN_POINT('Ctrl Pts',(-9.37040000459547,16.3016220547435,2.17883884604856));
#86838=CARTESIAN_POINT('Ctrl Pts',(-9.36540282217486,16.3013146741941,2.18123187451134));
#86839=CARTESIAN_POINT('Ctrl Pts',(-9.33881394923839,16.2996661800116,2.1941507544183));
#86840=CARTESIAN_POINT('Ctrl Pts',(-9.31747143916905,16.2982970985201,2.20517805399805));
#86841=CARTESIAN_POINT('Ctrl Pts',(-9.25252076616979,16.294009446776,2.24078893600373));
#86842=CARTESIAN_POINT('Ctrl Pts',(-9.20989621405615,16.2910236468348,2.26708754727458));
#86843=CARTESIAN_POINT('Ctrl Pts',(-9.06462463035638,16.2804181739965,2.36734913690631));
#86844=CARTESIAN_POINT('Ctrl Pts',(-8.97027201716319,16.2727852334712,2.45238540821475));
#86845=CARTESIAN_POINT('Ctrl Pts',(-8.87537049755298,16.2645899009743,2.56329325711897));
#86846=CARTESIAN_POINT('Ctrl Pts',(-8.86301278039784,16.2635089363818,2.57833240606659));
#86847=CARTESIAN_POINT('Ctrl Pts',(-8.84619017626691,16.2620171027929,2.59965872419743));
#86848=CARTESIAN_POINT('Ctrl Pts',(-8.84146977695941,16.2615961564136,2.60574095043141));
#86849=CARTESIAN_POINT('Ctrl Pts',(-8.83394151563374,16.2609209312797,2.61560076352859));
#86850=CARTESIAN_POINT('Ctrl Pts',(-8.83110353972844,16.2606654770197,2.61935508613345));
#86851=CARTESIAN_POINT('Ctrl Pts',(-8.82524773647433,16.2601364499133,2.62717983307557));
#86852=CARTESIAN_POINT('Ctrl Pts',(-8.82223283630973,16.2598629926943,2.63125237642151));
#86853=CARTESIAN_POINT('Ctrl Pts',(-8.81518970577999,16.2592215558686,2.64087032810612));
#86854=CARTESIAN_POINT('Ctrl Pts',(-8.81117914081665,16.2588542579799,2.64642856575206));
#86855=CARTESIAN_POINT('Ctrl Pts',(-8.79812279846009,16.2576515654163,2.66479386861437));
#86856=CARTESIAN_POINT('Ctrl Pts',(-8.78924360533658,16.2568224806806,2.6777183771426));
#86857=CARTESIAN_POINT('Ctrl Pts',(-8.71392253688211,16.2496834800432,2.79122136553634));
#86858=CARTESIAN_POINT('Ctrl Pts',(-8.65993569976571,16.2438796416924,2.89950628501159));
#86859=CARTESIAN_POINT('Ctrl Pts',(-8.59428367651107,16.2342658107381,3.08563890367132));
#86860=CARTESIAN_POINT('Ctrl Pts',(-8.57447743871951,16.2304963190294,3.15997599735643));
#86861=CARTESIAN_POINT('Ctrl Pts',(-8.55855094319861,16.2258479950539,3.2466521879023));
#86862=CARTESIAN_POINT('Ctrl Pts',(-8.55663375107693,16.2252446330111,3.25781339201078));
#86863=CARTESIAN_POINT('Ctrl Pts',(-8.55415604709014,16.22439868045,3.27331378734267));
#86864=CARTESIAN_POINT('Ctrl Pts',(-8.5534851274375,16.22416197217,3.27763521493868));
#86865=CARTESIAN_POINT('Ctrl Pts',(-8.55244111713695,16.2237809484068,3.28456446353685));
#86866=CARTESIAN_POINT('Ctrl Pts',(-8.55205567625175,16.2236373191879,3.28717043244637));
#86867=CARTESIAN_POINT('Ctrl Pts',(-8.55126531727836,16.2233364856879,3.29261558865705));
#86868=CARTESIAN_POINT('Ctrl Pts',(-8.55086170798363,16.2231792064975,3.29545493129895));
#86869=CARTESIAN_POINT('Ctrl Pts',(-8.54990271148155,16.2227964839828,3.30234668109798));
#86870=CARTESIAN_POINT('Ctrl Pts',(-8.54935596451256,16.222570563643,3.30640025279708));
#86871=CARTESIAN_POINT('Ctrl Pts',(-8.54748639373319,16.2217700767385,3.32071393335293));
#86872=CARTESIAN_POINT('Ctrl Pts',(-8.54625540448858,16.2211906941084,3.33098547792107));
#86873=CARTESIAN_POINT('Ctrl Pts',(-8.53444038804317,16.2150364135262,3.43927725404014));
#86874=CARTESIAN_POINT('Ctrl Pts',(-8.53367898396677,16.2090418751038,3.53810789670551));
#86875=CARTESIAN_POINT('Ctrl Pts',(-8.55195412443037,16.1972392174759,3.73354512733723));
#86876=CARTESIAN_POINT('Ctrl Pts',(-8.57077330088434,16.1914637974433,3.82969179931078));
#86877=CARTESIAN_POINT('Ctrl Pts',(-8.60400844990076,16.1850342483103,3.9396986070818));
#86878=CARTESIAN_POINT('Ctrl Pts',(-8.60926517271683,16.1840824675942,3.9560525721009));
#86879=CARTESIAN_POINT('Ctrl Pts',(-8.61717022482973,16.1827385453827,3.9792364820915));
#86880=CARTESIAN_POINT('Ctrl Pts',(-8.61958365138434,16.1823387822354,3.98614452590325));
#86881=CARTESIAN_POINT('Ctrl Pts',(-8.62376711032751,16.1816632591698,3.99783661826078));
#86882=CARTESIAN_POINT('Ctrl Pts',(-8.62551051126551,16.1813866292381,4.00262999450132));
#86883=CARTESIAN_POINT('Ctrl Pts',(-8.62908353459874,16.1808293832529,4.01229618895413));
#86884=CARTESIAN_POINT('Ctrl Pts',(-8.63091416475779,16.1805488053774,4.01716855765677));
#86885=CARTESIAN_POINT('Ctrl Pts',(-8.63547517187958,16.1798616262582,4.02911409551682));
#86886=CARTESIAN_POINT('Ctrl Pts',(-8.63823461172387,16.1794559955694,4.03617605584134));
#86887=CARTESIAN_POINT('Ctrl Pts',(-8.64856174983524,16.1779740561627,4.06201120683181));
#86888=CARTESIAN_POINT('Ctrl Pts',(-8.6564639831058,16.1769089200978,4.08064874470118));
#86889=CARTESIAN_POINT('Ctrl Pts',(-8.70070815944155,16.17128535954,4.17925554893343));
#86890=CARTESIAN_POINT('Ctrl Pts',(-8.74380800449931,16.1669651217598,4.25599676670985));
#86891=CARTESIAN_POINT('Ctrl Pts',(-8.85254035705587,16.1576148606236,4.41434947636516));
#86892=CARTESIAN_POINT('Ctrl Pts',(-8.92055116027678,16.1526286195492,4.49372185123336));
#86893=CARTESIAN_POINT('Ctrl Pts',(-9.00407727240567,16.1465638859934,4.57241846764813));
#86894=CARTESIAN_POINT('Ctrl Pts',(-9.0118300820101,16.146001302206,4.57956641738272));
#86895=CARTESIAN_POINT('Ctrl Pts',(-9.02281070751389,16.1452038363584,4.5894729699752));
#86896=CARTESIAN_POINT('Ctrl Pts',(-9.02597449697489,16.1449739917627,4.59230242341602));
#86897=CARTESIAN_POINT('Ctrl Pts',(-9.03110355979625,16.1446011676901,4.59684946569989));
#86898=CARTESIAN_POINT('Ctrl Pts',(-9.03306122219504,16.1444588201883,4.59857565146943));
#86899=CARTESIAN_POINT('Ctrl Pts',(-9.03719735531448,16.1441579431562,4.60220310196241));
#86900=CARTESIAN_POINT('Ctrl Pts',(-9.03937685220175,16.1439993238997,4.60410315554556));
#86901=CARTESIAN_POINT('Ctrl Pts',(-9.04474327557044,16.1436086145669,4.60875360734033));
#86902=CARTESIAN_POINT('Ctrl Pts',(-9.04793645205105,16.1433760004452,4.61149672564652));
#86903=CARTESIAN_POINT('Ctrl Pts',(-9.05961028796306,16.1425252642291,4.62143799421912));
#86904=CARTESIAN_POINT('Ctrl Pts',(-9.06816088831363,16.1419015074982,4.62855298501033));
#86905=CARTESIAN_POINT('Ctrl Pts',(-9.12425789433248,16.1378099588156,4.67415937827377));
#86906=CARTESIAN_POINT('Ctrl Pts',(-9.17409310297747,16.1341804694032,4.70973175487258));
#86907=CARTESIAN_POINT('Ctrl Pts',(-9.26068684141239,16.1280586795754,4.76369240136407));
#86908=CARTESIAN_POINT('Ctrl Pts',(-9.29626162910709,16.1255907035297,4.7838437376221));
#86909=CARTESIAN_POINT('Ctrl Pts',(-9.42323571391089,16.1170215991625,4.84890294263922));
#86910=CARTESIAN_POINT('Ctrl Pts',(-9.51844802721915,16.1110380274387,4.88575263745446));
#86911=CARTESIAN_POINT('Ctrl Pts',(-9.62696029245809,16.1048081742526,4.91519822330876));
#86912=CARTESIAN_POINT('Ctrl Pts',(-9.63722150704141,16.1042243462223,4.91786332487408));
#86913=CARTESIAN_POINT('Ctrl Pts',(-9.65375835184062,16.1032917663985,4.92196708978953));
#86914=CARTESIAN_POINT('Ctrl Pts',(-9.66001596368178,16.1029407743462,4.92347621696547));
#86915=CARTESIAN_POINT('Ctrl Pts',(-9.67117058804314,16.1023184303823,4.9260885885756));
#86916=CARTESIAN_POINT('Ctrl Pts',(-9.6760636741292,16.1020465666363,4.9272080094669));
#86917=CARTESIAN_POINT('Ctrl Pts',(-9.68630107322397,16.1014801002587,4.92949472054757));
#86918=CARTESIAN_POINT('Ctrl Pts',(-9.69164637370049,16.1011856521189,4.93065726678272));
#86919=CARTESIAN_POINT('Ctrl Pts',(-9.70562188698924,16.1004191938273,4.93361482854274));
#86920=CARTESIAN_POINT('Ctrl Pts',(-9.71426209194547,16.0999487060933,4.93536190646082));
#86921=CARTESIAN_POINT('Ctrl Pts',(-9.75285162354715,16.0978618339913,4.94280257960455));
#86922=CARTESIAN_POINT('Ctrl Pts',(-9.78295981495007,16.0962725482274,4.94763784628891));
#86923=CARTESIAN_POINT('Ctrl Pts',(-9.86538591947739,16.0920088076565,4.9582454956842));
#86924=CARTESIAN_POINT('Ctrl Pts',(-9.91789988718294,16.0893884868907,4.96214261278699));
#86925=CARTESIAN_POINT('Ctrl Pts',(-10.076072460101,16.0816219120699,4.96533023130551));
#86926=CARTESIAN_POINT('Ctrl Pts',(-10.1815426907608,16.0766267479744,4.95602825698673));
#86927=CARTESIAN_POINT('Ctrl Pts',(-10.3124864034093,16.0698070056283,4.93002271748299));
#86928=CARTESIAN_POINT('Ctrl Pts',(-10.3397250450732,16.0683521183909,4.923797534166));
#86929=CARTESIAN_POINT('Ctrl Pts',(-10.3720893578367,16.0665621395121,4.915419367255));
#86930=CARTESIAN_POINT('Ctrl Pts',(-10.3774037891972,16.0662662131697,4.91401161713932));
#86931=CARTESIAN_POINT('Ctrl Pts',(-10.3860858884793,16.0657792996803,4.91165936731473));
#86932=CARTESIAN_POINT('Ctrl Pts',(-10.3894583734814,16.065589304357,4.91073266688461));
#86933=CARTESIAN_POINT('Ctrl Pts',(-10.3955099143621,16.0652467839791,4.90904645481509));
#86934=CARTESIAN_POINT('Ctrl Pts',(-10.3981901530613,16.065094514761,4.90829137823229));
#86935=CARTESIAN_POINT('Ctrl Pts',(-10.4040338899206,16.0647612744982,4.90662706496039));
#86936=CARTESIAN_POINT('Ctrl Pts',(-10.4071964406046,16.0645801355038,4.90571481545962));
#86937=CARTESIAN_POINT('Ctrl Pts',(-10.4161511030771,16.0640650481834,4.90309905569145));
#86938=CARTESIAN_POINT('Ctrl Pts',(-10.4219357183245,16.0637296956144,4.90137038204972));
#86939=CARTESIAN_POINT('Ctrl Pts',(-10.4586558640148,16.0615850171189,4.89014897378434));
#86940=CARTESIAN_POINT('Ctrl Pts',(-10.4892779789864,16.0597247022061,4.87966884348865));
#86941=CARTESIAN_POINT('Ctrl Pts',(-10.599490720058,16.0528272637606,4.8378189761102));
#86942=CARTESIAN_POINT('Ctrl Pts',(-10.6766381064648,16.0476175432362,4.80050341449727));
#86943=CARTESIAN_POINT('Ctrl Pts',(-10.8302563364765,16.0369015018342,4.70881113823773));
#86944=CARTESIAN_POINT('Ctrl Pts',(-10.9056763196231,16.0314418058153,4.65338866581849));
#86945=CARTESIAN_POINT('Ctrl Pts',(-10.9832768662898,16.0256738580968,4.58402631076947));
#86946=CARTESIAN_POINT('Ctrl Pts',(-10.9911658962252,16.0250852875304,4.57681781787796));
#86947=CARTESIAN_POINT('Ctrl Pts',(-11.0036976570844,16.0241466315328,4.56511267827738));
#86948=CARTESIAN_POINT('Ctrl Pts',(-11.0083906843494,16.0237942590809,4.56067065286819));
#86949=CARTESIAN_POINT('Ctrl Pts',(-11.0166792810886,16.0231703342717,4.55272062784796));
#86950=CARTESIAN_POINT('Ctrl Pts',(-11.0202864768818,16.0228982610496,4.54922494578488));
#86951=CARTESIAN_POINT('Ctrl Pts',(-11.0272037998889,16.0223754407541,4.54245206081779));
#86952=CARTESIAN_POINT('Ctrl Pts',(-11.0305164143292,16.0221245846215,4.53917749499192));
#86953=CARTESIAN_POINT('Ctrl Pts',(-11.0391298748392,16.0214709981277,4.53058127806441));
#86954=CARTESIAN_POINT('Ctrl Pts',(-11.0444055232095,16.0210693738379,4.52523449679433));
#86955=CARTESIAN_POINT('Ctrl Pts',(-11.064393955728,16.0195423835162,4.50466214659077));
#86956=CARTESIAN_POINT('Ctrl Pts',(-11.0788172630665,16.0184294428988,4.48915817483372));
#86957=CARTESIAN_POINT('Ctrl Pts',(-11.1140872974781,16.0156743811656,4.44955601892534));
#86958=CARTESIAN_POINT('Ctrl Pts',(-11.1344933423461,16.0140495041917,4.42507954587033));
#86959=CARTESIAN_POINT('Ctrl Pts',(-11.1889601940384,16.0095962030362,4.35523232626712));
#86960=CARTESIAN_POINT('Ctrl Pts',(-11.2212072728127,16.006823249415,4.30851834683157));
#86961=CARTESIAN_POINT('Ctrl Pts',(-11.3035648260366,15.9991071228051,4.17299882279297));
#86962=CARTESIAN_POINT('Ctrl Pts',(-11.3472271175272,15.9942241944666,4.08067411036933));
#86963=CARTESIAN_POINT('Ctrl Pts',(-11.3844896104899,15.9882791648054,3.97448419050778));
#86964=CARTESIAN_POINT('Ctrl Pts',(-11.3879213916615,15.9877084989882,3.96435000365024));
#86965=CARTESIAN_POINT('Ctrl Pts',(-11.3925669130381,15.9869014074386,3.95011984956479));
#86966=CARTESIAN_POINT('Ctrl Pts',(-11.3938743862061,15.986670181498,3.9460545715614));
#86967=CARTESIAN_POINT('Ctrl Pts',(-11.3959537263924,15.9862957116515,3.93949093412466));
#86968=CARTESIAN_POINT('Ctrl Pts',(-11.3967367325264,15.9861531105323,3.93699609517209));
#86969=CARTESIAN_POINT('Ctrl Pts',(-11.3983699690903,15.9858522682238,3.93174299126924));
#86970=CARTESIAN_POINT('Ctrl Pts',(-11.3992187290161,15.9856939403813,3.92898429913406));
#86971=CARTESIAN_POINT('Ctrl Pts',(-11.401277903736,15.985304940307,3.92222031469942));
#86972=CARTESIAN_POINT('Ctrl Pts',(-11.4024793078821,15.9850737541201,3.91821232373061));
#86973=CARTESIAN_POINT('Ctrl Pts',(-11.4067636723387,15.9842339406782,3.90369321139507));
#86974=CARTESIAN_POINT('Ctrl Pts',(-11.4097457076662,15.9836198624403,3.89315297758475));
#86975=CARTESIAN_POINT('Ctrl Pts',(-11.4281109509877,15.9796454487502,3.82534266659133));
#86976=CARTESIAN_POINT('Ctrl Pts',(-11.4401183079515,15.9761326038071,3.76722035944168));
#86977=CARTESIAN_POINT('Ctrl Pts',(-11.4584491247974,15.9684199590326,3.63988794984887));
#86978=CARTESIAN_POINT('Ctrl Pts',(-11.4634394420433,15.9642166244403,3.57062294632637));
#86979=CARTESIAN_POINT('Ctrl Pts',(-11.4634994521832,15.9600990306171,3.50126627775981));
#86980=CARTESIAN_POINT('Ctrl Pts',(-11.4634994524634,15.9600990113915,3.50126595392359));
#86981=CARTESIAN_POINT('Ctrl Pts',(-11.4634998174897,15.9600739587178,3.50084396715964));
#86982=CARTESIAN_POINT('Ctrl Pts',(-11.4635,15.9600489093257,3.5004219824875));
#86983=CARTESIAN_POINT('Ctrl Pts',(-11.4635,15.960023863236,3.50000000002449));
#86984=CARTESIAN_POINT('',(-11.4634993427279,15.8897888773263,3.50124168730561));
#86985=CARTESIAN_POINT('Ctrl Pts',(-11.4635,15.8897282898296,3.49999999995642));
#86986=CARTESIAN_POINT('Ctrl Pts',(-11.4635,15.8897485812173,3.50041426557451));
#86987=CARTESIAN_POINT('Ctrl Pts',(-11.4634998241039,15.8897688707616,3.50082853505967));
#86988=CARTESIAN_POINT('Ctrl Pts',(-11.4634994723018,15.8897891584897,3.50124280830086));
#86989=CARTESIAN_POINT('Ctrl Pts',(-11.4634994732626,15.8897891030564,3.50124167636007));
#86990=CARTESIAN_POINT('Ctrl Pts',(-11.4634429208337,15.8930533426711,3.56789708876401));
#86991=CARTESIAN_POINT('Ctrl Pts',(-11.4588327255218,15.8962578075281,3.63447116018265));
#86992=CARTESIAN_POINT('Ctrl Pts',(-11.4421263112084,15.9022646502392,3.75526584806839));
#86993=CARTESIAN_POINT('Ctrl Pts',(-11.4314552758207,15.9050388591201,3.80955386092396));
#86994=CARTESIAN_POINT('Ctrl Pts',(-11.4151159284091,15.908520678393,3.87335115221185));
#86995=CARTESIAN_POINT('Ctrl Pts',(-11.4123801444055,15.9090853631532,3.88357070858721));
#86996=CARTESIAN_POINT('Ctrl Pts',(-11.4084232940843,15.9098788134638,3.89773497866231));
#86997=CARTESIAN_POINT('Ctrl Pts',(-11.4072959005409,15.910102435243,3.9017057829439));
#86998=CARTESIAN_POINT('Ctrl Pts',(-11.4053545701882,15.9104834914579,3.90843488173125));
#86999=CARTESIAN_POINT('Ctrl Pts',(-11.4045492639391,15.9106404310371,3.91119567798628));
#87000=CARTESIAN_POINT('Ctrl Pts',(-11.402992647264,15.9109416752255,3.9164742311754));
#87001=CARTESIAN_POINT('Ctrl Pts',(-11.4022426872647,15.9110858972966,3.91899236185908));
#87002=CARTESIAN_POINT('Ctrl Pts',(-11.4002377046772,15.9114690429023,3.92565878815586));
#87003=CARTESIAN_POINT('Ctrl Pts',(-11.3989710390601,15.911708630159,3.92980351839303));
#87004=CARTESIAN_POINT('Ctrl Pts',(-11.3944013296108,15.9125641772583,3.94452210165846));
#87005=CARTESIAN_POINT('Ctrl Pts',(-11.3909967447944,15.9131856421364,3.95506374031328));
#87006=CARTESIAN_POINT('Ctrl Pts',(-11.3579082451518,15.9190743963223,4.05367372978732));
#87007=CARTESIAN_POINT('Ctrl Pts',(-11.3200204464006,15.9247087990548,4.13875886812837));
#87008=CARTESIAN_POINT('Ctrl Pts',(-11.2519856905339,15.9330344154156,4.25922858108924));
#87009=CARTESIAN_POINT('Ctrl Pts',(-11.2278145792619,15.9357563648387,4.29772669859862));
#87010=CARTESIAN_POINT('Ctrl Pts',(-11.1766541726618,15.9410446506838,4.37136301478326));
#87011=CARTESIAN_POINT('Ctrl Pts',(-11.149782361342,15.9436105400264,4.40652611322557));
#87012=CARTESIAN_POINT('Ctrl Pts',(-11.1040452423892,15.9476462548384,4.46106304122844));
#87013=CARTESIAN_POINT('Ctrl Pts',(-11.0861659919513,15.94915186665,4.48122456128071));
#87014=CARTESIAN_POINT('Ctrl Pts',(-11.0621089130142,15.9510876569649,4.50688861821555));
#87015=CARTESIAN_POINT('Ctrl Pts',(-11.0564277192387,15.9515385664006,4.51284772325852));
#87016=CARTESIAN_POINT('Ctrl Pts',(-11.0468965809449,15.9522848527628,4.52267766009709));
#87017=CARTESIAN_POINT('Ctrl Pts',(-11.0430747713931,15.9525814304796,4.52657540885455));
#87018=CARTESIAN_POINT('Ctrl Pts',(-11.0356929578405,15.9531492101371,4.53402011572748));
#87019=CARTESIAN_POINT('Ctrl Pts',(-11.0321363232207,15.9534205525647,4.53757029342998));
#87020=CARTESIAN_POINT('Ctrl Pts',(-11.0239610096179,15.9540392530456,4.54564713070572));
#87021=CARTESIAN_POINT('Ctrl Pts',(-11.0193304528417,15.9543860799559,4.55016165465651));
#87022=CARTESIAN_POINT('Ctrl Pts',(-11.0069595389834,15.955303250955,4.56206366097577));
#87023=CARTESIAN_POINT('Ctrl Pts',(-10.9991677539915,15.9558712890916,4.56939727910808));
#87024=CARTESIAN_POINT('Ctrl Pts',(-10.9238562523922,15.9612725878394,4.63873861597449));
#87025=CARTESIAN_POINT('Ctrl Pts',(-10.8507291257415,15.9658227499381,4.69436122111318));
#87026=CARTESIAN_POINT('Ctrl Pts',(-10.6990431484781,15.9745374131878,4.78869283537293));
#87027=CARTESIAN_POINT('Ctrl Pts',(-10.6212775259882,15.9786973168724,4.82793175916797));
#87028=CARTESIAN_POINT('Ctrl Pts',(-10.5101876583657,15.9847657175092,4.87208035112681));
#87029=CARTESIAN_POINT('Ctrl Pts',(-10.479487147089,15.9864563812095,4.88310798698696));
#87030=CARTESIAN_POINT('Ctrl Pts',(-10.4426859771268,15.9885267196702,4.8949544779082));
#87031=CARTESIAN_POINT('Ctrl Pts',(-10.4369143003977,15.9888526770867,4.89677298131441));
#87032=CARTESIAN_POINT('Ctrl Pts',(-10.4279826321461,15.9893592694767,4.89952633951154));
#87033=CARTESIAN_POINT('Ctrl Pts',(-10.4248304133642,15.9895384756237,4.90048642544233));
#87034=CARTESIAN_POINT('Ctrl Pts',(-10.4190077020568,15.9898703143651,4.90223840849455));
#87035=CARTESIAN_POINT('Ctrl Pts',(-10.4163381758478,15.9900227699838,4.90303333232577));
#87036=CARTESIAN_POINT('Ctrl Pts',(-10.4103133162295,15.9903675610151,4.90480868871112));
#87037=CARTESIAN_POINT('Ctrl Pts',(-10.4069567497967,15.9905601445081,4.90578471773755));
#87038=CARTESIAN_POINT('Ctrl Pts',(-10.3983201012654,15.9910568822568,4.90826257559364));
#87039=CARTESIAN_POINT('Ctrl Pts',(-10.3930350559108,15.9913620107424,4.90974672469049));
#87040=CARTESIAN_POINT('Ctrl Pts',(-10.3609543643755,15.9932206444829,4.91856122147095));
#87041=CARTESIAN_POINT('Ctrl Pts',(-10.3339644315741,15.9948115944618,4.92515667422241));
#87042=CARTESIAN_POINT('Ctrl Pts',(-10.1925609974508,16.0032307835444,4.95547387081249));
#87043=CARTESIAN_POINT('Ctrl Pts',(-10.0757948519613,16.0104263324791,4.96619953579029));
#87044=CARTESIAN_POINT('Ctrl Pts',(-9.89725550988873,16.0209714852411,4.96119477694553));
#87045=CARTESIAN_POINT('Ctrl Pts',(-9.83568554052009,16.0245330917125,4.95555792456925));
#87046=CARTESIAN_POINT('Ctrl Pts',(-9.75985238290576,16.0288095707521,4.94374015888907));
#87047=CARTESIAN_POINT('Ctrl Pts',(-9.74509109358632,16.0296369765581,4.94120713197345));
#87048=CARTESIAN_POINT('Ctrl Pts',(-9.72375600627072,16.0308259034913,4.93720798772075));
#87049=CARTESIAN_POINT('Ctrl Pts',(-9.71714968285501,16.0311930803273,4.93592243671084));
#87050=CARTESIAN_POINT('Ctrl Pts',(-9.70560396383945,16.0318331462646,4.93359293649683));
#87051=CARTESIAN_POINT('Ctrl Pts',(-9.70066070046152,16.0321066605158,4.93256892271181));
#87052=CARTESIAN_POINT('Ctrl Pts',(-9.69108495880993,16.0326355004478,4.93053354683056));
#87053=CARTESIAN_POINT('Ctrl Pts',(-9.68645190787305,16.032890918161,4.92952520996757));
#87054=CARTESIAN_POINT('Ctrl Pts',(-9.67413273278485,16.0335689049781,4.92678129414028));
#87055=CARTESIAN_POINT('Ctrl Pts',(-9.66645552592589,16.0339902121404,4.92500611375972));
#87056=CARTESIAN_POINT('Ctrl Pts',(-9.63874984763337,16.0355065531902,4.91836363247497));
#87057=CARTESIAN_POINT('Ctrl Pts',(-9.61880991556881,16.0365900912884,4.91313525239739));
#87058=CARTESIAN_POINT('Ctrl Pts',(-9.47853700597395,16.044170491937,4.87316945828526));
#87059=CARTESIAN_POINT('Ctrl Pts',(-9.36299600318659,16.0501362356306,4.82353511653231));
#87060=CARTESIAN_POINT('Ctrl Pts',(-9.21229589674631,16.0587032543091,4.73443774680789));
#87061=CARTESIAN_POINT('Ctrl Pts',(-9.1707355869757,16.0611692351423,4.70691101069027));
#87062=CARTESIAN_POINT('Ctrl Pts',(-9.11139368996741,16.0649650667623,4.66309277921341));
#87063=CARTESIAN_POINT('Ctrl Pts',(-9.09247801072464,16.0662196627082,4.64839439856228));
#87064=CARTESIAN_POINT('Ctrl Pts',(-9.06964509611192,16.0678015447531,4.6297356601552));
#87065=CARTESIAN_POINT('Ctrl Pts',(-9.06537754536843,16.0681001923612,4.6262076959144));
#87066=CARTESIAN_POINT('Ctrl Pts',(-9.0586884197408,16.0685732155084,4.62061362252977));
#87067=CARTESIAN_POINT('Ctrl Pts',(-9.05625334531319,16.0687464479391,4.61856364749642));
#87068=CARTESIAN_POINT('Ctrl Pts',(-9.05168916595467,16.0690731391413,4.61469576563487));
#87069=CARTESIAN_POINT('Ctrl Pts',(-9.04955857913786,16.069226467191,4.61287968484958));
#87070=CARTESIAN_POINT('Ctrl Pts',(-9.04470262790791,16.0695778073536,4.60871642799783));
#87071=CARTESIAN_POINT('Ctrl Pts',(-9.04198069870504,16.0697761047855,4.60636531246047));
#87072=CARTESIAN_POINT('Ctrl Pts',(-9.03477672331327,16.0703044809455,4.60009623010691));
#87073=CARTESIAN_POINT('Ctrl Pts',(-9.03030991636911,16.0706357775209,4.59616095013628));
#87074=CARTESIAN_POINT('Ctrl Pts',(-8.99846952057362,16.0730230317316,4.56776247925283));
#87075=CARTESIAN_POINT('Ctrl Pts',(-8.97200299837268,16.0751442511612,4.54230597422903));
#87076=CARTESIAN_POINT('Ctrl Pts',(-8.93876085809529,16.0779610509686,4.50783371557471));
#87077=CARTESIAN_POINT('Ctrl Pts',(-8.93109070596816,16.078622282335,4.49969506732024));
#87078=CARTESIAN_POINT('Ctrl Pts',(-8.86877152234954,16.0840835199847,4.43203218125015));
#87079=CARTESIAN_POINT('Ctrl Pts',(-8.81904498565561,16.0890020786102,4.36816328068427));
#87080=CARTESIAN_POINT('Ctrl Pts',(-8.72983646451623,16.0987189168368,4.23163327763754));
#87081=CARTESIAN_POINT('Ctrl Pts',(-8.69071312446134,16.103494498167,4.15907061112101));
#87082=CARTESIAN_POINT('Ctrl Pts',(-8.6533300188433,16.1086855463525,4.07309960405249));
#87083=CARTESIAN_POINT('Ctrl Pts',(-8.64889005481879,16.1093150311084,4.06255232716928));
#87084=CARTESIAN_POINT('Ctrl Pts',(-8.64229560467415,16.1102705034516,4.04635842217766));
#87085=CARTESIAN_POINT('Ctrl Pts',(-8.6400516945561,16.1105994783246,4.04074888684293));
#87086=CARTESIAN_POINT('Ctrl Pts',(-8.63602461295747,16.1111970608495,4.03049798576373));
#87087=CARTESIAN_POINT('Ctrl Pts',(-8.63423024252627,16.1114660388623,4.02586114115142));
#87088=CARTESIAN_POINT('Ctrl Pts',(-8.6303971989463,16.1120465946868,4.01580417767325));
#87089=CARTESIAN_POINT('Ctrl Pts',(-8.628366990728,16.1123578880008,4.01038090829862));
#87090=CARTESIAN_POINT('Ctrl Pts',(-8.62292016424368,16.1132036482661,3.99556361207068));
#87091=CARTESIAN_POINT('Ctrl Pts',(-8.61956748048885,16.1137360031373,3.98614630860418));
#87092=CARTESIAN_POINT('Ctrl Pts',(-8.60311707408465,16.1164101251813,3.93839622275472));
#87093=CARTESIAN_POINT('Ctrl Pts',(-8.59151780351218,16.1185026402088,3.89956406303697));
#87094=CARTESIAN_POINT('Ctrl Pts',(-8.57816805651377,16.1212494549363,3.84700751100414));
#87095=CARTESIAN_POINT('Ctrl Pts',(-8.57497904628135,16.1219393904434,3.83366986919692));
#87096=CARTESIAN_POINT('Ctrl Pts',(-8.54326091589608,16.1291889042777,3.69225331118162));
#87097=CARTESIAN_POINT('Ctrl Pts',(-8.53189627573499,16.1352925243252,3.56095357763328));
#87098=CARTESIAN_POINT('Ctrl Pts',(-8.53957869214876,16.1434768631266,3.40072422397946));
#87099=CARTESIAN_POINT('Ctrl Pts',(-8.54185180459172,16.1449976201787,3.37158782018656));
#87100=CARTESIAN_POINT('Ctrl Pts',(-8.54562708361405,16.146877830445,3.33670223282864));
#87101=CARTESIAN_POINT('Ctrl Pts',(-8.54629407971528,16.1471943124988,3.33086740212575));
#87102=CARTESIAN_POINT('Ctrl Pts',(-8.54738549816016,16.1476892704291,3.32180357851776));
#87103=CARTESIAN_POINT('Ctrl Pts',(-8.54778561828998,16.1478664197631,3.3185716540454));
#87104=CARTESIAN_POINT('Ctrl Pts',(-8.54854840002927,16.1481964022131,3.31257460039337));
#87105=CARTESIAN_POINT('Ctrl Pts',(-8.54890817981985,16.1483490739492,3.30980915770685));
#87106=CARTESIAN_POINT('Ctrl Pts',(-8.54974339221648,16.1486968891717,3.30352965587547));
#87107=CARTESIAN_POINT('Ctrl Pts',(-8.5502236917122,16.1488923001878,3.30001630086117));
#87108=CARTESIAN_POINT('Ctrl Pts',(-8.55172689033268,16.1494901434328,3.28931059280308));
#87109=CARTESIAN_POINT('Ctrl Pts',(-8.55279056299814,16.1498947583583,3.28212419249358));
#87110=CARTESIAN_POINT('Ctrl Pts',(-8.56480342041571,16.154274078806,3.20493510227587));
#87111=CARTESIAN_POINT('Ctrl Pts',(-8.58076801131875,16.1584869612585,3.1358146181308));
#87112=CARTESIAN_POINT('Ctrl Pts',(-8.63048308582169,16.1686084351147,2.97484491496365));
#87113=CARTESIAN_POINT('Ctrl Pts',(-8.66856005668425,16.1745172112687,2.88466609873806));
#87114=CARTESIAN_POINT('Ctrl Pts',(-8.7364704133736,16.182714673906,2.76022201798481));
#87115=CARTESIAN_POINT('Ctrl Pts',(-8.75934465406478,16.1852118328955,2.72246969672117));
#87116=CARTESIAN_POINT('Ctrl Pts',(-8.7894107158728,16.1881952752186,2.67756200700994));
#87117=CARTESIAN_POINT('Ctrl Pts',(-8.79501361774546,16.1887398065995,2.66937463766826));
#87118=CARTESIAN_POINT('Ctrl Pts',(-8.80397486928208,16.1895931032315,2.65656132444671));
#87119=CARTESIAN_POINT('Ctrl Pts',(-8.80727774006488,16.1899039487145,2.65189710254192));
#87120=CARTESIAN_POINT('Ctrl Pts',(-8.81350797086442,16.1904835566353,2.64320732546038));
#87121=CARTESIAN_POINT('Ctrl Pts',(-8.81642870056186,16.1907525658682,2.63917713649062));
#87122=CARTESIAN_POINT('Ctrl Pts',(-8.82299677265504,16.1913515347051,2.63021076099476));
#87123=CARTESIAN_POINT('Ctrl Pts',(-8.82665473277363,16.191681079925,2.62528244391914));
#87124=CARTESIAN_POINT('Ctrl Pts',(-8.83598179746578,16.1925113194784,2.6128800129419));
#87125=CARTESIAN_POINT('Ctrl Pts',(-8.84169200687672,16.1930104134511,2.60543706436782));
#87126=CARTESIAN_POINT('Ctrl Pts',(-8.87498455462523,16.1958688863119,2.56289532761114));
#87127=CARTESIAN_POINT('Ctrl Pts',(-8.90409099571932,16.1981672116393,2.52901654402643));
#87128=CARTESIAN_POINT('Ctrl Pts',(-9.03041662352791,16.2074580622841,2.39490902338277));
#87129=CARTESIAN_POINT('Ctrl Pts',(-9.14016098901583,16.2139194369629,2.3075287537668));
#87130=CARTESIAN_POINT('Ctrl Pts',(-9.28637719863801,16.2225553276027,2.22192854637982));
#87131=CARTESIAN_POINT('Ctrl Pts',(-9.31260406773908,16.2241084332452,2.20763366922292));
#87132=CARTESIAN_POINT('Ctrl Pts',(-9.34452021458465,16.226024847343,2.19148427036018));
#87133=CARTESIAN_POINT('Ctrl Pts',(-9.34980851256189,16.2263432356556,2.18884852473925));
#87134=CARTESIAN_POINT('Ctrl Pts',(-9.35804293527525,16.2268405354254,2.18480646540317));
#87135=CARTESIAN_POINT('Ctrl Pts',(-9.36097811017378,16.2270181000329,2.18337783313053));
#87136=CARTESIAN_POINT('Ctrl Pts',(-9.36642892284749,16.2273484509214,2.18074728985268));
#87137=CARTESIAN_POINT('Ctrl Pts',(-9.36894322876594,16.2275010726497,2.17954274051282));
#87138=CARTESIAN_POINT('Ctrl Pts',(-9.37465377131094,16.2278482485287,2.17682697887323));
#87139=CARTESIAN_POINT('Ctrl Pts',(-9.37785203684649,16.2280430661356,2.17532016661546));
#87140=CARTESIAN_POINT('Ctrl Pts',(-9.3875904262919,16.2286373380291,2.17077512500257));
#87141=CARTESIAN_POINT('Ctrl Pts',(-9.39414747397611,16.2290389379656,2.16777368039821));
#87142=CARTESIAN_POINT('Ctrl Pts',(-9.45478043447993,16.2327641506433,2.14055954988788));
#87143=CARTESIAN_POINT('Ctrl Pts',(-9.51025285169229,16.2362552698517,2.11960548517195));
#87144=CARTESIAN_POINT('Ctrl Pts',(-9.68009853672908,16.2468902324134,2.06697681170343));
#87145=CARTESIAN_POINT('Ctrl Pts',(-9.79722675141693,16.2541114709821,2.04577079682824));
#87146=CARTESIAN_POINT('Ctrl Pts',(-9.93935188967328,16.2622715656758,2.03756421962031));
#87147=CARTESIAN_POINT('Ctrl Pts',(-9.96309924542753,16.2636171255825,2.03677239305236));
#87148=CARTESIAN_POINT('Ctrl Pts',(-10.0038847294892,16.2658973367962,2.03640608498709));
#87149=CARTESIAN_POINT('Ctrl Pts',(-10.0209149585324,16.266840275943,2.03655036365255));
#87150=CARTESIAN_POINT('Ctrl Pts',(-10.0450222965302,16.2681625326108,2.03717552482123));
#87151=CARTESIAN_POINT('Ctrl Pts',(-10.0521039358916,16.2685494224825,2.03741064043745));
#87152=CARTESIAN_POINT('Ctrl Pts',(-10.0642886801084,16.2692125428466,2.03790379271605));
#87153=CARTESIAN_POINT('Ctrl Pts',(-10.0693926102124,16.269489534483,2.03813714038811));
#87154=CARTESIAN_POINT('Ctrl Pts',(-10.0791458761303,16.2700173969798,2.03863424676978));
#87155=CARTESIAN_POINT('Ctrl Pts',(-10.0837953716329,16.270268404979,2.03889347725565));
#87156=CARTESIAN_POINT('Ctrl Pts',(-10.0958524630101,16.2709177226534,2.03962345678638));
#87157=CARTESIAN_POINT('Ctrl Pts',(-10.1032579083141,16.271314967056,2.04012837901467));
#87158=CARTESIAN_POINT('Ctrl Pts',(-10.1284145960952,16.2726593326,2.04203600686002));
#87159=CARTESIAN_POINT('Ctrl Pts',(-10.1461443284622,16.2735981504402,2.04370635334587));
#87160=CARTESIAN_POINT('Ctrl Pts',(-10.2913206411272,16.281223938107,2.06006174105072));
#87161=CARTESIAN_POINT('Ctrl Pts',(-10.4163541484964,16.2873373706702,2.09112077805399));
#87162=CARTESIAN_POINT('Ctrl Pts',(-10.5826658290999,16.2960794534488,2.15654352199211));
#87163=CARTESIAN_POINT('Ctrl Pts',(-10.6286010439063,16.2985736002872,2.17741358091135));
#87164=CARTESIAN_POINT('Ctrl Pts',(-10.6947898098933,16.3024084913463,2.2117136588335));
#87165=CARTESIAN_POINT('Ctrl Pts',(-10.7159361502919,16.3036721631857,2.22334426289036));
#87166=CARTESIAN_POINT('Ctrl Pts',(-10.7415792734289,16.3052642392268,2.23828559812841));
#87167=CARTESIAN_POINT('Ctrl Pts',(-10.7463584901551,16.305563565692,2.24110681435914));
#87168=CARTESIAN_POINT('Ctrl Pts',(-10.753855772242,16.3060374244808,2.24559022854256));
#87169=CARTESIAN_POINT('Ctrl Pts',(-10.75658470394,16.3062108069295,2.24723426554002));
#87170=CARTESIAN_POINT('Ctrl Pts',(-10.7617010945485,16.3065376173573,2.25033943510618));
#87171=CARTESIAN_POINT('Ctrl Pts',(-10.7640897415579,16.3066909134119,2.25179851334627));
#87172=CARTESIAN_POINT('Ctrl Pts',(-10.7695343565603,16.3070419686624,2.25514578031875));
#87173=CARTESIAN_POINT('Ctrl Pts',(-10.7725875654661,16.3072400114752,2.25703837255318));
#87174=CARTESIAN_POINT('Ctrl Pts',(-10.7806689126119,16.307767268733,2.26208903606904));
#87175=CARTESIAN_POINT('Ctrl Pts',(-10.7856847992492,16.308097693042,2.26526646618435));
#87176=CARTESIAN_POINT('Ctrl Pts',(-10.8211400406343,16.3104551112773,2.28802992905568));
#87177=CARTESIAN_POINT('Ctrl Pts',(-10.850860656992,16.3125455457606,2.30870736443489));
#87178=CARTESIAN_POINT('Ctrl Pts',(-10.889983757823,16.3154236451108,2.33813764282156));
#87179=CARTESIAN_POINT('Ctrl Pts',(-10.9000846742633,16.3161786893833,2.34594506480466));
#87180=CARTESIAN_POINT('Ctrl Pts',(-10.9780404983675,16.3220927880081,2.40784644086944));
#87181=CARTESIAN_POINT('Ctrl Pts',(-11.0410654047166,16.3273812225013,2.46774700270536));
#87182=CARTESIAN_POINT('Ctrl Pts',(-11.1317960502074,16.3355291550366,2.57079504022169));
#87183=CARTESIAN_POINT('Ctrl Pts',(-11.1631953606938,16.3384777505339,2.61041500492246));
#87184=CARTESIAN_POINT('Ctrl Pts',(-11.2096758111024,16.3430388786693,2.67574516583451));
#87185=CARTESIAN_POINT('Ctrl Pts',(-11.2261291153938,16.3446995376021,2.70042563079732));
#87186=CARTESIAN_POINT('Ctrl Pts',(-11.2464428171441,16.3468132937864,2.73300012363092));
#87187=CARTESIAN_POINT('Ctrl Pts',(-11.2509972732995,16.3472916848312,2.74045123026959));
#87188=CARTESIAN_POINT('Ctrl Pts',(-11.2582871263826,16.3480648767564,2.75262091583309));
#87189=CARTESIAN_POINT('Ctrl Pts',(-11.2610632732097,16.3483611491176,2.75731473021593));
#87190=CARTESIAN_POINT('Ctrl Pts',(-11.2663479948344,16.3489287125397,2.76636502539326));
#87191=CARTESIAN_POINT('Ctrl Pts',(-11.2688604817851,16.3492001416362,2.77071912226983));
#87192=CARTESIAN_POINT('Ctrl Pts',(-11.2745595435021,16.3498195477933,2.7807141094843));
#87193=CARTESIAN_POINT('Ctrl Pts',(-11.2777312084153,16.350166989459,2.78636340963398));
#87194=CARTESIAN_POINT('Ctrl Pts',(-11.2860605156266,16.3510868765282,2.80143294007527));
#87195=CARTESIAN_POINT('Ctrl Pts',(-11.2911522098383,16.3516569937792,2.81088929318332));
#87196=CARTESIAN_POINT('Ctrl Pts',(-11.33866645321,16.3570551302457,2.90150903466805));
#87197=CARTESIAN_POINT('Ctrl Pts',(-11.3734885037713,16.3616007524379,2.98643268033429));
#87198=CARTESIAN_POINT('Ctrl Pts',(-11.4330550950195,16.3715860348141,3.18224110963936));
#87199=CARTESIAN_POINT('Ctrl Pts',(-11.4533113551798,16.3769507256209,3.293852749732));
#87200=CARTESIAN_POINT('Ctrl Pts',(-11.4611845277739,16.3834803001121,3.41705195689414));
#87201=CARTESIAN_POINT('Ctrl Pts',(-11.4617375201281,16.3840360648367,3.42744648870476));
#87202=CARTESIAN_POINT('Ctrl Pts',(-11.462353748965,16.3848190010061,3.44194327713486));
#87203=CARTESIAN_POINT('Ctrl Pts',(-11.4625107000311,16.385041207398,3.44604148212911));
#87204=CARTESIAN_POINT('Ctrl Pts',(-11.4627482229919,16.3854205677168,3.45300928691118));
#87205=CARTESIAN_POINT('Ctrl Pts',(-11.4628375825116,16.3855772373467,3.45587859872773));
#87206=CARTESIAN_POINT('Ctrl Pts',(-11.4629927204368,16.3858785321493,3.46138027023476));
#87207=CARTESIAN_POINT('Ctrl Pts',(-11.4630598374641,16.3860230779656,3.46401256677904));
#87208=CARTESIAN_POINT('Ctrl Pts',(-11.4632030117003,16.3863688545646,3.47029291813981));
#87209=CARTESIAN_POINT('Ctrl Pts',(-11.463272529837,16.3865704415006,3.47394108602005));
#87210=CARTESIAN_POINT('Ctrl Pts',(-11.4634418718914,16.3871835756994,3.4849985064854));
#87211=CARTESIAN_POINT('Ctrl Pts',(-11.4634990664671,16.3875973454599,3.49240817566415));
#87212=CARTESIAN_POINT('Ctrl Pts',(-11.4634999963152,16.3880172148887,3.4998785531803));
#87213=CARTESIAN_POINT('Ctrl Pts',(-11.4635,16.3880206279513,3.49993927663728));
#87214=CARTESIAN_POINT('Ctrl Pts',(-11.4635,16.3880240412434,3.49999999999839));
#87215=CARTESIAN_POINT('Origin',(-10.,13.2,3.5));
#87216=CARTESIAN_POINT('',(-11.4635,16.9599527886714,3.50000000001837));
#87217=CARTESIAN_POINT('',(-11.4635,16.8902616844768,3.4999999999813));
#87218=CARTESIAN_POINT('',(-11.4635,13.2,3.5));
#87219=CARTESIAN_POINT('',(-11.4634995966695,16.9598988801815,3.49891346965536));
#87220=CARTESIAN_POINT('Ctrl Pts',(-11.4635,16.9599527886714,3.50000000001837));
#87221=CARTESIAN_POINT('Ctrl Pts',(-11.4635,16.9599348168433,3.49963782541032));
#87222=CARTESIAN_POINT('Ctrl Pts',(-11.4634998655581,16.9599168473517,3.49927564859787));
#87223=CARTESIAN_POINT('Ctrl Pts',(-11.4634995966695,16.9598988801815,3.49891346965532));
#87224=CARTESIAN_POINT('Ctrl Pts',(-11.4634995979088,16.9598989630521,3.4989151401456));
#87225=CARTESIAN_POINT('Ctrl Pts',(-11.4634505510007,16.9566165950605,3.43274979180149));
#87226=CARTESIAN_POINT('Ctrl Pts',(-11.4589144860793,16.9534233256929,3.36666071639118));
#87227=CARTESIAN_POINT('Ctrl Pts',(-11.4420526131649,16.9473774955259,3.24374040176786));
#87228=CARTESIAN_POINT('Ctrl Pts',(-11.430786897264,16.9445362947727,3.18689830496202));
#87229=CARTESIAN_POINT('Ctrl Pts',(-11.4095708260853,16.9402241967998,3.1055002145385));
#87230=CARTESIAN_POINT('Ctrl Pts',(-11.4022758947889,16.9388544197586,3.0803070884726));
#87231=CARTESIAN_POINT('Ctrl Pts',(-11.392579590649,16.9371433711262,3.04990365950361));
#87232=CARTESIAN_POINT('Ctrl Pts',(-11.3908189862349,16.9368365715305,3.04449239588263));
#87233=CARTESIAN_POINT('Ctrl Pts',(-11.388014013278,16.9363535536954,3.03603912595516));
#87234=CARTESIAN_POINT('Ctrl Pts',(-11.3869910795332,16.9361785611847,3.03299000161903));
#87235=CARTESIAN_POINT('Ctrl Pts',(-11.3850610953427,16.935850498388,3.02729944777417));
#87236=CARTESIAN_POINT('Ctrl Pts',(-11.3841565302295,16.9356975731559,3.0246572296684));
#87237=CARTESIAN_POINT('Ctrl Pts',(-11.3820681126217,16.9353464110128,3.0186135089699));
#87238=CARTESIAN_POINT('Ctrl Pts',(-11.3808792660396,16.9351478849696,3.01521378554841));
#87239=CARTESIAN_POINT('Ctrl Pts',(-11.3777292503128,16.9346254963236,3.0063113439938));
#87240=CARTESIAN_POINT('Ctrl Pts',(-11.3757476815438,16.9343004875987,3.00081597517593));
#87241=CARTESIAN_POINT('Ctrl Pts',(-11.3618763629126,16.932050532595,2.9630574503832));
#87242=CARTESIAN_POINT('Ctrl Pts',(-11.3488865384744,16.9300682729349,2.93121245532271));
#87243=CARTESIAN_POINT('Ctrl Pts',(-11.293718808576,16.922174719466,2.80851293127426));
#87244=CARTESIAN_POINT('Ctrl Pts',(-11.2433816407423,16.9160426227228,2.72162635652017));
#87245=CARTESIAN_POINT('Ctrl Pts',(-11.1543378701479,16.907036750944,2.59889747505946));
#87246=CARTESIAN_POINT('Ctrl Pts',(-11.1219317177388,16.9040296668239,2.55885617874726));
#87247=CARTESIAN_POINT('Ctrl Pts',(-11.0741732928337,16.8999679898767,2.50582728916153));
#87248=CARTESIAN_POINT('Ctrl Pts',(-11.0605661263867,16.8988479581727,2.49132404247235));
#87249=CARTESIAN_POINT('Ctrl Pts',(-11.0363968235167,16.8969216271248,2.46659311391925));
#87250=CARTESIAN_POINT('Ctrl Pts',(-11.0259685650123,16.8961098616748,2.45623915874379));
#87251=CARTESIAN_POINT('Ctrl Pts',(-11.0106696827442,16.8949462177781,2.44150015165882));
#87252=CARTESIAN_POINT('Ctrl Pts',(-11.0059230055867,16.8945888710161,2.43698821956649));
#87253=CARTESIAN_POINT('Ctrl Pts',(-10.9974474697348,16.8939572515617,2.42903944613702));
#87254=CARTESIAN_POINT('Ctrl Pts',(-10.9937307562888,16.8936824374249,2.42558986056712));
#87255=CARTESIAN_POINT('Ctrl Pts',(-10.986534182009,16.8931544420089,2.4189798085762));
#87256=CARTESIAN_POINT('Ctrl Pts',(-10.9830568803333,16.8929011491501,2.41581665882687));
#87257=CARTESIAN_POINT('Ctrl Pts',(-10.9747914194238,16.8923033508257,2.40837038843208));
#87258=CARTESIAN_POINT('Ctrl Pts',(-10.9699901572121,16.8919594575289,2.40410191307195));
#87259=CARTESIAN_POINT('Ctrl Pts',(-10.9529945420396,16.8907537297291,2.38919146550323));
#87260=CARTESIAN_POINT('Ctrl Pts',(-10.9406516713332,16.8898988864544,2.37872008040215));
#87261=CARTESIAN_POINT('Ctrl Pts',(-10.8225067423732,16.8819019333641,2.28181297904141));
#87262=CARTESIAN_POINT('Ctrl Pts',(-10.7052728600729,16.8754302215461,2.21039232986514));
#87263=CARTESIAN_POINT('Ctrl Pts',(-10.537623296873,16.8664692659895,2.13805041288576));
#87264=CARTESIAN_POINT('Ctrl Pts',(-10.4945831035662,16.8641836797743,2.1218372742373));
#87265=CARTESIAN_POINT('Ctrl Pts',(-10.4291872197754,16.8606393198545,2.10066112810666));
#87266=CARTESIAN_POINT('Ctrl Pts',(-10.4073602879359,16.8594446526317,2.09415206032007));
#87267=CARTESIAN_POINT('Ctrl Pts',(-10.38013517239,16.8579302037356,2.08672041343235));
#87268=CARTESIAN_POINT('Ctrl Pts',(-10.3748708316213,16.8576362479258,2.08531494783818));
#87269=CARTESIAN_POINT('Ctrl Pts',(-10.3665384469342,16.857169037837,2.08314015476809));
#87270=CARTESIAN_POINT('Ctrl Pts',(-10.363475492954,16.856996880599,2.08235130594908));
#87271=CARTESIAN_POINT('Ctrl Pts',(-10.3576937785843,16.8566710936699,2.08088222294295));
#87272=CARTESIAN_POINT('Ctrl Pts',(-10.3549756081898,16.8565175864081,2.08019986564182));
#87273=CARTESIAN_POINT('Ctrl Pts',(-10.3487349485336,16.8561643729621,2.07865227961618));
#87274=CARTESIAN_POINT('Ctrl Pts',(-10.3452111910898,16.8559643698027,2.07779233600281));
#87275=CARTESIAN_POINT('Ctrl Pts',(-10.3357927334898,16.8554283587612,2.07553090523285));
#87276=CARTESIAN_POINT('Ctrl Pts',(-10.3298925294139,16.8550910773904,2.0741529260608));
#87277=CARTESIAN_POINT('Ctrl Pts',(-10.285557765369,16.8525463825345,2.06408855289314));
#87278=CARTESIAN_POINT('Ctrl Pts',(-10.2467979378014,16.8502638710549,2.05692163188722));
#87279=CARTESIAN_POINT('Ctrl Pts',(-10.1077261063655,16.8419782180728,2.03697295504369));
#87280=CARTESIAN_POINT('Ctrl Pts',(-10.0064338543024,16.8357892791638,2.03302588819919));
#87281=CARTESIAN_POINT('Ctrl Pts',(-9.84136043219604,16.8260031288557,2.04370265268689));
#87282=CARTESIAN_POINT('Ctrl Pts',(-9.77751885899916,16.8222871579585,2.05208000632784));
#87283=CARTESIAN_POINT('Ctrl Pts',(-9.69942826141916,16.8178482850114,2.06761639188507));
#87284=CARTESIAN_POINT('Ctrl Pts',(-9.68447511395744,16.8170029725733,2.07083582395915));
#87285=CARTESIAN_POINT('Ctrl Pts',(-9.66296407630395,16.8157933210572,2.07582125955562));
#87286=CARTESIAN_POINT('Ctrl Pts',(-9.65636404431078,16.8154230458648,2.07739934249798));
#87287=CARTESIAN_POINT('Ctrl Pts',(-9.64486632553198,16.8147794632248,2.08023315872866));
#87288=CARTESIAN_POINT('Ctrl Pts',(-9.63996376326172,16.8145055091208,2.08146846371276));
#87289=CARTESIAN_POINT('Ctrl Pts',(-9.63049308560946,16.8139771597648,2.083907063649));
#87290=CARTESIAN_POINT('Ctrl Pts',(-9.62592420726582,16.8137226647164,2.08510711847995));
#87291=CARTESIAN_POINT('Ctrl Pts',(-9.61383413929475,16.8130502276327,2.08834533300278));
#87292=CARTESIAN_POINT('Ctrl Pts',(-9.60632322247638,16.8126335094872,2.09042149248491));
#87293=CARTESIAN_POINT('Ctrl Pts',(-9.57951634167599,16.811149633807,2.09806240129607));
#87294=CARTESIAN_POINT('Ctrl Pts',(-9.5603183195409,16.8100933330598,2.10396432390656));
#87295=CARTESIAN_POINT('Ctrl Pts',(-9.42177424697449,16.8025046244441,2.14969767431031));
#87296=CARTESIAN_POINT('Ctrl Pts',(-9.30789043075783,16.7965112324549,2.20437387210448));
#87297=CARTESIAN_POINT('Ctrl Pts',(-9.16053025606825,16.7879112334743,2.30015983276175));
#87298=CARTESIAN_POINT('Ctrl Pts',(-9.12008474140615,16.7854398240238,2.32949824368207));
#87299=CARTESIAN_POINT('Ctrl Pts',(-9.06255077725626,16.7816365418002,2.37590191275258));
#87300=CARTESIAN_POINT('Ctrl Pts',(-9.04425504121095,16.780380279607,2.39141576928095));
#87301=CARTESIAN_POINT('Ctrl Pts',(-9.02221514660181,16.7787965924843,2.41105569405283));
#87302=CARTESIAN_POINT('Ctrl Pts',(-9.01810146243788,16.7784978875836,2.41476353685228));
#87303=CARTESIAN_POINT('Ctrl Pts',(-9.01165704475714,16.7780248304845,2.4206388082833));
#87304=CARTESIAN_POINT('Ctrl Pts',(-9.00931212431326,16.7778516222012,2.42279068332406));
#87305=CARTESIAN_POINT('Ctrl Pts',(-9.00491854616952,16.7775250163079,2.42684904047287));
#87306=CARTESIAN_POINT('Ctrl Pts',(-9.00286832750737,16.7773717496192,2.42875375895468));
#87307=CARTESIAN_POINT('Ctrl Pts',(-8.99819729805911,16.7770206048863,2.43311832152913));
#87308=CARTESIAN_POINT('Ctrl Pts',(-8.99558007992412,16.7768224421555,2.43558194629183));
#87309=CARTESIAN_POINT('Ctrl Pts',(-8.98865671149561,16.7762945407183,2.44214728344486));
#87310=CARTESIAN_POINT('Ctrl Pts',(-8.98436648736165,16.7759635870576,2.4462656014528));
#87311=CARTESIAN_POINT('Ctrl Pts',(-8.95385266558713,16.7735829679234,2.47591622289546));
#87312=CARTESIAN_POINT('Ctrl Pts',(-8.9285718478928,16.7714684311253,2.50239631510661));
#87313=CARTESIAN_POINT('Ctrl Pts',(-8.89656418863795,16.7686288758347,2.53854368063939));
#87314=CARTESIAN_POINT('Ctrl Pts',(-8.88892145670163,16.7679377470337,2.54738606703397));
#87315=CARTESIAN_POINT('Ctrl Pts',(-8.82539449770146,16.7620871529143,2.62268922950463));
#87316=CARTESIAN_POINT('Ctrl Pts',(-8.77542089830049,16.7567948256325,2.69391125049634));
#87317=CARTESIAN_POINT('Ctrl Pts',(-8.6975801841063,16.7475413175796,2.82895557027836));
#87318=CARTESIAN_POINT('Ctrl Pts',(-8.66737704869881,16.7435384840293,2.89113537144882));
#87319=CARTESIAN_POINT('Ctrl Pts',(-8.63576709211558,16.738799909474,2.96995035869295));
#87320=CARTESIAN_POINT('Ctrl Pts',(-8.63010004258949,16.7379223360277,2.98477365773653));
#87321=CARTESIAN_POINT('Ctrl Pts',(-8.62232066124691,16.7366753390207,3.0061586091418));
#87322=CARTESIAN_POINT('Ctrl Pts',(-8.62001197629201,16.7362994592426,3.01264721561729));
#87323=CARTESIAN_POINT('Ctrl Pts',(-8.61608249733157,16.7356493468252,3.02394293719634));
#87324=CARTESIAN_POINT('Ctrl Pts',(-8.61444074906282,16.7353744291465,3.02874259233389));
#87325=CARTESIAN_POINT('Ctrl Pts',(-8.61132658429202,16.7348464660836,3.03800382389259));
#87326=CARTESIAN_POINT('Ctrl Pts',(-8.60985063444537,16.7345933077595,3.04246413868554));
#87327=CARTESIAN_POINT('Ctrl Pts',(-8.60641052446307,16.7339961813672,3.05303046676262));
#87328=CARTESIAN_POINT('Ctrl Pts',(-8.60446496765342,16.7336528221063,3.05914246604871));
#87329=CARTESIAN_POINT('Ctrl Pts',(-8.5977698010131,16.7324508032018,3.08066394893246));
#87330=CARTESIAN_POINT('Ctrl Pts',(-8.59323463821695,16.7315990774522,3.09613925831642));
#87331=CARTESIAN_POINT('Ctrl Pts',(-8.55653952176319,16.7243605403908,3.22948115749335));
#87332=CARTESIAN_POINT('Ctrl Pts',(-8.53900015189412,16.7184929782355,3.35086770589383));
#87333=CARTESIAN_POINT('Ctrl Pts',(-8.53570058869568,16.7097645653421,3.52988618448959));
#87334=CARTESIAN_POINT('Ctrl Pts',(-8.53796740850145,16.7069711807532,3.58675126277679));
#87335=CARTESIAN_POINT('Ctrl Pts',(-8.54607741690219,16.7027244199626,3.66915863880108));
#87336=CARTESIAN_POINT('Ctrl Pts',(-8.54930487280592,16.7013686738462,3.69490768634974));
#87337=CARTESIAN_POINT('Ctrl Pts',(-8.5540696632921,16.6996733540424,3.72616341122331));
#87338=CARTESIAN_POINT('Ctrl Pts',(-8.55495711411148,16.6993675118403,3.73176600917943));
#87339=CARTESIAN_POINT('Ctrl Pts',(-8.55639808290768,16.6988856716973,3.74053289435875));
#87340=CARTESIAN_POINT('Ctrl Pts',(-8.55692949645908,16.6987108896822,3.74370082007357));
#87341=CARTESIAN_POINT('Ctrl Pts',(-8.55794253261088,16.6983830028226,3.74962033970232));
#87342=CARTESIAN_POINT('Ctrl Pts',(-8.55842160601236,16.6982300413816,3.75237231783145));
#87343=CARTESIAN_POINT('Ctrl Pts',(-8.55953745755101,16.697878506009,3.75867533535166));
#87344=CARTESIAN_POINT('Ctrl Pts',(-8.56017948779137,16.6976796406277,3.76222539420633));
#87345=CARTESIAN_POINT('Ctrl Pts',(-8.56189917038474,16.6971557817959,3.77153750492745));
#87346=CARTESIAN_POINT('Ctrl Pts',(-8.5629983166613,16.6968296320128,3.77729546057872));
#87347=CARTESIAN_POINT('Ctrl Pts',(-8.57086177896742,16.6945553387951,3.81718604933112));
#87348=CARTESIAN_POINT('Ctrl Pts',(-8.57880647809686,16.6925485101136,3.85107213138752));
#87349=CARTESIAN_POINT('Ctrl Pts',(-8.61416277230028,16.6846517604419,3.98086838599768));
#87350=CARTESIAN_POINT('Ctrl Pts',(-8.65014264478111,16.6785461257338,4.07416466700464));
#87351=CARTESIAN_POINT('Ctrl Pts',(-8.72690957835493,16.6684828595072,4.22521074513935));
#87352=CARTESIAN_POINT('Ctrl Pts',(-8.76288837434592,16.6644396541601,4.28501387943824));
#87353=CARTESIAN_POINT('Ctrl Pts',(-8.81217229757436,16.6596591360626,4.35507420532179));
#87354=CARTESIAN_POINT('Ctrl Pts',(-8.8215601090728,16.6587771451913,4.36796658865068));
#87355=CARTESIAN_POINT('Ctrl Pts',(-8.83530964021091,16.6575250471504,4.38621455276451));
#87356=CARTESIAN_POINT('Ctrl Pts',(-8.83950122630601,16.6571484109448,4.39169639802833));
#87357=CARTESIAN_POINT('Ctrl Pts',(-8.8468424935228,16.6564974140959,4.40115801623208));
#87358=CARTESIAN_POINT('Ctrl Pts',(-8.84997436962335,16.6562223632046,4.40515139912759));
#87359=CARTESIAN_POINT('Ctrl Pts',(-8.85604342268691,16.6556944388202,4.41280755952471));
#87360=CARTESIAN_POINT('Ctrl Pts',(-8.85897757295679,16.6554414506537,4.41647264727055));
#87361=CARTESIAN_POINT('Ctrl Pts',(-8.86595384655399,16.6548451758194,4.42510137117518));
#87362=CARTESIAN_POINT('Ctrl Pts',(-8.87001101784079,16.654502493703,4.43005275498897));
#87363=CARTESIAN_POINT('Ctrl Pts',(-8.88435319922937,16.6533051898675,4.4473236038106));
#87364=CARTESIAN_POINT('Ctrl Pts',(-8.89480844094996,16.6524574294324,4.45950061956521));
#87365=CARTESIAN_POINT('Ctrl Pts',(-8.98711689877095,16.6451783376181,4.56349931730929));
#87366=CARTESIAN_POINT('Ctrl Pts',(-9.08004075503841,16.6392746440423,4.64483200697732));
#87367=CARTESIAN_POINT('Ctrl Pts',(-9.22874769995715,16.6305304575254,4.74505958107827));
#87368=CARTESIAN_POINT('Ctrl Pts',(-9.27721961215285,16.6277626068333,4.77380969143141));
#87369=CARTESIAN_POINT('Ctrl Pts',(-9.35013386353142,16.6235507898639,4.81155319672937));
#87370=CARTESIAN_POINT('Ctrl Pts',(-9.37335249344405,16.6222026129317,4.82280403834688));
#87371=CARTESIAN_POINT('Ctrl Pts',(-9.4020142524743,16.6205157796641,4.83576845361831));
#87372=CARTESIAN_POINT('Ctrl Pts',(-9.40718708947211,16.6202104588071,4.83807218300337));
#87373=CARTESIAN_POINT('Ctrl Pts',(-9.41531301069147,16.619729260021,4.84163470401166));
#87374=CARTESIAN_POINT('Ctrl Pts',(-9.41825714495305,16.6195545926937,4.84291392303114));
#87375=CARTESIAN_POINT('Ctrl Pts',(-9.42377142700586,16.6192268012539,4.84528832849124));
#87376=CARTESIAN_POINT('Ctrl Pts',(-9.42634051475876,16.6190738196438,4.84638584724973));
#87377=CARTESIAN_POINT('Ctrl Pts',(-9.43223744858918,16.618722078918,4.84888508574561));
#87378=CARTESIAN_POINT('Ctrl Pts',(-9.43556734261051,16.6185230270796,4.85028184614459));
#87379=CARTESIAN_POINT('Ctrl Pts',(-9.44432662641474,16.6179983598569,4.85391796096234));
#87380=CARTESIAN_POINT('Ctrl Pts',(-9.44976433100091,16.6176715825077,4.85613695817576));
#87381=CARTESIAN_POINT('Ctrl Pts',(-9.48772140460113,16.6153838974898,4.87136046296472));
#87382=CARTESIAN_POINT('Ctrl Pts',(-9.520682759239,16.613363543386,4.88322575100979));
#87383=CARTESIAN_POINT('Ctrl Pts',(-9.64880703307678,16.605465073032,4.9242179803999));
#87384=CARTESIAN_POINT('Ctrl Pts',(-9.74642354967697,16.5993740197994,4.94479516224972));
#87385=CARTESIAN_POINT('Ctrl Pts',(-9.89652529098856,16.5904089066308,4.96074336300252));
#87386=CARTESIAN_POINT('Ctrl Pts',(-9.94793039616041,16.5874038992011,4.96347795868971));
#87387=CARTESIAN_POINT('Ctrl Pts',(-10.0293970093133,16.5827673594069,4.96351265151782));
#87388=CARTESIAN_POINT('Ctrl Pts',(-10.0594119368165,16.5810856962556,4.96260174813191));
#87389=CARTESIAN_POINT('Ctrl Pts',(-10.0981308889068,16.5789496295749,4.96023267207046));
#87390=CARTESIAN_POINT('Ctrl Pts',(-10.1068776691884,16.5784692638795,4.95961854484892));
#87391=CARTESIAN_POINT('Ctrl Pts',(-10.121061329657,16.5776937440279,4.95849450272809));
#87392=CARTESIAN_POINT('Ctrl Pts',(-10.1265017148023,16.5773971010036,4.95803270789957));
#87393=CARTESIAN_POINT('Ctrl Pts',(-10.136941519766,16.5768293977552,4.95708767615026));
#87394=CARTESIAN_POINT('Ctrl Pts',(-10.1419412774326,16.5765581957941,4.95660912754752));
#87395=CARTESIAN_POINT('Ctrl Pts',(-10.1533641933419,16.5759400936031,4.95545641775633));
#87396=CARTESIAN_POINT('Ctrl Pts',(-10.1597855765533,16.575593721823,4.95476545571316));
#87397=CARTESIAN_POINT('Ctrl Pts',(-10.1768073477316,16.5746783516421,4.9528197924749));
#87398=CARTESIAN_POINT('Ctrl Pts',(-10.1873990481804,16.5741116454794,4.951491575025));
#87399=CARTESIAN_POINT('Ctrl Pts',(-10.2950374637156,16.5683794873798,4.93679566764981));
#87400=CARTESIAN_POINT('Ctrl Pts',(-10.3905267454149,16.5635415900345,4.91383196217092));
#87401=CARTESIAN_POINT('Ctrl Pts',(-10.5593075488035,16.5548341843128,4.85482080836481));
#87402=CARTESIAN_POINT('Ctrl Pts',(-10.6332543843851,16.5509508837894,4.82187424852942));
#87403=CARTESIAN_POINT('Ctrl Pts',(-10.7325920023136,16.5451976834576,4.76735852213373));
#87404=CARTESIAN_POINT('Ctrl Pts',(-10.760554920684,16.5435125836994,4.75077758700944));
#87405=CARTESIAN_POINT('Ctrl Pts',(-10.7930342758906,16.5414485466426,4.73002659454609));
#87406=CARTESIAN_POINT('Ctrl Pts',(-10.7981076368049,16.541122956629,4.72674079721484));
#87407=CARTESIAN_POINT('Ctrl Pts',(-10.8059132472803,16.5406168521236,4.72161652409847));
#87408=CARTESIAN_POINT('Ctrl Pts',(-10.8086599508535,16.5404377626776,4.71980005637847));
#87409=CARTESIAN_POINT('Ctrl Pts',(-10.8137178574439,16.540106089571,4.71643053731557));
#87410=CARTESIAN_POINT('Ctrl Pts',(-10.8160307721753,16.5399536823543,4.71488015135012));
#87411=CARTESIAN_POINT('Ctrl Pts',(-10.8212373134589,16.5396089395748,4.71136854189779));
#87412=CARTESIAN_POINT('Ctrl Pts',(-10.8241283291991,16.5394163556338,4.70940355787654));
#87413=CARTESIAN_POINT('Ctrl Pts',(-10.8315429212018,16.5389195048439,4.70432502972887));
#87414=CARTESIAN_POINT('Ctrl Pts',(-10.8360560213095,16.5386142625798,4.70119637625286));
#87415=CARTESIAN_POINT('Ctrl Pts',(-10.8633364370759,16.5367525146598,4.68205632835596));
#87416=CARTESIAN_POINT('Ctrl Pts',(-10.8856593950103,16.5351584179006,4.66542447088776));
#87417=CARTESIAN_POINT('Ctrl Pts',(-10.9909613289468,16.5273438729891,4.58219552331111));
#87418=CARTESIAN_POINT('Ctrl Pts',(-11.0669859044227,16.5208156003626,4.50731975952143));
#87419=CARTESIAN_POINT('Ctrl Pts',(-11.1788159931942,16.5102991949617,4.37017500146768));
#87420=CARTESIAN_POINT('Ctrl Pts',(-11.2194003851939,16.5062029656009,4.31232787288269));
#87421=CARTESIAN_POINT('Ctrl Pts',(-11.2639003112585,16.5013674460147,4.23800123589068));
#87422=CARTESIAN_POINT('Ctrl Pts',(-11.2719175317066,16.5004796980069,4.224096431662));
#87423=CARTESIAN_POINT('Ctrl Pts',(-11.2830612488159,16.4992209563954,4.20401274424045));
#87424=CARTESIAN_POINT('Ctrl Pts',(-11.2863749560413,16.4988433382746,4.19793952964295));
#87425=CARTESIAN_POINT('Ctrl Pts',(-11.2920460416399,16.4981911923057,4.18736821447288));
#87426=CARTESIAN_POINT('Ctrl Pts',(-11.2944232839424,16.4979159674379,4.18288095512766));
#87427=CARTESIAN_POINT('Ctrl Pts',(-11.2989514209203,16.4973880887414,4.17422507988745));
#87428=CARTESIAN_POINT('Ctrl Pts',(-11.3011057203239,16.4971353180025,4.1700583239585));
#87429=CARTESIAN_POINT('Ctrl Pts',(-11.3061449502822,16.4965401341449,4.16019571572897));
#87430=CARTESIAN_POINT('Ctrl Pts',(-11.3090127270379,16.496198320132,4.15449117367747));
#87431=CARTESIAN_POINT('Ctrl Pts',(-11.3189139535921,16.4950070428047,4.13447037092822));
#87432=CARTESIAN_POINT('Ctrl Pts',(-11.3257507522875,16.4941643485673,4.12005776959551));
#87433=CARTESIAN_POINT('Ctrl Pts',(-11.383670451414,16.4868354722167,3.99261800050048));
#87434=CARTESIAN_POINT('Ctrl Pts',(-11.4204271278246,16.4808873786295,3.87363819008585));
#87435=CARTESIAN_POINT('Ctrl Pts',(-11.4448776580043,16.4739460446586,3.73344087256024));
#87436=CARTESIAN_POINT('Ctrl Pts',(-11.4476794056018,16.4730521087111,3.71538433178781));
#87437=CARTESIAN_POINT('Ctrl Pts',(-11.4576173709659,16.4694210514421,3.64233363242904));
#87438=CARTESIAN_POINT('Ctrl Pts',(-11.4619627599203,16.4666390583929,3.58701144672067));
#87439=CARTESIAN_POINT('Ctrl Pts',(-11.4633863975749,16.4631513064801,3.52105591908527));
#87440=CARTESIAN_POINT('Ctrl Pts',(-11.4635,16.4625893807927,3.51052796134199));
#87441=CARTESIAN_POINT('Ctrl Pts',(-11.4635,16.4620214545711,3.5));
#87442=CARTESIAN_POINT('',(-11.4634995813664,16.8901969352951,3.49889304900151));
#87443=CARTESIAN_POINT('Ctrl Pts',(-11.4635,16.3880240412434,3.49999999999839));
#87444=CARTESIAN_POINT('Ctrl Pts',(-11.4635,16.3931801882591,3.59172920727273));
#87445=CARTESIAN_POINT('Ctrl Pts',(-11.4548759495079,16.3987234838506,3.6832472985968));
#87446=CARTESIAN_POINT('Ctrl Pts',(-11.4176111906088,16.4107369833002,3.87925201809585));
#87447=CARTESIAN_POINT('Ctrl Pts',(-11.3858332866077,16.4171472519497,3.98262500487411));
#87448=CARTESIAN_POINT('Ctrl Pts',(-11.3362257707668,16.424129631001,4.09717824540646));
#87449=CARTESIAN_POINT('Ctrl Pts',(-11.3291996942818,16.4250713372376,4.11265763212551));
#87450=CARTESIAN_POINT('Ctrl Pts',(-11.3190904515954,16.4263637814336,4.13393663748888));
#87451=CARTESIAN_POINT('Ctrl Pts',(-11.3162357366293,16.4267222847214,4.13984276773713));
#87452=CARTESIAN_POINT('Ctrl Pts',(-11.3112514155487,16.4273373012125,4.14998031660428));
#87453=CARTESIAN_POINT('Ctrl Pts',(-11.3091408143689,16.4275944652624,4.15422092265529));
#87454=CARTESIAN_POINT('Ctrl Pts',(-11.3047372189894,16.4281243663789,4.16296195200507));
#87455=CARTESIAN_POINT('Ctrl Pts',(-11.3024414382342,16.4283970021939,4.16746090617847));
#87456=CARTESIAN_POINT('Ctrl Pts',(-11.2970246869188,16.4290319323183,4.17794153931007));
#87457=CARTESIAN_POINT('Ctrl Pts',(-11.2938855373527,16.4293935860143,4.18391372811532));
#87458=CARTESIAN_POINT('Ctrl Pts',(-11.2836022134155,16.4305583430662,4.20315337255562));
#87459=CARTESIAN_POINT('Ctrl Pts',(-11.27629427864,16.4313556853812,4.2163324955626));
#87460=CARTESIAN_POINT('Ctrl Pts',(-11.2376377263323,16.4354247081208,4.28357547800333));
#87461=CARTESIAN_POINT('Ctrl Pts',(-11.2030517617731,16.4385781624238,4.33570644424629));
#87462=CARTESIAN_POINT('Ctrl Pts',(-11.1110468408351,16.4460900895755,4.45678035221242));
#87463=CARTESIAN_POINT('Ctrl Pts',(-11.0504290663564,16.4503573169292,4.52296220127521));
#87464=CARTESIAN_POINT('Ctrl Pts',(-10.945338350377,16.4573958303877,4.61844384484336));
#87465=CARTESIAN_POINT('Ctrl Pts',(-10.9046695933794,16.4600521107499,4.65158719627362));
#87466=CARTESIAN_POINT('Ctrl Pts',(-10.8565577731584,16.463229992384,4.68667257769171));
#87467=CARTESIAN_POINT('Ctrl Pts',(-10.8507699136273,16.4636128562546,4.69082894462523));
#87468=CARTESIAN_POINT('Ctrl Pts',(-10.8420793077374,16.4641889438487,4.69697413023724));
#87469=CARTESIAN_POINT('Ctrl Pts',(-10.83919927963,16.4643800529696,4.69899507818673));
#87470=CARTESIAN_POINT('Ctrl Pts',(-10.8340250536535,16.4647238017809,4.70259811500445));
#87471=CARTESIAN_POINT('Ctrl Pts',(-10.8317335986452,16.4648761779959,4.7041840544719));
#87472=CARTESIAN_POINT('Ctrl Pts',(-10.8267374314621,16.4652087347354,4.70762088849826));
#87473=CARTESIAN_POINT('Ctrl Pts',(-10.8240310633824,16.4653890771003,4.7094692212142));
#87474=CARTESIAN_POINT('Ctrl Pts',(-10.8163785367876,16.4658995230326,4.71465795910971));
#87475=CARTESIAN_POINT('Ctrl Pts',(-10.8114181785268,16.4662309914072,4.71797717959226));
#87476=CARTESIAN_POINT('Ctrl Pts',(-10.7805880623926,16.4682941525806,4.73833521069324));
#87477=CARTESIAN_POINT('Ctrl Pts',(-10.7542047482493,16.4700725589853,4.75457831055091));
#87478=CARTESIAN_POINT('Ctrl Pts',(-10.590082747963,16.4811202693212,4.84857300899681));
#87479=CARTESIAN_POINT('Ctrl Pts',(-10.4409930404533,16.490944853355,4.90441804275674));
#87480=CARTESIAN_POINT('Ctrl Pts',(-10.2585434265272,16.5015105828399,4.94075022572236));
#87481=CARTESIAN_POINT('Ctrl Pts',(-10.2311136817078,16.5030670935772,4.94540393353071));
#87482=CARTESIAN_POINT('Ctrl Pts',(-10.1947869504817,16.5050875314302,4.95050642755518));
#87483=CARTESIAN_POINT('Ctrl Pts',(-10.1859961768655,16.5055733367188,4.95165983601738));
#87484=CARTESIAN_POINT('Ctrl Pts',(-10.1717530185874,16.5063555169609,4.95339712741371));
#87485=CARTESIAN_POINT('Ctrl Pts',(-10.1663069730138,16.5066534274817,4.95403036461971));
#87486=CARTESIAN_POINT('Ctrl Pts',(-10.1558697446845,16.5072221737813,4.95518454295686));
#87487=CARTESIAN_POINT('Ctrl Pts',(-10.1508791982187,16.5074931606319,4.95571044503378));
#87488=CARTESIAN_POINT('Ctrl Pts',(-10.1393924158685,16.5081147301189,4.9568612131095));
#87489=CARTESIAN_POINT('Ctrl Pts',(-10.132894480934,16.508464754818,4.95746831824342));
#87490=CARTESIAN_POINT('Ctrl Pts',(-10.112570897897,16.5095546983652,4.95923011167431));
#87491=CARTESIAN_POINT('Ctrl Pts',(-10.0987325304649,16.5102898588875,4.96023170447868));
#87492=CARTESIAN_POINT('Ctrl Pts',(-10.0666348602718,16.5119800662877,4.96209647969414));
#87493=CARTESIAN_POINT('Ctrl Pts',(-10.0483693056904,16.512930681251,4.96281467305182));
#87494=CARTESIAN_POINT('Ctrl Pts',(-9.98472315620391,16.5162092832952,4.96412373234447));
#87495=CARTESIAN_POINT('Ctrl Pts',(-9.93933088742377,16.5184868547295,4.96294612254834));
#87496=CARTESIAN_POINT('Ctrl Pts',(-9.80857053458222,16.5249660434233,4.95345612520352));
#87497=CARTESIAN_POINT('Ctrl Pts',(-9.72379001921425,16.5290582179531,4.93975256620771));
#87498=CARTESIAN_POINT('Ctrl Pts',(-9.62381203559086,16.5341517004134,4.91443214209929));
#87499=CARTESIAN_POINT('Ctrl Pts',(-9.60700426248252,16.5350177910798,4.90985460029978));
#87500=CARTESIAN_POINT('Ctrl Pts',(-9.5518288556204,16.5379045404512,4.89376443966103));
#87501=CARTESIAN_POINT('Ctrl Pts',(-9.51385482115936,16.5399614332783,4.88097755935368));
#87502=CARTESIAN_POINT('Ctrl Pts',(-9.47077463775093,16.5424263247385,4.86447417897149));
#87503=CARTESIAN_POINT('Ctrl Pts',(-9.46510666962518,16.542753302647,4.86226223308327));
#87504=CARTESIAN_POINT('Ctrl Pts',(-9.45607458405374,16.5432788857912,4.8586723691638));
#87505=CARTESIAN_POINT('Ctrl Pts',(-9.45270146195518,16.5434761856947,4.85731712378299));
#87506=CARTESIAN_POINT('Ctrl Pts',(-9.44673516066509,16.5438270253892,4.85489414057631));
#87507=CARTESIAN_POINT('Ctrl Pts',(-9.44413995893464,16.5439802600057,4.85383149958612));
#87508=CARTESIAN_POINT('Ctrl Pts',(-9.43862675233822,16.5443071456383,4.85155551619068));
#87509=CARTESIAN_POINT('Ctrl Pts',(-9.43570966501676,16.544480909512,4.85034019935334));
#87510=CARTESIAN_POINT('Ctrl Pts',(-9.42778804029564,16.5449549294327,4.84700974106772));
#87511=CARTESIAN_POINT('Ctrl Pts',(-9.42279136023704,16.5452562623008,4.84487618524535));
#87512=CARTESIAN_POINT('Ctrl Pts',(-9.39711345763482,16.546816440524,4.83374239841065));
#87513=CARTESIAN_POINT('Ctrl Pts',(-9.37663148297218,16.5480998932401,4.82429322462625));
#87514=CARTESIAN_POINT('Ctrl Pts',(-9.3157234456813,16.5520171710776,4.79446779811624));
#87515=CARTESIAN_POINT('Ctrl Pts',(-9.27601749540531,16.5547065480505,4.77268618166388));
#87516=CARTESIAN_POINT('Ctrl Pts',(-9.18080049301202,16.5613952172425,4.71455343493635));
#87517=CARTESIAN_POINT('Ctrl Pts',(-9.12662471568174,16.5654120816084,4.67619893687998));
#87518=CARTESIAN_POINT('Ctrl Pts',(-9.01460132407091,16.5740074643417,4.58486954158093));
#87519=CARTESIAN_POINT('Ctrl Pts',(-8.95802159746886,16.578539913458,4.53064859576869));
#87520=CARTESIAN_POINT('Ctrl Pts',(-8.8989656985755,16.5834663997762,4.46419354430413));
#87521=CARTESIAN_POINT('Ctrl Pts',(-8.89197666623584,16.5840530964361,4.45615376590983));
#87522=CARTESIAN_POINT('Ctrl Pts',(-8.88089568501535,16.5849894141752,4.44312216822952));
#87523=CARTESIAN_POINT('Ctrl Pts',(-8.87674798086112,16.5853413032756,4.43817844538799));
#87524=CARTESIAN_POINT('Ctrl Pts',(-8.86943001400414,16.5859647498678,4.42933793048835));
#87525=CARTESIAN_POINT('Ctrl Pts',(-8.86624688001899,16.5862368246155,4.42545196854624));
#87526=CARTESIAN_POINT('Ctrl Pts',(-8.85964233623009,16.5868032470903,4.41730394004426));
#87527=CARTESIAN_POINT('Ctrl Pts',(-8.85622466260814,16.587097443206,4.41303893587688));
#87528=CARTESIAN_POINT('Ctrl Pts',(-8.84737448651616,16.587862193174,4.40186689280143));
#87529=CARTESIAN_POINT('Ctrl Pts',(-8.84198011378171,16.5883312382589,4.39492983765594));
#87530=CARTESIAN_POINT('Ctrl Pts',(-8.81832982760106,16.5904012420737,4.36394412148767));
#87531=CARTESIAN_POINT('Ctrl Pts',(-8.80075753444055,16.5919756559307,4.33938162819158));
#87532=CARTESIAN_POINT('Ctrl Pts',(-8.75509688571016,16.5961875208373,4.27119315531665));
#87533=CARTESIAN_POINT('Ctrl Pts',(-8.7285472486907,16.5987725644281,4.22658867551589));
#87534=CARTESIAN_POINT('Ctrl Pts',(-8.65549313553559,16.6064882822691,4.08753758299332));
#87535=CARTESIAN_POINT('Ctrl Pts',(-8.61675383388309,16.6114650354277,3.98941360058881));
#87536=CARTESIAN_POINT('Ctrl Pts',(-8.5811102198745,16.6183188830102,3.85977826741604));
#87537=CARTESIAN_POINT('Ctrl Pts',(-8.57420057649422,16.6198404290076,3.83133726956228));
#87538=CARTESIAN_POINT('Ctrl Pts',(-8.56699488810879,16.6217051353892,3.79725360452117));
#87539=CARTESIAN_POINT('Ctrl Pts',(-8.5658725030529,16.6220052749347,3.79179046697166));
#87540=CARTESIAN_POINT('Ctrl Pts',(-8.56409226819519,16.6224977668794,3.78286682885399));
#87541=CARTESIAN_POINT('Ctrl Pts',(-8.56341562646414,16.6226890892882,3.77941008268206));
#87542=CARTESIAN_POINT('Ctrl Pts',(-8.56222595806813,16.6230330650534,3.77321387624022));
#87543=CARTESIAN_POINT('Ctrl Pts',(-8.56170827151446,16.6231854534177,3.77047536194942));
#87544=CARTESIAN_POINT('Ctrl Pts',(-8.56059940163914,16.6235178519028,3.7645163290109));
#87545=CARTESIAN_POINT('Ctrl Pts',(-8.56001121040862,16.6236980226177,3.76129534303752));
#87546=CARTESIAN_POINT('Ctrl Pts',(-8.5583838549246,16.624207507531,3.75221140825435));
#87547=CARTESIAN_POINT('Ctrl Pts',(-8.5573696678812,16.6245381785504,3.74634412223357));
#87548=CARTESIAN_POINT('Ctrl Pts',(-8.55134556880129,16.6265854626481,3.71017990810905));
#87549=CARTESIAN_POINT('Ctrl Pts',(-8.54725479528341,16.6283479803188,3.67973968361974));
#87550=CARTESIAN_POINT('Ctrl Pts',(-8.5285311135885,16.639072922007,3.49703100312817));
#87551=CARTESIAN_POINT('Ctrl Pts',(-8.53688494605726,16.6485691405206,3.34335109958162));
#87552=CARTESIAN_POINT('Ctrl Pts',(-8.57566707559699,16.659153265462,3.16213651885384));
#87553=CARTESIAN_POINT('Ctrl Pts',(-8.58347270923564,16.660967740492,3.13077557289536));
#87554=CARTESIAN_POINT('Ctrl Pts',(-8.59487270734675,16.6632658523272,3.09068681023922));
#87555=CARTESIAN_POINT('Ctrl Pts',(-8.59752137310757,16.6637795661655,3.08170141918379));
#87556=CARTESIAN_POINT('Ctrl Pts',(-8.60188912971016,16.6645955717653,3.06739217437182));
#87557=CARTESIAN_POINT('Ctrl Pts',(-8.60355276122148,16.6648996496659,3.06205177596288));
#87558=CARTESIAN_POINT('Ctrl Pts',(-8.60660809910554,16.6654462275488,3.05243832333154));
#87559=CARTESIAN_POINT('Ctrl Pts',(-8.60798894163173,16.6656890768795,3.04816191184848));
#87560=CARTESIAN_POINT('Ctrl Pts',(-8.61128337021697,16.6662588213993,3.0381176547298));
#87561=CARTESIAN_POINT('Ctrl Pts',(-8.61321323588071,16.6665851808715,3.03235520841634));
#87562=CARTESIAN_POINT('Ctrl Pts',(-8.61893525489873,16.6675318060512,3.01561660642798));
#87563=CARTESIAN_POINT('Ctrl Pts',(-8.6228222725748,16.6681489595967,3.00467321942347));
#87564=CARTESIAN_POINT('Ctrl Pts',(-8.65854569652286,16.6736008560058,2.90777124321152));
#87565=CARTESIAN_POINT('Ctrl Pts',(-8.69826304939138,16.678152806262,2.82493093549761));
#87566=CARTESIAN_POINT('Ctrl Pts',(-8.79777360647408,16.6875817513774,2.65928737288595));
#87567=CARTESIAN_POINT('Ctrl Pts',(-8.85898594760522,16.6924178420713,2.57792151721275));
#87568=CARTESIAN_POINT('Ctrl Pts',(-8.94147503544416,16.6986964128879,2.48918745539993));
#87569=CARTESIAN_POINT('Ctrl Pts',(-8.95511887106203,16.6997288644021,2.47509002708458));
#87570=CARTESIAN_POINT('Ctrl Pts',(-8.97288692182853,16.7010724267843,2.4574548773814));
#87571=CARTESIAN_POINT('Ctrl Pts',(-8.97675370519814,16.7013647636604,2.45365941187148));
#87572=CARTESIAN_POINT('Ctrl Pts',(-8.98290657404069,16.7018300166335,2.44768674881562));
#87573=CARTESIAN_POINT('Ctrl Pts',(-8.98517882041117,16.7020018517127,2.4454952874364));
#87574=CARTESIAN_POINT('Ctrl Pts',(-8.98928045095832,16.7023121018062,2.44156501697216));
#87575=CARTESIAN_POINT('Ctrl Pts',(-8.99110725918038,16.7024503107574,2.4398235725568));
#87576=CARTESIAN_POINT('Ctrl Pts',(-8.99551134324725,16.7027835639416,2.4356469754949));
#87577=CARTESIAN_POINT('Ctrl Pts',(-8.99809296158382,16.7029789573942,2.43321646612632));
#87578=CARTESIAN_POINT('Ctrl Pts',(-9.00598968278818,16.7035766947655,2.42583590974852));
#87579=CARTESIAN_POINT('Ctrl Pts',(-9.01133274247707,16.7039812202781,2.4209161047594));
#87580=CARTESIAN_POINT('Ctrl Pts',(-9.02378380351619,16.7049236230549,2.40962146572087));
#87581=CARTESIAN_POINT('Ctrl Pts',(-9.03091795075709,16.7054633935459,2.40327606803278));
#87582=CARTESIAN_POINT('Ctrl Pts',(-9.06175229133653,16.7077935235339,2.37638652533085));
#87583=CARTESIAN_POINT('Ctrl Pts',(-9.08604630846293,16.709622277208,2.35653840758735));
#87584=CARTESIAN_POINT('Ctrl Pts',(-9.16668436619694,16.7156214222931,2.29486969796859));
#87585=CARTESIAN_POINT('Ctrl Pts',(-9.22540234026355,16.7198782159552,2.25631507270421));
#87586=CARTESIAN_POINT('Ctrl Pts',(-9.37244114266306,16.7299820050387,2.17423456077122));
#87587=CARTESIAN_POINT('Ctrl Pts',(-9.4628400781496,16.735743835191,2.13510103251226));
#87588=CARTESIAN_POINT('Ctrl Pts',(-9.56663521271319,16.7417792056597,2.10209424952478));
#87589=CARTESIAN_POINT('Ctrl Pts',(-9.57681291714972,16.7423653826097,2.0989795763813));
#87590=CARTESIAN_POINT('Ctrl Pts',(-9.59321208410454,16.7433010344993,2.09415596585986));
#87591=CARTESIAN_POINT('Ctrl Pts',(-9.59941231513204,16.7436527723339,2.09237669618511));
#87592=CARTESIAN_POINT('Ctrl Pts',(-9.61046115101857,16.744276045692,2.08928494605108));
#87593=CARTESIAN_POINT('Ctrl Pts',(-9.61530510159173,16.7445480974814,2.08795633413268));
#87594=CARTESIAN_POINT('Ctrl Pts',(-9.62543513290881,16.745114566219,2.08523383755892));
#87595=CARTESIAN_POINT('Ctrl Pts',(-9.63072238379831,16.7454088309738,2.08384457867999));
#87596=CARTESIAN_POINT('Ctrl Pts',(-9.64453428630998,16.7461739642978,2.08029802515142));
#87597=CARTESIAN_POINT('Ctrl Pts',(-9.65307088599521,16.746643321243,2.07818785861079));
#87598=CARTESIAN_POINT('Ctrl Pts',(-9.69105792969666,16.7487167411341,2.06916031618848));
#87599=CARTESIAN_POINT('Ctrl Pts',(-9.72070072987075,16.7502941484425,2.06307985964075));
#87600=CARTESIAN_POINT('Ctrl Pts',(-9.80176894720044,16.7545163770963,2.04905458620525));
#87601=CARTESIAN_POINT('Ctrl Pts',(-9.85346440375555,16.7571084503633,2.04292552629819));
#87602=CARTESIAN_POINT('Ctrl Pts',(-10.0111817393311,16.7648710809417,2.032707118987));
#87603=CARTESIAN_POINT('Ctrl Pts',(-10.1174058516349,16.7698851706157,2.03737030296771));
#87604=CARTESIAN_POINT('Ctrl Pts',(-10.2501813310216,16.7767431854769,2.05776427657442));
#87605=CARTESIAN_POINT('Ctrl Pts',(-10.2780459094226,16.778217607675,2.06287619026194));
#87606=CARTESIAN_POINT('Ctrl Pts',(-10.3111430660749,16.7800295247208,2.06994659648807));
#87607=CARTESIAN_POINT('Ctrl Pts',(-10.3165367368317,16.7803267447539,2.07113078388423));
#87608=CARTESIAN_POINT('Ctrl Pts',(-10.3253432169485,16.7808153949202,2.07311656736173));
#87609=CARTESIAN_POINT('Ctrl Pts',(-10.3287601252649,16.7810058217434,2.07389996190164));
#87610=CARTESIAN_POINT('Ctrl Pts',(-10.3348874431459,16.7813488470887,2.07532796326748));
#87611=CARTESIAN_POINT('Ctrl Pts',(-10.3375988562978,16.7815011869912,2.07596803973086));
#87612=CARTESIAN_POINT('Ctrl Pts',(-10.3435056361329,16.7818342614672,2.07738025665292));
#87613=CARTESIAN_POINT('Ctrl Pts',(-10.3467001928995,16.7820151619234,2.07815541214193));
#87614=CARTESIAN_POINT('Ctrl Pts',(-10.3557322528661,16.7825287369463,2.08037927964959));
#87615=CARTESIAN_POINT('Ctrl Pts',(-10.3615634046876,16.7828628024721,2.08185320674961));
#87616=CARTESIAN_POINT('Ctrl Pts',(-10.3982377228345,16.7849788992025,2.09136418368387));
#87617=CARTESIAN_POINT('Ctrl Pts',(-10.4288184432168,16.7868103938086,2.10037055271427));
#87618=CARTESIAN_POINT('Ctrl Pts',(-10.5378047993339,16.7935220462815,2.1363752297819));
#87619=CARTESIAN_POINT('Ctrl Pts',(-10.6141762955048,16.7985662315793,2.16902539349438));
#87620=CARTESIAN_POINT('Ctrl Pts',(-10.7726139081881,16.8093281580329,2.25331516186067));
#87621=CARTESIAN_POINT('Ctrl Pts',(-10.853171809803,16.8149852562567,2.30699590570295));
#87622=CARTESIAN_POINT('Ctrl Pts',(-10.9361127509703,16.8209286447559,2.37499380210717));
#87623=CARTESIAN_POINT('Ctrl Pts',(-10.9442875758992,16.8215161397155,2.3818466069894));
#87624=CARTESIAN_POINT('Ctrl Pts',(-10.9572897892086,16.8224534801286,2.39299042210945));
#87625=CARTESIAN_POINT('Ctrl Pts',(-10.962164862265,16.8228056014878,2.39722498860482));
#87626=CARTESIAN_POINT('Ctrl Pts',(-10.9707826746308,16.8234293141669,2.40481120940784));
#87627=CARTESIAN_POINT('Ctrl Pts',(-10.974536459162,16.823701424263,2.40815011148967));
#87628=CARTESIAN_POINT('Ctrl Pts',(-10.9784375559301,16.8239846818701,2.41165619030982));
#87629=CARTESIAN_POINT('Ctrl Pts',(-10.9786020687069,16.8239966279747,2.41180411227211));
#87630=CARTESIAN_POINT('Ctrl Pts',(-10.978883013027,16.8240170302606,2.41205683910078));
#87631=CARTESIAN_POINT('Ctrl Pts',(-10.9789994614962,16.8240254872336,2.41216162554785));
#87632=CARTESIAN_POINT('Ctrl Pts',(-10.9791991379893,16.8240399893278,2.41234136297016));
#87633=CARTESIAN_POINT('Ctrl Pts',(-10.979282374201,16.8240460348283,2.4124163047729));
#87634=CARTESIAN_POINT('Ctrl Pts',(-10.9794255190017,16.8240564319165,2.41254521508711));
#87635=CARTESIAN_POINT('Ctrl Pts',(-10.9794854317386,16.8240607836968,2.4125991789991));
#87636=CARTESIAN_POINT('Ctrl Pts',(-10.9796288689124,16.8240712025807,2.41272839555485));
#87637=CARTESIAN_POINT('Ctrl Pts',(-10.9797123891492,16.8240772694894,2.41280365288192));
#87638=CARTESIAN_POINT('Ctrl Pts',(-10.9798739720527,16.8240890073094,2.4129492836395));
#87639=CARTESIAN_POINT('Ctrl Pts',(-10.9799520358144,16.8240946782714,2.41301965585873));
#87640=CARTESIAN_POINT('Ctrl Pts',(-10.9801031638922,16.8241056573949,2.41315592295441));
#87641=CARTESIAN_POINT('Ctrl Pts',(-10.9801762291377,16.8241109655992,2.41322181678415));
#87642=CARTESIAN_POINT('Ctrl Pts',(-10.9803177700751,16.8241212489141,2.41334949124347));
#87643=CARTESIAN_POINT('Ctrl Pts',(-10.9803862465808,16.8241262240627,2.41341127098571));
#87644=CARTESIAN_POINT('Ctrl Pts',(-10.9805189777553,16.8241358679206,2.41353104427522));
#87645=CARTESIAN_POINT('Ctrl Pts',(-10.9805832331218,16.8241405366624,2.41358903705255));
#87646=CARTESIAN_POINT('Ctrl Pts',(-10.9807078527477,16.824149591684,2.41370153080602));
#87647=CARTESIAN_POINT('Ctrl Pts',(-10.980768217595,16.8241539779905,2.41375603110089));
#87648=CARTESIAN_POINT('Ctrl Pts',(-10.9808853543462,16.8241624897608,2.41386180553246));
#87649=CARTESIAN_POINT('Ctrl Pts',(-10.9809421267811,16.8241666152493,2.4139130790962));
#87650=CARTESIAN_POINT('Ctrl Pts',(-10.9810523481726,16.8241746249244,2.4140126403436));
#87651=CARTESIAN_POINT('Ctrl Pts',(-10.9811057975903,16.8241785091325,2.41406092752715));
#87652=CARTESIAN_POINT('Ctrl Pts',(-10.9812096170324,16.8241860539494,2.41415473383529));
#87653=CARTESIAN_POINT('Ctrl Pts',(-10.9812599874718,16.8241897145779,2.41420025253456));
#87654=CARTESIAN_POINT('Ctrl Pts',(-10.9813578705746,16.8241968283109,2.41428871979553));
#87655=CARTESIAN_POINT('Ctrl Pts',(-10.9814053835613,16.8242002814296,2.41433166794877));
#87656=CARTESIAN_POINT('Ctrl Pts',(-10.9814977533478,16.8242069947669,2.41441517428151));
#87657=CARTESIAN_POINT('Ctrl Pts',(-10.9815426104624,16.8242102550004,2.41445573213073));
#87658=CARTESIAN_POINT('Ctrl Pts',(-10.9816298522714,16.8242165958999,2.41453462220327));
#87659=CARTESIAN_POINT('Ctrl Pts',(-10.9816722372521,16.8242196765796,2.41457295414467));
#87660=CARTESIAN_POINT('Ctrl Pts',(-10.9817547027085,16.8242256705554,2.41464754267074));
#87661=CARTESIAN_POINT('Ctrl Pts',(-10.9817947833755,16.8242285838591,2.41468379895186));
#87662=CARTESIAN_POINT('Ctrl Pts',(-10.9818727938503,16.8242342542325,2.4147543737416));
#87663=CARTESIAN_POINT('Ctrl Pts',(-10.9819107238404,16.8242370113098,2.41478869199417));
#87664=CARTESIAN_POINT('Ctrl Pts',(-10.981984573807,16.824242379452,2.41485551692321));
#87665=CARTESIAN_POINT('Ctrl Pts',(-10.9820204939596,16.8242449905248,2.41488802338639));
#87666=CARTESIAN_POINT('Ctrl Pts',(-10.9864840609031,16.8245694570916,2.41892779620237));
#87667=CARTESIAN_POINT('Ctrl Pts',(-10.9908871843587,16.8248901779442,2.4229621633576));
#87668=CARTESIAN_POINT('Ctrl Pts',(-11.0034563171722,16.8258076715597,2.43462096823811));
#87669=CARTESIAN_POINT('Ctrl Pts',(-11.0115599786645,16.8264016112962,2.44231220080105));
#87670=CARTESIAN_POINT('Ctrl Pts',(-11.0297128920729,16.8277381782892,2.45994071603958));
#87671=CARTESIAN_POINT('Ctrl Pts',(-11.0397079374658,16.8284784413074,2.46993234363439));
#87672=CARTESIAN_POINT('Ctrl Pts',(-11.0713776113711,16.8308402135887,2.50252187509461));
#87673=CARTESIAN_POINT('Ctrl Pts',(-11.0924728774062,16.8324383234404,2.52567163089498));
#87674=CARTESIAN_POINT('Ctrl Pts',(-11.148578632239,16.8367851899325,2.59135688103372));
#87675=CARTESIAN_POINT('Ctrl Pts',(-11.1819560770153,16.8394819065812,2.63521941757095));
#87676=CARTESIAN_POINT('Ctrl Pts',(-11.271384801929,16.8472598936627,2.76762371280278));
#87677=CARTESIAN_POINT('Ctrl Pts',(-11.3204992235894,16.8522661009677,2.86041389248033));
#87678=CARTESIAN_POINT('Ctrl Pts',(-11.3631790047849,16.8583530634548,2.9673787933051));
#87679=CARTESIAN_POINT('Ctrl Pts',(-11.3669625602156,16.8589129074277,2.9771657094962));
#87680=CARTESIAN_POINT('Ctrl Pts',(-11.3721255049102,16.8597071562594,2.99095992575757));
#87681=CARTESIAN_POINT('Ctrl Pts',(-11.3735933111791,16.8599365785517,2.99493405085427));
#87682=CARTESIAN_POINT('Ctrl Pts',(-11.3759371798355,16.8603089344008,3.00136593073956));
#87683=CARTESIAN_POINT('Ctrl Pts',(-11.3768239722316,16.860451239458,3.00381978359858));
#87684=CARTESIAN_POINT('Ctrl Pts',(-11.3786806437567,16.8607522380591,3.00900070251351));
#87685=CARTESIAN_POINT('Ctrl Pts',(-11.37964899918,16.8609110225285,3.01172828645264));
#87686=CARTESIAN_POINT('Ctrl Pts',(-11.3820095406738,16.8613025117397,3.01844035267416));
#87687=CARTESIAN_POINT('Ctrl Pts',(-11.383392587008,16.8615357446942,3.02242800150299));
#87688=CARTESIAN_POINT('Ctrl Pts',(-11.3883800039903,16.8623909267684,3.0370113655561));
#87689=CARTESIAN_POINT('Ctrl Pts',(-11.3918799531538,16.8630185848786,3.04764207589597));
#87690=CARTESIAN_POINT('Ctrl Pts',(-11.4139463028609,16.8671570758978,3.11734786036031));
#87691=CARTESIAN_POINT('Ctrl Pts',(-11.428867689185,16.8708333387061,3.1775057498141));
#87692=CARTESIAN_POINT('Ctrl Pts',(-11.4555460369151,16.8797916031711,3.32436425349679));
#87693=CARTESIAN_POINT('Ctrl Pts',(-11.4634335076646,16.885086436231,3.41153702785937));
#87694=CARTESIAN_POINT('Ctrl Pts',(-11.4634995813664,16.8901969352951,3.49889304900151));
#87695=CARTESIAN_POINT('Ctrl Pts',(-11.4634995826939,16.890197038059,3.49889480559032));
#87696=CARTESIAN_POINT('Ctrl Pts',(-11.4634998608992,16.890218590156,3.49926320529145));
#87697=CARTESIAN_POINT('Ctrl Pts',(-11.4635,16.8902401389654,3.49963160344776));
#87698=CARTESIAN_POINT('Ctrl Pts',(-11.4635,16.8902616844768,3.4999999999813));
#87699=CARTESIAN_POINT('Origin',(-10.,13.2,3.5));
#87700=CARTESIAN_POINT('',(-11.4635,17.4596976889334,3.50000000000126));
#87701=CARTESIAN_POINT('',(-11.4635,17.3900944100234,3.49999999998336));
#87702=CARTESIAN_POINT('',(-11.4635,13.2,3.5));
#87703=CARTESIAN_POINT('Ctrl Pts',(-11.4635,17.4596976889334,3.50000000000147));
#87704=CARTESIAN_POINT('Ctrl Pts',(-11.4635,17.4588719371887,3.48584184115301));
#87705=CARTESIAN_POINT('Ctrl Pts',(-11.4632945474571,17.4580511124813,3.47168412291088));
#87706=CARTESIAN_POINT('Ctrl Pts',(-11.4617357048981,17.4549574656788,3.4179879946723));
#87707=CARTESIAN_POINT('Ctrl Pts',(-11.4589848080041,17.4527234553376,3.37850518135659));
#87708=CARTESIAN_POINT('Ctrl Pts',(-11.4535468662214,17.449990889183,3.32931846457098));
#87709=CARTESIAN_POINT('Ctrl Pts',(-11.4523563944236,17.449446188232,3.31946859212755));
#87710=CARTESIAN_POINT('Ctrl Pts',(-11.4503149758051,17.4485895184532,3.30390807950675));
#87711=CARTESIAN_POINT('Ctrl Pts',(-11.4495302569239,17.4482754901577,3.29818918284064));
#87712=CARTESIAN_POINT('Ctrl Pts',(-11.4480068193935,17.4476930029131,3.28755421347788));
#87713=CARTESIAN_POINT('Ctrl Pts',(-11.4472768509405,17.4474242743337,3.28263698843374));
#87714=CARTESIAN_POINT('Ctrl Pts',(-11.4456015620945,17.4468297329295,3.27173461105017));
#87715=CARTESIAN_POINT('Ctrl Pts',(-11.4446440941169,17.4465043060991,3.26575139922252));
#87716=CARTESIAN_POINT('Ctrl Pts',(-11.4417563026737,17.4455627940984,3.24839706262894));
#87717=CARTESIAN_POINT('Ctrl Pts',(-11.439728659212,17.444949769973,3.237042451386));
#87718=CARTESIAN_POINT('Ctrl Pts',(-11.4212560322287,17.439745904489,3.14022555393402));
#87719=CARTESIAN_POINT('Ctrl Pts',(-11.3973518866666,17.4354076449411,3.05635982505373));
#87720=CARTESIAN_POINT('Ctrl Pts',(-11.3368870788253,17.4271664335753,2.89898877971933));
#87721=CARTESIAN_POINT('Ctrl Pts',(-11.3013321761466,17.4232639563814,2.82545208426932));
#87722=CARTESIAN_POINT('Ctrl Pts',(-11.2528409195864,17.4184884305442,2.74342145455409));
#87723=CARTESIAN_POINT('Ctrl Pts',(-11.2456746272575,17.4177938767176,2.73167964255244));
#87724=CARTESIAN_POINT('Ctrl Pts',(-11.2227759201119,17.4156033675284,2.69532327946387));
#87725=CARTESIAN_POINT('Ctrl Pts',(-11.2064722390614,17.4140844559099,2.67107896315827));
#87726=CARTESIAN_POINT('Ctrl Pts',(-11.1862038979949,17.4122223715673,2.64280474480666));
#87727=CARTESIAN_POINT('Ctrl Pts',(-11.1829266803051,17.4119220561996,2.63828783217934));
#87728=CARTESIAN_POINT('Ctrl Pts',(-11.1775387254835,17.4114293667268,2.63095039852335));
#87729=CARTESIAN_POINT('Ctrl Pts',(-11.1754434660505,17.4112380244696,2.62811851870324));
#87730=CARTESIAN_POINT('Ctrl Pts',(-11.1716727526436,17.4108940762779,2.62306045033981));
#87731=CARTESIAN_POINT('Ctrl Pts',(-11.170001146857,17.4107417357631,2.62083145573305));
#87732=CARTESIAN_POINT('Ctrl Pts',(-11.1663526868104,17.4104095193109,2.61599526867111));
#87733=CARTESIAN_POINT('Ctrl Pts',(-11.1643734780443,17.4102294834094,2.61338996270255));
#87734=CARTESIAN_POINT('Ctrl Pts',(-11.1587726500321,17.4097205816032,2.6060684846663));
#87735=CARTESIAN_POINT('Ctrl Pts',(-11.1551310428714,17.4093903631586,2.60136777273101));
#87736=CARTESIAN_POINT('Ctrl Pts',(-11.1325838526483,17.4073505385665,2.57262659433001));
#87737=CARTESIAN_POINT('Ctrl Pts',(-11.1129583976579,17.4055953987589,2.54916302460806));
#87738=CARTESIAN_POINT('Ctrl Pts',(-10.9923092576155,17.3950075509727,2.41377489206962));
#87739=CARTESIAN_POINT('Ctrl Pts',(-10.8752091535502,17.3856502841544,2.31738195737113));
#87740=CARTESIAN_POINT('Ctrl Pts',(-10.7159445468671,17.3750557738834,2.22311735372003));
#87741=CARTESIAN_POINT('Ctrl Pts',(-10.685857934446,17.3731288013647,2.20670766809175));
#87742=CARTESIAN_POINT('Ctrl Pts',(-10.6466688701293,17.3707111786293,2.18708602686426));
#87743=CARTESIAN_POINT('Ctrl Pts',(-10.6380746363782,17.3701864857458,2.18288782066128));
#87744=CARTESIAN_POINT('Ctrl Pts',(-10.6243518940195,17.3693572509917,2.17635022625761));
#87745=CARTESIAN_POINT('Ctrl Pts',(-10.6192500629466,17.3690508198836,2.17395574286725));
#87746=CARTESIAN_POINT('Ctrl Pts',(-10.6100626227117,17.3685022901652,2.16970831394235));
#87747=CARTESIAN_POINT('Ctrl Pts',(-10.6059821036659,17.3682598248807,2.16784457953252));
#87748=CARTESIAN_POINT('Ctrl Pts',(-10.5964126946358,17.3676938870697,2.16352691901005));
#87749=CARTESIAN_POINT('Ctrl Pts',(-10.5909171009728,17.367370927685,2.16108798654001));
#87750=CARTESIAN_POINT('Ctrl Pts',(-10.5750410937572,17.3664437412566,2.15415903627054));
#87751=CARTESIAN_POINT('Ctrl Pts',(-10.5646233332933,17.3658424310925,2.14975533319732));
#87752=CARTESIAN_POINT('Ctrl Pts',(-10.4831436430933,17.361192415147,2.11642089267606));
#87753=CARTESIAN_POINT('Ctrl Pts',(-10.4099537300422,17.357336072496,2.09299650642095));
#87754=CARTESIAN_POINT('Ctrl Pts',(-10.240214844078,17.3487666817711,2.05305067782795));
#87755=CARTESIAN_POINT('Ctrl Pts',(-10.1431799978249,17.3441320348349,2.04025250242193));
#87756=CARTESIAN_POINT('Ctrl Pts',(-10.0087459137742,17.3373492062003,2.03606170318592));
#87757=CARTESIAN_POINT('Ctrl Pts',(-9.97186391986774,17.3354489564038,2.03630612429924));
#87758=CARTESIAN_POINT('Ctrl Pts',(-9.92908098177803,17.3331598033239,2.03820718072639));
#87759=CARTESIAN_POINT('Ctrl Pts',(-9.92313013547809,17.3328394820369,2.03850803110607));
#87760=CARTESIAN_POINT('Ctrl Pts',(-9.91358942151782,17.3323226230293,2.03904880107409));
#87761=CARTESIAN_POINT('Ctrl Pts',(-9.9099982511157,17.3321273237122,2.03926563730749));
#87762=CARTESIAN_POINT('Ctrl Pts',(-9.90361478882863,17.3317787781931,2.03967470237341));
#87763=CARTESIAN_POINT('Ctrl Pts',(-9.90082220755039,17.3316258235908,2.03986170202779));
#87764=CARTESIAN_POINT('Ctrl Pts',(-9.89485727500514,17.3312980782213,2.04027832327276));
#87765=CARTESIAN_POINT('Ctrl Pts',(-9.89168518077645,17.3311231654501,2.0405102721618));
#87766=CARTESIAN_POINT('Ctrl Pts',(-9.883001255395,17.3306426710013,2.04117372165756));
#87767=CARTESIAN_POINT('Ctrl Pts',(-9.87749113210737,17.3303359629823,2.04162611381486));
#87768=CARTESIAN_POINT('Ctrl Pts',(-9.84822082163298,17.3286974769836,2.04419631684733));
#87769=CARTESIAN_POINT('Ctrl Pts',(-9.82451378207117,17.327338122719,2.04686348366081));
#87770=CARTESIAN_POINT('Ctrl Pts',(-9.75184869707101,17.3230934662459,2.05684270121569));
#87771=CARTESIAN_POINT('Ctrl Pts',(-9.70318939514233,17.3201423387567,2.06605964751645));
#87772=CARTESIAN_POINT('Ctrl Pts',(-9.53475145373394,17.3097308080808,2.10690632475298));
#87773=CARTESIAN_POINT('Ctrl Pts',(-9.41857560594761,17.3022497347082,2.15125173290631));
#87774=CARTESIAN_POINT('Ctrl Pts',(-9.28998635481199,17.2940309858853,2.22007968992839));
#87775=CARTESIAN_POINT('Ctrl Pts',(-9.27084304642886,17.2928072528494,2.23088787441236));
#87776=CARTESIAN_POINT('Ctrl Pts',(-9.24499743085002,17.2911540794358,2.2462580813855));
#87777=CARTESIAN_POINT('Ctrl Pts',(-9.23807945970624,17.2907114747922,2.25045017231042));
#87778=CARTESIAN_POINT('Ctrl Pts',(-9.22712872176797,17.290010600403,2.25721076174272));
#87779=CARTESIAN_POINT('Ctrl Pts',(-9.2230732395625,17.289750982392,2.25974199735861));
#87780=CARTESIAN_POINT('Ctrl Pts',(-9.21477948163198,17.2892198994985,2.26497520271294));
#87781=CARTESIAN_POINT('Ctrl Pts',(-9.21054257357367,17.2889485147359,2.26767922799648));
#87782=CARTESIAN_POINT('Ctrl Pts',(-9.20077963473035,17.2883229507987,2.27398102094854));
#87783=CARTESIAN_POINT('Ctrl Pts',(-9.19526379724946,17.2879693552617,2.27759443097687));
#87784=CARTESIAN_POINT('Ctrl Pts',(-9.17791282614335,17.2868563908497,2.28912934509186));
#87785=CARTESIAN_POINT('Ctrl Pts',(-9.16616859921466,17.2861020796294,2.29718651559571));
#87786=CARTESIAN_POINT('Ctrl Pts',(-9.10871167666106,17.2824040253735,2.33785108524658));
#87787=CARTESIAN_POINT('Ctrl Pts',(-9.0647820844768,17.2795546378667,2.37290049232021));
#87788=CARTESIAN_POINT('Ctrl Pts',(-8.95427107604367,17.272181957524,2.47199321365247));
#87789=CARTESIAN_POINT('Ctrl Pts',(-8.89155268798925,17.2677865891433,2.53995264471238));
#87790=CARTESIAN_POINT('Ctrl Pts',(-8.80100736605511,17.2604078516403,2.6588585628784));
#87791=CARTESIAN_POINT('Ctrl Pts',(-8.76906314919216,17.2575252796585,2.70634052589192));
#87792=CARTESIAN_POINT('Ctrl Pts',(-8.73631900626414,17.2540906028738,2.76176261325652));
#87793=CARTESIAN_POINT('Ctrl Pts',(-8.73270235508965,17.2537037971662,2.76798854648252));
#87794=CARTESIAN_POINT('Ctrl Pts',(-8.72738006167122,17.2531229609349,2.77730834974984));
#87795=CARTESIAN_POINT('Ctrl Pts',(-8.72563938765842,17.2529310973758,2.78038221398421));
#87796=CARTESIAN_POINT('Ctrl Pts',(-8.72254539080068,17.2525865925548,2.78589234823257));
#87797=CARTESIAN_POINT('Ctrl Pts',(-8.72118788173025,17.2524342204151,2.78832621034666));
#87798=CARTESIAN_POINT('Ctrl Pts',(-8.71825528267471,17.2521023820623,2.79361951713532));
#87799=CARTESIAN_POINT('Ctrl Pts',(-8.71668282709452,17.2519227588881,2.79648031991992));
#87800=CARTESIAN_POINT('Ctrl Pts',(-8.71228943145303,17.2514161645559,2.80453706259117));
#87801=CARTESIAN_POINT('Ctrl Pts',(-8.7094904204342,17.2510878599189,2.80974480931377));
#87802=CARTESIAN_POINT('Ctrl Pts',(-8.69270201478475,17.2490852816903,2.84143982206972));
#87803=CARTESIAN_POINT('Ctrl Pts',(-8.67949788894564,17.2473673360417,2.86833280008957));
#87804=CARTESIAN_POINT('Ctrl Pts',(-8.60895715249976,17.2374021561013,3.02389738295745));
#87805=CARTESIAN_POINT('Ctrl Pts',(-8.56960624630163,17.2286736701308,3.15991650228304));
#87806=CARTESIAN_POINT('Ctrl Pts',(-8.54435426268167,17.2180163853223,3.34248124600827));
#87807=CARTESIAN_POINT('Ctrl Pts',(-8.54032226325154,17.2155582110068,3.38572783271756));
#87808=CARTESIAN_POINT('Ctrl Pts',(-8.53772415869821,17.2125953871458,3.4392890782443));
#87809=CARTESIAN_POINT('Ctrl Pts',(-8.53733626225622,17.2120346931571,3.44949010209176));
#87810=CARTESIAN_POINT('Ctrl Pts',(-8.53689434022903,17.2111585446041,3.46553029840875));
#87811=CARTESIAN_POINT('Ctrl Pts',(-8.53676847821691,17.210840872091,3.47136702911846));
#87812=CARTESIAN_POINT('Ctrl Pts',(-8.53660789717808,17.2102818071517,3.48167524696837));
#87813=CARTESIAN_POINT('Ctrl Pts',(-8.53655873990505,17.2100399701515,3.48614640689652));
#87814=CARTESIAN_POINT('Ctrl Pts',(-8.53649301699805,17.2094869526471,3.49639805930451));
#87815=CARTESIAN_POINT('Ctrl Pts',(-8.53649020558537,17.2091762024518,3.5021785864081));
#87816=CARTESIAN_POINT('Ctrl Pts',(-8.53657725138206,17.2083186661712,3.51818424825574));
#87817=CARTESIAN_POINT('Ctrl Pts',(-8.53674002402275,17.2077741435633,3.52840876386831));
#87818=CARTESIAN_POINT('Ctrl Pts',(-8.53830768351442,17.2046302898279,3.58777754786572));
#87819=CARTESIAN_POINT('Ctrl Pts',(-8.54208111514923,17.2021055854962,3.63683019445787));
#87820=CARTESIAN_POINT('Ctrl Pts',(-8.56430267392771,17.1933033964237,3.81063429632922));
#87821=CARTESIAN_POINT('Ctrl Pts',(-8.59637155545103,17.1874121537591,3.93306316566266));
#87822=CARTESIAN_POINT('Ctrl Pts',(-8.65796316384873,17.1791560648551,4.08498345037961));
#87823=CARTESIAN_POINT('Ctrl Pts',(-8.67355983529974,17.1772052307554,4.11953574262304));
#87824=CARTESIAN_POINT('Ctrl Pts',(-8.69315747562584,17.1748593711467,4.15881019524725));
#87825=CARTESIAN_POINT('Ctrl Pts',(-8.69586963399928,17.174536823591,4.16416281353827));
#87826=CARTESIAN_POINT('Ctrl Pts',(-8.70026607206328,17.1740170569888,4.17270870316964));
#87827=CARTESIAN_POINT('Ctrl Pts',(-8.70192941258629,17.1738210986347,4.1759127401315));
#87828=CARTESIAN_POINT('Ctrl Pts',(-8.70490404535399,17.1734718145413,4.18159119747568));
#87829=CARTESIAN_POINT('Ctrl Pts',(-8.70621060448901,17.1733187849594,4.18406804645771));
#87830=CARTESIAN_POINT('Ctrl Pts',(-8.7090128036779,17.1729913834971,4.18934343929973));
#87831=CARTESIAN_POINT('Ctrl Pts',(-8.71051041474702,17.1728168928174,4.19214082924066));
#87832=CARTESIAN_POINT('Ctrl Pts',(-8.71462619802512,17.1723387187295,4.19976898363119));
#87833=CARTESIAN_POINT('Ctrl Pts',(-8.71726246976421,17.1720339266524,4.20458985787021));
#87834=CARTESIAN_POINT('Ctrl Pts',(-8.73126238782974,17.1704235518174,4.22985211183068));
#87835=CARTESIAN_POINT('Ctrl Pts',(-8.74308708315786,17.1690914772971,4.25003268284968));
#87836=CARTESIAN_POINT('Ctrl Pts',(-8.78061491428403,17.1649660644128,4.31069811705124));
#87837=CARTESIAN_POINT('Ctrl Pts',(-8.80782773898504,17.162110727891,4.35020948480728));
#87838=CARTESIAN_POINT('Ctrl Pts',(-8.89694144030263,17.1532969468388,4.46688658068318));
#87839=CARTESIAN_POINT('Ctrl Pts',(-8.96476965324224,17.147305422279,4.53918703624663));
#87840=CARTESIAN_POINT('Ctrl Pts',(-9.07293359322012,17.1390057685644,4.63329556498269));
#87841=CARTESIAN_POINT('Ctrl Pts',(-9.10780825204643,17.1364849441852,4.66095023107085));
#87842=CARTESIAN_POINT('Ctrl Pts',(-9.15148991167338,17.1335087445268,4.69245572290251));
#87843=CARTESIAN_POINT('Ctrl Pts',(-9.15914092484352,17.1329938202377,4.69786311511011));
#87844=CARTESIAN_POINT('Ctrl Pts',(-9.17188525710374,17.1321464540739,4.70668795916275));
#87845=CARTESIAN_POINT('Ctrl Pts',(-9.1769489982348,17.1318124283438,4.71014747377519));
#87846=CARTESIAN_POINT('Ctrl Pts',(-9.18616003279409,17.1312095803267,4.71635583248166));
#87847=CARTESIAN_POINT('Ctrl Pts',(-9.19029986374403,17.1309403535939,4.71911553744044));
#87848=CARTESIAN_POINT('Ctrl Pts',(-9.19922522766028,17.1303635534775,4.72499986819879));
#87849=CARTESIAN_POINT('Ctrl Pts',(-9.20401516365908,17.1300562358402,4.72811768763778));
#87850=CARTESIAN_POINT('Ctrl Pts',(-9.21717399626281,17.1292179836665,4.7365735837972));
#87851=CARTESIAN_POINT('Ctrl Pts',(-9.22557921600713,17.1286891452882,4.74185475644286));
#87852=CARTESIAN_POINT('Ctrl Pts',(-9.27173319756821,17.1258200506561,4.77020342660559));
#87853=CARTESIAN_POINT('Ctrl Pts',(-9.31046106934512,17.1235394953266,4.79163688108015));
#87854=CARTESIAN_POINT('Ctrl Pts',(-9.43809348435907,17.1163472351902,4.85489387143371));
#87855=CARTESIAN_POINT('Ctrl Pts',(-9.53024751009269,17.1116542407632,4.88953564061091));
#87856=CARTESIAN_POINT('Ctrl Pts',(-9.69300105913799,17.103411975441,4.93265723552733));
#87857=CARTESIAN_POINT('Ctrl Pts',(-9.76202090600701,17.0999224390044,4.94572430051905));
#87858=CARTESIAN_POINT('Ctrl Pts',(-9.83891811822245,17.0957928662048,4.95462629041437));
#87859=CARTESIAN_POINT('Ctrl Pts',(-9.84614001542342,17.0954026816337,4.95540788722569));
#87860=CARTESIAN_POINT('Ctrl Pts',(-9.85689465785521,17.0948177446156,4.95649087865386));
#87861=CARTESIAN_POINT('Ctrl Pts',(-9.86042327484176,17.0946252042526,4.95683326287034));
#87862=CARTESIAN_POINT('Ctrl Pts',(-9.86672885274059,17.094279973561,4.95742197852261));
#87863=CARTESIAN_POINT('Ctrl Pts',(-9.86950530737975,17.0941275571565,4.95767319973102));
#87864=CARTESIAN_POINT('Ctrl Pts',(-9.87552523888234,17.093796195244,4.95820056229092));
#87865=CARTESIAN_POINT('Ctrl Pts',(-9.87876887914131,17.0936170966035,4.95847381221962));
#87866=CARTESIAN_POINT('Ctrl Pts',(-9.8878635091424,17.0931134296229,4.95920941109442));
#87867=CARTESIAN_POINT('Ctrl Pts',(-9.89371633997681,17.0927875518086,4.95964738181367));
#87868=CARTESIAN_POINT('Ctrl Pts',(-9.92868329617756,17.0908308720101,4.96205255773235));
#87869=CARTESIAN_POINT('Ctrl Pts',(-9.95784648607544,17.0891586370505,4.96318372025525));
#87870=CARTESIAN_POINT('Ctrl Pts',(-10.1177500595326,17.0798383367533,4.9646017841344));
#87871=CARTESIAN_POINT('Ctrl Pts',(-10.2480475836458,17.0717550698591,4.94824077043991));
#87872=CARTESIAN_POINT('Ctrl Pts',(-10.38789059818,17.0633100862285,4.91122870207017));
#87873=CARTESIAN_POINT('Ctrl Pts',(-10.4012804875305,17.0625030973958,4.90747985847637));
#87874=CARTESIAN_POINT('Ctrl Pts',(-10.4537320255814,17.0593492265492,4.89198532720959));
#87875=CARTESIAN_POINT('Ctrl Pts',(-10.4923510385893,17.0570438384852,4.8787990490063));
#87876=CARTESIAN_POINT('Ctrl Pts',(-10.5397055721509,17.0542377249167,4.86038613694877));
#87877=CARTESIAN_POINT('Ctrl Pts',(-10.5490022521349,17.0536878017002,4.85666100422027));
#87878=CARTESIAN_POINT('Ctrl Pts',(-10.563615887336,17.0528247679377,4.85063057503489));
#87879=CARTESIAN_POINT('Ctrl Pts',(-10.5689585275346,17.0525095467221,4.84838867318386));
#87880=CARTESIAN_POINT('Ctrl Pts',(-10.578859026172,17.0519259191515,4.84416486249757));
#87881=CARTESIAN_POINT('Ctrl Pts',(-10.5834203591988,17.0516572349134,4.84219135560843));
#87882=CARTESIAN_POINT('Ctrl Pts',(-10.5933865100063,17.0510705905544,4.83781899551509));
#87883=CARTESIAN_POINT('Ctrl Pts',(-10.5987870354664,17.0507529610569,4.8354105370934));
#87884=CARTESIAN_POINT('Ctrl Pts',(-10.614171316581,17.0498488102283,4.82843755980087));
#87885=CARTESIAN_POINT('Ctrl Pts',(-10.6241186312251,17.049265007791,4.82379329931589));
#87886=CARTESIAN_POINT('Ctrl Pts',(-10.6464347007082,17.0479565860162,4.8130667831795));
#87887=CARTESIAN_POINT('Ctrl Pts',(-10.6587717597692,17.0472341614664,4.80692080262556));
#87888=CARTESIAN_POINT('Ctrl Pts',(-10.7583526944973,17.0414056960573,4.755543919716));
#87889=CARTESIAN_POINT('Ctrl Pts',(-10.8409262174507,17.0366127041982,4.70180478580885));
#87890=CARTESIAN_POINT('Ctrl Pts',(-10.9897659684842,17.0273246723573,4.58203531155994));
#87891=CARTESIAN_POINT('Ctrl Pts',(-11.0563342554216,17.0228408600507,4.51714838519754));
#87892=CARTESIAN_POINT('Ctrl Pts',(-11.1234752021129,17.0173613556811,4.43795447626451));
#87893=CARTESIAN_POINT('Ctrl Pts',(-11.1305471517439,17.0167705152673,4.4294182332478));
#87894=CARTESIAN_POINT('Ctrl Pts',(-11.1402483058166,17.0159394243218,4.41743383277184));
#87895=CARTESIAN_POINT('Ctrl Pts',(-11.1429603594425,17.0157047897291,4.41405287166858));
#87896=CARTESIAN_POINT('Ctrl Pts',(-11.1472919002623,17.0153262488602,4.40860356931809));
#87897=CARTESIAN_POINT('Ctrl Pts',(-11.1489209284143,17.0151830122948,4.40654280131246));
#87898=CARTESIAN_POINT('Ctrl Pts',(-11.1523209227531,17.0148821984651,4.40221782513491));
#87899=CARTESIAN_POINT('Ctrl Pts',(-11.1540907710381,17.0147245419303,4.39995277917936));
#87900=CARTESIAN_POINT('Ctrl Pts',(-11.1583838339886,17.0143395352862,4.3944250416352));
#87901=CARTESIAN_POINT('Ctrl Pts',(-11.1608999422113,17.0141116947388,4.39115688028216));
#87902=CARTESIAN_POINT('Ctrl Pts',(-11.1698111860631,17.0132970377654,4.37948032283051));
#87903=CARTESIAN_POINT('Ctrl Pts',(-11.1761288990633,17.0127051812362,4.37101357559034));
#87904=CARTESIAN_POINT('Ctrl Pts',(-11.2148507413235,17.0089912990027,4.31793064812813));
#87905=CARTESIAN_POINT('Ctrl Pts',(-11.2448007594101,17.0057363308705,4.27158463023519));
#87906=CARTESIAN_POINT('Ctrl Pts',(-11.3106678187458,16.9977663443143,4.15580308637658));
#87907=CARTESIAN_POINT('Ctrl Pts',(-11.3437832115782,16.9930251080985,4.08495758407182));
#87908=CARTESIAN_POINT('Ctrl Pts',(-11.3825432396478,16.9864614586067,3.98112288061025));
#87909=CARTESIAN_POINT('Ctrl Pts',(-11.3929647398744,16.9845428485684,3.9500605103055));
#87910=CARTESIAN_POINT('Ctrl Pts',(-11.4141575606403,16.9802684479199,3.87907566903711));
#87911=CARTESIAN_POINT('Ctrl Pts',(-11.4242978289732,16.9779318108585,3.83899283489547));
#87912=CARTESIAN_POINT('Ctrl Pts',(-11.4347804835949,16.9750933406917,3.78868390867136));
#87913=CARTESIAN_POINT('Ctrl Pts',(-11.4367308346483,16.9745409480612,3.77881526339706));
#87914=CARTESIAN_POINT('Ctrl Pts',(-11.4396458364024,16.9736749061692,3.76322196330849));
#87915=CARTESIAN_POINT('Ctrl Pts',(-11.440678416869,16.9733591218415,3.75751045951987));
#87916=CARTESIAN_POINT('Ctrl Pts',(-11.4425237947289,16.9727775328631,3.74694447946007));
#87917=CARTESIAN_POINT('Ctrl Pts',(-11.4433461293506,16.9725114314014,3.74209177186111));
#87918=CARTESIAN_POINT('Ctrl Pts',(-11.4449133311798,16.9719902371055,3.73255158851063));
#87919=CARTESIAN_POINT('Ctrl Pts',(-11.4456599065061,16.9717350936399,3.72786445836986));
#87920=CARTESIAN_POINT('Ctrl Pts',(-11.4472790070098,16.9711659122954,3.71737110676397));
#87921=CARTESIAN_POINT('Ctrl Pts',(-11.4481394222268,16.9708522559021,3.71156308122382));
#87922=CARTESIAN_POINT('Ctrl Pts',(-11.4502077361232,16.9700690209958,3.69699727558352));
#87923=CARTESIAN_POINT('Ctrl Pts',(-11.4513712851896,16.9696008198982,3.68823336989376));
#87924=CARTESIAN_POINT('Ctrl Pts',(-11.4598112228208,16.9659742048019,3.61992467438711));
#87925=CARTESIAN_POINT('Ctrl Pts',(-11.4634999999992,16.9629297445978,3.55999266409901));
#87926=CARTESIAN_POINT('Ctrl Pts',(-11.4635,16.9599527886714,3.50000000001837));
#87927=CARTESIAN_POINT('Ctrl Pts',(-11.4635,16.8902616844768,3.4999999999813));
#87928=CARTESIAN_POINT('Ctrl Pts',(-11.4635000000007,16.89335037922,3.55281213409296));
#87929=CARTESIAN_POINT('Ctrl Pts',(-11.4606413650418,16.8963691047965,3.60559104637156));
#87930=CARTESIAN_POINT('Ctrl Pts',(-11.4539818303754,16.8997896038938,3.66687379711066));
#87931=CARTESIAN_POINT('Ctrl Pts',(-11.4529498272705,16.9002765088671,3.67563266053759));
#87932=CARTESIAN_POINT('Ctrl Pts',(-11.4511000140096,16.9010830101854,3.6901982549013));
#87933=CARTESIAN_POINT('Ctrl Pts',(-11.4503263766903,16.9014039737232,3.69601027857511));
#87934=CARTESIAN_POINT('Ctrl Pts',(-11.4488634630115,16.9019827164314,3.70651738951463));
#87935=CARTESIAN_POINT('Ctrl Pts',(-11.4481862422548,16.9022408691368,3.7112140504469));
#87936=CARTESIAN_POINT('Ctrl Pts',(-11.4468244644374,16.9027416456609,3.72034368110697));
#87937=CARTESIAN_POINT('Ctrl Pts',(-11.446142347434,16.9029843429946,3.72477695673199));
#87938=CARTESIAN_POINT('Ctrl Pts',(-11.444554207869,16.9035315721379,3.73479218144835));
#87939=CARTESIAN_POINT('Ctrl Pts',(-11.4436361892395,16.9038357232631,3.74037217453491));
#87940=CARTESIAN_POINT('Ctrl Pts',(-11.4410647658515,16.9046559646691,3.75545574832366));
#87941=CARTESIAN_POINT('Ctrl Pts',(-11.4393496905578,16.9051701108722,3.76494862332372));
#87942=CARTESIAN_POINT('Ctrl Pts',(-11.4309564475946,16.9075425178259,3.80891573088206));
#87943=CARTESIAN_POINT('Ctrl Pts',(-11.4231325205218,16.9093644722255,3.84316084965163));
#87944=CARTESIAN_POINT('Ctrl Pts',(-11.4057440918486,16.9128043699665,3.90836671804323));
#87945=CARTESIAN_POINT('Ctrl Pts',(-11.3963689959624,16.9144261951841,3.93935589572659));
#87946=CARTESIAN_POINT('Ctrl Pts',(-11.3649004917138,16.919279613917,4.03215080401589));
#87947=CARTESIAN_POINT('Ctrl Pts',(-11.3396715959119,16.9224448694413,4.09280521524113));
#87948=CARTESIAN_POINT('Ctrl Pts',(-11.2852129221592,16.9284083102357,4.20233560235017));
#87949=CARTESIAN_POINT('Ctrl Pts',(-11.2570400848649,16.9311941940619,4.25159624418857));
#87950=CARTESIAN_POINT('Ctrl Pts',(-11.2119382436526,16.9354307788527,4.32079781009414));
#87951=CARTESIAN_POINT('Ctrl Pts',(-11.1972204389118,16.9367844011855,4.34212018644379));
#87952=CARTESIAN_POINT('Ctrl Pts',(-11.1786012370859,16.9384774087478,4.36761946434593));
#87953=CARTESIAN_POINT('Ctrl Pts',(-11.1752304199506,16.9387831751503,4.37217995211778));
#87954=CARTESIAN_POINT('Ctrl Pts',(-11.1699087221228,16.9392649587196,4.37929298446356));
#87955=CARTESIAN_POINT('Ctrl Pts',(-11.1679757604145,16.9394397609743,4.38185894183996));
#87956=CARTESIAN_POINT('Ctrl Pts',(-11.1643456071108,16.9397677284019,4.38664500593607));
#87957=CARTESIAN_POINT('Ctrl Pts',(-11.1626504970261,16.9399207503906,4.38886662705221));
#87958=CARTESIAN_POINT('Ctrl Pts',(-11.1587509086081,16.9402724849199,4.3939472104895));
#87959=CARTESIAN_POINT('Ctrl Pts',(-11.1565422128257,16.9404714895862,4.39680287283134));
#87960=CARTESIAN_POINT('Ctrl Pts',(-11.1507156676456,16.9409958365497,4.40427879440517));
#87961=CARTESIAN_POINT('Ctrl Pts',(-11.1470805926991,16.9413223380852,4.40888546983398));
#87962=CARTESIAN_POINT('Ctrl Pts',(-11.1216363415272,16.9436026535979,4.44073480434506));
#87963=CARTESIAN_POINT('Ctrl Pts',(-11.0988881056078,16.9456154872101,4.46720970148674));
#87964=CARTESIAN_POINT('Ctrl Pts',(-11.0647434647968,16.9485702712058,4.50418722040169));
#87965=CARTESIAN_POINT('Ctrl Pts',(-11.054090824053,16.9494834867763,4.5153635472015));
#87966=CARTESIAN_POINT('Ctrl Pts',(-11.0159207566497,16.9527198717537,4.55416191571789));
#87967=CARTESIAN_POINT('Ctrl Pts',(-10.9874787585536,16.9550672571449,4.58085054767258));
#87968=CARTESIAN_POINT('Ctrl Pts',(-10.9019234678886,16.9618829091466,4.65493280004682));
#87969=CARTESIAN_POINT('Ctrl Pts',(-10.8422256118354,16.9663371410483,4.69916361321554));
#87970=CARTESIAN_POINT('Ctrl Pts',(-10.7517143338406,16.9725545796161,4.75611699236872));
#87971=CARTESIAN_POINT('Ctrl Pts',(-10.7234227541251,16.9744304313362,4.7726209509193));
#87972=CARTESIAN_POINT('Ctrl Pts',(-10.6817630579084,16.9770949285099,4.7950845818074));
#87973=CARTESIAN_POINT('Ctrl Pts',(-10.6688233222588,16.9779094254456,4.80181424414476));
#87974=CARTESIAN_POINT('Ctrl Pts',(-10.6455079960456,16.9793539818661,4.81350059898834));
#87975=CARTESIAN_POINT('Ctrl Pts',(-10.6351706410618,16.9799865177513,4.81853049408695));
#87976=CARTESIAN_POINT('Ctrl Pts',(-10.6193292975166,16.9809440067562,4.82600894964108));
#87977=CARTESIAN_POINT('Ctrl Pts',(-10.6138678417599,16.9812719926295,4.8285461180024));
#87978=CARTESIAN_POINT('Ctrl Pts',(-10.6038636537693,16.9818689793916,4.83311879244297));
#87979=CARTESIAN_POINT('Ctrl Pts',(-10.5993259182395,16.9821383412929,4.83516496047631));
#87980=CARTESIAN_POINT('Ctrl Pts',(-10.5895606365362,16.9827150026944,4.83950853287391));
#87981=CARTESIAN_POINT('Ctrl Pts',(-10.5843298948976,16.983022049085,4.84179857988866));
#87982=CARTESIAN_POINT('Ctrl Pts',(-10.5702282550169,16.9838449596233,4.84787425520504));
#87983=CARTESIAN_POINT('Ctrl Pts',(-10.5613330313325,16.9843589008717,4.85160293894766));
#87984=CARTESIAN_POINT('Ctrl Pts',(-10.5187725085019,16.9867942688017,4.86895074027179));
#87985=CARTESIAN_POINT('Ctrl Pts',(-10.4846434944711,16.9886766311215,4.88140218961791));
#87986=CARTESIAN_POINT('Ctrl Pts',(-10.4288846717029,16.9916593118974,4.89942365779989));
#87987=CARTESIAN_POINT('Ctrl Pts',(-10.4075305316961,16.9927803697149,4.9057907214393));
#87988=CARTESIAN_POINT('Ctrl Pts',(-10.2948851271674,16.9986036591346,4.9365950587712));
#87989=CARTESIAN_POINT('Ctrl Pts',(-10.2015346873645,17.0031048980956,4.95263414952543));
#87990=CARTESIAN_POINT('Ctrl Pts',(-10.0524265594114,17.0104712656073,4.96359489872749));
#87991=CARTESIAN_POINT('Ctrl Pts',(-9.9973837213499,17.013232520144,4.96453084290432));
#87992=CARTESIAN_POINT('Ctrl Pts',(-9.93187984411485,17.0166986107852,4.96195186618962));
#87993=CARTESIAN_POINT('Ctrl Pts',(-9.92134016759578,17.0172619092052,4.96142267419591));
#87994=CARTESIAN_POINT('Ctrl Pts',(-9.90669143169571,17.0180537263068,4.96052824888311));
#87995=CARTESIAN_POINT('Ctrl Pts',(-9.90257655223886,17.0182771291985,4.96025954052425));
#87996=CARTESIAN_POINT('Ctrl Pts',(-9.89559478404722,17.0186579228885,4.95977397799846));
#87997=CARTESIAN_POINT('Ctrl Pts',(-9.8927272625583,17.0188148204667,4.95956605730135));
#87998=CARTESIAN_POINT('Ctrl Pts',(-9.88723951302259,17.0191160713747,4.95915188745093));
#87999=CARTESIAN_POINT('Ctrl Pts',(-9.88461920395984,17.0192603426548,4.95894702774076));
#88000=CARTESIAN_POINT('Ctrl Pts',(-9.87767504600098,17.0196437916327,4.95838529845521));
#88001=CARTESIAN_POINT('Ctrl Pts',(-9.8733522426987,17.0198836349663,4.95801626112554));
#88002=CARTESIAN_POINT('Ctrl Pts',(-9.85796992065983,17.0207410106391,4.95663414976264));
#88003=CARTESIAN_POINT('Ctrl Pts',(-9.84692064786682,17.0213640781786,4.95551444047278));
#88004=CARTESIAN_POINT('Ctrl Pts',(-9.74400316615693,17.0272281388411,4.94390018908303));
#88005=CARTESIAN_POINT('Ctrl Pts',(-9.6533173247774,17.0328324558723,4.92484761846273));
#88006=CARTESIAN_POINT('Ctrl Pts',(-9.45910243890625,17.0450734821342,4.86439468900163));
#88007=CARTESIAN_POINT('Ctrl Pts',(-9.35723804009431,17.0516348228704,4.81947276901191));
#88008=CARTESIAN_POINT('Ctrl Pts',(-9.25113506556167,17.0584462851287,4.75744798118398));
#88009=CARTESIAN_POINT('Ctrl Pts',(-9.240925936346,17.0591019052583,4.75131158913208));
#88010=CARTESIAN_POINT('Ctrl Pts',(-9.22557039878675,17.060088584932,4.74182475574203));
#88011=CARTESIAN_POINT('Ctrl Pts',(-9.22036845455,17.0604229395197,4.73856553567167));
#88012=CARTESIAN_POINT('Ctrl Pts',(-9.21098603712189,17.0610262242354,4.73260455519468));
#88013=CARTESIAN_POINT('Ctrl Pts',(-9.20679856807581,17.0612955604987,4.72991402640408));
#88014=CARTESIAN_POINT('Ctrl Pts',(-9.19783320450969,17.0618724255376,4.72408877760042));
#88015=CARTESIAN_POINT('Ctrl Pts',(-9.19305976907069,17.0621796995026,4.72094732409402));
#88016=CARTESIAN_POINT('Ctrl Pts',(-9.18026382357236,17.0630038317806,4.71241834118109));
#88017=CARTESIAN_POINT('Ctrl Pts',(-9.17227599569888,17.0635187572762,4.70697912645057));
#88018=CARTESIAN_POINT('Ctrl Pts',(-9.13436238111056,17.0659658059864,4.68060890404718));
#88019=CARTESIAN_POINT('Ctrl Pts',(-9.10517188190542,17.0678583988897,4.65864092643342));
#88020=CARTESIAN_POINT('Ctrl Pts',(-9.05982403226755,17.0708323663943,4.62177620032891));
#88021=CARTESIAN_POINT('Ctrl Pts',(-9.04312832804937,17.0719352408389,4.60756911568014));
#88022=CARTESIAN_POINT('Ctrl Pts',(-8.93123262666583,17.0794070765859,4.50793285170755));
#88023=CARTESIAN_POINT('Ctrl Pts',(-8.84728187068836,17.0853689010154,4.41072904220659));
#88024=CARTESIAN_POINT('Ctrl Pts',(-8.76114283325084,17.0933735187918,4.2796811296197));
#88025=CARTESIAN_POINT('Ctrl Pts',(-8.74596892839718,17.0948801619964,4.25503350423086));
#88026=CARTESIAN_POINT('Ctrl Pts',(-8.72861535363916,17.0967445744688,4.22487766853542));
#88027=CARTESIAN_POINT('Ctrl Pts',(-8.72572463740558,17.0970602087341,4.21978389208233));
#88028=CARTESIAN_POINT('Ctrl Pts',(-8.72127600741376,17.0975541249693,4.21183409849562));
#88029=CARTESIAN_POINT('Ctrl Pts',(-8.71969687718765,17.0977310893847,4.20898994794834));
#88030=CARTESIAN_POINT('Ctrl Pts',(-8.7167814726013,17.0980609088623,4.20369754902429));
#88031=CARTESIAN_POINT('Ctrl Pts',(-8.71544270709535,17.0982136039617,4.2012507329159));
#88032=CARTESIAN_POINT('Ctrl Pts',(-8.71241546813742,17.0985617088266,4.19568019361937));
#88033=CARTESIAN_POINT('Ctrl Pts',(-8.71073137050195,17.0987573879611,4.19255415595445));
#88034=CARTESIAN_POINT('Ctrl Pts',(-8.70638715100488,17.0992673802706,4.1844196142826));
#88035=CARTESIAN_POINT('Ctrl Pts',(-8.70374476120458,17.099582754664,4.17940177013524));
#88036=CARTESIAN_POINT('Ctrl Pts',(-8.68686353710805,17.1016306962625,4.14688767928945));
#88037=CARTESIAN_POINT('Ctrl Pts',(-8.67347216346431,17.1034097810314,4.11896257040469));
#88038=CARTESIAN_POINT('Ctrl Pts',(-8.65608963689965,17.1059271632573,4.07955488685148));
#88039=CARTESIAN_POINT('Ctrl Pts',(-8.65133966569054,17.1066396110208,4.06841377708649));
#88040=CARTESIAN_POINT('Ctrl Pts',(-8.60080211628567,17.1144874411172,3.94567660801309));
#88041=CARTESIAN_POINT('Ctrl Pts',(-8.56883517412668,17.1218969886633,3.82886916603102));
#88042=CARTESIAN_POINT('Ctrl Pts',(-8.54442653661582,17.1318145132362,3.6600858367712));
#88043=CARTESIAN_POINT('Ctrl Pts',(-8.53981477302907,17.1346499176092,3.61036991531203));
#88044=CARTESIAN_POINT('Ctrl Pts',(-8.53732692991212,17.1379739913432,3.55025121128117));
#88045=CARTESIAN_POINT('Ctrl Pts',(-8.53701034204621,17.1385379245376,3.53998702876895));
#88046=CARTESIAN_POINT('Ctrl Pts',(-8.53668420183079,17.1394146461739,3.52393033477724));
#88047=CARTESIAN_POINT('Ctrl Pts',(-8.53660096505459,17.1397297094864,3.51813978944827));
#88048=CARTESIAN_POINT('Ctrl Pts',(-8.53651435601033,17.1402862436664,3.50787584676922));
#88049=CARTESIAN_POINT('Ctrl Pts',(-8.5364971193733,17.1405281412553,3.5034026664653));
#88050=CARTESIAN_POINT('Ctrl Pts',(-8.5365046570984,17.1410839102337,3.49309826001539));
#88051=CARTESIAN_POINT('Ctrl Pts',(-8.53654377336601,17.1413973330742,3.48726709836156));
#88052=CARTESIAN_POINT('Ctrl Pts',(-8.53674677810797,17.1422545982633,3.47126419914061));
#88053=CARTESIAN_POINT('Ctrl Pts',(-8.53698187445544,17.1427962302983,3.46109358731615));
#88054=CARTESIAN_POINT('Ctrl Pts',(-8.53876093803724,17.1456043971672,3.40806755523621));
#88055=CARTESIAN_POINT('Ctrl Pts',(-8.54208194713816,17.14781536184,3.36529080194802));
#88056=CARTESIAN_POINT('Ctrl Pts',(-8.56441014325499,17.1571281113155,3.18232341650703));
#88057=CARTESIAN_POINT('Ctrl Pts',(-8.6018005334906,17.1636681683375,3.04517314002671));
#88058=CARTESIAN_POINT('Ctrl Pts',(-8.67025364937187,17.1724029956135,2.88803060341119));
#88059=CARTESIAN_POINT('Ctrl Pts',(-8.68307400391874,17.1739626017201,2.86090878996597));
#88060=CARTESIAN_POINT('Ctrl Pts',(-8.69940889791892,17.1758862903973,2.82893365977738));
#88061=CARTESIAN_POINT('Ctrl Pts',(-8.70213212062496,17.1762050556995,2.82368186991408));
#88062=CARTESIAN_POINT('Ctrl Pts',(-8.70640801965747,17.1767028185314,2.81555664599556));
#88063=CARTESIAN_POINT('Ctrl Pts',(-8.70793863171435,17.1768804651792,2.81267159479299));
#88064=CARTESIAN_POINT('Ctrl Pts',(-8.71079367157516,17.1772108892496,2.80733336665678));
#88065=CARTESIAN_POINT('Ctrl Pts',(-8.71211545892147,17.1773635014945,2.80487883741931));
#88066=CARTESIAN_POINT('Ctrl Pts',(-8.71512843807533,17.1777105528542,2.79932189678595));
#88067=CARTESIAN_POINT('Ctrl Pts',(-8.7168238491555,17.1779052546297,2.79622183869518));
#88068=CARTESIAN_POINT('Ctrl Pts',(-8.72124182175142,17.1784110513087,2.78821261322978));
#88069=CARTESIAN_POINT('Ctrl Pts',(-8.72398140633879,17.1787231795314,2.7833129630281));
#88070=CARTESIAN_POINT('Ctrl Pts',(-8.74149798929534,17.1807087991807,2.75240399611916));
#88071=CARTESIAN_POINT('Ctrl Pts',(-8.757040392671,17.1824257109178,2.72683878781948));
#88072=CARTESIAN_POINT('Ctrl Pts',(-8.83039316897241,17.1902761721673,2.61411707835031));
#88073=CARTESIAN_POINT('Ctrl Pts',(-8.89666210949767,17.1966890873366,2.53283155719234));
#88074=CARTESIAN_POINT('Ctrl Pts',(-9.00786071697484,17.2059794949853,2.4228859923147));
#88075=CARTESIAN_POINT('Ctrl Pts',(-9.04660170425233,17.2090063177096,2.38844818476036));
#88076=CARTESIAN_POINT('Ctrl Pts',(-9.11066594023569,17.2136721137163,2.33731904039774));
#88077=CARTESIAN_POINT('Ctrl Pts',(-9.13481872247482,17.2153619961065,2.31923599736667));
#88078=CARTESIAN_POINT('Ctrl Pts',(-9.16670577816148,17.2175069302329,2.29686652646461));
#88079=CARTESIAN_POINT('Ctrl Pts',(-9.17394245689282,17.2179882061084,2.29188644760052));
#88080=CARTESIAN_POINT('Ctrl Pts',(-9.18575307003271,17.2187648952296,2.28391445624249));
#88081=CARTESIAN_POINT('Ctrl Pts',(-9.190299621419,17.2190618047691,2.28088252791108));
#88082=CARTESIAN_POINT('Ctrl Pts',(-9.19905795357079,17.2196298216614,2.27511252659459));
#88083=CARTESIAN_POINT('Ctrl Pts',(-9.2032670517212,17.2199010721537,2.27237053870466));
#88084=CARTESIAN_POINT('Ctrl Pts',(-9.21291637723249,17.220519016497,2.26615508261436));
#88085=CARTESIAN_POINT('Ctrl Pts',(-9.21836565383983,17.220865183764,2.26269580938639));
#88086=CARTESIAN_POINT('Ctrl Pts',(-9.23287249434296,17.2217794432786,2.25362075931515));
#88087=CARTESIAN_POINT('Ctrl Pts',(-9.24196890831453,17.2223452532561,2.24806761622092));
#88088=CARTESIAN_POINT('Ctrl Pts',(-9.31856015257893,17.2270491664284,2.20245135112076));
#88089=CARTESIAN_POINT('Ctrl Pts',(-9.38911985454486,17.2309852611936,2.16777620024398));
#88090=CARTESIAN_POINT('Ctrl Pts',(-9.47696599294441,17.2356204052849,2.13306099793535));
#88091=CARTESIAN_POINT('Ctrl Pts',(-9.49189925243254,17.2363999368057,2.1274401848359));
#88092=CARTESIAN_POINT('Ctrl Pts',(-9.58492216299372,17.2412159237708,2.09415299738017));
#88093=CARTESIAN_POINT('Ctrl Pts',(-9.66514665899465,17.2451885944046,2.07291664305876));
#88094=CARTESIAN_POINT('Ctrl Pts',(-9.78009805732002,17.2511028118691,2.05271870301203));
#88095=CARTESIAN_POINT('Ctrl Pts',(-9.81365669131164,17.2528564663376,2.04801658213785));
#88096=CARTESIAN_POINT('Ctrl Pts',(-9.85342394220545,17.2549972999964,2.04384579719927));
#88097=CARTESIAN_POINT('Ctrl Pts',(-9.85950614430575,17.2553264555888,2.04324639113841));
#88098=CARTESIAN_POINT('Ctrl Pts',(-9.86888598383427,17.255836971341,2.0423812883255));
#88099=CARTESIAN_POINT('Ctrl Pts',(-9.87218114048978,17.2560168673899,2.0420886403593));
#88100=CARTESIAN_POINT('Ctrl Pts',(-9.87825172965127,17.2563493454796,2.04157024075065));
#88101=CARTESIAN_POINT('Ctrl Pts',(-9.88102683081592,17.2565017453747,2.04134123638593));
#88102=CARTESIAN_POINT('Ctrl Pts',(-9.88727135032299,17.2568455975948,2.04084387050219));
#88103=CARTESIAN_POINT('Ctrl Pts',(-9.89074105948706,17.2570372918597,2.04057996378357));
#88104=CARTESIAN_POINT('Ctrl Pts',(-9.90091087071076,17.2576009496986,2.03984291602412));
#88105=CARTESIAN_POINT('Ctrl Pts',(-9.90761323485814,17.2579747096085,2.03940353022375));
#88106=CARTESIAN_POINT('Ctrl Pts',(-9.95554117129185,17.2606625959298,2.03659273057803));
#88107=CARTESIAN_POINT('Ctrl Pts',(-9.99684455670688,17.2630587374229,2.03592115081653));
#88108=CARTESIAN_POINT('Ctrl Pts',(-10.120386982239,17.2703597784982,2.03913993008715));
#88109=CARTESIAN_POINT('Ctrl Pts',(-10.202328520742,17.2753715873642,2.0482188816));
#88110=CARTESIAN_POINT('Ctrl Pts',(-10.3405837684763,17.2837873104213,2.0754751554899));
#88111=CARTESIAN_POINT('Ctrl Pts',(-10.397365972315,17.2872338856815,2.09025898361895));
#88112=CARTESIAN_POINT('Ctrl Pts',(-10.4842638695639,17.2924524093954,2.11855364923184));
#88113=CARTESIAN_POINT('Ctrl Pts',(-10.5150670675056,17.2942915208246,2.12974028992148));
#88114=CARTESIAN_POINT('Ctrl Pts',(-10.5538550286932,17.296594648696,2.14531978090492));
#88115=CARTESIAN_POINT('Ctrl Pts',(-10.5622081647165,17.2970898911657,2.14876505614868));
#88116=CARTESIAN_POINT('Ctrl Pts',(-10.5756123665536,17.2978835121415,2.15443947551393));
#88117=CARTESIAN_POINT('Ctrl Pts',(-10.5806835719353,17.2981835092858,2.15662019070045));
#88118=CARTESIAN_POINT('Ctrl Pts',(-10.5903320360833,17.2987538380874,2.16083405799658));
#88119=CARTESIAN_POINT('Ctrl Pts',(-10.5949114244475,17.2990243370432,2.16286211220678));
#88120=CARTESIAN_POINT('Ctrl Pts',(-10.6053653725786,17.2996414375386,2.16755614305354));
#88121=CARTESIAN_POINT('Ctrl Pts',(-10.6112329197835,17.2999875089762,2.17023754534025));
#88122=CARTESIAN_POINT('Ctrl Pts',(-10.6265229437274,17.3008886688687,2.17734749789746));
#88123=CARTESIAN_POINT('Ctrl Pts',(-10.635916321421,17.3014416370989,2.18183799177558));
#88124=CARTESIAN_POINT('Ctrl Pts',(-10.706154980103,17.3055730585518,2.2163410809698));
#88125=CARTESIAN_POINT('Ctrl Pts',(-10.7648984811528,17.3090036579923,2.25045333873286));
#88126=CARTESIAN_POINT('Ctrl Pts',(-10.8429548295491,17.313662117074,2.30335533918458));
#88127=CARTESIAN_POINT('Ctrl Pts',(-10.8644355218974,17.3149562520115,2.31877920765174));
#88128=CARTESIAN_POINT('Ctrl Pts',(-10.9366821680572,17.3193802119256,2.37368152666745));
#88129=CARTESIAN_POINT('Ctrl Pts',(-10.9852561675272,17.3224774912393,2.41591670478913));
#88130=CARTESIAN_POINT('Ctrl Pts',(-11.0645338892668,17.3280195049125,2.49459162579542));
#88131=CARTESIAN_POINT('Ctrl Pts',(-11.0965295312416,17.3304194677486,2.52958740422337));
#88132=CARTESIAN_POINT('Ctrl Pts',(-11.1330129578751,17.3334481403963,2.57360394959969));
#88133=CARTESIAN_POINT('Ctrl Pts',(-11.1391816357424,17.3339711740101,2.58120013310973));
#88134=CARTESIAN_POINT('Ctrl Pts',(-11.1477645250759,17.3347154103938,2.59198851656597));
#88135=CARTESIAN_POINT('Ctrl Pts',(-11.1502426612193,17.3349322771497,2.5951298001296));
#88136=CARTESIAN_POINT('Ctrl Pts',(-11.154465064848,17.335305278341,2.60052748914215));
#88137=CARTESIAN_POINT('Ctrl Pts',(-11.1562156958889,17.3354609678447,2.60277893011944));
#88138=CARTESIAN_POINT('Ctrl Pts',(-11.1595844787085,17.3357626114881,2.60713766696617));
#88139=CARTESIAN_POINT('Ctrl Pts',(-11.1612034821628,17.335908498797,2.60924426367743));
#88140=CARTESIAN_POINT('Ctrl Pts',(-11.1650865367989,17.3362605970419,2.61432535016366));
#88141=CARTESIAN_POINT('Ctrl Pts',(-11.1673449333696,17.3364671933104,2.61730411267632));
#88142=CARTESIAN_POINT('Ctrl Pts',(-11.175585578828,17.3372276275163,2.628260232211));
#88143=CARTESIAN_POINT('Ctrl Pts',(-11.1814975275428,17.3377860168106,2.63628983034558));
#88144=CARTESIAN_POINT('Ctrl Pts',(-11.2515593078446,17.3445536178853,2.73351304884013));
#88145=CARTESIAN_POINT('Ctrl Pts',(-11.3055466259008,17.3512792384178,2.82959076645209));
#88146=CARTESIAN_POINT('Ctrl Pts',(-11.3734912880735,17.3617503272508,2.99053156222294));
#88147=CARTESIAN_POINT('Ctrl Pts',(-11.3947138580813,17.3655826748097,3.051880485676));
#88148=CARTESIAN_POINT('Ctrl Pts',(-11.4210080933477,17.3712966023831,3.14816167448934));
#88149=CARTESIAN_POINT('Ctrl Pts',(-11.4290067638186,17.3732622520977,3.18220420014149));
#88150=CARTESIAN_POINT('Ctrl Pts',(-11.4375673537468,17.3756982717713,3.22555951952907));
#88151=CARTESIAN_POINT('Ctrl Pts',(-11.439269932196,17.3762044368888,3.23463319415922));
#88152=CARTESIAN_POINT('Ctrl Pts',(-11.441860804296,17.3770112965359,3.24920003326018));
#88153=CARTESIAN_POINT('Ctrl Pts',(-11.4428038072576,17.3773137079633,3.2546831085364));
#88154=CARTESIAN_POINT('Ctrl Pts',(-11.4445346874309,17.3778859616642,3.26510263078824));
#88155=CARTESIAN_POINT('Ctrl Pts',(-11.4453285821394,17.3781559895576,3.27003798626276));
#88156=CARTESIAN_POINT('Ctrl Pts',(-11.4470767804593,17.3787683762951,3.28127269851218));
#88157=CARTESIAN_POINT('Ctrl Pts',(-11.4480152703731,17.3791102345977,3.28757443779273));
#88158=CARTESIAN_POINT('Ctrl Pts',(-11.4503414674635,17.3799931653142,3.30392652295263));
#88159=CARTESIAN_POINT('Ctrl Pts',(-11.4516658838143,17.3805322576375,3.31398562068876));
#88160=CARTESIAN_POINT('Ctrl Pts',(-11.4599550046097,17.3841744734214,3.38243507604782));
#88161=CARTESIAN_POINT('Ctrl Pts',(-11.4634999999993,17.387168492118,3.4411881824418));
#88162=CARTESIAN_POINT('Ctrl Pts',(-11.4635,17.3900944100234,3.49999999998336));
#88163=CARTESIAN_POINT('Origin',(-10.,13.2,3.5));
#88164=CARTESIAN_POINT('',(-11.4635,17.9619558011997,3.500000000001));
#88165=CARTESIAN_POINT('',(-11.4635,17.8879846534521,3.50000000000001));
#88166=CARTESIAN_POINT('',(-11.4635,13.2,3.5));
#88167=CARTESIAN_POINT('Ctrl Pts',(-11.4635,17.9619558011997,3.500000000001));
#88168=CARTESIAN_POINT('Ctrl Pts',(-11.4635000000001,17.9578239784063,3.4269116130009));
#88169=CARTESIAN_POINT('Ctrl Pts',(-11.4580248356914,17.9534532242815,3.35392967682306));
#88170=CARTESIAN_POINT('Ctrl Pts',(-11.4386952867223,17.9456567463325,3.22581223811122));
#88171=CARTESIAN_POINT('Ctrl Pts',(-11.427041201044,17.9422473245681,3.17048996468713));
#88172=CARTESIAN_POINT('Ctrl Pts',(-11.3989284884513,17.9358886003781,3.06710694649229));
#88173=CARTESIAN_POINT('Ctrl Pts',(-11.3831101110572,17.9329320672596,3.01895479262035));
#88174=CARTESIAN_POINT('Ctrl Pts',(-11.3541030665059,17.9283604139683,2.94401487060868));
#88175=CARTESIAN_POINT('Ctrl Pts',(-11.3425393561018,17.9266968833111,2.91664518778092));
#88176=CARTESIAN_POINT('Ctrl Pts',(-11.3265067049631,17.9245801650968,2.88170514673387));
#88177=CARTESIAN_POINT('Ctrl Pts',(-11.3227923620327,17.9241015917339,2.87379800744325));
#88178=CARTESIAN_POINT('Ctrl Pts',(-11.31664492699,17.923328244677,2.8610100793101));
#88179=CARTESIAN_POINT('Ctrl Pts',(-11.3142550004792,17.9230319975196,2.85610887772145));
#88180=CARTESIAN_POINT('Ctrl Pts',(-11.3096102118658,17.9224645756437,2.84671706660158));
#88181=CARTESIAN_POINT('Ctrl Pts',(-11.3073595088221,17.92219326236,2.84222449600517));
#88182=CARTESIAN_POINT('Ctrl Pts',(-11.3021563952054,17.9215742502647,2.83197090117125));
#88183=CARTESIAN_POINT('Ctrl Pts',(-11.2991887975369,17.921227085385,2.82621767265183));
#88184=CARTESIAN_POINT('Ctrl Pts',(-11.2912031422431,17.920308212583,2.81098495506568));
#88185=CARTESIAN_POINT('Ctrl Pts',(-11.2861188326014,17.9197388254639,2.80154052140793));
#88186=CARTESIAN_POINT('Ctrl Pts',(-11.2389266539427,17.9145910892826,2.71614085320336));
#88187=CARTESIAN_POINT('Ctrl Pts',(-11.1902382435879,17.9102642492208,2.64401527820695));
#88188=CARTESIAN_POINT('Ctrl Pts',(-11.0654196758604,17.9005952699772,2.49053097405107));
#88189=CARTESIAN_POINT('Ctrl Pts',(-10.9858480790831,17.8953398435327,2.41268933228949));
#88190=CARTESIAN_POINT('Ctrl Pts',(-10.8899467279994,17.8889918056793,2.33813170259552));
#88191=CARTESIAN_POINT('Ctrl Pts',(-10.8815646440005,17.8884366667639,2.33175906337484));
#88192=CARTESIAN_POINT('Ctrl Pts',(-10.8687195194081,17.8875842818664,2.32221027341934));
#88193=CARTESIAN_POINT('Ctrl Pts',(-10.8643060493826,17.8872911164504,2.31896769958697));
#88194=CARTESIAN_POINT('Ctrl Pts',(-10.8570466201691,17.8868082445939,2.31369668539351));
#88195=CARTESIAN_POINT('Ctrl Pts',(-10.8542113726267,17.8866194896457,2.31165350433316));
#88196=CARTESIAN_POINT('Ctrl Pts',(-10.8487351897889,17.8862545441104,2.30773689485491));
#88197=CARTESIAN_POINT('Ctrl Pts',(-10.8460952984626,17.8860784503454,2.30586203486353));
#88198=CARTESIAN_POINT('Ctrl Pts',(-10.8434384098184,17.8859010338455,2.30398833658764));
#88199=CARTESIAN_POINT('Ctrl Pts',(-10.8434275861427,17.8859003110802,2.30398070370547));
#88200=CARTESIAN_POINT('Ctrl Pts',(-10.8434058271742,17.8858988580898,2.3039653596707));
#88201=CARTESIAN_POINT('Ctrl Pts',(-10.8433948918587,17.8858981278632,2.30395764850664));
#88202=CARTESIAN_POINT('Ctrl Pts',(-10.843372907423,17.885896659804,2.30394214637937));
#88203=CARTESIAN_POINT('Ctrl Pts',(-10.8433618582589,17.8858959219684,2.30393435538978));
#88204=CARTESIAN_POINT('Ctrl Pts',(-10.8433396437819,17.8858944385345,2.30391869197265));
#88205=CARTESIAN_POINT('Ctrl Pts',(-10.8433284786114,17.8858936929456,2.30391081965029));
#88206=CARTESIAN_POINT('Ctrl Pts',(-10.8433060299012,17.8858921938567,2.30389499201663));
#88207=CARTESIAN_POINT('Ctrl Pts',(-10.8432947463136,17.8858914403534,2.30388703667655));
#88208=CARTESIAN_POINT('Ctrl Pts',(-10.8432720585338,17.885889925286,2.30387104144625));
#88209=CARTESIAN_POINT('Ctrl Pts',(-10.8432606542248,17.8858891637141,2.30386300147888));
#88210=CARTESIAN_POINT('Ctrl Pts',(-10.8432377224495,17.8858876323389,2.30384683521));
#88211=CARTESIAN_POINT('Ctrl Pts',(-10.8432261951198,17.8858868625446,2.30383870901004));
#88212=CARTESIAN_POINT('Ctrl Pts',(-10.8432030147971,17.8858853145572,2.30382236852533));
#88213=CARTESIAN_POINT('Ctrl Pts',(-10.8431913618671,17.8858845363681,2.30381415429038));
#88214=CARTESIAN_POINT('Ctrl Pts',(-10.8431679279395,17.8858829714301,2.30379763605739));
#88215=CARTESIAN_POINT('Ctrl Pts',(-10.843156146843,17.8858821846745,2.30378933199517));
#88216=CARTESIAN_POINT('Ctrl Pts',(-10.8431324539833,17.8858806024298,2.30377263229248));
#88217=CARTESIAN_POINT('Ctrl Pts',(-10.8431205421937,17.8858798069388,2.30376423663924));
#88218=CARTESIAN_POINT('Ctrl Pts',(-10.8430965851956,17.8858782070392,2.30374735183211));
#88219=CARTESIAN_POINT('Ctrl Pts',(-10.8430845400392,17.885877402634,2.30373886272102));
#88220=CARTESIAN_POINT('Ctrl Pts',(-10.8430603135512,17.8858757847215,2.30372178907369));
#88221=CARTESIAN_POINT('Ctrl Pts',(-10.8430481322439,17.8858749712158,2.30371320456085));
#88222=CARTESIAN_POINT('Ctrl Pts',(-10.8430236306788,17.8858733349168,2.30369593817276));
#88223=CARTESIAN_POINT('Ctrl Pts',(-10.8430113103858,17.8858725121211,2.3036872562792));
#88224=CARTESIAN_POINT('Ctrl Pts',(-10.8429865280067,17.8858708570519,2.3036697931459));
#88225=CARTESIAN_POINT('Ctrl Pts',(-10.8429740658253,17.885870024772,2.30366101184557));
#88226=CARTESIAN_POINT('Ctrl Pts',(-10.8429489966553,17.8858683505329,2.30364334779481));
#88227=CARTESIAN_POINT('Ctrl Pts',(-10.8429363896473,17.8858675085723,2.30363446503748));
#88228=CARTESIAN_POINT('Ctrl Pts',(-10.8429110276435,17.8858658147591,2.30361659585214));
#88229=CARTESIAN_POINT('Ctrl Pts',(-10.8428982727602,17.8858649629139,2.30360760951048));
#88230=CARTESIAN_POINT('Ctrl Pts',(-10.8428726119136,17.8858632491246,2.30358953099901));
#88231=CARTESIAN_POINT('Ctrl Pts',(-10.8428597059039,17.8858623871774,2.30358043880382));
#88232=CARTESIAN_POINT('Ctrl Pts',(-10.8428337396388,17.8858606529723,2.30356214637712));
#88233=CARTESIAN_POINT('Ctrl Pts',(-10.8428206792984,17.8858597807086,2.30355294609324));
#88234=CARTESIAN_POINT('Ctrl Pts',(-10.8427944009659,17.885858025643,2.30353443511238));
#88235=CARTESIAN_POINT('Ctrl Pts',(-10.8427811830113,17.8858571428433,2.30352512444957));
#88236=CARTESIAN_POINT('Ctrl Pts',(-10.8427545859658,17.8858553664726,2.30350639027972));
#88237=CARTESIAN_POINT('Ctrl Pts',(-10.8427412069267,17.8858544729048,2.30349696681726));
#88238=CARTESIAN_POINT('Ctrl Pts',(-10.842714284224,17.8858526747645,2.30347800461539));
#88239=CARTESIAN_POINT('Ctrl Pts',(-10.8427007405361,17.8858517701902,2.30346846586716));
#88240=CARTESIAN_POINT('Ctrl Pts',(-10.8404691647733,17.8857027238442,2.30189683546785));
#88241=CARTESIAN_POINT('Ctrl Pts',(-10.8382468456193,17.8855541588349,2.30034095043559));
#88242=CARTESIAN_POINT('Ctrl Pts',(-10.8330583046954,17.8852069902392,2.29672981692358));
#88243=CARTESIAN_POINT('Ctrl Pts',(-10.8300888051139,17.8850080690524,2.29467935902838));
#88244=CARTESIAN_POINT('Ctrl Pts',(-10.8222730246246,17.8844839683172,2.28932509537366));
#88245=CARTESIAN_POINT('Ctrl Pts',(-10.8174144624592,17.8841576307521,2.28603943806788));
#88246=CARTESIAN_POINT('Ctrl Pts',(-10.7836405927923,17.8818861545121,2.26349415627565));
#88247=CARTESIAN_POINT('Ctrl Pts',(-10.7540692663234,17.8798825235075,2.24524167790199));
#88248=CARTESIAN_POINT('Ctrl Pts',(-10.6032233788279,17.8696946768747,2.15939314137159));
#88249=CARTESIAN_POINT('Ctrl Pts',(-10.4734052830455,17.8611155959333,2.10823768925242));
#88250=CARTESIAN_POINT('Ctrl Pts',(-10.2986176619481,17.8507636209629,2.06670879154108));
#88251=CARTESIAN_POINT('Ctrl Pts',(-10.258551709108,17.8484600692726,2.05894216926438));
#88252=CARTESIAN_POINT('Ctrl Pts',(-10.2086289047256,17.8456742942333,2.05141443943374));
#88253=CARTESIAN_POINT('Ctrl Pts',(-10.1990329485125,17.845142607357,2.05006481595887));
#88254=CARTESIAN_POINT('Ctrl Pts',(-10.1838084353106,17.8443049085491,2.04807755632345));
#88255=CARTESIAN_POINT('Ctrl Pts',(-10.1781884790737,17.8439969407621,2.04737713410297));
#88256=CARTESIAN_POINT('Ctrl Pts',(-10.1676185234017,17.8434200424035,2.04612205167216));
#88257=CARTESIAN_POINT('Ctrl Pts',(-10.1626694965585,17.8431508848909,2.04556000682067));
#88258=CARTESIAN_POINT('Ctrl Pts',(-10.1515485599541,17.8425481694316,2.04435451126075));
#88259=CARTESIAN_POINT('Ctrl Pts',(-10.145375211774,17.8422150513704,2.04372502447737));
#88260=CARTESIAN_POINT('Ctrl Pts',(-10.1296368357753,17.8413694091386,2.04222128193478));
#88261=CARTESIAN_POINT('Ctrl Pts',(-10.1200667829685,17.8408585933469,2.04140188073448));
#88262=CARTESIAN_POINT('Ctrl Pts',(-10.062435512613,17.8378018763012,2.03703846571261));
#88263=CARTESIAN_POINT('Ctrl Pts',(-10.0142289255224,17.8353276865979,2.03577570216286));
#88264=CARTESIAN_POINT('Ctrl Pts',(-9.83019161944957,17.8260784313615,2.04004682925809));
#88265=CARTESIAN_POINT('Ctrl Pts',(-9.69545837745759,17.8197750539726,2.06210368799201));
#88266=CARTESIAN_POINT('Ctrl Pts',(-9.5374567626927,17.811338270566,2.11120139820152));
#88267=CARTESIAN_POINT('Ctrl Pts',(-9.50947450521493,17.8097989529983,2.12083637474761));
#88268=CARTESIAN_POINT('Ctrl Pts',(-9.47629497950738,17.8078980422194,2.13339836837976));
#88269=CARTESIAN_POINT('Ctrl Pts',(-9.4707972449517,17.8075805344892,2.13551789688634));
#88270=CARTESIAN_POINT('Ctrl Pts',(-9.46227778772306,17.8070843533241,2.13886161581068));
#88271=CARTESIAN_POINT('Ctrl Pts',(-9.45924704052482,17.8069070175854,2.14006282686155));
#88272=CARTESIAN_POINT('Ctrl Pts',(-9.45363255578693,17.8065769304739,2.14230981617012));
#88273=CARTESIAN_POINT('Ctrl Pts',(-9.45104777842761,17.8064243422645,2.14335285449391));
#88274=CARTESIAN_POINT('Ctrl Pts',(-9.44518846632145,17.8060770357351,2.14573675658051));
#88275=CARTESIAN_POINT('Ctrl Pts',(-9.44191581964567,17.8058820525349,2.14708210985472));
#88276=CARTESIAN_POINT('Ctrl Pts',(-9.43344675395032,17.805374936047,2.15059961814272));
#88277=CARTESIAN_POINT('Ctrl Pts',(-9.42825798729957,17.8050617602296,2.15278990502998));
#88278=CARTESIAN_POINT('Ctrl Pts',(-9.39526196264111,17.8030549984217,2.16694316912226));
#88279=CARTESIAN_POINT('Ctrl Pts',(-9.36782067236811,17.8013169475566,2.17973576615908));
#88280=CARTESIAN_POINT('Ctrl Pts',(-9.24949964985647,17.7935776189337,2.23942934116641));
#88281=CARTESIAN_POINT('Ctrl Pts',(-9.16328154215047,17.7873119295541,2.29493079105269));
#88282=CARTESIAN_POINT('Ctrl Pts',(-9.02758784870345,17.7769605572523,2.40391635103249));
#88283=CARTESIAN_POINT('Ctrl Pts',(-8.97500043135013,17.7727900003606,2.45292648651613));
#88284=CARTESIAN_POINT('Ctrl Pts',(-8.9152158207681,17.7678775462634,2.51748400504331));
#88285=CARTESIAN_POINT('Ctrl Pts',(-8.90441227605018,17.7669818123857,2.52954548556323));
#88286=CARTESIAN_POINT('Ctrl Pts',(-8.88926512874283,17.7657138636953,2.54703174425177));
#88287=CARTESIAN_POINT('Ctrl Pts',(-8.88475681066598,17.7653348908372,2.55231171703899));
#88288=CARTESIAN_POINT('Ctrl Pts',(-8.87701362477559,17.7646811575558,2.56151202445327));
#88289=CARTESIAN_POINT('Ctrl Pts',(-8.87376131796731,17.7644056907506,2.56541746689523));
#88290=CARTESIAN_POINT('Ctrl Pts',(-8.86755013074508,17.763877866892,2.57295550650969));
#88291=CARTESIAN_POINT('Ctrl Pts',(-8.86458822511482,17.7636253898667,2.57658552023413));
#88292=CARTESIAN_POINT('Ctrl Pts',(-8.8576452398546,17.7630316850439,2.5851785251133));
#88293=CARTESIAN_POINT('Ctrl Pts',(-8.85367897367856,17.7626910489818,2.59015340013253));
#88294=CARTESIAN_POINT('Ctrl Pts',(-8.83996499907785,17.7615079166721,2.60758682558888));
#88295=CARTESIAN_POINT('Ctrl Pts',(-8.83038674689719,17.7606720659456,2.62017766508086));
#88296=CARTESIAN_POINT('Ctrl Pts',(-8.74674393411434,17.7532791232034,2.73390866112099));
#88297=CARTESIAN_POINT('Ctrl Pts',(-8.68575762727706,17.7472738200766,2.84401529859718));
#88298=CARTESIAN_POINT('Ctrl Pts',(-8.61935589402173,17.7384836200859,3.01147680254895));
#88299=CARTESIAN_POINT('Ctrl Pts',(-8.60204043507687,17.7357868222409,3.06348961712328));
#88300=CARTESIAN_POINT('Ctrl Pts',(-8.58102961438722,17.7316724426748,3.14083533779503));
#88301=CARTESIAN_POINT('Ctrl Pts',(-8.57501570909544,17.7303456128719,3.16549166542026));
#88302=CARTESIAN_POINT('Ctrl Pts',(-8.56845372326699,17.7286827195154,3.19579734255523));
#88303=CARTESIAN_POINT('Ctrl Pts',(-8.56729313849824,17.7283788876822,3.20131112148117));
#88304=CARTESIAN_POINT('Ctrl Pts',(-8.56552263529681,17.7278995208726,3.20997033744673));
#88305=CARTESIAN_POINT('Ctrl Pts',(-8.56489114420386,17.7277251813479,3.21311136896306));
#88306=CARTESIAN_POINT('Ctrl Pts',(-8.5637281287112,17.7273976609008,3.21899613462274));
#88307=CARTESIAN_POINT('Ctrl Pts',(-8.56319414661685,17.7272446198982,3.22173933108814));
#88308=CARTESIAN_POINT('Ctrl Pts',(-8.56198641520402,17.7268922843095,3.22803991315835));
#88309=CARTESIAN_POINT('Ctrl Pts',(-8.56131800893608,17.7266926933202,3.23159827329077));
#88310=CARTESIAN_POINT('Ctrl Pts',(-8.55959418159968,17.7261656863293,3.24096679676589));
#88311=CARTESIAN_POINT('Ctrl Pts',(-8.55856072181247,17.7258370919892,3.2467808716604));
#88312=CARTESIAN_POINT('Ctrl Pts',(-8.55154323838913,17.7235146954363,3.28769566456115));
#88313=CARTESIAN_POINT('Ctrl Pts',(-8.54680723604831,17.7214594734258,3.32299572999621));
#88314=CARTESIAN_POINT('Ctrl Pts',(-8.54319327805999,17.7192645070637,3.36018041392662));
#88315=CARTESIAN_POINT('Ctrl Pts',(-8.54302634261115,17.7191611137012,3.36193080220547));
#88316=CARTESIAN_POINT('Ctrl Pts',(-8.53018468905039,17.7110476105424,3.49919795017696));
#88317=CARTESIAN_POINT('Ctrl Pts',(-8.53647081074344,17.7026501029379,3.635827922689));
#88318=CARTESIAN_POINT('Ctrl Pts',(-8.56907111877884,17.6924542680991,3.80974090697808));
#88319=CARTESIAN_POINT('Ctrl Pts',(-8.57826232761715,17.690150220451,3.84951301165193));
#88320=CARTESIAN_POINT('Ctrl Pts',(-8.5916791977902,17.6873639368033,3.89819426936433));
#88321=CARTESIAN_POINT('Ctrl Pts',(-8.59434676426212,17.686832215656,3.90751091433013));
#88322=CARTESIAN_POINT('Ctrl Pts',(-8.59871965684432,17.6859944753849,3.92222946931813));
#88323=CARTESIAN_POINT('Ctrl Pts',(-8.60036411147688,17.685686500077,3.92764904500284));
#88324=CARTESIAN_POINT('Ctrl Pts',(-8.60351383613661,17.6851095950187,3.93781668766136));
#88325=CARTESIAN_POINT('Ctrl Pts',(-8.60501196209861,17.6848404382733,3.94256686818767));
#88326=CARTESIAN_POINT('Ctrl Pts',(-8.60843085066892,17.6842377340939,3.95321744790083));
#88327=CARTESIAN_POINT('Ctrl Pts',(-8.61036495403166,17.6839046264723,3.9591134860673));
#88328=CARTESIAN_POINT('Ctrl Pts',(-8.6153880054529,17.683059028771,3.97410348257388));
#88329=CARTESIAN_POINT('Ctrl Pts',(-8.6185291049438,17.6825482467557,3.98317973840741));
#88330=CARTESIAN_POINT('Ctrl Pts',(-8.6379644586361,17.6794920708317,4.03759919658659));
#88331=CARTESIAN_POINT('Ctrl Pts',(-8.6564012139647,17.6770183582863,4.08214828575086));
#88332=CARTESIAN_POINT('Ctrl Pts',(-8.73510654454,17.6677689893309,4.24856225075011));
#88333=CARTESIAN_POINT('Ctrl Pts',(-8.81002895951557,17.6614651798074,4.36270683062671));
#88334=CARTESIAN_POINT('Ctrl Pts',(-8.91911828506474,17.6530278511486,4.48711831444707));
#88335=CARTESIAN_POINT('Ctrl Pts',(-8.9392959813472,17.6514884948445,4.50876885197372));
#88336=CARTESIAN_POINT('Ctrl Pts',(-8.96426060298913,17.6495875407139,4.53397817676267));
#88337=CARTESIAN_POINT('Ctrl Pts',(-8.96843185532628,17.6492700307065,4.5381397444796));
#88338=CARTESIAN_POINT('Ctrl Pts',(-8.97494986446247,17.6487738467438,4.54456454955388));
#88339=CARTESIAN_POINT('Ctrl Pts',(-8.97727929380474,17.6485965105091,4.54684537313068));
#88340=CARTESIAN_POINT('Ctrl Pts',(-8.98161443411119,17.6482664229571,4.55106177675149));
#88341=CARTESIAN_POINT('Ctrl Pts',(-8.98361806431465,17.6481138348071,4.55299942060114));
#88342=CARTESIAN_POINT('Ctrl Pts',(-8.98817779696077,17.6477665290395,4.55738384692001));
#88343=CARTESIAN_POINT('Ctrl Pts',(-8.99073723378629,17.6475715465466,4.55982707951923));
#88344=CARTESIAN_POINT('Ctrl Pts',(-8.9985530973578,17.6469760853124,4.56723409831569));
#88345=CARTESIAN_POINT('Ctrl Pts',(-9.00383738690238,17.6465734479188,4.57216815999237));
#88346=CARTESIAN_POINT('Ctrl Pts',(-9.05416188240701,17.6427404158983,4.61846409589018));
#88347=CARTESIAN_POINT('Ctrl Pts',(-9.10171217327623,17.6391317510532,4.65700005529325));
#88348=CARTESIAN_POINT('Ctrl Pts',(-9.22323811343783,17.6302030209578,4.74347065517678));
#88349=CARTESIAN_POINT('Ctrl Pts',(-9.29941152893627,17.624854729779,4.78792696285389));
#88350=CARTESIAN_POINT('Ctrl Pts',(-9.43014256999832,17.6163708146461,4.84917364584562));
#88351=CARTESIAN_POINT('Ctrl Pts',(-9.48250758203226,17.6131349431901,4.87011305201036));
#88352=CARTESIAN_POINT('Ctrl Pts',(-9.54948642130707,17.6092044557011,4.89250613356463));
#88353=CARTESIAN_POINT('Ctrl Pts',(-9.5630836262307,17.6084168115938,4.89683210129315));
#88354=CARTESIAN_POINT('Ctrl Pts',(-9.58305907327476,17.6072743308619,4.90286708486127));
#88355=CARTESIAN_POINT('Ctrl Pts',(-9.5893887856905,17.6069144364822,4.90473279553286));
#88356=CARTESIAN_POINT('Ctrl Pts',(-9.60056225899826,17.6062828228035,4.9079442498121));
#88357=CARTESIAN_POINT('Ctrl Pts',(-9.60540070734563,17.6060105270658,4.90930795734217));
#88358=CARTESIAN_POINT('Ctrl Pts',(-9.61485246839317,17.6054809339384,4.91191942654198));
#88359=CARTESIAN_POINT('Ctrl Pts',(-9.61946505154907,17.6052235626942,4.91316957294662));
#88360=CARTESIAN_POINT('Ctrl Pts',(-9.63189308756626,17.6045329590859,4.91647267721811));
#88361=CARTESIAN_POINT('Ctrl Pts',(-9.639719620246,17.6041010790802,4.9184835549955));
#88362=CARTESIAN_POINT('Ctrl Pts',(-9.66884158486058,17.6025049679884,4.92570930729709));
#88363=CARTESIAN_POINT('Ctrl Pts',(-9.69023728368727,17.6013539024372,4.93051041619764));
#88364=CARTESIAN_POINT('Ctrl Pts',(-9.83321543457981,17.5937893420194,4.95923565003717));
#88365=CARTESIAN_POINT('Ctrl Pts',(-9.957299462264,17.5878883868208,4.96811566504678));
#88366=CARTESIAN_POINT('Ctrl Pts',(-10.1304558421928,17.5794000935249,4.95851451678677));
#88367=CARTESIAN_POINT('Ctrl Pts',(-10.1797142162176,17.5769486768567,4.95326717481122));
#88368=CARTESIAN_POINT('Ctrl Pts',(-10.2521736082169,17.5731731433739,4.94180786873347));
#88369=CARTESIAN_POINT('Ctrl Pts',(-10.2756428542167,17.5719233564681,4.9375055985162));
#88370=CARTESIAN_POINT('Ctrl Pts',(-10.3044074310637,17.5703469432101,4.93150233513576));
#88371=CARTESIAN_POINT('Ctrl Pts',(-10.309813259346,17.5700487251547,4.93034211360473));
#88372=CARTESIAN_POINT('Ctrl Pts',(-10.3183182907482,17.569576267359,4.92846625171156));
#88373=CARTESIAN_POINT('Ctrl Pts',(-10.3214220135591,17.5694031666901,4.92777107944794));
#88374=CARTESIAN_POINT('Ctrl Pts',(-10.3272526413961,17.5690766460578,4.92644515932871));
#88375=CARTESIAN_POINT('Ctrl Pts',(-10.3299800164562,17.5689233561522,4.92581670356375));
#88376=CARTESIAN_POINT('Ctrl Pts',(-10.3362090010159,17.5685720058649,4.9243625594138));
#88377=CARTESIAN_POINT('Ctrl Pts',(-10.3397093774856,17.5683736595702,4.92353178092481));
#88378=CARTESIAN_POINT('Ctrl Pts',(-10.3489986291461,17.5678449511419,4.92129085924924));
#88379=CARTESIAN_POINT('Ctrl Pts',(-10.3547819553959,17.5675133682873,4.91985827158666));
#88380=CARTESIAN_POINT('Ctrl Pts',(-10.3962846576127,17.5651172426492,4.90930824305567));
#88381=CARTESIAN_POINT('Ctrl Pts',(-10.4316543743009,17.5629868948466,4.89888002205068));
#88382=CARTESIAN_POINT('Ctrl Pts',(-10.4740090227203,17.5603580698054,4.88463315418522));
#88383=CARTESIAN_POINT('Ctrl Pts',(-10.4814081602794,17.5598958869296,4.88207803891197));
#88384=CARTESIAN_POINT('Ctrl Pts',(-10.5738298382263,17.5540886316416,4.84933020041805));
#88385=CARTESIAN_POINT('Ctrl Pts',(-10.6559048637199,17.5485832701968,4.81139706520054));
#88386=CARTESIAN_POINT('Ctrl Pts',(-10.799984597677,17.5386954894317,4.72787618470692));
#88387=CARTESIAN_POINT('Ctrl Pts',(-10.8629157447394,17.5342835172413,4.68449759238966));
#88388=CARTESIAN_POINT('Ctrl Pts',(-10.930957353166,17.5294327267869,4.6292822165174));
#88389=CARTESIAN_POINT('Ctrl Pts',(-10.9396484202009,17.5288112897752,4.62206094951987));
#88390=CARTESIAN_POINT('Ctrl Pts',(-10.952833039658,17.5278655176554,4.61084543035098));
#88391=CARTESIAN_POINT('Ctrl Pts',(-10.9573869321956,17.5275382868186,4.60692304843774));
#88392=CARTESIAN_POINT('Ctrl Pts',(-10.9656262254777,17.5269451510172,4.59973745541037));
#88393=CARTESIAN_POINT('Ctrl Pts',(-10.9693195553986,17.5266788720254,4.59648350580626));
#88394=CARTESIAN_POINT('Ctrl Pts',(-10.9773256792928,17.5261007403383,4.58935777227946));
#88395=CARTESIAN_POINT('Ctrl Pts',(-10.981632043298,17.5257891895024,4.58547886774723));
#88396=CARTESIAN_POINT('Ctrl Pts',(-10.9933223423192,17.5249417548551,4.57482250964639));
#88397=CARTESIAN_POINT('Ctrl Pts',(-11.0006599533003,17.5244079982775,4.5679945540802));
#88398=CARTESIAN_POINT('Ctrl Pts',(-11.0375756975071,17.521712250289,4.53292842725173));
#88399=CARTESIAN_POINT('Ctrl Pts',(-11.0660324666245,17.5196005097642,4.50353357470093));
#88400=CARTESIAN_POINT('Ctrl Pts',(-11.1022345768859,17.5168433420942,4.462857692943));
#88401=CARTESIAN_POINT('Ctrl Pts',(-11.1111056863723,17.5161615391143,4.45260703573738));
#88402=CARTESIAN_POINT('Ctrl Pts',(-11.1845009977094,17.5104605487613,4.36537767396796));
#88403=CARTESIAN_POINT('Ctrl Pts',(-11.241082235174,17.5056887480822,4.282071235387));
#88404=CARTESIAN_POINT('Ctrl Pts',(-11.3137233050653,17.4981232185244,4.14711201045561));
#88405=CARTESIAN_POINT('Ctrl Pts',(-11.3362213109601,17.4954650164465,4.09927827994936));
#88406=CARTESIAN_POINT('Ctrl Pts',(-11.3599703610437,17.4921239996376,4.04075849799416));
#88407=CARTESIAN_POINT('Ctrl Pts',(-11.3637563742515,17.4915719389034,4.03113809474442));
#88408=CARTESIAN_POINT('Ctrl Pts',(-11.3688971448324,17.4907934175572,4.01765778190089));
#88409=CARTESIAN_POINT('Ctrl Pts',(-11.3703382141775,17.4905718491006,4.01383085761642));
#88410=CARTESIAN_POINT('Ctrl Pts',(-11.3727625386571,17.4901932911696,4.00731004933062));
#88411=CARTESIAN_POINT('Ctrl Pts',(-11.3737539616162,17.4900367814853,4.00461918960409));
#88412=CARTESIAN_POINT('Ctrl Pts',(-11.37564102332,17.4897355675442,3.99945066411598));
#88413=CARTESIAN_POINT('Ctrl Pts',(-11.3765378879962,17.4895909413184,3.99697347374855));
#88414=CARTESIAN_POINT('Ctrl Pts',(-11.3789060998942,17.4892051405479,3.99037674620755));
#88415=CARTESIAN_POINT('Ctrl Pts',(-11.3803656621054,17.4889632850971,3.98625304463578));
#88416=CARTESIAN_POINT('Ctrl Pts',(-11.3855398127446,17.4880912300412,3.97142347368022));
#88417=CARTESIAN_POINT('Ctrl Pts',(-11.3891484184817,17.4874552490466,3.96068136443337));
#88418=CARTESIAN_POINT('Ctrl Pts',(-11.416662355422,17.4823852448033,3.87551379928805));
#88419=CARTESIAN_POINT('Ctrl Pts',(-11.4346925467503,17.4776902797076,3.79932930308715));
#88420=CARTESIAN_POINT('Ctrl Pts',(-11.4577793617561,17.4685288148826,3.64894812463189));
#88421=CARTESIAN_POINT('Ctrl Pts',(-11.4634454599711,17.4640771657698,3.57506731411596));
#88422=CARTESIAN_POINT('Ctrl Pts',(-11.4634998694394,17.4597393327923,3.50071396372807));
#88423=CARTESIAN_POINT('Ctrl Pts',(-11.4635,17.4597185093157,3.5003569817236));
#88424=CARTESIAN_POINT('Ctrl Pts',(-11.4635,17.4596976889334,3.50000000000147));
#88425=CARTESIAN_POINT('Ctrl Pts',(-11.4635,17.3900944100234,3.49999999998336));
#88426=CARTESIAN_POINT('Ctrl Pts',(-11.4635,17.3901118316435,3.50035017971462));
#88427=CARTESIAN_POINT('Ctrl Pts',(-11.4634998743219,17.3901292509645,3.50070036152164));
#88428=CARTESIAN_POINT('Ctrl Pts',(-11.4634232107731,17.3954410713135,3.60749892398405));
#88429=CARTESIAN_POINT('Ctrl Pts',(-11.4517336778086,17.4004712680935,3.71361410049286));
#88430=CARTESIAN_POINT('Ctrl Pts',(-11.4265572899447,17.4062653768113,3.82689258636057));
#88431=CARTESIAN_POINT('Ctrl Pts',(-11.4243816898007,17.4067472219701,3.83624583449666));
#88432=CARTESIAN_POINT('Ctrl Pts',(-11.4135765864115,17.4090570377892,3.88071088108472));
#88433=CARTESIAN_POINT('Ctrl Pts',(-11.4037405105374,17.4109219057271,3.91551379594425));
#88434=CARTESIAN_POINT('Ctrl Pts',(-11.3908044029715,17.4131714204938,3.95555516354608));
#88435=CARTESIAN_POINT('Ctrl Pts',(-11.3889476865259,17.4134901425403,3.96118512126444));
#88436=CARTESIAN_POINT('Ctrl Pts',(-11.3859119343481,17.414004946086,3.97020553439422));
#88437=CARTESIAN_POINT('Ctrl Pts',(-11.3847545215386,17.4141998053295,3.97360326103394));
#88438=CARTESIAN_POINT('Ctrl Pts',(-11.3826724427108,17.414547904469,3.97964257435268));
#88439=CARTESIAN_POINT('Ctrl Pts',(-11.3817526860329,17.4147008560748,3.98228580478788));
#88440=CARTESIAN_POINT('Ctrl Pts',(-11.3797691210174,17.4150289910918,3.9879339952793));
#88441=CARTESIAN_POINT('Ctrl Pts',(-11.378703092195,17.4152042991161,3.99093807576274));
#88442=CARTESIAN_POINT('Ctrl Pts',(-11.3757515294863,17.4156868029366,3.99917017810984));
#88443=CARTESIAN_POINT('Ctrl Pts',(-11.373846036362,17.4159951399575,4.0043909237259));
#88444=CARTESIAN_POINT('Ctrl Pts',(-11.3634697797325,17.4176569957082,4.03232515171355));
#88445=CARTESIAN_POINT('Ctrl Pts',(-11.3544658479301,17.4190390050037,4.05483514030286));
#88446=CARTESIAN_POINT('Ctrl Pts',(-11.3248763417866,17.423383834201,4.12379109733525));
#88447=CARTESIAN_POINT('Ctrl Pts',(-11.3024292909585,17.4264157589203,4.16939523533212));
#88448=CARTESIAN_POINT('Ctrl Pts',(-11.2134287976125,17.4373835713428,4.32871474393081));
#88449=CARTESIAN_POINT('Ctrl Pts',(-11.1339572335214,17.4453196294646,4.43452212936244));
#88450=CARTESIAN_POINT('Ctrl Pts',(-11.0305686817836,17.4535245710539,4.53922929663182));
#88451=CARTESIAN_POINT('Ctrl Pts',(-11.0195775655764,17.4543756868927,4.55001473898854));
#88452=CARTESIAN_POINT('Ctrl Pts',(-11.0039785927214,17.4555548920237,4.5648458852139));
#88453=CARTESIAN_POINT('Ctrl Pts',(-10.9995127015503,17.4558892900867,4.56903888373531));
#88454=CARTESIAN_POINT('Ctrl Pts',(-10.9912871632337,17.4564994221153,4.57666518926656));
#88455=CARTESIAN_POINT('Ctrl Pts',(-10.9875356899264,17.4567755207186,4.58010713903906));
#88456=CARTESIAN_POINT('Ctrl Pts',(-10.9799015531358,17.4573330368785,4.58703838242448));
#88457=CARTESIAN_POINT('Ctrl Pts',(-10.9760180279437,17.4576144081816,4.59052661994265));
#88458=CARTESIAN_POINT('Ctrl Pts',(-10.9663976867104,17.4583059808391,4.5990751917334));
#88459=CARTESIAN_POINT('Ctrl Pts',(-10.9606396642389,17.4587151838444,4.6041115000149));
#88460=CARTESIAN_POINT('Ctrl Pts',(-10.9391536579251,17.4602250190152,4.62260911289105));
#88461=CARTESIAN_POINT('Ctrl Pts',(-10.9231796797913,17.461313912191,4.63578173463947));
#88462=CARTESIAN_POINT('Ctrl Pts',(-10.8262236512845,17.4677373760064,4.71233715438699));
#88463=CARTESIAN_POINT('Ctrl Pts',(-10.7390244388223,17.4727330272248,4.76738001320493));
#88464=CARTESIAN_POINT('Ctrl Pts',(-10.5681313606736,17.4819959013363,4.85157077544888));
#88465=CARTESIAN_POINT('Ctrl Pts',(-10.4861818901234,17.4862531774624,4.88316316703846));
#88466=CARTESIAN_POINT('Ctrl Pts',(-10.3910954852738,17.4914700777515,4.91032020450472));
#88467=CARTESIAN_POINT('Ctrl Pts',(-10.380245438761,17.4920694113205,4.91328417128766));
#88468=CARTESIAN_POINT('Ctrl Pts',(-10.3651422310072,17.4929106292886,4.91722349145991));
#88469=CARTESIAN_POINT('Ctrl Pts',(-10.3609169759793,17.4931467182116,4.91830540049501));
#88470=CARTESIAN_POINT('Ctrl Pts',(-10.3541336692455,17.4935270337457,4.92001004416762));
#88471=CARTESIAN_POINT('Ctrl Pts',(-10.3515786297263,17.4936705792308,4.9206448001254));
#88472=CARTESIAN_POINT('Ctrl Pts',(-10.3462336226318,17.4939715083602,4.9219573734681));
#88473=CARTESIAN_POINT('Ctrl Pts',(-10.3434433669256,17.4941289684383,4.92263387652933));
#88474=CARTESIAN_POINT('Ctrl Pts',(-10.3366606061746,17.4945125933328,4.92425725313198));
#88475=CARTESIAN_POINT('Ctrl Pts',(-10.3326660877724,17.4947392400125,4.925195551515));
#88476=CARTESIAN_POINT('Ctrl Pts',(-10.3185117594551,17.4955447689318,4.92845760562177));
#88477=CARTESIAN_POINT('Ctrl Pts',(-10.3083313731042,17.496128545168,4.93068956228364));
#88478=CARTESIAN_POINT('Ctrl Pts',(-10.2455902909537,17.4997496787971,4.94374423138855));
#88479=CARTESIAN_POINT('Ctrl Pts',(-10.1924952005466,17.5029132940792,4.95177703559117));
#88480=CARTESIAN_POINT('Ctrl Pts',(-10.0456223210248,17.5117337608868,4.9657986311013));
#88481=CARTESIAN_POINT('Ctrl Pts',(-9.95150994499491,17.517447464102,4.96570733375202));
#88482=CARTESIAN_POINT('Ctrl Pts',(-9.80019365985088,17.5263611925037,4.9509614905418));
#88483=CARTESIAN_POINT('Ctrl Pts',(-9.74271634377965,17.5296864863694,4.94188010459113));
#88484=CARTESIAN_POINT('Ctrl Pts',(-9.67604753182678,17.5334646805047,4.92723135503667));
#88485=CARTESIAN_POINT('Ctrl Pts',(-9.66619180273169,17.5340212531672,4.92495846855044));
#88486=CARTESIAN_POINT('Ctrl Pts',(-9.65017652801991,17.5349226063282,4.92108981353197));
#88487=CARTESIAN_POINT('Ctrl Pts',(-9.6440025453729,17.5352693387079,4.91955575225472));
#88488=CARTESIAN_POINT('Ctrl Pts',(-9.63299648130918,17.5358861620822,4.91674473486965));
#88489=CARTESIAN_POINT('Ctrl Pts',(-9.62816059589988,17.5361567412584,4.91548319839224));
#88490=CARTESIAN_POINT('Ctrl Pts',(-9.61794993275202,17.5367271488579,4.91276360682446));
#88491=CARTESIAN_POINT('Ctrl Pts',(-9.61257681493703,17.5370267811562,4.91129959239862));
#88492=CARTESIAN_POINT('Ctrl Pts',(-9.5982955130578,17.537821831745,4.90732065745172));
#88493=CARTESIAN_POINT('Ctrl Pts',(-9.58940252946597,17.5383155091124,4.90475181089187));
#88494=CARTESIAN_POINT('Ctrl Pts',(-9.54677043447824,17.5406760592543,4.89199757467937));
#88495=CARTESIAN_POINT('Ctrl Pts',(-9.51338085990163,17.5425060392056,4.88067967296219));
#88496=CARTESIAN_POINT('Ctrl Pts',(-9.37419781118695,17.5500997038759,4.82782408244247));
#88497=CARTESIAN_POINT('Ctrl Pts',(-9.27302938255267,17.5554988953047,4.77524864099147));
#88498=CARTESIAN_POINT('Ctrl Pts',(-9.12513788524783,17.5642702890941,4.67502166454493));
#88499=CARTESIAN_POINT('Ctrl Pts',(-9.07381148279971,17.5675211284077,4.63500333362759));
#88500=CARTESIAN_POINT('Ctrl Pts',(-9.0199042704289,17.5713762511422,4.58687503687647));
#88501=CARTESIAN_POINT('Ctrl Pts',(-9.01452338673882,17.5717663172343,4.58199853293749));
#88502=CARTESIAN_POINT('Ctrl Pts',(-9.00656977660599,17.5723511494341,4.5746819119016));
#88503=CARTESIAN_POINT('Ctrl Pts',(-9.00396918328724,17.5725437053308,4.57227208866901));
#88504=CARTESIAN_POINT('Ctrl Pts',(-8.9993387550151,17.5728890007823,4.56794995198253));
#88505=CARTESIAN_POINT('Ctrl Pts',(-8.99730560421565,17.5730414665856,4.56604126358206));
#88506=CARTESIAN_POINT('Ctrl Pts',(-8.9929096653069,17.5733729821718,4.56189072697876));
#88507=CARTESIAN_POINT('Ctrl Pts',(-8.99054893467253,17.5735521854983,4.55964683010825));
#88508=CARTESIAN_POINT('Ctrl Pts',(-8.98395114377067,17.5740562661145,4.55333351071517));
#88509=CARTESIAN_POINT('Ctrl Pts',(-8.97973111711057,17.574382455711,4.54924647593237));
#88510=CARTESIAN_POINT('Ctrl Pts',(-8.95464460600604,17.5763435820412,4.52465611233313));
#88511=CARTESIAN_POINT('Ctrl Pts',(-8.93437342704047,17.5780201598257,4.50355758071698));
#88512=CARTESIAN_POINT('Ctrl Pts',(-8.82645584321613,17.5873963767549,4.38427710832873));
#88513=CARTESIAN_POINT('Ctrl Pts',(-8.75172550222423,17.5955351852506,4.27522152949078));
#88514=CARTESIAN_POINT('Ctrl Pts',(-8.6858230676814,17.6040902584944,4.14420280271838));
#88515=CARTESIAN_POINT('Ctrl Pts',(-8.67927480077941,17.6049616629923,4.13066887432615));
#88516=CARTESIAN_POINT('Ctrl Pts',(-8.65651336366731,17.6080686923473,4.08171569292694));
#88517=CARTESIAN_POINT('Ctrl Pts',(-8.64150633373492,17.6102674235222,4.04575163792697));
#88518=CARTESIAN_POINT('Ctrl Pts',(-8.62451288263724,17.6129639794557,3.99996508175568));
#88519=CARTESIAN_POINT('Ctrl Pts',(-8.62116845990515,17.6135064680905,3.99066636707362));
#88520=CARTESIAN_POINT('Ctrl Pts',(-8.61602252330961,17.6143605062135,3.97589055785633));
#88521=CARTESIAN_POINT('Ctrl Pts',(-8.61415879484026,17.6146740931979,3.97043557949224));
#88522=CARTESIAN_POINT('Ctrl Pts',(-8.61074723463179,17.6152562600888,3.96025399322193));
#88523=CARTESIAN_POINT('Ctrl Pts',(-8.60919117785093,17.615525105987,3.9555302464576));
#88524=CARTESIAN_POINT('Ctrl Pts',(-8.60578839601599,17.6161205256032,3.94502038301076));
#88525=CARTESIAN_POINT('Ctrl Pts',(-8.60395354374617,17.6164467085272,3.93923049926078));
#88526=CARTESIAN_POINT('Ctrl Pts',(-8.59872036833839,17.6173923032128,3.92235307708058));
#88527=CARTESIAN_POINT('Ctrl Pts',(-8.59541767493327,17.6180086133816,3.91123622194467));
#88528=CARTESIAN_POINT('Ctrl Pts',(-8.56747824567873,17.6234039610684,3.81292663561796));
#88529=CARTESIAN_POINT('Ctrl Pts',(-8.55085475199813,17.6279072818749,3.72365695569299));
#88530=CARTESIAN_POINT('Ctrl Pts',(-8.533580578868,17.6371570833504,3.53495418990895));
#88531=CARTESIAN_POINT('Ctrl Pts',(-8.53456894239786,17.6418671210789,3.43584470829085));
#88532=CARTESIAN_POINT('Ctrl Pts',(-8.54807202494477,17.6481363896877,3.31490854797101));
#88533=CARTESIAN_POINT('Ctrl Pts',(-8.55113658133171,17.6493331163671,3.29227814268081));
#88534=CARTESIAN_POINT('Ctrl Pts',(-8.55561816506595,17.6508601616528,3.26414985019038));
#88535=CARTESIAN_POINT('Ctrl Pts',(-8.55653952240296,17.6511647629068,3.25857501004589));
#88536=CARTESIAN_POINT('Ctrl Pts',(-8.55804020900779,17.6516469034471,3.24981063341906));
#88537=CARTESIAN_POINT('Ctrl Pts',(-8.55859790152844,17.6518232524112,3.24661738794344));
#88538=CARTESIAN_POINT('Ctrl Pts',(-8.55965541389894,17.6521525344702,3.2406787507769));
#88539=CARTESIAN_POINT('Ctrl Pts',(-8.56015247923612,17.6523053123376,3.23793292164641));
#88540=CARTESIAN_POINT('Ctrl Pts',(-8.56130283555837,17.6526544038414,3.23168033414738));
#88541=CARTESIAN_POINT('Ctrl Pts',(-8.56196109393796,17.6528509930842,3.22817454469519));
#88542=CARTESIAN_POINT('Ctrl Pts',(-8.56401891739766,17.6534559626331,3.21743157247173));
#88543=CARTESIAN_POINT('Ctrl Pts',(-8.56546032705713,17.6538666005006,3.21020264331594));
#88544=CARTESIAN_POINT('Ctrl Pts',(-8.5689306762007,17.6548254945706,3.19345883145994));
#88545=CARTESIAN_POINT('Ctrl Pts',(-8.57099998959353,17.6553757334034,3.18395275969089));
#88546=CARTESIAN_POINT('Ctrl Pts',(-8.57849725574626,17.6572964512541,3.15109153798487));
#88547=CARTESIAN_POINT('Ctrl Pts',(-8.58440407701065,17.6586875463456,3.12785051971576));
#88548=CARTESIAN_POINT('Ctrl Pts',(-8.61956688884625,17.6663328876613,3.00248503434452));
#88549=CARTESIAN_POINT('Ctrl Pts',(-8.65930538374638,17.6728484501436,2.9036308438086));
#88550=CARTESIAN_POINT('Ctrl Pts',(-8.74220046611629,17.6832461170692,2.74859271691442));
#88551=CARTESIAN_POINT('Ctrl Pts',(-8.7793407174693,17.6872548381788,2.68965089974101));
#88552=CARTESIAN_POINT('Ctrl Pts',(-8.82672939338587,17.6916886023975,2.62514133882135));
#88553=CARTESIAN_POINT('Ctrl Pts',(-8.83301031450446,17.6922643482836,2.61678050558614));
#88554=CARTESIAN_POINT('Ctrl Pts',(-8.8432762975806,17.6931866248221,2.60341568834927));
#88555=CARTESIAN_POINT('Ctrl Pts',(-8.84720541888654,17.6935353165691,2.59836936209461));
#88556=CARTESIAN_POINT('Ctrl Pts',(-8.85427438624654,17.6941551124248,2.58941215777186));
#88557=CARTESIAN_POINT('Ctrl Pts',(-8.8574014761455,17.6944267128967,2.58549138080646));
#88558=CARTESIAN_POINT('Ctrl Pts',(-8.86399630381798,17.6949941681164,2.57730935074074));
#88559=CARTESIAN_POINT('Ctrl Pts',(-8.86746801186787,17.6952898587108,2.57305138817842));
#88560=CARTESIAN_POINT('Ctrl Pts',(-8.8766369162829,17.6960629488439,2.56193436571817));
#88561=CARTESIAN_POINT('Ctrl Pts',(-8.88237301143417,17.6965387770117,2.55510758747513));
#88562=CARTESIAN_POINT('Ctrl Pts',(-8.90865565954354,17.6986845061437,2.52440165625672));
#88563=CARTESIAN_POINT('Ctrl Pts',(-8.92990829573542,17.7003253466624,2.50113638001455));
#88564=CARTESIAN_POINT('Ctrl Pts',(-8.9904530631839,17.7047702522717,2.43901030343049));
#88565=CARTESIAN_POINT('Ctrl Pts',(-9.03122073871089,17.7075139161828,2.40165964840001));
#88566=CARTESIAN_POINT('Ctrl Pts',(-9.13563208172349,17.7141199661283,2.31634724544742));
#88567=CARTESIAN_POINT('Ctrl Pts',(-9.20126134074058,17.7179283050911,2.27110560290923));
#88568=CARTESIAN_POINT('Ctrl Pts',(-9.31230364533523,17.7243025098907,2.20722746515281));
#88569=CARTESIAN_POINT('Ctrl Pts',(-9.35554082193359,17.7267714388952,2.18513932948893));
#88570=CARTESIAN_POINT('Ctrl Pts',(-9.40611147556573,17.7297316157522,2.16239889929933));
#88571=CARTESIAN_POINT('Ctrl Pts',(-9.4124524456134,17.7301040600874,2.15960149522739));
#88572=CARTESIAN_POINT('Ctrl Pts',(-9.42204864971335,17.7306699624267,2.15544917650193));
#88573=CARTESIAN_POINT('Ctrl Pts',(-9.42528939379872,17.7308614600435,2.15406077445715));
#88574=CARTESIAN_POINT('Ctrl Pts',(-9.43110111608624,17.7312056225211,2.15159572866431));
#88575=CARTESIAN_POINT('Ctrl Pts',(-9.43367018266171,17.7313580211446,2.15051470667567));
#88576=CARTESIAN_POINT('Ctrl Pts',(-9.43926164896605,17.7316902908853,2.14818068654894));
#88577=CARTESIAN_POINT('Ctrl Pts',(-9.44228512644287,17.731870321579,2.14693049922756));
#88578=CARTESIAN_POINT('Ctrl Pts',(-9.45081215716482,17.7323790230291,2.1434380662092));
#88579=CARTESIAN_POINT('Ctrl Pts',(-9.45632514717821,17.7327090441116,2.14121921603814));
#88580=CARTESIAN_POINT('Ctrl Pts',(-9.4902068885551,17.7347435125991,2.12782181136136));
#88581=CARTESIAN_POINT('Ctrl Pts',(-9.51890391212215,17.7364932168763,2.11749926359997));
#88582=CARTESIAN_POINT('Ctrl Pts',(-9.68976715258485,17.7469809485578,2.06200231590536));
#88583=CARTESIAN_POINT('Ctrl Pts',(-9.83785353769738,17.7562366134552,2.03787712513248));
#88584=CARTESIAN_POINT('Ctrl Pts',(-10.022750255126,17.7668392697681,2.03624148279399));
#88585=CARTESIAN_POINT('Ctrl Pts',(-10.0584480154951,17.7688493976806,2.037231832681));
#88586=CARTESIAN_POINT('Ctrl Pts',(-10.1036437061987,17.7713484283084,2.04014310637531));
#88587=CARTESIAN_POINT('Ctrl Pts',(-10.1132051167827,17.7718745279285,2.04085340853659));
#88588=CARTESIAN_POINT('Ctrl Pts',(-10.1284356838471,17.772708569787,2.04213547338658));
#88589=CARTESIAN_POINT('Ctrl Pts',(-10.1341095636404,17.7730183929772,2.04264646394079));
#88590=CARTESIAN_POINT('Ctrl Pts',(-10.1447365703374,17.7735970653998,2.04366612164185));
#88591=CARTESIAN_POINT('Ctrl Pts',(-10.1496903513523,17.7738661541973,2.04416696025721));
#88592=CARTESIAN_POINT('Ctrl Pts',(-10.1607695559939,17.7744665366552,2.04534424117778));
#88593=CARTESIAN_POINT('Ctrl Pts',(-10.1668934776774,17.7747974066536,2.04603411473797));
#88594=CARTESIAN_POINT('Ctrl Pts',(-10.1849565524343,17.7757705348163,2.04818458616306));
#88595=CARTESIAN_POINT('Ctrl Pts',(-10.1968824234658,17.7764094028898,2.04975372955319));
#88596=CARTESIAN_POINT('Ctrl Pts',(-10.3145222023831,17.7826786809046,2.06671005826602));
#88597=CARTESIAN_POINT('Ctrl Pts',(-10.4182719623035,17.7879136466969,2.09348082910684));
#88598=CARTESIAN_POINT('Ctrl Pts',(-10.6086148518675,17.797810547104,2.16554568724975));
#88599=CARTESIAN_POINT('Ctrl Pts',(-10.6954106355574,17.802467316993,2.20865197085244));
#88600=CARTESIAN_POINT('Ctrl Pts',(-10.7865368028056,17.8081459059013,2.26577527437407));
#88601=CARTESIAN_POINT('Ctrl Pts',(-10.7956976482237,17.8087264481061,2.27166126244881));
#88602=CARTESIAN_POINT('Ctrl Pts',(-10.8083954067449,17.8095459718198,2.28002142120657));
#88603=CARTESIAN_POINT('Ctrl Pts',(-10.8119885673194,17.8097795586055,2.28240999020734));
#88604=CARTESIAN_POINT('Ctrl Pts',(-10.8179436068104,17.8101695823702,2.28640671123506));
#88605=CARTESIAN_POINT('Ctrl Pts',(-10.8203114573716,17.8103254300458,2.28800597069467));
#88606=CARTESIAN_POINT('Ctrl Pts',(-10.8250403624105,17.8106382457493,2.29122010571193));
#88607=CARTESIAN_POINT('Ctrl Pts',(-10.8274013960218,17.8107952141674,2.29283498973477));
#88608=CARTESIAN_POINT('Ctrl Pts',(-10.8332399417959,17.8111852997872,2.29685357484579));
#88609=CARTESIAN_POINT('Ctrl Pts',(-10.8367117792895,17.8114189582012,2.2992654254785));
#88610=CARTESIAN_POINT('Ctrl Pts',(-10.8441874103144,17.8119256661923,2.30450683688911));
#88611=CARTESIAN_POINT('Ctrl Pts',(-10.8481875217635,17.8121990415199,2.30734153533154));
#88612=CARTESIAN_POINT('Ctrl Pts',(-10.9042380773631,17.8160604130468,2.34748662992855));
#88613=CARTESIAN_POINT('Ctrl Pts',(-10.9537939315528,17.8198464211563,2.38815064265674));
#88614=CARTESIAN_POINT('Ctrl Pts',(-11.0526219357131,17.8279614156668,2.48072793096994));
#88615=CARTESIAN_POINT('Ctrl Pts',(-11.1010830048244,17.8322899445141,2.53328114616172));
#88616=CARTESIAN_POINT('Ctrl Pts',(-11.1918909404484,17.8409473916704,2.64748570978296));
#88617=CARTESIAN_POINT('Ctrl Pts',(-11.2337491099602,17.8452543222788,2.70927222607752));
#88618=CARTESIAN_POINT('Ctrl Pts',(-11.2759690350652,17.8499696596895,2.78316870735907));
#88619=CARTESIAN_POINT('Ctrl Pts',(-11.2811154986643,17.8505520234833,2.79240748457018));
#88620=CARTESIAN_POINT('Ctrl Pts',(-11.2892296449729,17.8514827883663,2.80735252733558));
#88621=CARTESIAN_POINT('Ctrl Pts',(-11.2922605761713,17.8518334148956,2.81302386942059));
#88622=CARTESIAN_POINT('Ctrl Pts',(-11.2975909164472,17.8524554171044,2.82315787441935));
#88623=CARTESIAN_POINT('Ctrl Pts',(-11.2999049141898,17.852727301782,2.82761271253535));
#88624=CARTESIAN_POINT('Ctrl Pts',(-11.3046952994113,17.8532941181707,2.83695217650359));
#88625=CARTESIAN_POINT('Ctrl Pts',(-11.3071672861186,17.8535888933793,2.84183898036212));
#88626=CARTESIAN_POINT('Ctrl Pts',(-11.3135565241108,17.8543568766343,2.85464768788544));
#88627=CARTESIAN_POINT('Ctrl Pts',(-11.3174295860666,17.8548285517584,2.8625914660458));
#88628=CARTESIAN_POINT('Ctrl Pts',(-11.3344312558645,17.8569275597156,2.89827950674739));
#88629=CARTESIAN_POINT('Ctrl Pts',(-11.3467575681557,17.8585273990875,2.92639860804597));
#88630=CARTESIAN_POINT('Ctrl Pts',(-11.3779860108728,17.862827697885,3.00420653259897));
#88631=CARTESIAN_POINT('Ctrl Pts',(-11.3950807055843,17.8654727992214,3.05457097368899));
#88632=CARTESIAN_POINT('Ctrl Pts',(-11.4422329324372,17.8740621023824,3.22313749027782));
#88633=CARTESIAN_POINT('Ctrl Pts',(-11.460270395434,17.8797855169432,3.34414361695665));
#88634=CARTESIAN_POINT('Ctrl Pts',(-11.4633680666843,17.8867754093377,3.47730877028001));
#88635=CARTESIAN_POINT('Ctrl Pts',(-11.4635,17.8873766710606,3.48865438790481));
#88636=CARTESIAN_POINT('Ctrl Pts',(-11.4635,17.8879846534521,3.50000000000001));
#88637=CARTESIAN_POINT('Origin',(-10.,13.2,3.5));
#88638=CARTESIAN_POINT('',(-11.4635,18.4603263886907,3.50000000004768));
#88639=CARTESIAN_POINT('',(-11.4635,18.3899253605917,3.49999999994518));
#88640=CARTESIAN_POINT('',(-11.4635,13.2,3.5));
#88641=CARTESIAN_POINT('',(-11.463499980138,17.9619694309472,3.50024111453588));
#88642=CARTESIAN_POINT('Ctrl Pts',(-11.4635,18.4603263886907,3.50000000004768));
#88643=CARTESIAN_POINT('Ctrl Pts',(-11.4635,18.460305879277,3.49958063693336));
#88644=CARTESIAN_POINT('Ctrl Pts',(-11.4634998197481,18.4602853715295,3.49916126965186));
#88645=CARTESIAN_POINT('Ctrl Pts',(-11.4634249137899,18.4560247057668,3.41202621381093));
#88646=CARTESIAN_POINT('Ctrl Pts',(-11.4556434752369,18.4518825987025,3.32549418675632));
#88647=CARTESIAN_POINT('Ctrl Pts',(-11.4378193502063,18.4468251008909,3.22669595506432));
#88648=CARTESIAN_POINT('Ctrl Pts',(-11.4352005304622,18.4461299873744,3.21326143532275));
#88649=CARTESIAN_POINT('Ctrl Pts',(-11.4272159367172,18.4441323921311,3.17515485567764));
#88650=CARTESIAN_POINT('Ctrl Pts',(-11.4213998510644,18.4428132252866,3.15058332916228));
#88651=CARTESIAN_POINT('Ctrl Pts',(-11.4134598854698,18.4411478132214,3.12052996780278));
#88652=CARTESIAN_POINT('Ctrl Pts',(-11.4119344631874,18.4408331646694,3.11489297263277));
#88653=CARTESIAN_POINT('Ctrl Pts',(-11.4094985223399,18.4403386017206,3.10610032778138));
#88654=CARTESIAN_POINT('Ctrl Pts',(-11.4086110313423,18.44015998106,3.10293829421691));
#88655=CARTESIAN_POINT('Ctrl Pts',(-11.4069512519329,18.439828737345,3.09710028297323));
#88656=CARTESIAN_POINT('Ctrl Pts',(-11.4061819639129,18.4396762872046,3.09442350746303));
#88657=CARTESIAN_POINT('Ctrl Pts',(-11.4044268224553,18.4393308837154,3.08838142973162));
#88658=CARTESIAN_POINT('Ctrl Pts',(-11.4034365171435,18.4391376777022,3.08501748369245));
#88659=CARTESIAN_POINT('Ctrl Pts',(-11.4004128728132,18.4385528517805,3.0748811512526));
#88660=CARTESIAN_POINT('Ctrl Pts',(-11.3983425626439,18.4381591820158,3.06812001286215));
#88661=CARTESIAN_POINT('Ctrl Pts',(-11.3728629401674,18.4333958802512,2.98701385942724));
#88662=CARTESIAN_POINT('Ctrl Pts',(-11.3436016507737,18.4287379334421,2.91464580565684));
#88663=CARTESIAN_POINT('Ctrl Pts',(-11.2527196815604,18.4165204839546,2.73307023446575));
#88664=CARTESIAN_POINT('Ctrl Pts',(-11.1825871214322,18.409007181454,2.62880155910358));
#88665=CARTESIAN_POINT('Ctrl Pts',(-11.0895831235252,18.4011348357045,2.52281435772815));
#88666=CARTESIAN_POINT('Ctrl Pts',(-11.0789425202442,18.4002583535346,2.51107824967673));
#88667=CARTESIAN_POINT('Ctrl Pts',(-11.0637612340603,18.3990407746432,2.49487074824493));
#88668=CARTESIAN_POINT('Ctrl Pts',(-11.0593789778347,18.3986930308012,2.49025302231686));
#88669=CARTESIAN_POINT('Ctrl Pts',(-11.0517189109866,18.3980915581022,2.4822861206325));
#88670=CARTESIAN_POINT('Ctrl Pts',(-11.04845491002,18.3978372425868,2.47892384693884));
#88671=CARTESIAN_POINT('Ctrl Pts',(-11.04161781106,18.3973085991602,2.47194824660048));
#88672=CARTESIAN_POINT('Ctrl Pts',(-11.0380419249297,18.3970343976213,2.46833773211748));
#88673=CARTESIAN_POINT('Ctrl Pts',(-11.0295390167171,18.3963877222697,2.45984145077911));
#88674=CARTESIAN_POINT('Ctrl Pts',(-11.0245958858855,18.3960159626125,2.45497192987823));
#88675=CARTESIAN_POINT('Ctrl Pts',(-11.0080203867486,18.3947830139337,2.43887393179582));
#88676=CARTESIAN_POINT('Ctrl Pts',(-10.9962363865108,18.393928590349,2.4278028528805));
#88677=CARTESIAN_POINT('Ctrl Pts',(-10.9312974310554,18.3893336115024,2.36878776201491));
#88678=CARTESIAN_POINT('Ctrl Pts',(-10.8748609018125,18.3857506221195,2.32459540473324));
#88679=CARTESIAN_POINT('Ctrl Pts',(-10.7602217348753,18.3789751071697,2.2476772451079));
#88680=CARTESIAN_POINT('Ctrl Pts',(-10.7025747185099,18.3757794943974,2.21445032764282));
#88681=CARTESIAN_POINT('Ctrl Pts',(-10.5848150770486,18.3693420686225,2.1568694164821));
#88682=CARTESIAN_POINT('Ctrl Pts',(-10.5249499028337,18.3661096351238,2.13236182701676));
#88683=CARTESIAN_POINT('Ctrl Pts',(-10.4567851587557,18.3622757321086,2.10959277657474));
#88684=CARTESIAN_POINT('Ctrl Pts',(-10.449884208799,18.3618858722579,2.10734457867439));
#88685=CARTESIAN_POINT('Ctrl Pts',(-10.4395892032237,18.3613013292265,2.10407516594304));
#88686=CARTESIAN_POINT('Ctrl Pts',(-10.4362075924814,18.3611088537747,2.10301476541483));
#88687=CARTESIAN_POINT('Ctrl Pts',(-10.4301591372461,18.3607636928539,2.10114220226178));
#88688=CARTESIAN_POINT('Ctrl Pts',(-10.4274937914302,18.3606112808486,2.10032536645806));
#88689=CARTESIAN_POINT('Ctrl Pts',(-10.4217102482266,18.3602798739353,2.0985709727797));
#88690=CARTESIAN_POINT('Ctrl Pts',(-10.418591294329,18.3601007255307,2.09763621706746));
#88691=CARTESIAN_POINT('Ctrl Pts',(-10.4098375950896,18.3595967810701,2.09504452326377));
#88692=CARTESIAN_POINT('Ctrl Pts',(-10.404196022321,18.359270673273,2.0934111051519));
#88693=CARTESIAN_POINT('Ctrl Pts',(-10.3703976567771,18.3573097057194,2.08384550561585));
#88694=CARTESIAN_POINT('Ctrl Pts',(-10.3420198034,18.3556332063853,2.07672553850967));
#88695=CARTESIAN_POINT('Ctrl Pts',(-10.1848960761534,18.3462568893866,2.04227359048706));
#88696=CARTESIAN_POINT('Ctrl Pts',(-10.0531243701796,18.3381178417071,2.0315530670365));
#88697=CARTESIAN_POINT('Ctrl Pts',(-9.90666535343219,18.3295622095059,2.03940180630877));
#88698=CARTESIAN_POINT('Ctrl Pts',(-9.89166027498138,18.3286904618118,2.04043809171958));
#88699=CARTESIAN_POINT('Ctrl Pts',(-9.83785841115321,18.32558299914,2.04498806172054));
#88700=CARTESIAN_POINT('Ctrl Pts',(-9.79918761131266,18.3233841785883,2.049819176046));
#88701=CARTESIAN_POINT('Ctrl Pts',(-9.75100867613171,18.3206877824563,2.05780267367915));
#88702=CARTESIAN_POINT('Ctrl Pts',(-9.74128086831317,18.3201455351903,2.05951597543374));
#88703=CARTESIAN_POINT('Ctrl Pts',(-9.72590646228866,18.3192918566514,2.06238454851116));
#88704=CARTESIAN_POINT('Ctrl Pts',(-9.72024818115562,18.3189783897852,2.0634748958149));
#88705=CARTESIAN_POINT('Ctrl Pts',(-9.70972022318426,18.3183964350008,2.06556818963613));
#88706=CARTESIAN_POINT('Ctrl Pts',(-9.7048489475392,18.3181276813513,2.06656258438403));
#88707=CARTESIAN_POINT('Ctrl Pts',(-9.69404005504112,18.3175324535535,2.06882648589941));
#88708=CARTESIAN_POINT('Ctrl Pts',(-9.68810506205997,18.317206370015,2.07010816332517));
#88709=CARTESIAN_POINT('Ctrl Pts',(-9.67086131093827,18.3162610291871,2.07394446699512));
#88710=CARTESIAN_POINT('Ctrl Pts',(-9.65957457624271,18.3156448720494,2.07659661339339));
#88711=CARTESIAN_POINT('Ctrl Pts',(-9.56037669508277,18.3102500411353,2.10115345727933));
#88712=CARTESIAN_POINT('Ctrl Pts',(-9.47464097754121,18.3057470404164,2.13104385555205));
#88713=CARTESIAN_POINT('Ctrl Pts',(-9.30227910286357,18.2964980561357,2.20973209765766));
#88714=CARTESIAN_POINT('Ctrl Pts',(-9.21674722820046,18.29178851166,2.25979147703072));
#88715=CARTESIAN_POINT('Ctrl Pts',(-9.11846348162114,18.2855188745269,2.33156170886885));
#88716=CARTESIAN_POINT('Ctrl Pts',(-9.10032389052748,18.2843210490912,2.3454708939321));
#88717=CARTESIAN_POINT('Ctrl Pts',(-9.07811571368894,18.2827928218647,2.36334105916751));
#88718=CARTESIAN_POINT('Ctrl Pts',(-9.07373360048407,18.2824881884611,2.3669092092179));
#88719=CARTESIAN_POINT('Ctrl Pts',(-9.06687094261138,18.2820060441997,2.37256356417207));
#88720=CARTESIAN_POINT('Ctrl Pts',(-9.06437642869678,18.2818297242262,2.37463282126245));
#88721=CARTESIAN_POINT('Ctrl Pts',(-9.0597478100679,18.2815005288813,2.37849839478609));
#88722=CARTESIAN_POINT('Ctrl Pts',(-9.05761195636958,18.2813478088793,2.38029253552979));
#88723=CARTESIAN_POINT('Ctrl Pts',(-9.0527581605981,18.2809988956974,2.38439350295164));
#88724=CARTESIAN_POINT('Ctrl Pts',(-9.05004351961214,18.2808024274578,2.38670415280383));
#88725=CARTESIAN_POINT('Ctrl Pts',(-9.04174726067114,18.2801979904188,2.3938182043957));
#88726=CARTESIAN_POINT('Ctrl Pts',(-9.03619352091398,18.2797877689786,2.39865375852849));
#88727=CARTESIAN_POINT('Ctrl Pts',(-9.02339644429872,18.2788299553239,2.40996689593485));
#88728=CARTESIAN_POINT('Ctrl Pts',(-9.01618072135711,18.2782803858726,2.41647506245189));
#88729=CARTESIAN_POINT('Ctrl Pts',(-8.99161186198607,18.2763778638458,2.43908250913721));
#88730=CARTESIAN_POINT('Ctrl Pts',(-8.97458544319715,18.2750049034491,2.45553006933888));
#88731=CARTESIAN_POINT('Ctrl Pts',(-8.88492225065472,18.2675092661216,2.54645112277648));
#88732=CARTESIAN_POINT('Ctrl Pts',(-8.81998344828882,18.2611325988924,2.62809635084505));
#88733=CARTESIAN_POINT('Ctrl Pts',(-8.72567769569843,18.2507048969611,2.77673087629157));
#88734=CARTESIAN_POINT('Ctrl Pts',(-8.69164126348345,18.2465502234151,2.84029144468313));
#88735=CARTESIAN_POINT('Ctrl Pts',(-8.65815195033402,18.2419784701932,2.91571701249542));
#88736=CARTESIAN_POINT('Ctrl Pts',(-8.65398887242578,18.241399510519,2.92537242457397));
#88737=CARTESIAN_POINT('Ctrl Pts',(-8.64745530838666,18.2404731726366,2.9409863941933));
#88738=CARTESIAN_POINT('Ctrl Pts',(-8.64501935067858,18.240123601725,2.94691700796016));
#88739=CARTESIAN_POINT('Ctrl Pts',(-8.64074723753743,18.2395028808195,2.95751558923527));
#88740=CARTESIAN_POINT('Ctrl Pts',(-8.63889597138808,18.2392312282752,2.96217732257645));
#88741=CARTESIAN_POINT('Ctrl Pts',(-8.63507131302106,18.23866430484,2.97195455633938));
#88742=CARTESIAN_POINT('Ctrl Pts',(-8.633102625493,18.2383691940049,2.97707182156747));
#88743=CARTESIAN_POINT('Ctrl Pts',(-8.62802372429944,18.2375990373238,2.99049822234671));
#88744=CARTESIAN_POINT('Ctrl Pts',(-8.62496020263657,18.2371255416287,2.99882485810536));
#88745=CARTESIAN_POINT('Ctrl Pts',(-8.61151180889401,18.2350051508829,3.03642929147105));
#88746=CARTESIAN_POINT('Ctrl Pts',(-8.60198460000047,18.2333864648875,3.06600647269196));
#88747=CARTESIAN_POINT('Ctrl Pts',(-8.57846400182034,18.229019738145,3.14787026383066));
#88748=CARTESIAN_POINT('Ctrl Pts',(-8.56641727500736,18.2263293464914,3.20066553553344));
#88749=CARTESIAN_POINT('Ctrl Pts',(-8.54183678321948,18.219158459604,3.34482448731));
#88750=CARTESIAN_POINT('Ctrl Pts',(-8.53496245012168,18.2147723729107,3.43689280186033));
#88751=CARTESIAN_POINT('Ctrl Pts',(-8.53754423832916,18.2082109869565,3.56720180067189));
#88752=CARTESIAN_POINT('Ctrl Pts',(-8.53979779232265,18.2062443440248,3.60536592954274));
#88753=CARTESIAN_POINT('Ctrl Pts',(-8.54413110599138,18.2038807562438,3.64937929689087));
#88754=CARTESIAN_POINT('Ctrl Pts',(-8.54475717141538,18.2035575305676,3.65535996349483));
#88755=CARTESIAN_POINT('Ctrl Pts',(-8.54581845721097,18.2030368785766,3.66492831928239));
#88756=CARTESIAN_POINT('Ctrl Pts',(-8.54623014663386,18.2028407197793,3.66851861250998));
#88757=CARTESIAN_POINT('Ctrl Pts',(-8.54698450569791,18.202491210542,3.67488873074131));
#88758=CARTESIAN_POINT('Ctrl Pts',(-8.54732186238593,18.2023381576455,3.67766913976863));
#88759=CARTESIAN_POINT('Ctrl Pts',(-8.54805816432342,18.2020108584658,3.68359523384247));
#88760=CARTESIAN_POINT('Ctrl Pts',(-8.5484593453137,18.2018364943468,3.68674054588089));
#88761=CARTESIAN_POINT('Ctrl Pts',(-8.54958233143627,18.2013590155019,3.69532259462514));
#88762=CARTESIAN_POINT('Ctrl Pts',(-8.55032447393351,18.201054797379,3.70075656009415));
#88763=CARTESIAN_POINT('Ctrl Pts',(-8.55437270390683,18.1994527304693,3.72920411785553));
#88764=CARTESIAN_POINT('Ctrl Pts',(-8.55819614186551,18.1981287061099,3.75213947688313));
#88765=CARTESIAN_POINT('Ctrl Pts',(-8.57148853977891,18.1940381126278,3.82162628792636));
#88766=CARTESIAN_POINT('Ctrl Pts',(-8.58267859708684,18.1912106438536,3.86781510999968));
#88767=CARTESIAN_POINT('Ctrl Pts',(-8.6003107719879,18.1874638655781,3.92769759981641));
#88768=CARTESIAN_POINT('Ctrl Pts',(-8.60474691571355,18.1865655478461,3.94195474631465));
#88769=CARTESIAN_POINT('Ctrl Pts',(-8.64656934134801,18.1784864386296,4.06945521901297));
#88770=CARTESIAN_POINT('Ctrl Pts',(-8.69745621073154,18.1713485237048,4.1778223515542));
#88771=CARTESIAN_POINT('Ctrl Pts',(-8.76965133232844,18.1637680148181,4.29268047655825));
#88772=CARTESIAN_POINT('Ctrl Pts',(-8.77859424787018,18.1628617674995,4.30639208900063));
#88773=CARTESIAN_POINT('Ctrl Pts',(-8.79138228111036,18.1616099622326,4.32529820714146));
#88774=CARTESIAN_POINT('Ctrl Pts',(-8.79503436204307,18.1612572570753,4.33062129417682));
#88775=CARTESIAN_POINT('Ctrl Pts',(-8.80141107217604,18.160649576428,4.33978509369104));
#88776=CARTESIAN_POINT('Ctrl Pts',(-8.80411921791235,18.160393984744,4.34363711229598));
#88777=CARTESIAN_POINT('Ctrl Pts',(-8.80977914911257,18.1598649053192,4.35160567984025));
#88778=CARTESIAN_POINT('Ctrl Pts',(-8.81273381393622,18.1595915319445,4.35572011320508));
#88779=CARTESIAN_POINT('Ctrl Pts',(-8.81973081911321,18.1589506969351,4.36535758699385));
#88780=CARTESIAN_POINT('Ctrl Pts',(-8.82379067892185,18.1585839132971,4.37086780161749));
#88781=CARTESIAN_POINT('Ctrl Pts',(-8.83724460269244,18.1573846738881,4.38886232623131));
#88782=CARTESIAN_POINT('Ctrl Pts',(-8.84680011058927,18.1565584771449,4.401224937952));
#88783=CARTESIAN_POINT('Ctrl Pts',(-8.89836939328373,18.1522279516469,4.46578011162198));
#88784=CARTESIAN_POINT('Ctrl Pts',(-8.94373413819298,18.1488605888867,4.51519701152448));
#88785=CARTESIAN_POINT('Ctrl Pts',(-9.06481012093965,18.1406413167421,4.63015092244525));
#88786=CARTESIAN_POINT('Ctrl Pts',(-9.14414358080489,18.1359038938782,4.69135582410406));
#88787=CARTESIAN_POINT('Ctrl Pts',(-9.23652317510664,18.1304278437169,4.74860397759186));
#88788=CARTESIAN_POINT('Ctrl Pts',(-9.24399906008339,18.1299848224608,4.75314457642625));
#88789=CARTESIAN_POINT('Ctrl Pts',(-9.27687815983106,18.1280350488744,4.77271292993974));
#88790=CARTESIAN_POINT('Ctrl Pts',(-9.30269041516959,18.1265008754473,4.78703632725073));
#88791=CARTESIAN_POINT('Ctrl Pts',(-9.33388411192781,18.124622099306,4.80313204432515));
#88792=CARTESIAN_POINT('Ctrl Pts',(-9.33886659823773,18.1243212710927,4.80566692703695));
#88793=CARTESIAN_POINT('Ctrl Pts',(-9.34701491198261,18.1238279070188,4.80975385298613));
#88794=CARTESIAN_POINT('Ctrl Pts',(-9.35017208711968,18.1236364077278,4.81132313473618));
#88795=CARTESIAN_POINT('Ctrl Pts',(-9.35583452461162,18.1232922920906,4.81411219250663));
#88796=CARTESIAN_POINT('Ctrl Pts',(-9.35833762876833,18.1231399422797,4.81533623661545));
#88797=CARTESIAN_POINT('Ctrl Pts',(-9.36378557944347,18.1228078407614,4.81798108921505));
#88798=CARTESIAN_POINT('Ctrl Pts',(-9.36673165664286,18.1226279299996,4.81939916072543));
#88799=CARTESIAN_POINT('Ctrl Pts',(-9.37503966427136,18.1221197282104,4.82336392003349));
#88800=CARTESIAN_POINT('Ctrl Pts',(-9.38041230908795,18.1217900904387,4.82588784476125));
#88801=CARTESIAN_POINT('Ctrl Pts',(-9.4133852256455,18.1197616676322,4.84113346643551));
#88802=CARTESIAN_POINT('Ctrl Pts',(-9.44135909527531,18.118017923052,4.85302473898123));
#88803=CARTESIAN_POINT('Ctrl Pts',(-9.60717476930379,18.1076332521575,4.91749171127662));
#88804=CARTESIAN_POINT('Ctrl Pts',(-9.75196863201047,18.098481726129,4.94985759566105));
#88805=CARTESIAN_POINT('Ctrl Pts',(-9.93627684388861,18.087870032089,4.96258483165601));
#88806=CARTESIAN_POINT('Ctrl Pts',(-9.97346048288491,18.0857737466383,4.96373188640445));
#88807=CARTESIAN_POINT('Ctrl Pts',(-10.0203754660057,18.0831841761497,4.96339047443034));
#88808=CARTESIAN_POINT('Ctrl Pts',(-10.0301001733236,18.0826503653312,4.96322275346304));
#88809=CARTESIAN_POINT('Ctrl Pts',(-10.0455479906651,18.0818069766843,4.96280225399948));
#88810=CARTESIAN_POINT('Ctrl Pts',(-10.0512724179839,18.0814954444591,4.96261279709148));
#88811=CARTESIAN_POINT('Ctrl Pts',(-10.061966088498,18.0809153026888,4.96219601857289));
#88812=CARTESIAN_POINT('Ctrl Pts',(-10.0669355555847,18.0806464409274,4.96197695778642));
#88813=CARTESIAN_POINT('Ctrl Pts',(-10.0780126845546,18.0800487430345,4.96143206451101));
#88814=CARTESIAN_POINT('Ctrl Pts',(-10.0841196351042,18.0797203139707,4.96109327103889));
#88815=CARTESIAN_POINT('Ctrl Pts',(-10.1020104719013,18.0787612406288,4.95998820418168));
#88816=CARTESIAN_POINT('Ctrl Pts',(-10.1137875738955,18.0781338387717,4.95911757292547));
#88817=CARTESIAN_POINT('Ctrl Pts',(-10.2383763393507,18.0715350691834,4.94838960110358));
#88818=CARTESIAN_POINT('Ctrl Pts',(-10.3496915224269,18.0660147711867,4.92561390740946));
#88819=CARTESIAN_POINT('Ctrl Pts',(-10.5430357221998,18.0561195033918,4.86201860559945));
#88820=CARTESIAN_POINT('Ctrl Pts',(-10.6259903220343,18.0517457478222,4.82593917085188));
#88821=CARTESIAN_POINT('Ctrl Pts',(-10.7148714271918,18.0463938439508,4.77707317547384));
#88822=CARTESIAN_POINT('Ctrl Pts',(-10.7245987176453,18.0457984844762,4.77157922926082));
#88823=CARTESIAN_POINT('Ctrl Pts',(-10.7380233564547,18.0449620298901,4.76379297504879));
#88824=CARTESIAN_POINT('Ctrl Pts',(-10.7417750592143,18.0447266461463,4.76159459375992));
#88825=CARTESIAN_POINT('Ctrl Pts',(-10.7477796778929,18.0443472088053,4.75804003036361));
#88826=CARTESIAN_POINT('Ctrl Pts',(-10.7500388626585,18.0442038308838,4.75669442146568));
#88827=CARTESIAN_POINT('Ctrl Pts',(-10.7547082675129,18.0439061825315,4.75389616808107));
#88828=CARTESIAN_POINT('Ctrl Pts',(-10.757117931372,18.0437518534961,4.75244265614762));
#88829=CARTESIAN_POINT('Ctrl Pts',(-10.7629272918916,18.0433780576804,4.74891555166151));
#88830=CARTESIAN_POINT('Ctrl Pts',(-10.766322736036,18.0431581454986,4.74683502171039));
#88831=CARTESIAN_POINT('Ctrl Pts',(-10.7735832420335,18.0426848905361,4.74234534665398));
#88832=CARTESIAN_POINT('Ctrl Pts',(-10.7774456252167,18.0424312879585,4.73993197048965));
#88833=CARTESIAN_POINT('Ctrl Pts',(-10.7881472967579,18.04172361975,4.73317546495951));
#88834=CARTESIAN_POINT('Ctrl Pts',(-10.7949617823173,18.0412672879427,4.72879357406561));
#88835=CARTESIAN_POINT('Ctrl Pts',(-10.8612425498917,18.036775376924,4.6853912249787));
#88836=CARTESIAN_POINT('Ctrl Pts',(-10.9178210664261,18.032522085959,4.64214438463844));
#88837=CARTESIAN_POINT('Ctrl Pts',(-11.0644954775595,18.0207259893287,4.51207153969219));
#88838=CARTESIAN_POINT('Ctrl Pts',(-11.1469853518544,18.01322510673,4.4175375367201));
#88839=CARTESIAN_POINT('Ctrl Pts',(-11.2252839631058,18.0053622405181,4.30047672833203));
#88840=CARTESIAN_POINT('Ctrl Pts',(-11.2338868586401,18.0044846565566,4.28715121212105));
#88841=CARTESIAN_POINT('Ctrl Pts',(-11.2456388705706,18.003265809474,4.26828160350215));
#88842=CARTESIAN_POINT('Ctrl Pts',(-11.2489707526794,18.0029178810214,4.26285311751713));
#88843=CARTESIAN_POINT('Ctrl Pts',(-11.2546926658241,18.0023161777078,4.25339267992669));
#88844=CARTESIAN_POINT('Ctrl Pts',(-11.257098945586,18.0020618150956,4.2493707076995));
#88845=CARTESIAN_POINT('Ctrl Pts',(-11.2620735029621,18.0015331576576,4.2409646001257));
#88846=CARTESIAN_POINT('Ctrl Pts',(-11.2646383566638,18.0012589887489,4.23657850448676));
#88847=CARTESIAN_POINT('Ctrl Pts',(-11.2706498608229,18.0006125394463,4.22617441092761));
#88848=CARTESIAN_POINT('Ctrl Pts',(-11.2740766970947,18.0002409718061,4.22014506598883));
#88849=CARTESIAN_POINT('Ctrl Pts',(-11.2853388293614,17.999009336301,4.19999788635851));
#88850=CARTESIAN_POINT('Ctrl Pts',(-11.2929834927825,17.9981560137514,4.18577449780025));
#88851=CARTESIAN_POINT('Ctrl Pts',(-11.3331476541466,17.9935715335456,4.1079862632371));
#88852=CARTESIAN_POINT('Ctrl Pts',(-11.3612191673311,17.9899970914573,4.04223045109406));
#88853=CARTESIAN_POINT('Ctrl Pts',(-11.4226428766687,17.9807015803029,3.86309204643886));
#88854=CARTESIAN_POINT('Ctrl Pts',(-11.4472680267064,17.9751526385864,3.74729994583407));
#88855=CARTESIAN_POINT('Ctrl Pts',(-11.4592437504637,17.9681213374443,3.61283172611907));
#88856=CARTESIAN_POINT('Ctrl Pts',(-11.4604598594377,17.9672202794926,3.59581372707619));
#88857=CARTESIAN_POINT('Ctrl Pts',(-11.4616550083964,17.9660274655777,3.57364332553573));
#88858=CARTESIAN_POINT('Ctrl Pts',(-11.461904785929,17.9657497546037,3.56850619131987));
#88859=CARTESIAN_POINT('Ctrl Pts',(-11.4622614894896,17.9653025539731,3.56027574860804));
#88860=CARTESIAN_POINT('Ctrl Pts',(-11.46238569214,17.9651340072504,3.55718318435738));
#88861=CARTESIAN_POINT('Ctrl Pts',(-11.4625994671436,17.9648179939412,3.55140310766918));
#88862=CARTESIAN_POINT('Ctrl Pts',(-11.4626914434299,17.9646706616208,3.54871572285166));
#88863=CARTESIAN_POINT('Ctrl Pts',(-11.4628630676688,17.9643708328295,3.54326149629697));
#88864=CARTESIAN_POINT('Ctrl Pts',(-11.4629422732561,17.9642183134261,3.5404946499136));
#88865=CARTESIAN_POINT('Ctrl Pts',(-11.4631079706877,17.9638631658427,3.53406918213765));
#88866=CARTESIAN_POINT('Ctrl Pts',(-11.4631885891396,17.9636602249721,3.53041044377951));
#88867=CARTESIAN_POINT('Ctrl Pts',(-11.4634170261843,17.9629648009995,3.51791536916427));
#88868=CARTESIAN_POINT('Ctrl Pts',(-11.4634985242079,17.9624689422961,3.50907821602269));
#88869=CARTESIAN_POINT('Ctrl Pts',(-11.463499980138,17.9619694309472,3.50024111453588));
#88870=CARTESIAN_POINT('Ctrl Pts',(-11.4634999799479,17.9619694960085,3.50024226556802));
#88871=CARTESIAN_POINT('Ctrl Pts',(-11.463499993316,17.9619649313701,3.50016151024927));
#88872=CARTESIAN_POINT('Ctrl Pts',(-11.4635,17.9619603664338,3.50008075505999));
#88873=CARTESIAN_POINT('Ctrl Pts',(-11.4635,17.9619558011997,3.500000000001));
#88874=CARTESIAN_POINT('',(-11.4634999772434,17.8879984848035,3.50025808640535));
#88875=CARTESIAN_POINT('Ctrl Pts',(-11.4635,17.8879846534521,3.50000000000001));
#88876=CARTESIAN_POINT('Ctrl Pts',(-11.4635,17.887989263516,3.50008602880244));
#88877=CARTESIAN_POINT('Ctrl Pts',(-11.4634999924145,17.8879938739664,3.50017205760456));
#88878=CARTESIAN_POINT('Ctrl Pts',(-11.4634999772434,17.8879984848035,3.50025808640535));
#88879=CARTESIAN_POINT('Ctrl Pts',(-11.4634999771172,17.887998523106,3.50025880105015));
#88880=CARTESIAN_POINT('Ctrl Pts',(-11.4634996087456,17.8881101705811,3.50234191384813));
#88881=CARTESIAN_POINT('Ctrl Pts',(-11.4634947927927,17.8882220441916,3.50442501346896));
#88882=CARTESIAN_POINT('Ctrl Pts',(-11.4634714769766,17.8885042117665,3.50966808511906));
#88883=CARTESIAN_POINT('Ctrl Pts',(-11.4634471899595,17.8886748059766,3.51282800156928));
#88884=CARTESIAN_POINT('Ctrl Pts',(-11.4633823754428,17.8889961405689,3.51876067975669));
#88885=CARTESIAN_POINT('Ctrl Pts',(-11.4633442007053,17.8891467536511,3.5215334591941));
#88886=CARTESIAN_POINT('Ctrl Pts',(-11.4632535428089,17.8894440913529,3.52699133134601));
#88887=CARTESIAN_POINT('Ctrl Pts',(-11.4632015487399,17.8895907894249,3.52967642531825));
#88888=CARTESIAN_POINT('Ctrl Pts',(-11.4630824093265,17.8898859408203,3.53506302975147));
#88889=CARTESIAN_POINT('Ctrl Pts',(-11.4630151725527,17.8900343938093,3.53776449617177));
#88890=CARTESIAN_POINT('Ctrl Pts',(-11.4628100360454,17.8904430863153,3.54518070824536));
#88891=CARTESIAN_POINT('Ctrl Pts',(-11.462656825867,17.8907041566108,3.54989495404495));
#88892=CARTESIAN_POINT('Ctrl Pts',(-11.4619714825889,17.8917253615931,3.56824932931909));
#88893=CARTESIAN_POINT('Ctrl Pts',(-11.4612713258228,17.8924940946772,3.5818820591066));
#88894=CARTESIAN_POINT('Ctrl Pts',(-11.4517366343295,17.9008109229354,3.72768223507119));
#88895=CARTESIAN_POINT('Ctrl Pts',(-11.4251887040487,17.9090236194612,3.85807459512349));
#88896=CARTESIAN_POINT('Ctrl Pts',(-11.360756277425,17.9205562276393,4.0423170640801));
#88897=CARTESIAN_POINT('Ctrl Pts',(-11.3362677186452,17.9241755032336,4.10012965474018));
#88898=CARTESIAN_POINT('Ctrl Pts',(-11.3013731368282,17.9285127985954,4.16969255369424));
#88899=CARTESIAN_POINT('Ctrl Pts',(-11.2943956174074,17.9293469927661,4.18308137683167));
#88900=CARTESIAN_POINT('Ctrl Pts',(-11.2839993316971,17.9305438111077,4.20229876397182));
#88901=CARTESIAN_POINT('Ctrl Pts',(-11.2807455757794,17.9309121963055,4.20821508734007));
#88902=CARTESIAN_POINT('Ctrl Pts',(-11.2749860500647,17.9315536606731,4.21851815616438));
#88903=CARTESIAN_POINT('Ctrl Pts',(-11.272498311363,17.931827373199,4.22291480622881));
#88904=CARTESIAN_POINT('Ctrl Pts',(-11.2676345724193,17.9323560900038,4.23140772773798));
#88905=CARTESIAN_POINT('Ctrl Pts',(-11.2652613601635,17.9326111892698,4.23550551635607));
#88906=CARTESIAN_POINT('Ctrl Pts',(-11.2595560068576,17.9332176857829,4.24524752570933));
#88907=CARTESIAN_POINT('Ctrl Pts',(-11.2562057396522,17.9335684276562,4.25088104953298));
#88908=CARTESIAN_POINT('Ctrl Pts',(-11.2440491297574,17.934822115061,4.27101347300195));
#88909=CARTESIAN_POINT('Ctrl Pts',(-11.2350285156226,17.9357173061254,4.28538182424198));
#88910=CARTESIAN_POINT('Ctrl Pts',(-11.1663487169399,17.9422875970031,4.39066689345395));
#88911=CARTESIAN_POINT('Ctrl Pts',(-11.0969726289713,17.9475663700131,4.47483874800094));
#88912=CARTESIAN_POINT('Ctrl Pts',(-10.9776803205141,17.9556474304084,4.59053730667888));
#88913=CARTESIAN_POINT('Ctrl Pts',(-10.9341394120926,17.9584430351183,4.6280573191357));
#88914=CARTESIAN_POINT('Ctrl Pts',(-10.8690077875601,17.9625812994912,4.67782003646447));
#88915=CARTESIAN_POINT('Ctrl Pts',(-10.8491353127244,17.9638388754578,4.69222635359976));
#88916=CARTESIAN_POINT('Ctrl Pts',(-10.8206982501887,17.9656453678623,4.71176975521268));
#88917=CARTESIAN_POINT('Ctrl Pts',(-10.8124282279415,17.9661715317254,4.71732983286636));
#88918=CARTESIAN_POINT('Ctrl Pts',(-10.7997008921494,17.9669835334379,4.72569918099538));
#88919=CARTESIAN_POINT('Ctrl Pts',(-10.7952839741127,17.9672657406665,4.7285696553665));
#88920=CARTESIAN_POINT('Ctrl Pts',(-10.7879834304738,17.9677330250821,4.73325827940501));
#88921=CARTESIAN_POINT('Ctrl Pts',(-10.7851087417519,17.9679172364231,4.7350903341782));
#88922=CARTESIAN_POINT('Ctrl Pts',(-10.779545419841,17.9682741969351,4.73860859857566));
#88923=CARTESIAN_POINT('Ctrl Pts',(-10.7768576476883,17.9684468591731,4.74029614080542));
#88924=CARTESIAN_POINT('Ctrl Pts',(-10.7718826276345,17.9687668745793,4.74339723693117));
#88925=CARTESIAN_POINT('Ctrl Pts',(-10.7695969615272,17.9689140653315,4.7448132374431));
#88926=CARTESIAN_POINT('Ctrl Pts',(-10.7643185742832,17.9692543570505,4.74806317412578));
#88927=CARTESIAN_POINT('Ctrl Pts',(-10.7613231646898,17.9694477427382,4.74989263858129));
#88928=CARTESIAN_POINT('Ctrl Pts',(-10.7535860170618,17.9699479056553,4.75458001608911));
#88929=CARTESIAN_POINT('Ctrl Pts',(-10.7488346345796,17.9702556792723,4.75742180271658));
#88930=CARTESIAN_POINT('Ctrl Pts',(-10.7194682177947,17.9721611784279,4.77476028702277));
#88931=CARTESIAN_POINT('Ctrl Pts',(-10.6944507460462,17.9737985017231,4.78855975656396));
#88932=CARTESIAN_POINT('Ctrl Pts',(-10.5756576750906,17.9815822313934,4.84962085526537));
#88933=CARTESIAN_POINT('Ctrl Pts',(-10.477374481719,17.9880222210261,4.88743370361108));
#88934=CARTESIAN_POINT('Ctrl Pts',(-10.3001367619972,17.9989243097765,4.93453619122959));
#88935=CARTESIAN_POINT('Ctrl Pts',(-10.2228802093233,18.003462250837,4.94855225895876));
#88936=CARTESIAN_POINT('Ctrl Pts',(-10.1335643216425,18.008431491231,4.95743670003048));
#88937=CARTESIAN_POINT('Ctrl Pts',(-10.1222532008044,18.009055997427,4.9584290616));
#88938=CARTESIAN_POINT('Ctrl Pts',(-10.1049258693375,18.010005512237,4.95974624073034));
#88939=CARTESIAN_POINT('Ctrl Pts',(-10.0989174692475,18.0103334510483,4.9601656964797));
#88940=CARTESIAN_POINT('Ctrl Pts',(-10.0884273542918,18.0109037547198,4.96083298077675));
#88941=CARTESIAN_POINT('Ctrl Pts',(-10.0839468002151,18.0111466289908,4.96109730342239));
#88942=CARTESIAN_POINT('Ctrl Pts',(-10.0738419275788,18.0116927929174,4.96164678801592));
#88943=CARTESIAN_POINT('Ctrl Pts',(-10.0682170181941,18.0119957111346,4.96192010822445));
#88944=CARTESIAN_POINT('Ctrl Pts',(-10.0530596984043,18.0128090727179,4.96256894649914));
#88945=CARTESIAN_POINT('Ctrl Pts',(-10.043524872726,18.0133176284255,4.96288374319325));
#88946=CARTESIAN_POINT('Ctrl Pts',(-9.99999183384938,18.0156261071092,4.96389500258682));
#88947=CARTESIAN_POINT('Ctrl Pts',(-9.96597749113655,18.0173921232223,4.96349966908337));
#88948=CARTESIAN_POINT('Ctrl Pts',(-9.78108619632389,18.0268394819998,4.95490035299515));
#88949=CARTESIAN_POINT('Ctrl Pts',(-9.63218764684898,18.0337900855613,4.92455732752997));
#88950=CARTESIAN_POINT('Ctrl Pts',(-9.46189257301755,18.0430388384167,4.86132622355269));
#88951=CARTESIAN_POINT('Ctrl Pts',(-9.43354805247602,18.0446288798754,4.8497779897763));
#88952=CARTESIAN_POINT('Ctrl Pts',(-9.4001524608048,18.046586626404,4.83493466739257));
#88953=CARTESIAN_POINT('Ctrl Pts',(-9.3947314374909,18.0469071304095,4.83248549759034));
#88954=CARTESIAN_POINT('Ctrl Pts',(-9.38635110371162,18.0474070286117,4.8286376462023));
#88955=CARTESIAN_POINT('Ctrl Pts',(-9.38338123727799,18.0475850532611,4.82726194244078));
#88956=CARTESIAN_POINT('Ctrl Pts',(-9.37789093821161,18.0479158161645,4.82469631755533));
#88957=CARTESIAN_POINT('Ctrl Pts',(-9.37536927608101,18.0480683863659,4.82350915254318));
#88958=CARTESIAN_POINT('Ctrl Pts',(-9.36966698942193,18.0484148714559,4.8208046654541));
#88959=CARTESIAN_POINT('Ctrl Pts',(-9.36648846052105,18.0486090453774,4.81928306186363));
#88960=CARTESIAN_POINT('Ctrl Pts',(-9.35708210139169,18.0491866873134,4.81473828244191));
#88961=CARTESIAN_POINT('Ctrl Pts',(-9.35087028261773,18.0495720846605,4.81168242414956));
#88962=CARTESIAN_POINT('Ctrl Pts',(-9.30237405746508,18.0526104411209,4.78739620787788));
#88963=CARTESIAN_POINT('Ctrl Pts',(-9.26112366012086,18.0553707932687,4.76417240627522));
#88964=CARTESIAN_POINT('Ctrl Pts',(-9.196573746687,18.0598976390821,4.72359145243149));
#88965=CARTESIAN_POINT('Ctrl Pts',(-9.17253583938214,18.0616331493684,4.70746543446746));
#88966=CARTESIAN_POINT('Ctrl Pts',(-9.10087630023947,18.0669313104379,4.65624682541889));
#88967=CARTESIAN_POINT('Ctrl Pts',(-9.05488740484713,18.0705033852549,4.61896951611743));
#88968=CARTESIAN_POINT('Ctrl Pts',(-8.96099606454717,18.0780591133946,4.53293489082242));
#88969=CARTESIAN_POINT('Ctrl Pts',(-8.91399017038175,18.0820112074612,4.48339631386365));
#88970=CARTESIAN_POINT('Ctrl Pts',(-8.86057649106344,18.0866971070263,4.4185831671818));
#88971=CARTESIAN_POINT('Ctrl Pts',(-8.85074373803303,18.0875692031448,4.40625109072412));
#88972=CARTESIAN_POINT('Ctrl Pts',(-8.83691561492532,18.0888099478358,4.38832098849814));
#88973=CARTESIAN_POINT('Ctrl Pts',(-8.83275759429778,18.089184962231,4.38285028968508));
#88974=CARTESIAN_POINT('Ctrl Pts',(-8.82559803179066,18.0898341362901,4.37329146624862));
#88975=CARTESIAN_POINT('Ctrl Pts',(-8.82257894870636,18.0901089746129,4.36921668002116));
#88976=CARTESIAN_POINT('Ctrl Pts',(-8.81680031278948,18.0906371756653,4.36133203753208));
#88977=CARTESIAN_POINT('Ctrl Pts',(-8.81403783317806,18.0908906491108,4.35752441263949));
#88978=CARTESIAN_POINT('Ctrl Pts',(-8.80754090980717,18.091489119169,4.34847802421088));
#88979=CARTESIAN_POINT('Ctrl Pts',(-8.80382253929078,18.0918335008506,4.34322780056042));
#88980=CARTESIAN_POINT('Ctrl Pts',(-8.79084497680795,18.0930422045479,4.32464529100944));
#88981=CARTESIAN_POINT('Ctrl Pts',(-8.78177289882597,18.0938994907646,4.31118338475427));
#88982=CARTESIAN_POINT('Ctrl Pts',(-8.70700508299732,18.101078930073,4.1961523900241));
#88983=CARTESIAN_POINT('Ctrl Pts',(-8.65391226871675,18.1068938705064,4.08695338616846));
#88984=CARTESIAN_POINT('Ctrl Pts',(-8.59624173516248,18.1155995993522,3.91787652720263));
#88985=CARTESIAN_POINT('Ctrl Pts',(-8.58086803654647,18.1184301359661,3.86224526518128));
#88986=CARTESIAN_POINT('Ctrl Pts',(-8.56334897873854,18.1227277589649,3.78026900655125));
#88987=CARTESIAN_POINT('Ctrl Pts',(-8.5585682162571,18.1240945177659,3.75454099360245));
#88988=CARTESIAN_POINT('Ctrl Pts',(-8.55359102390566,18.1258022523152,3.72308222037375));
#88989=CARTESIAN_POINT('Ctrl Pts',(-8.55273494057883,18.1261089173885,3.71745907388404));
#88990=CARTESIAN_POINT('Ctrl Pts',(-8.55144613864575,18.126591806441,3.70864876042961));
#88991=CARTESIAN_POINT('Ctrl Pts',(-8.55099110139725,18.1267668063105,3.7054648530403));
#88992=CARTESIAN_POINT('Ctrl Pts',(-8.55016039743586,18.1270949386858,3.69951236309469));
#88993=CARTESIAN_POINT('Ctrl Pts',(-8.5497821615139,18.1272479264566,3.69674419102849));
#88994=CARTESIAN_POINT('Ctrl Pts',(-8.5489341119503,18.1275993095779,3.69040228667864));
#88995=CARTESIAN_POINT('Ctrl Pts',(-8.54846957402789,18.1277979948724,3.6868278997851));
#88996=CARTESIAN_POINT('Ctrl Pts',(-8.54728584671542,18.1283209578516,3.67744872986739));
#88997=CARTESIAN_POINT('Ctrl Pts',(-8.54658825216556,18.1286463851502,3.67164134644519));
#88998=CARTESIAN_POINT('Ctrl Pts',(-8.5420151639162,18.130903836636,3.63154239267359));
#88999=CARTESIAN_POINT('Ctrl Pts',(-8.53931911876848,18.1328935881627,3.59712969771141));
#89000=CARTESIAN_POINT('Ctrl Pts',(-8.5358585157125,18.1376369505387,3.51637307954069));
#89001=CARTESIAN_POINT('Ctrl Pts',(-8.53607397644721,18.1404156644546,3.4700231354266));
#89002=CARTESIAN_POINT('Ctrl Pts',(-8.54492883175439,18.1506467534406,3.30026839031113));
#89003=CARTESIAN_POINT('Ctrl Pts',(-8.56699893240249,18.1580617792506,3.17806274418342));
#89004=CARTESIAN_POINT('Ctrl Pts',(-8.60893570279792,18.1658460437972,3.04500311375358));
#89005=CARTESIAN_POINT('Ctrl Pts',(-8.61393060122558,18.1667200597582,3.0300067077447));
#89006=CARTESIAN_POINT('Ctrl Pts',(-8.62144626553979,18.1679630234602,3.00860489570334));
#89007=CARTESIAN_POINT('Ctrl Pts',(-8.62377068244079,18.1683383684147,3.0021321309092));
#89008=CARTESIAN_POINT('Ctrl Pts',(-8.62788858897168,18.168987928468,2.99091429606747));
#89009=CARTESIAN_POINT('Ctrl Pts',(-8.62966126817891,18.1692628244981,2.98616175775453));
#89010=CARTESIAN_POINT('Ctrl Pts',(-8.63312498941516,18.1697910064823,2.97702096563025));
#89011=CARTESIAN_POINT('Ctrl Pts',(-8.63481254280004,18.170044403917,2.97263146437586));
#89012=CARTESIAN_POINT('Ctrl Pts',(-8.63885669885756,18.1706424949359,2.9622616997818));
#89013=CARTESIAN_POINT('Ctrl Pts',(-8.64123161098919,18.1709865754877,2.95628864957481));
#89014=CARTESIAN_POINT('Ctrl Pts',(-8.64972965805799,18.1721932012086,2.93531899424917));
#89015=CARTESIAN_POINT('Ctrl Pts',(-8.6560624617088,18.1730487427763,2.92040828574774));
#89016=CARTESIAN_POINT('Ctrl Pts',(-8.7119290733633,18.1802473442794,2.79471118872531));
#89017=CARTESIAN_POINT('Ctrl Pts',(-8.7748155740205,18.1860793198079,2.69037997932913));
#89018=CARTESIAN_POINT('Ctrl Pts',(-8.8853635842846,18.1947922348901,2.54988766795997));
#89019=CARTESIAN_POINT('Ctrl Pts',(-8.92348415812956,18.1976106183449,2.50690356087113));
#89020=CARTESIAN_POINT('Ctrl Pts',(-8.97629785877265,18.2014443852056,2.45397516166054));
#89021=CARTESIAN_POINT('Ctrl Pts',(-8.98878590472146,18.2023463288817,2.44189790488529));
#89022=CARTESIAN_POINT('Ctrl Pts',(-9.00991098520214,18.2038705105562,2.42218331420514));
#89023=CARTESIAN_POINT('Ctrl Pts',(-9.0184288233795,18.2044846692273,2.4144203971475));
#89024=CARTESIAN_POINT('Ctrl Pts',(-9.03022653676245,18.2053361998756,2.40392066489235));
#89025=CARTESIAN_POINT('Ctrl Pts',(-9.03342825634286,18.2055673800023,2.4010962088129));
#89026=CARTESIAN_POINT('Ctrl Pts',(-9.03882866374633,18.2059575527906,2.39637399998643));
#89027=CARTESIAN_POINT('Ctrl Pts',(-9.04102075045574,18.2061159932624,2.39446868689435));
#89028=CARTESIAN_POINT('Ctrl Pts',(-9.04518634891259,18.2064172303025,2.39086975300984));
#89029=CARTESIAN_POINT('Ctrl Pts',(-9.04715873032829,18.2065599282459,2.38917484378417));
#89030=CARTESIAN_POINT('Ctrl Pts',(-9.05232038334082,18.2069335066419,2.38476318818663));
#89031=CARTESIAN_POINT('Ctrl Pts',(-9.05551679758988,18.2071649911372,2.38205488429413));
#89032=CARTESIAN_POINT('Ctrl Pts',(-9.06654506946966,18.2079640092833,2.37279174644536));
#89033=CARTESIAN_POINT('Ctrl Pts',(-9.07443370609425,18.2085361572852,2.36630534187619));
#89034=CARTESIAN_POINT('Ctrl Pts',(-9.16618876500408,18.2151913918364,2.29245604532219));
#89035=CARTESIAN_POINT('Ctrl Pts',(-9.25716317435109,18.2217682499649,2.23445878972017));
#89036=CARTESIAN_POINT('Ctrl Pts',(-9.44109545425367,18.2340646247692,2.14391946224767));
#89037=CARTESIAN_POINT('Ctrl Pts',(-9.53261868003092,18.2397757914085,2.10971616412372));
#89038=CARTESIAN_POINT('Ctrl Pts',(-9.63817833650661,18.2458235153786,2.08188366322053));
#89039=CARTESIAN_POINT('Ctrl Pts',(-9.64951566279887,18.2464666887299,2.07903919781908));
#89040=CARTESIAN_POINT('Ctrl Pts',(-9.66681283178383,18.2474385203373,2.07491906186062));
#89041=CARTESIAN_POINT('Ctrl Pts',(-9.67274839694089,18.2477703253788,2.07354433676447));
#89042=CARTESIAN_POINT('Ctrl Pts',(-9.68307821917085,18.2483449020125,2.07121973557085));
#89043=CARTESIAN_POINT('Ctrl Pts',(-9.68746855863009,18.2485882077633,2.07025297413599));
#89044=CARTESIAN_POINT('Ctrl Pts',(-9.6973210561208,18.2491322325151,2.06813098519359));
#89045=CARTESIAN_POINT('Ctrl Pts',(-9.7027855272989,18.2494325994448,2.06698674917736));
#89046=CARTESIAN_POINT('Ctrl Pts',(-9.71738896165846,18.2502317418174,2.0640159802438));
#89047=CARTESIAN_POINT('Ctrl Pts',(-9.72653913288657,18.2507287439758,2.06224540913756));
#89048=CARTESIAN_POINT('Ctrl Pts',(-9.76703927070889,18.2529127676223,2.05480920380854));
#89049=CARTESIAN_POINT('Ctrl Pts',(-9.79855360886277,18.2545702847652,2.05008045577953));
#89050=CARTESIAN_POINT('Ctrl Pts',(-9.98267534778406,18.2640573038775,2.02857265150947));
#89051=CARTESIAN_POINT('Ctrl Pts',(-10.1369792643312,18.2711112119794,2.03486311084391));
#89052=CARTESIAN_POINT('Ctrl Pts',(-10.3176100446488,18.2804886518688,2.07104904688613));
#89053=CARTESIAN_POINT('Ctrl Pts',(-10.3475477689308,18.2820854523383,2.07803401845936));
#89054=CARTESIAN_POINT('Ctrl Pts',(-10.3829957838397,18.2840507620222,2.08749090220312));
#89055=CARTESIAN_POINT('Ctrl Pts',(-10.388740816691,18.2843716463479,2.08906120019572));
#89056=CARTESIAN_POINT('Ctrl Pts',(-10.3976294015769,18.2848720115687,2.09154913753787));
#89057=CARTESIAN_POINT('Ctrl Pts',(-10.4007797951124,18.2850501188187,2.09244235344751));
#89058=CARTESIAN_POINT('Ctrl Pts',(-10.4066059410909,18.285380956119,2.09411535807451));
#89059=CARTESIAN_POINT('Ctrl Pts',(-10.4092824785304,18.2855335174898,2.09489222117054));
#89060=CARTESIAN_POINT('Ctrl Pts',(-10.4153363291556,18.2858798804483,2.09666811200862));
#89061=CARTESIAN_POINT('Ctrl Pts',(-10.4187122479847,18.2860739402845,2.09767168358409));
#89062=CARTESIAN_POINT('Ctrl Pts',(-10.4289245109951,18.2866636686938,2.10074768370778));
#89063=CARTESIAN_POINT('Ctrl Pts',(-10.4357492301552,18.2870614362393,2.10285795819934));
#89064=CARTESIAN_POINT('Ctrl Pts',(-10.493262076955,18.2904428245268,2.12110391151845));
#89065=CARTESIAN_POINT('Ctrl Pts',(-10.5430466602286,18.2935617722061,2.13994076776042));
#89066=CARTESIAN_POINT('Ctrl Pts',(-10.67297216189,18.3020295654065,2.19737249957229));
#89067=CARTESIAN_POINT('Ctrl Pts',(-10.7508180731415,18.307442779777,2.24063369505736));
#89068=CARTESIAN_POINT('Ctrl Pts',(-10.8758212052372,18.316378916286,2.3258350079595));
#89069=CARTESIAN_POINT('Ctrl Pts',(-10.925088345171,18.3199792427879,2.36424504518652));
#89070=CARTESIAN_POINT('Ctrl Pts',(-10.9830163101908,18.3242965685847,2.41568551673987));
#89071=CARTESIAN_POINT('Ctrl Pts',(-10.9941203317286,18.3251285396392,2.4258567346156));
#89072=CARTESIAN_POINT('Ctrl Pts',(-11.0099683928408,18.326322774443,2.44082976484213));
#89073=CARTESIAN_POINT('Ctrl Pts',(-11.0148390511286,18.3266907646281,2.44549564058799));
#89074=CARTESIAN_POINT('Ctrl Pts',(-11.0233001570769,18.3273317716017,2.45371392742774));
#89075=CARTESIAN_POINT('Ctrl Pts',(-11.0269047682177,18.3276054190621,2.45725153798602));
#89076=CARTESIAN_POINT('Ctrl Pts',(-11.0338548678405,18.3281341750756,2.4641434440977));
#89077=CARTESIAN_POINT('Ctrl Pts',(-11.0372025199864,18.3283893776532,2.4674954598534));
#89078=CARTESIAN_POINT('Ctrl Pts',(-11.0451482068862,18.3289963794379,2.47552914429914));
#89079=CARTESIAN_POINT('Ctrl Pts',(-11.0497311690379,18.3293475207092,2.48022562142863));
#89080=CARTESIAN_POINT('Ctrl Pts',(-11.0660811265318,18.3306041327653,2.49720756410111));
#89081=CARTESIAN_POINT('Ctrl Pts',(-11.0776655487432,18.3315018008122,2.50966741212571));
#89082=CARTESIAN_POINT('Ctrl Pts',(-11.1607853913352,18.3380046036386,2.60225462224212));
#89083=CARTESIAN_POINT('Ctrl Pts',(-11.2235240166911,18.3432243978081,2.68983880930622));
#89084=CARTESIAN_POINT('Ctrl Pts',(-11.3090981423567,18.3517232941099,2.84225165472479));
#89085=CARTESIAN_POINT('Ctrl Pts',(-11.3379825296583,18.3549990369876,2.90319823702338));
#89086=CARTESIAN_POINT('Ctrl Pts',(-11.3729990341876,18.3598992749333,2.99253236341333));
#89087=CARTESIAN_POINT('Ctrl Pts',(-11.3826503272776,18.3613884403787,3.01945072323726));
#89088=CARTESIAN_POINT('Ctrl Pts',(-11.3933146265079,18.3632332878534,3.05218232439173));
#89089=CARTESIAN_POINT('Ctrl Pts',(-11.3950895412571,18.3635478584082,3.05774273482604));
#89090=CARTESIAN_POINT('Ctrl Pts',(-11.3978005079577,18.3640404674818,3.06641431686641));
#89091=CARTESIAN_POINT('Ctrl Pts',(-11.3987595621253,18.3642171996847,3.06951830281881));
#89092=CARTESIAN_POINT('Ctrl Pts',(-11.400522910386,18.3645468154811,3.07529350162224));
#89093=CARTESIAN_POINT('Ctrl Pts',(-11.401329906553,18.3646995408946,3.07796383462544));
#89094=CARTESIAN_POINT('Ctrl Pts',(-11.4031484898235,18.3650480138882,3.08404421253774));
#89095=CARTESIAN_POINT('Ctrl Pts',(-11.4041552791101,18.3652440331692,3.08745563485443));
#89096=CARTESIAN_POINT('Ctrl Pts',(-11.4067406090546,18.3657554880852,3.09633491819155));
#89097=CARTESIAN_POINT('Ctrl Pts',(-11.4082996934079,18.3660719947437,3.10180832401046));
#89098=CARTESIAN_POINT('Ctrl Pts',(-11.4182370686533,18.3681423322619,3.13748350147459));
#89099=CARTESIAN_POINT('Ctrl Pts',(-11.4256746729285,18.3699438206818,3.16793669692388));
#89100=CARTESIAN_POINT('Ctrl Pts',(-11.4528988643753,18.3776735780483,3.29729601855312));
#89101=CARTESIAN_POINT('Ctrl Pts',(-11.4634117725477,18.3838503472647,3.39787060296645));
#89102=CARTESIAN_POINT('Ctrl Pts',(-11.4634998156995,18.389874919343,3.49915186239209));
#89103=CARTESIAN_POINT('Ctrl Pts',(-11.4635,18.3899001415702,3.49957593289561));
#89104=CARTESIAN_POINT('Ctrl Pts',(-11.4635,18.3899253605917,3.49999999994518));
#89105=CARTESIAN_POINT('Origin',(-10.,13.2,3.5));
#89106=CARTESIAN_POINT('',(-11.4635,18.9594567372512,3.50000000000276));
#89107=CARTESIAN_POINT('',(-11.4635,18.8903920399481,3.49999999999848));
#89108=CARTESIAN_POINT('',(-11.4635,13.2,3.5));
#89109=CARTESIAN_POINT('Ctrl Pts',(-11.4635,18.9594567372512,3.50000000000276));
#89110=CARTESIAN_POINT('Ctrl Pts',(-11.4635000000001,18.9578291943808,3.47145831790744));
#89111=CARTESIAN_POINT('Ctrl Pts',(-11.462665060547,18.9562256754957,3.44292102721574));
#89112=CARTESIAN_POINT('Ctrl Pts',(-11.4605522721912,18.954228287802,3.4068502485034));
#89113=CARTESIAN_POINT('Ctrl Pts',(-11.4600497231483,18.9538106957395,3.39927947085835));
#89114=CARTESIAN_POINT('Ctrl Pts',(-11.4590919408327,18.9531013841429,3.38637053391844));
#89115=CARTESIAN_POINT('Ctrl Pts',(-11.4586662336761,18.9528087540919,3.38103039393257));
#89116=CARTESIAN_POINT('Ctrl Pts',(-11.4578155799634,18.9522633951236,3.37105163649082));
#89117=CARTESIAN_POINT('Ctrl Pts',(-11.4573977917925,18.9520104467364,3.36641249005495));
#89118=CARTESIAN_POINT('Ctrl Pts',(-11.4564834460767,18.951486156403,3.35677482078956));
#89119=CARTESIAN_POINT('Ctrl Pts',(-11.4559832875043,18.9512149303026,3.35177669537899));
#89120=CARTESIAN_POINT('Ctrl Pts',(-11.4547809158592,18.9505966298355,3.34035511580458));
#89121=CARTESIAN_POINT('Ctrl Pts',(-11.4540618714463,18.9502500851136,3.33393351322411));
#89122=CARTESIAN_POINT('Ctrl Pts',(-11.4516608367582,18.9491616239936,3.31370299390724));
#89123=CARTESIAN_POINT('Ctrl Pts',(-11.4498244554434,18.9484245248361,3.29991295529326));
#89124=CARTESIAN_POINT('Ctrl Pts',(-11.442968009881,18.9459579681926,3.25349375770704));
#89125=CARTESIAN_POINT('Ctrl Pts',(-11.4370405709005,18.944256503438,3.22100787230089));
#89126=CARTESIAN_POINT('Ctrl Pts',(-11.4085163732689,18.93745415692,3.08995576641959));
#89127=CARTESIAN_POINT('Ctrl Pts',(-11.3768348745937,18.9326202645166,2.99365926308));
#89128=CARTESIAN_POINT('Ctrl Pts',(-11.3147856679703,18.9252004746787,2.85522834193555));
#89129=CARTESIAN_POINT('Ctrl Pts',(-11.2917134742703,18.922698433926,2.81016852005433));
#89130=CARTESIAN_POINT('Ctrl Pts',(-11.2542362093617,18.9188526869045,2.74547470155571));
#89131=CARTESIAN_POINT('Ctrl Pts',(-11.2415999240966,18.9175865732557,2.72485718204888));
#89132=CARTESIAN_POINT('Ctrl Pts',(-11.2254419267573,18.9159918217724,2.69990303174952));
#89133=CARTESIAN_POINT('Ctrl Pts',(-11.2223978880725,18.9156923816115,2.69525999496594));
#89134=CARTESIAN_POINT('Ctrl Pts',(-11.2175657435833,18.9152184194566,2.68798025957375));
#89135=CARTESIAN_POINT('Ctrl Pts',(-11.2157952889568,18.9150450487089,2.68533183826622));
#89136=CARTESIAN_POINT('Ctrl Pts',(-11.2124536734647,18.9147183135099,2.68036827284475));
#89137=CARTESIAN_POINT('Ctrl Pts',(-11.2108845131558,18.9145650812808,2.6780518423833));
#89138=CARTESIAN_POINT('Ctrl Pts',(-11.2072871023027,18.9142142442614,2.67277392036233));
#89139=CARTESIAN_POINT('Ctrl Pts',(-11.2052545944049,18.9140163566227,2.66981538419494));
#89140=CARTESIAN_POINT('Ctrl Pts',(-11.1998352403013,18.9134896637938,2.66198877384909));
#89141=CARTESIAN_POINT('Ctrl Pts',(-11.1964296888148,18.9131596522619,2.65713380877139));
#89142=CARTESIAN_POINT('Ctrl Pts',(-11.1720354369948,18.9108033320287,2.62280302316445));
#89143=CARTESIAN_POINT('Ctrl Pts',(-11.1499909314023,18.9087136076269,2.59409600858215));
#89144=CARTESIAN_POINT('Ctrl Pts',(-11.120690503431,18.9060139185949,2.55873490049831));
#89145=CARTESIAN_POINT('Ctrl Pts',(-11.1143989322536,18.9054384570796,2.55129445753025));
#89146=CARTESIAN_POINT('Ctrl Pts',(-11.022462339847,18.8970959369846,2.44474629186931));
#89147=CARTESIAN_POINT('Ctrl Pts',(-10.9239448553004,18.8890514035154,2.35749200973739));
#89148=CARTESIAN_POINT('Ctrl Pts',(-10.7944785686214,18.8800991801085,2.27066919219183));
#89149=CARTESIAN_POINT('Ctrl Pts',(-10.7734785295382,18.8786887966517,2.25734900371317));
#89150=CARTESIAN_POINT('Ctrl Pts',(-10.7418555516207,18.8766259650343,2.23840317068915));
#89151=CARTESIAN_POINT('Ctrl Pts',(-10.7314870722249,18.8759590209082,2.23236326402638));
#89152=CARTESIAN_POINT('Ctrl Pts',(-10.7147980827225,18.8749003001296,2.22291445535111));
#89153=CARTESIAN_POINT('Ctrl Pts',(-10.7085248848645,18.8745056258549,2.2194234589353));
#89154=CARTESIAN_POINT('Ctrl Pts',(-10.6965336402723,18.8737573740352,2.21286549456926));
#89155=CARTESIAN_POINT('Ctrl Pts',(-10.6908204040481,18.8734035051903,2.20979012623903));
#89156=CARTESIAN_POINT('Ctrl Pts',(-10.680720760227,18.8727825230568,2.2044399246955));
#89157=CARTESIAN_POINT('Ctrl Pts',(-10.6763429596706,18.8725148518274,2.20214913650963));
#89158=CARTESIAN_POINT('Ctrl Pts',(-10.6677353349726,18.8719914605706,2.19770037266136));
#89159=CARTESIAN_POINT('Ctrl Pts',(-10.6635064465607,18.8717356845554,2.19554072771858));
#89160=CARTESIAN_POINT('Ctrl Pts',(-10.6521947357998,18.8710551061784,2.18983320573347));
#89161=CARTESIAN_POINT('Ctrl Pts',(-10.6450934360713,18.8706315847703,2.1863221611519));
#89162=CARTESIAN_POINT('Ctrl Pts',(-10.6191738998113,18.8690989621495,2.17376780874764));
#89163=CARTESIAN_POINT('Ctrl Pts',(-10.6001907456747,18.8680016867728,2.16506956369669));
#89164=CARTESIAN_POINT('Ctrl Pts',(-10.4663302910516,18.8604247647738,2.10716647191824));
#89165=CARTESIAN_POINT('Ctrl Pts',(-10.3457566208648,18.8544723974564,2.07244867197357));
#89166=CARTESIAN_POINT('Ctrl Pts',(-10.1730514120716,18.8459214830301,2.04591561735527));
#89167=CARTESIAN_POINT('Ctrl Pts',(-10.1235194088822,18.8434583642121,2.04087338114476));
#89168=CARTESIAN_POINT('Ctrl Pts',(-10.0499282429259,18.8396665857575,2.03715612671095));
#89169=CARTESIAN_POINT('Ctrl Pts',(-10.0260012858663,18.8384130043831,2.0365353339157));
#89170=CARTESIAN_POINT('Ctrl Pts',(-9.99653694512305,18.8368323285651,2.03649363297941));
#89171=CARTESIAN_POINT('Ctrl Pts',(-9.99100268723458,18.8365338248773,2.03651719331993));
#89172=CARTESIAN_POINT('Ctrl Pts',(-9.98228711176768,18.8360610154672,2.03660373526586));
#89173=CARTESIAN_POINT('Ctrl Pts',(-9.97910558038905,18.835887851657,2.03664570356983));
#89174=CARTESIAN_POINT('Ctrl Pts',(-9.97312594475074,18.8355612810369,2.0367440867218));
#89175=CARTESIAN_POINT('Ctrl Pts',(-9.9703278518384,18.8354080047915,2.03679815276146));
#89176=CARTESIAN_POINT('Ctrl Pts',(-9.96393511218208,18.8350567752785,2.03694002069192));
#89177=CARTESIAN_POINT('Ctrl Pts',(-9.96034062508318,18.8348585368182,2.03703304459769));
#89178=CARTESIAN_POINT('Ctrl Pts',(-9.95079753599882,18.8343303025055,2.03731521190371));
#89179=CARTESIAN_POINT('Ctrl Pts',(-9.94484974566822,18.8339990893216,2.0375273955443));
#89180=CARTESIAN_POINT('Ctrl Pts',(-9.90222655173997,18.8316120934399,2.03930833121028));
#89181=CARTESIAN_POINT('Ctrl Pts',(-9.86562304320559,18.8294910562788,2.04222011333611));
#89182=CARTESIAN_POINT('Ctrl Pts',(-9.818036327895,18.8266727987988,2.04781297247808));
#89183=CARTESIAN_POINT('Ctrl Pts',(-9.80691735349685,18.8260099083856,2.04924949616924));
#89184=CARTESIAN_POINT('Ctrl Pts',(-9.70949540439554,18.8201688953874,2.06297580970964));
#89185=CARTESIAN_POINT('Ctrl Pts',(-9.6244334270762,18.8148552283334,2.08282606282197));
#89186=CARTESIAN_POINT('Ctrl Pts',(-9.46932776818362,18.8051593116639,2.13397758086038));
#89187=CARTESIAN_POINT('Ctrl Pts',(-9.39897788043555,18.8007572881146,2.16343518342935));
#89188=CARTESIAN_POINT('Ctrl Pts',(-9.32118529193298,18.7959158614292,2.20340044214389));
#89189=CARTESIAN_POINT('Ctrl Pts',(-9.31119868307332,18.7952946633065,2.20867797309247));
#89190=CARTESIAN_POINT('Ctrl Pts',(-9.29599386014975,18.794349177264,2.21693970685566));
#89191=CARTESIAN_POINT('Ctrl Pts',(-9.29073141822298,18.7940219963281,2.21984124375142));
#89192=CARTESIAN_POINT('Ctrl Pts',(-9.28119126483665,18.7934289127674,2.2251782555804));
#89193=CARTESIAN_POINT('Ctrl Pts',(-9.27690770363486,18.7931626364467,2.22760304560641));
#89194=CARTESIAN_POINT('Ctrl Pts',(-9.26760659221794,18.7925844665923,2.2329302526694));
#89195=CARTESIAN_POINT('Ctrl Pts',(-9.26259387481363,18.792272875214,2.2358409687759));
#89196=CARTESIAN_POINT('Ctrl Pts',(-9.24895831080855,18.791425221753,2.24386738297079));
#89197=CARTESIAN_POINT('Ctrl Pts',(-9.24037044228102,18.7908912887596,2.2490420821605));
#89198=CARTESIAN_POINT('Ctrl Pts',(-9.19699109352886,18.7881929986118,2.27579215671435));
#89199=CARTESIAN_POINT('Ctrl Pts',(-9.16306112427864,18.7860790096998,2.29873322758832));
#89200=CARTESIAN_POINT('Ctrl Pts',(-9.1193267985195,18.7833255144796,2.33105705393178));
#89201=CARTESIAN_POINT('Ctrl Pts',(-9.10862843243184,18.7826494810306,2.33919440098863));
#89202=CARTESIAN_POINT('Ctrl Pts',(-8.99486002225649,18.7754244934497,2.42822885269533));
#89203=CARTESIAN_POINT('Ctrl Pts',(-8.90300049832303,18.7693290904473,2.52245937698914));
#89204=CARTESIAN_POINT('Ctrl Pts',(-8.8075067865231,18.7611551842407,2.65109188041892));
#89205=CARTESIAN_POINT('Ctrl Pts',(-8.79080652531311,18.7596352954806,2.67505395789347));
#89206=CARTESIAN_POINT('Ctrl Pts',(-8.77162427778422,18.7577561293549,2.70441229399017));
#89207=CARTESIAN_POINT('Ctrl Pts',(-8.76844289227744,18.7574397730328,2.7093459663302));
#89208=CARTESIAN_POINT('Ctrl Pts',(-8.76354360579448,18.7569450064434,2.71704506321135));
#89209=CARTESIAN_POINT('Ctrl Pts',(-8.7618050676932,18.7567679216277,2.71979736157814));
#89210=CARTESIAN_POINT('Ctrl Pts',(-8.75859477684193,18.7564380567307,2.72491736311356));
#89211=CARTESIAN_POINT('Ctrl Pts',(-8.75712059851864,18.756285437895,2.72728348337096));
#89212=CARTESIAN_POINT('Ctrl Pts',(-8.75378728448964,18.7559377431985,2.73266781406443));
#89213=CARTESIAN_POINT('Ctrl Pts',(-8.75193235644096,18.7557423999877,2.73568856319722));
#89214=CARTESIAN_POINT('Ctrl Pts',(-8.74631078210339,18.755144766432,2.7449183258558));
#89215=CARTESIAN_POINT('Ctrl Pts',(-8.74257941991845,18.7547402948701,2.75114856610679));
#89216=CARTESIAN_POINT('Ctrl Pts',(-8.70231213597262,18.7502914778474,2.81953223133805));
#89217=CARTESIAN_POINT('Ctrl Pts',(-8.67037403145688,18.7460006796192,2.88427051163823));
#89218=CARTESIAN_POINT('Ctrl Pts',(-8.60708928850038,18.7358603453108,3.04068227358088));
#89219=CARTESIAN_POINT('Ctrl Pts',(-8.57979994851503,18.7300149683673,3.13365528258996));
#89220=CARTESIAN_POINT('Ctrl Pts',(-8.55373819961013,18.7218892903862,3.2717772272273));
#89221=CARTESIAN_POINT('Ctrl Pts',(-8.54754378370078,18.7194051674711,3.31525601120711));
#89222=CARTESIAN_POINT('Ctrl Pts',(-8.54235836658396,18.7164350912081,3.36880853377542));
#89223=CARTESIAN_POINT('Ctrl Pts',(-8.54150394302759,18.7158915010358,3.37867567906812));
#89224=CARTESIAN_POINT('Ctrl Pts',(-8.54031488289668,18.7150394081234,3.39424454859444));
#89225=CARTESIAN_POINT('Ctrl Pts',(-8.53991335812582,18.7147288339642,3.39994073703175));
#89226=CARTESIAN_POINT('Ctrl Pts',(-8.53922436195622,18.7141495768639,3.41060456816035));
#89227=CARTESIAN_POINT('Ctrl Pts',(-8.53892886784122,18.7138806484491,3.41557159509564));
#89228=CARTESIAN_POINT('Ctrl Pts',(-8.53832538304471,18.7132816639919,3.42667023703583));
#89229=CARTESIAN_POINT('Ctrl Pts',(-8.53803063053482,18.7129520235042,3.43280249778797));
#89230=CARTESIAN_POINT('Ctrl Pts',(-8.53738267060471,18.7121211849862,3.4483185343291));
#89231=CARTESIAN_POINT('Ctrl Pts',(-8.53708117020793,18.7116215922586,3.4577042665429));
#89232=CARTESIAN_POINT('Ctrl Pts',(-8.53586225876163,18.708753215202,3.51189922046019));
#89233=CARTESIAN_POINT('Ctrl Pts',(-8.53691318857981,18.7064460014785,3.55673096663508));
#89234=CARTESIAN_POINT('Ctrl Pts',(-8.54968398214165,18.6971569430534,3.74052264773319));
#89235=CARTESIAN_POINT('Ctrl Pts',(-8.57916718813452,18.6907032628381,3.87748462954363));
#89236=CARTESIAN_POINT('Ctrl Pts',(-8.63793376626102,18.6820770777782,4.03618919786933));
#89237=CARTESIAN_POINT('Ctrl Pts',(-8.64915245984553,18.6805246905454,4.06385633100031));
#89238=CARTESIAN_POINT('Ctrl Pts',(-8.66359422740778,18.6786091533332,4.0965624434258));
#89239=CARTESIAN_POINT('Ctrl Pts',(-8.66601275945561,18.6782908813501,4.10195114220656));
#89240=CARTESIAN_POINT('Ctrl Pts',(-8.66981799446867,18.6777937613714,4.1102939709825));
#89241=CARTESIAN_POINT('Ctrl Pts',(-8.67118209836014,18.6776162592269,4.11325841430237));
#89242=CARTESIAN_POINT('Ctrl Pts',(-8.67372959951746,18.6772860240727,4.11874618579013));
#89243=CARTESIAN_POINT('Ctrl Pts',(-8.67491029629567,18.6771334554957,4.12127070941791));
#89244=CARTESIAN_POINT('Ctrl Pts',(-8.67760458946536,18.676786403326,4.12698893032943));
#89245=CARTESIAN_POINT('Ctrl Pts',(-8.67912254085213,18.6765916564754,4.13018051218103));
#89246=CARTESIAN_POINT('Ctrl Pts',(-8.68377172557635,18.675997611975,4.13986509793267));
#89247=CARTESIAN_POINT('Ctrl Pts',(-8.68693933659286,18.6755961703262,4.14634039314462));
#89248=CARTESIAN_POINT('Ctrl Pts',(-8.71653709972075,18.6718768605277,4.2057291433559));
#89249=CARTESIAN_POINT('Ctrl Pts',(-8.74610203361513,18.6683920460409,4.25701328215571));
#89250=CARTESIAN_POINT('Ctrl Pts',(-8.82481791271013,18.6598477659351,4.37623623054966));
#89251=CARTESIAN_POINT('Ctrl Pts',(-8.8768657948442,18.6547586832,4.44202636772783));
#89252=CARTESIAN_POINT('Ctrl Pts',(-8.97649241125211,18.6461771310912,4.54788486957857));
#89253=CARTESIAN_POINT('Ctrl Pts',(-9.02152644143322,18.6426234263662,4.59005572209119));
#89254=CARTESIAN_POINT('Ctrl Pts',(-9.08063182070296,18.638355406718,4.63877922239412));
#89255=CARTESIAN_POINT('Ctrl Pts',(-9.0923185113176,18.6375290491734,4.64811598060108));
#89256=CARTESIAN_POINT('Ctrl Pts',(-9.10946471013047,18.6363414165798,4.66138898644044));
#89257=CARTESIAN_POINT('Ctrl Pts',(-9.11481119916441,18.6359745013952,4.66546911984733));
#89258=CARTESIAN_POINT('Ctrl Pts',(-9.12421805958479,18.6353348120661,4.67254582218144));
#89259=CARTESIAN_POINT('Ctrl Pts',(-9.12826612854073,18.6350614141095,4.67555849301908));
#89260=CARTESIAN_POINT('Ctrl Pts',(-9.13614722561148,18.6345327425181,4.68136070121678));
#89261=CARTESIAN_POINT('Ctrl Pts',(-9.13997838087901,18.6342773772397,4.68415266649632));
#89262=CARTESIAN_POINT('Ctrl Pts',(-9.14915793260964,18.6336693615064,4.69077424233487));
#89263=CARTESIAN_POINT('Ctrl Pts',(-9.15451874174152,18.6333173747335,4.69458652415774));
#89264=CARTESIAN_POINT('Ctrl Pts',(-9.1739254525707,18.6320540589711,4.70819131998691));
#89265=CARTESIAN_POINT('Ctrl Pts',(-9.18811754223349,18.6311506458519,4.71777351370964));
#89266=CARTESIAN_POINT('Ctrl Pts',(-9.28875326198152,18.6248789732538,4.7831791049219));
#89267=CARTESIAN_POINT('Ctrl Pts',(-9.38070554854212,18.6198602707876,4.82999908465359));
#89268=CARTESIAN_POINT('Ctrl Pts',(-9.50545663544112,18.6133661425768,4.87775161444595));
#89269=CARTESIAN_POINT('Ctrl Pts',(-9.53443329508618,18.6118760658344,4.88781131737711));
#89270=CARTESIAN_POINT('Ctrl Pts',(-9.60869360125336,18.608061574664,4.9110042635383));
#89271=CARTESIAN_POINT('Ctrl Pts',(-9.65433276132393,18.6057213963754,4.92287290912014));
#89272=CARTESIAN_POINT('Ctrl Pts',(-9.72310857799154,18.6021007305993,4.93725387481766));
#89273=CARTESIAN_POINT('Ctrl Pts',(-9.74586342164085,18.6008876361038,4.94145136592426));
#89274=CARTESIAN_POINT('Ctrl Pts',(-9.77411408771597,18.5993524618504,4.94597295672184));
#89275=CARTESIAN_POINT('Ctrl Pts',(-9.77952602960481,18.5990570571561,4.94680802576002));
#89276=CARTESIAN_POINT('Ctrl Pts',(-9.7880769981455,18.5985880630172,4.94807835891727));
#89277=CARTESIAN_POINT('Ctrl Pts',(-9.79121302620802,18.5984155848264,4.94853384201511));
#89278=CARTESIAN_POINT('Ctrl Pts',(-9.79712395640153,18.5980895511239,4.94937276366743));
#89279=CARTESIAN_POINT('Ctrl Pts',(-9.79989849359706,18.597936120649,4.94975842256653));
#89280=CARTESIAN_POINT('Ctrl Pts',(-9.80625804520421,18.5975835536242,4.95062379251562));
#89281=CARTESIAN_POINT('Ctrl Pts',(-9.8098437415754,18.5973841239265,4.95109818043584));
#89282=CARTESIAN_POINT('Ctrl Pts',(-9.81940602022508,18.5968506442323,4.95232721989833));
#89283=CARTESIAN_POINT('Ctrl Pts',(-9.82538550133075,18.5965153391574,4.9530582622521));
#89284=CARTESIAN_POINT('Ctrl Pts',(-9.86960229252743,18.5940240749958,4.95818727339153));
#89285=CARTESIAN_POINT('Ctrl Pts',(-9.90799242254303,18.5917964330933,4.96111183710114));
#89286=CARTESIAN_POINT('Ctrl Pts',(-10.0381681247916,18.5841209538749,4.96587823235985));
#89287=CARTESIAN_POINT('Ctrl Pts',(-10.1299984413347,18.5785163252143,4.96060145746879));
#89288=CARTESIAN_POINT('Ctrl Pts',(-10.3004774010799,18.5682509548979,4.93459163435388));
#89289=CARTESIAN_POINT('Ctrl Pts',(-10.3790904158726,18.5635738346236,4.91585084707607));
#89290=CARTESIAN_POINT('Ctrl Pts',(-10.4666057508596,18.5584746346053,4.88717028308612));
#89291=CARTESIAN_POINT('Ctrl Pts',(-10.4774017884599,18.5578472853668,4.88349190953207));
#89292=CARTESIAN_POINT('Ctrl Pts',(-10.493840810038,18.5568944361162,4.87767553992463));
#89293=CARTESIAN_POINT('Ctrl Pts',(-10.4995152382987,18.5565659728823,4.87562828089422));
#89294=CARTESIAN_POINT('Ctrl Pts',(-10.5093889127066,18.5559951648206,4.87199683907327));
#89295=CARTESIAN_POINT('Ctrl Pts',(-10.5135938029111,18.5557523068487,4.87042832612619));
#89296=CARTESIAN_POINT('Ctrl Pts',(-10.5230490322838,18.5552067048538,4.86685169544319));
#89297=CARTESIAN_POINT('Ctrl Pts',(-10.5282951676456,18.5549043287108,4.86483261411838));
#89298=CARTESIAN_POINT('Ctrl Pts',(-10.5423744106431,18.5540936903237,4.85932059137314));
#89299=CARTESIAN_POINT('Ctrl Pts',(-10.5511854447853,18.5535872945577,4.85577176641991));
#89300=CARTESIAN_POINT('Ctrl Pts',(-10.5910026463331,18.5513023723958,4.83928224505634));
#89301=CARTESIAN_POINT('Ctrl Pts',(-10.6215933144883,18.5495568946276,4.82536147420745));
#89302=CARTESIAN_POINT('Ctrl Pts',(-10.6661529404654,18.5470154986339,4.8032013678181));
#89303=CARTESIAN_POINT('Ctrl Pts',(-10.6805065703623,18.5461969780945,4.79576401164056));
#89304=CARTESIAN_POINT('Ctrl Pts',(-10.814775093416,18.5385283747616,4.72334598477918));
#89305=CARTESIAN_POINT('Ctrl Pts',(-10.9251604654451,18.5322037135823,4.64214936086016));
#89306=CARTESIAN_POINT('Ctrl Pts',(-11.0438952489654,18.5237400798321,4.52615435144233));
#89307=CARTESIAN_POINT('Ctrl Pts',(-11.0644532018346,18.5221988623762,4.50481301125365));
#89308=CARTESIAN_POINT('Ctrl Pts',(-11.0883064659294,18.5202958253574,4.47849682116792));
#89309=CARTESIAN_POINT('Ctrl Pts',(-11.0922385022404,18.5199782060204,4.47410576667655));
#89310=CARTESIAN_POINT('Ctrl Pts',(-11.0983042536294,18.5194818877506,4.46724901029832));
#89311=CARTESIAN_POINT('Ctrl Pts',(-11.1004564798394,18.5193045277037,4.46479967714465));
#89312=CARTESIAN_POINT('Ctrl Pts',(-11.1044333140265,18.5189744189999,4.46024323688067));
#89313=CARTESIAN_POINT('Ctrl Pts',(-11.1062600974178,18.5188218336919,4.45813809838841));
#89314=CARTESIAN_POINT('Ctrl Pts',(-11.1103919138853,18.51847456447,4.45334912995422));
#89315=CARTESIAN_POINT('Ctrl Pts',(-11.1126932255873,18.5182796159138,4.45066216459677));
#89316=CARTESIAN_POINT('Ctrl Pts',(-11.1196657734697,18.5176843588288,4.44246115626137));
#89317=CARTESIAN_POINT('Ctrl Pts',(-11.1243058575673,18.5172818937623,4.43692091960949));
#89318=CARTESIAN_POINT('Ctrl Pts',(-11.1676255132608,18.513466196205,4.38441226581151));
#89319=CARTESIAN_POINT('Ctrl Pts',(-11.2033780175825,18.5098764432556,4.3351133024829));
#89320=CARTESIAN_POINT('Ctrl Pts',(-11.2753617041683,18.5018308010741,4.22159508366675));
#89321=CARTESIAN_POINT('Ctrl Pts',(-11.3100266684528,18.4973654266722,4.15656508946262));
#89322=CARTESIAN_POINT('Ctrl Pts',(-11.3600685296333,18.4899878363907,4.04278647233013));
#89323=CARTESIAN_POINT('Ctrl Pts',(-11.3780586971039,18.4870275331359,3.99533680351693));
#89324=CARTESIAN_POINT('Ctrl Pts',(-11.4026314683836,18.4824508258297,3.91873740137572));
#89325=CARTESIAN_POINT('Ctrl Pts',(-11.4108482702535,18.4807858785617,3.89015815636262));
#89326=CARTESIAN_POINT('Ctrl Pts',(-11.4203467654776,18.4786676477986,3.85287912080897));
#89327=CARTESIAN_POINT('Ctrl Pts',(-11.4224284561605,18.478188933693,3.84439207287755));
#89328=CARTESIAN_POINT('Ctrl Pts',(-11.4256856256605,18.4774154160204,3.83057901533335));
#89329=CARTESIAN_POINT('Ctrl Pts',(-11.4269075458637,18.4771191377824,3.8252642698995));
#89330=CARTESIAN_POINT('Ctrl Pts',(-11.4291981885138,18.476551693937,3.81503973443032));
#89331=CARTESIAN_POINT('Ctrl Pts',(-11.4302713862357,18.4762803895147,3.81013103505893));
#89332=CARTESIAN_POINT('Ctrl Pts',(-11.432669081689,18.4756614494362,3.79888700442992));
#89333=CARTESIAN_POINT('Ctrl Pts',(-11.4339768810146,18.4753143472781,3.7925481936284));
#89334=CARTESIAN_POINT('Ctrl Pts',(-11.4373392798564,18.4743957516364,3.77568640533997));
#89335=CARTESIAN_POINT('Ctrl Pts',(-11.4393203886253,18.4738265766896,3.76514906469495));
#89336=CARTESIAN_POINT('Ctrl Pts',(-11.456032501873,18.4687580889258,3.67054523624139));
#89337=CARTESIAN_POINT('Ctrl Pts',(-11.4634999999972,18.4645009776468,3.58535927216356));
#89338=CARTESIAN_POINT('Ctrl Pts',(-11.4635,18.4603263886907,3.50000000004768));
#89339=CARTESIAN_POINT('Ctrl Pts',(-11.4635,18.3899253605917,3.49999999994518));
#89340=CARTESIAN_POINT('Ctrl Pts',(-11.4635000000029,18.3945771388639,3.57822134916453));
#89341=CARTESIAN_POINT('Ctrl Pts',(-11.4572289891273,18.3991090574555,3.65632582354247));
#89342=CARTESIAN_POINT('Ctrl Pts',(-11.4430408401938,18.4040355085825,3.74408811969543));
#89343=CARTESIAN_POINT('Ctrl Pts',(-11.441224692596,18.4046226067156,3.75459236153278));
#89344=CARTESIAN_POINT('Ctrl Pts',(-11.4381247168033,18.4055594387835,3.77142442432346));
#89345=CARTESIAN_POINT('Ctrl Pts',(-11.4369135242059,18.4059114447033,3.77776508964052));
#89346=CARTESIAN_POINT('Ctrl Pts',(-11.4346852373581,18.4065350251148,3.78902552666228));
#89347=CARTESIAN_POINT('Ctrl Pts',(-11.4336846945519,18.406807117627,3.79394843567765));
#89348=CARTESIAN_POINT('Ctrl Pts',(-11.4315429299953,18.4073735045454,3.80421529925514));
#89349=CARTESIAN_POINT('Ctrl Pts',(-11.4303970847225,18.4076676477889,3.80955821722363));
#89350=CARTESIAN_POINT('Ctrl Pts',(-11.4273315913403,18.4084321024381,3.82347165981112));
#89351=CARTESIAN_POINT('Ctrl Pts',(-11.4253646544717,18.4089009072752,3.83203161393671));
#89352=CARTESIAN_POINT('Ctrl Pts',(-11.4163051351005,18.4109682836516,3.86989305352903));
#89353=CARTESIAN_POINT('Ctrl Pts',(-11.4083849675585,18.4125403953376,3.89899004593538));
#89354=CARTESIAN_POINT('Ctrl Pts',(-11.3844419289713,18.4167442984087,3.97731679489139));
#89355=CARTESIAN_POINT('Ctrl Pts',(-11.3666971787622,18.4193239430853,4.02597542888947));
#89356=CARTESIAN_POINT('Ctrl Pts',(-11.305566318069,18.4269863086776,4.16946930926579));
#89357=CARTESIAN_POINT('Ctrl Pts',(-11.2546020226093,18.4319185081065,4.26069904141007));
#89358=CARTESIAN_POINT('Ctrl Pts',(-11.1768742706503,18.4387644485129,4.370469811124));
#89359=CARTESIAN_POINT('Ctrl Pts',(-11.1585976051872,18.4403382749099,4.39465193214756));
#89360=CARTESIAN_POINT('Ctrl Pts',(-11.1360490403333,18.4422614959794,4.4226356729963));
#89361=CARTESIAN_POINT('Ctrl Pts',(-11.1324879819438,18.4425647110403,4.42700322320252));
#89362=CARTESIAN_POINT('Ctrl Pts',(-11.1266490361908,18.4430612477817,4.43408068757959));
#89363=CARTESIAN_POINT('Ctrl Pts',(-11.1243863505771,18.4432535110348,4.43680313607298));
#89364=CARTESIAN_POINT('Ctrl Pts',(-11.1203238155486,18.4435984923092,4.44165523050985));
#89365=CARTESIAN_POINT('Ctrl Pts',(-11.1185277360159,18.4437509386556,4.44378796794327));
#89366=CARTESIAN_POINT('Ctrl Pts',(-11.1146178009627,18.4440826588219,4.44840394467078));
#89367=CARTESIAN_POINT('Ctrl Pts',(-11.1125017663161,18.4442620878345,4.45088522125727));
#89368=CARTESIAN_POINT('Ctrl Pts',(-11.1065384325569,18.4447674274733,4.45783071488683));
#89369=CARTESIAN_POINT('Ctrl Pts',(-11.1026724804649,18.4450946607164,4.46227874314975));
#89370=CARTESIAN_POINT('Ctrl Pts',(-11.0792379011744,18.447075400211,4.48891509090154));
#89371=CARTESIAN_POINT('Ctrl Pts',(-11.0590282504532,18.4487714992823,4.51052779486213));
#89372=CARTESIAN_POINT('Ctrl Pts',(-10.9424796200404,18.4584142138015,4.62782976782654));
#89373=CARTESIAN_POINT('Ctrl Pts',(-10.8338396162752,18.4668191002877,4.71036626633017));
#89374=CARTESIAN_POINT('Ctrl Pts',(-10.6732575175743,18.4775151120482,4.80034081350232));
#89375=CARTESIAN_POINT('Ctrl Pts',(-10.6300057613722,18.4802576589133,4.82183789131803));
#89376=CARTESIAN_POINT('Ctrl Pts',(-10.5769585323694,18.4834581943366,4.84500687276494));
#89377=CARTESIAN_POINT('Ctrl Pts',(-10.5681124353432,18.4839866977325,4.84876717889631));
#89378=CARTESIAN_POINT('Ctrl Pts',(-10.5534924103709,18.4848517409329,4.8548125137176));
#89379=CARTESIAN_POINT('Ctrl Pts',(-10.5477399386922,18.4851899806868,4.85714839162369));
#89380=CARTESIAN_POINT('Ctrl Pts',(-10.5373443873484,18.485797458194,4.86129279932157));
#89381=CARTESIAN_POINT('Ctrl Pts',(-10.5327066289094,18.4860671278402,4.8631143475392));
#89382=CARTESIAN_POINT('Ctrl Pts',(-10.5227766826792,18.4866416893098,4.86695606252127));
#89383=CARTESIAN_POINT('Ctrl Pts',(-10.5174818756021,18.4869463460354,4.86896926425603));
#89384=CARTESIAN_POINT('Ctrl Pts',(-10.5030983226591,18.4877694109149,4.87434283278086));
#89385=CARTESIAN_POINT('Ctrl Pts',(-10.4939875869587,18.4882858516315,4.87764379077817));
#89386=CARTESIAN_POINT('Ctrl Pts',(-10.4463860301156,18.4909595575676,4.89435761860032));
#89387=CARTESIAN_POINT('Ctrl Pts',(-10.4073782491194,18.493066615075,4.90624926980271));
#89388=CARTESIAN_POINT('Ctrl Pts',(-10.2222492191598,18.502760558043,4.95433484845058));
#89389=CARTESIAN_POINT('Ctrl Pts',(-10.0716367098282,18.5096711303314,4.9694700847652));
#89390=CARTESIAN_POINT('Ctrl Pts',(-9.89708857762196,18.5186534628246,4.96007991369904));
#89391=CARTESIAN_POINT('Ctrl Pts',(-9.87283316913323,18.5199260337265,4.95816754039881));
#89392=CARTESIAN_POINT('Ctrl Pts',(-9.84289620320358,18.5215389859063,4.95505462900815));
#89393=CARTESIAN_POINT('Ctrl Pts',(-9.83715794117221,18.5218500844385,4.95442361023682));
#89394=CARTESIAN_POINT('Ctrl Pts',(-9.82817577117257,18.5223402833644,4.95338204716033));
#89395=CARTESIAN_POINT('Ctrl Pts',(-9.82492918699121,18.5225181271451,4.952994545972));
#89396=CARTESIAN_POINT('Ctrl Pts',(-9.81891721500178,18.5228487275864,4.95225653560759));
#89397=CARTESIAN_POINT('Ctrl Pts',(-9.81615151501714,18.5230013175686,4.95190900349485));
#89398=CARTESIAN_POINT('Ctrl Pts',(-9.80988714944279,18.523348072093,4.95110365039489));
#89399=CARTESIAN_POINT('Ctrl Pts',(-9.80638915329023,18.5235424973962,4.95064107884556));
#89400=CARTESIAN_POINT('Ctrl Pts',(-9.79578203754632,18.5241344147196,4.94919935562773));
#89401=CARTESIAN_POINT('Ctrl Pts',(-9.78867852484275,18.5245340281366,4.94818057520031));
#89402=CARTESIAN_POINT('Ctrl Pts',(-9.69523325299222,18.5298305984014,4.93407657012682));
#89403=CARTESIAN_POINT('Ctrl Pts',(-9.61023158522235,18.5350858865448,4.91334214191407));
#89404=CARTESIAN_POINT('Ctrl Pts',(-9.41941685056852,18.547227291252,4.84826518681616));
#89405=CARTESIAN_POINT('Ctrl Pts',(-9.31591476615047,18.5540493253382,4.7988193632697));
#89406=CARTESIAN_POINT('Ctrl Pts',(-9.20508493694049,18.5613752325927,4.72891060719764));
#89407=CARTESIAN_POINT('Ctrl Pts',(-9.1911108736851,18.5623003254658,4.71975803001214));
#89408=CARTESIAN_POINT('Ctrl Pts',(-9.17191033486806,18.5635738081848,4.70670715784962));
#89409=CARTESIAN_POINT('Ctrl Pts',(-9.16654897057532,18.563929670229,4.70301040800854));
#89410=CARTESIAN_POINT('Ctrl Pts',(-9.1573409695375,18.5645413678452,4.69657023532857));
#89411=CARTESIAN_POINT('Ctrl Pts',(-9.1534826439643,18.5647978382758,4.6938437654709));
#89412=CARTESIAN_POINT('Ctrl Pts',(-9.14552091471016,18.5653274245818,4.68815963879319));
#89413=CARTESIAN_POINT('Ctrl Pts',(-9.14141950202428,18.5656004331313,4.68519929287771));
#89414=CARTESIAN_POINT('Ctrl Pts',(-9.13184673438077,18.5662381456105,4.67821402612228));
#89415=CARTESIAN_POINT('Ctrl Pts',(-9.12638786262747,18.5666021917373,4.6741721421963));
#89416=CARTESIAN_POINT('Ctrl Pts',(-9.10870704111983,18.5677827480732,4.6608892610103));
#89417=CARTESIAN_POINT('Ctrl Pts',(-9.09660181337867,18.5685932725393,4.65149414009487));
#89418=CARTESIAN_POINT('Ctrl Pts',(-9.03430284268052,18.5727801824782,4.60155536321842));
#89419=CARTESIAN_POINT('Ctrl Pts',(-8.98668079926833,18.5760300968124,4.55791333902873));
#89420=CARTESIAN_POINT('Ctrl Pts',(-8.87247084567277,18.5841820677194,4.43843568637325));
#89421=CARTESIAN_POINT('Ctrl Pts',(-8.81056274972724,18.5889550555506,4.35861539172998));
#89422=CARTESIAN_POINT('Ctrl Pts',(-8.73648141049508,18.596003882923,4.23953583888169));
#89423=CARTESIAN_POINT('Ctrl Pts',(-8.71698421076062,18.5980335030499,4.2051683867065));
#89424=CARTESIAN_POINT('Ctrl Pts',(-8.69612600058251,18.60046779899,4.16466654462355));
#89425=CARTESIAN_POINT('Ctrl Pts',(-8.69338321127876,18.6007937005894,4.15925836118495));
#89426=CARTESIAN_POINT('Ctrl Pts',(-8.6890527411901,18.6013178794442,4.15058643261032));
#89427=CARTESIAN_POINT('Ctrl Pts',(-8.68744342486895,18.6015148623385,4.14733349842246));
#89428=CARTESIAN_POINT('Ctrl Pts',(-8.68461239035154,18.6018653441285,4.14155712659661));
#89429=CARTESIAN_POINT('Ctrl Pts',(-8.68338580361434,18.6020185400425,4.13903612424483));
#89430=CARTESIAN_POINT('Ctrl Pts',(-8.68079052281459,18.6023455791189,4.13366285486749));
#89431=CARTESIAN_POINT('Ctrl Pts',(-8.67942385268337,18.6025195366235,4.13080971543014));
#89432=CARTESIAN_POINT('Ctrl Pts',(-8.6757285313285,18.6029946185873,4.12303050980669));
#89433=CARTESIAN_POINT('Ctrl Pts',(-8.67341814666634,18.6032968278426,4.1180958852591));
#89434=CARTESIAN_POINT('Ctrl Pts',(-8.66160051125302,18.6048693130499,4.09248376055741));
#89435=CARTESIAN_POINT('Ctrl Pts',(-8.65254946860621,18.6061646506607,4.07160051174937));
#89436=CARTESIAN_POINT('Ctrl Pts',(-8.62671914249961,18.6101321803157,4.00797621518228));
#89437=CARTESIAN_POINT('Ctrl Pts',(-8.61146111572676,18.6128614491138,3.96464976342717));
#89438=CARTESIAN_POINT('Ctrl Pts',(-8.581325859582,18.6191491171178,3.86423724445855));
#89439=CARTESIAN_POINT('Ctrl Pts',(-8.56781060561573,18.6227161704226,3.80682056626437));
#89440=CARTESIAN_POINT('Ctrl Pts',(-8.5434141997546,18.6312813780389,3.66537208161505));
#89441=CARTESIAN_POINT('Ctrl Pts',(-8.53628922971168,18.6362024089687,3.58089939650866));
#89442=CARTESIAN_POINT('Ctrl Pts',(-8.53653204370949,18.6414866062904,3.48555390740052));
#89443=CARTESIAN_POINT('Ctrl Pts',(-8.53667710508559,18.6420770352681,3.47483529261879));
#89444=CARTESIAN_POINT('Ctrl Pts',(-8.53709860769564,18.6430181332781,3.45764836303294));
#89445=CARTESIAN_POINT('Ctrl Pts',(-8.5373002250128,18.6433711072986,3.45117874544495));
#89446=CARTESIAN_POINT('Ctrl Pts',(-8.53773463689923,18.643995797825,3.43968815245667));
#89447=CARTESIAN_POINT('Ctrl Pts',(-8.53795038803866,18.644268038691,3.4346666691707));
#89448=CARTESIAN_POINT('Ctrl Pts',(-8.53845428893852,18.6448341366366,3.42419661686861));
#89449=CARTESIAN_POINT('Ctrl Pts',(-8.53874704881716,18.6451278462459,3.41874834042412));
#89450=CARTESIAN_POINT('Ctrl Pts',(-8.53958834237091,18.6458898780341,3.40457191647122));
#89451=CARTESIAN_POINT('Ctrl Pts',(-8.54018465753275,18.6463567116404,3.39584675119378));
#89452=CARTESIAN_POINT('Ctrl Pts',(-8.54315578744952,18.6484026668579,3.35743801304619));
#89453=CARTESIAN_POINT('Ctrl Pts',(-8.54635810963059,18.649956016134,3.32782452149933));
#89454=CARTESIAN_POINT('Ctrl Pts',(-8.55746592606879,18.654095307351,3.24798598949941));
#89455=CARTESIAN_POINT('Ctrl Pts',(-8.56708800104811,18.6566311889731,3.19804081191957));
#89456=CARTESIAN_POINT('Ctrl Pts',(-8.59003794673595,18.66133169548,3.10522910337996));
#89457=CARTESIAN_POINT('Ctrl Pts',(-8.60277512639161,18.6635024111371,3.06227887389326));
#89458=CARTESIAN_POINT('Ctrl Pts',(-8.64478818450335,18.6697332921894,2.94127417799491));
#89459=CARTESIAN_POINT('Ctrl Pts',(-8.67878299831601,18.6737960375407,2.86505429119046));
#89460=CARTESIAN_POINT('Ctrl Pts',(-8.72454675093081,18.6787867304896,2.78223997708675));
#89461=CARTESIAN_POINT('Ctrl Pts',(-8.73013757597537,18.6793899617017,2.77239444100173));
#89462=CARTESIAN_POINT('Ctrl Pts',(-8.73804558528531,18.6802358052865,2.75883710669789));
#89463=CARTESIAN_POINT('Ctrl Pts',(-8.74026616993627,18.680472538678,2.75506909338957));
#89464=CARTESIAN_POINT('Ctrl Pts',(-8.74385160213527,18.6808536262899,2.74904700813513));
#89465=CARTESIAN_POINT('Ctrl Pts',(-8.74520572331474,18.6809972942244,2.74678653993729));
#89466=CARTESIAN_POINT('Ctrl Pts',(-8.7480469901349,18.6812982320707,2.74207246856585));
#89467=CARTESIAN_POINT('Ctrl Pts',(-8.74953524924617,18.6814555770695,2.73961957648321));
#89468=CARTESIAN_POINT('Ctrl Pts',(-8.75316399382042,18.6818385023396,2.73367828263712));
#89469=CARTESIAN_POINT('Ctrl Pts',(-8.75531191171081,18.6820645603632,2.73019446426505));
#89470=CARTESIAN_POINT('Ctrl Pts',(-8.76294593512555,18.6828657638731,2.71792792887253));
#89471=CARTESIAN_POINT('Ctrl Pts',(-8.76851048461643,18.6834457354618,2.70919468584696));
#89472=CARTESIAN_POINT('Ctrl Pts',(-8.82812234263739,18.6896108577193,2.61779238159771));
#89473=CARTESIAN_POINT('Ctrl Pts',(-8.89030968622555,18.695616987207,2.54074391230127));
#89474=CARTESIAN_POINT('Ctrl Pts',(-9.02838495177893,18.7074193181971,2.40122341709625));
#89475=CARTESIAN_POINT('Ctrl Pts',(-9.10376226169663,18.7131836117415,2.33891898377669));
#89476=CARTESIAN_POINT('Ctrl Pts',(-9.19904284257417,18.7196024029165,2.27501247650816));
#89477=CARTESIAN_POINT('Ctrl Pts',(-9.2134636367918,18.7205534098203,2.26570368819759));
#89478=CARTESIAN_POINT('Ctrl Pts',(-9.23426110936365,18.7218965228191,2.2527912238526));
#89479=CARTESIAN_POINT('Ctrl Pts',(-9.24050586496314,18.722296236083,2.2489786406692));
#89480=CARTESIAN_POINT('Ctrl Pts',(-9.25115308112507,18.722971768689,2.24258735156718));
#89481=CARTESIAN_POINT('Ctrl Pts',(-9.25554086963213,18.7232484572739,2.23998457133406));
#89482=CARTESIAN_POINT('Ctrl Pts',(-9.26443476749019,18.7238058991792,2.23477150055442));
#89483=CARTESIAN_POINT('Ctrl Pts',(-9.26894137932951,18.7240866138239,2.2321622102194));
#89484=CARTESIAN_POINT('Ctrl Pts',(-9.28004891647597,18.724774270396,2.225809956376));
#89485=CARTESIAN_POINT('Ctrl Pts',(-9.28666525024447,18.7251802395231,2.22209414757217));
#89486=CARTESIAN_POINT('Ctrl Pts',(-9.31106422645601,18.7266642803851,2.20863994313104));
#89487=CARTESIAN_POINT('Ctrl Pts',(-9.32902022793352,18.7277311395461,2.19921965917409));
#89488=CARTESIAN_POINT('Ctrl Pts',(-9.42725372019766,18.7334418551944,2.15025884621249));
#89489=CARTESIAN_POINT('Ctrl Pts',(-9.5108347760018,18.7378373903956,2.11777028976397));
#89490=CARTESIAN_POINT('Ctrl Pts',(-9.69528033882753,18.7471738754549,2.06491864368276));
#89491=CARTESIAN_POINT('Ctrl Pts',(-9.79636786818284,18.7520789374639,2.04712660131601));
#89492=CARTESIAN_POINT('Ctrl Pts',(-9.90911196850621,18.7580496802623,2.03928597871431));
#89493=CARTESIAN_POINT('Ctrl Pts',(-9.91976313814106,18.7586187716164,2.03866221595384));
#89494=CARTESIAN_POINT('Ctrl Pts',(-9.93468121458127,18.7594240320447,2.03795215313455));
#89495=CARTESIAN_POINT('Ctrl Pts',(-9.93894337795214,18.7596550335478,2.03776796019554));
#89496=CARTESIAN_POINT('Ctrl Pts',(-9.94581894463226,18.7600292700937,2.03750094023769));
#89497=CARTESIAN_POINT('Ctrl Pts',(-9.94843190391166,18.7601718642918,2.03740647553399));
#89498=CARTESIAN_POINT('Ctrl Pts',(-9.95393194051589,18.7604728184479,2.03722239312029));
#89499=CARTESIAN_POINT('Ctrl Pts',(-9.95681904118807,18.7606312658007,2.03713432002078));
#89500=CARTESIAN_POINT('Ctrl Pts',(-9.96389610477852,18.7610207822941,2.03693939765707));
#89501=CARTESIAN_POINT('Ctrl Pts',(-9.96808628506719,18.7612523679918,2.03684200057313));
#89502=CARTESIAN_POINT('Ctrl Pts',(-9.98327034169327,18.7620949101606,2.03655431584109));
#89503=CARTESIAN_POINT('Ctrl Pts',(-9.99426557663278,18.7627113619199,2.0364699341982));
#89504=CARTESIAN_POINT('Ctrl Pts',(-10.0649999890705,18.7667133959952,2.03672418211309));
#89505=CARTESIAN_POINT('Ctrl Pts',(-10.1246652906782,18.7702536171005,2.04059656495621));
#89506=CARTESIAN_POINT('Ctrl Pts',(-10.1982460606775,18.7747011000034,2.0499175013927));
#89507=CARTESIAN_POINT('Ctrl Pts',(-10.2125434928297,18.7755692801554,2.05194405787678));
#89508=CARTESIAN_POINT('Ctrl Pts',(-10.3481711280124,18.7838322218326,2.07322024615524));
#89509=CARTESIAN_POINT('Ctrl Pts',(-10.4666778091345,18.7911997754611,2.10746778044932));
#89510=CARTESIAN_POINT('Ctrl Pts',(-10.5942714054837,18.7989601922179,2.16249047262196));
#89511=CARTESIAN_POINT('Ctrl Pts',(-10.608915178728,18.7998491676177,2.16909332663192));
#89512=CARTESIAN_POINT('Ctrl Pts',(-10.6292422630092,18.8010811854801,2.17866452195563));
#89513=CARTESIAN_POINT('Ctrl Pts',(-10.6350189046432,18.801431082406,2.1814309787995));
#89514=CARTESIAN_POINT('Ctrl Pts',(-10.6449999453007,18.802035303737,2.18629174450317));
#89515=CARTESIAN_POINT('Ctrl Pts',(-10.6492127355964,18.8022902272634,2.18836852178129));
#89516=CARTESIAN_POINT('Ctrl Pts',(-10.6578669933686,18.8028137202805,2.19268671755451));
#89517=CARTESIAN_POINT('Ctrl Pts',(-10.6623071797158,18.8030822008843,2.19493057657343));
#89518=CARTESIAN_POINT('Ctrl Pts',(-10.6726808868895,18.8037092529278,2.20023953197276));
#89519=CARTESIAN_POINT('Ctrl Pts',(-10.6786050677288,18.8040671891047,2.20332270248199));
#89520=CARTESIAN_POINT('Ctrl Pts',(-10.6910908468669,18.8048213386004,2.20992978505063));
#89521=CARTESIAN_POINT('Ctrl Pts',(-10.6976470814831,18.8052172005832,2.21346345930166));
#89522=CARTESIAN_POINT('Ctrl Pts',(-10.7152721691126,18.8062812227657,2.22313736538282));
#89523=CARTESIAN_POINT('Ctrl Pts',(-10.7262889344517,18.8069461135178,2.2293714704402));
#89524=CARTESIAN_POINT('Ctrl Pts',(-10.8197795298147,18.8125906660714,2.28388866377502));
#89525=CARTESIAN_POINT('Ctrl Pts',(-10.8974235835359,18.8172722031773,2.34000061921834));
#89526=CARTESIAN_POINT('Ctrl Pts',(-11.0426344495342,18.8266961752259,2.46830809838115));
#89527=CARTESIAN_POINT('Ctrl Pts',(-11.1094805591221,18.8314191755474,2.54056120241384));
#89528=CARTESIAN_POINT('Ctrl Pts',(-11.1751087459218,18.8371759796641,2.62760717380487));
#89529=CARTESIAN_POINT('Ctrl Pts',(-11.1815394503109,18.837754124242,2.6363366850984));
#89530=CARTESIAN_POINT('Ctrl Pts',(-11.1903814953133,18.8385701870271,2.64862311681924));
#89531=CARTESIAN_POINT('Ctrl Pts',(-11.1928752185691,18.8388027536703,2.65212063736747));
#89532=CARTESIAN_POINT('Ctrl Pts',(-11.1968651964447,18.8391788572451,2.65776914276756));
#89533=CARTESIAN_POINT('Ctrl Pts',(-11.1983711543682,18.8393217410231,2.65991328335112));
#89534=CARTESIAN_POINT('Ctrl Pts',(-11.2015219394555,18.8396226689237,2.66442499444997));
#89535=CARTESIAN_POINT('Ctrl Pts',(-11.2031655345118,18.8397807970039,2.66679338876023));
#89536=CARTESIAN_POINT('Ctrl Pts',(-11.2071655744408,18.8401684281312,2.67259389759016));
#89537=CARTESIAN_POINT('Ctrl Pts',(-11.2095143835328,18.8403984366162,2.67603122779192));
#89538=CARTESIAN_POINT('Ctrl Pts',(-11.2179091213831,18.8412290166541,2.68842962325464));
#89539=CARTESIAN_POINT('Ctrl Pts',(-11.2238702373381,18.8418348851805,2.69744736471882));
#89540=CARTESIAN_POINT('Ctrl Pts',(-11.2610278974344,18.8457108417614,2.75503482030055));
#89541=CARTESIAN_POINT('Ctrl Pts',(-11.2894251684542,18.8491258879651,2.80534468732222));
#89542=CARTESIAN_POINT('Ctrl Pts',(-11.3603170823029,18.8587955058051,2.95034487485124));
#89543=CARTESIAN_POINT('Ctrl Pts',(-11.3958362314279,18.8650966776298,3.04808334101784));
#89544=CARTESIAN_POINT('Ctrl Pts',(-11.428530157041,18.8729875691269,3.18032639978974));
#89545=CARTESIAN_POINT('Ctrl Pts',(-11.4352804511279,18.8748428025503,3.21214608978472));
#89546=CARTESIAN_POINT('Ctrl Pts',(-11.4441814339091,18.8776969539278,3.26228020459244));
#89547=CARTESIAN_POINT('Ctrl Pts',(-11.4470557275583,18.8787176641047,3.2804539230847));
#89548=CARTESIAN_POINT('Ctrl Pts',(-11.4506210494256,18.8801404540088,3.30612540022741));
#89549=CARTESIAN_POINT('Ctrl Pts',(-11.4515980169538,18.880551428578,3.31358114470718));
#89550=CARTESIAN_POINT('Ctrl Pts',(-11.4530890471029,18.881214955985,3.32568327950151));
#89551=CARTESIAN_POINT('Ctrl Pts',(-11.453638377954,18.8814686072157,3.33032512059649));
#89552=CARTESIAN_POINT('Ctrl Pts',(-11.4546996683609,18.881977937171,3.33967667889566));
#89553=CARTESIAN_POINT('Ctrl Pts',(-11.455211016886,18.8822335939466,3.34438640971473));
#89554=CARTESIAN_POINT('Ctrl Pts',(-11.4562112003746,18.8827556143257,3.3540348715201));
#89555=CARTESIAN_POINT('Ctrl Pts',(-11.4566978010851,18.8830219053279,3.3589737755919));
#89556=CARTESIAN_POINT('Ctrl Pts',(-11.4577688305633,18.8836381435864,3.37044206157947));
#89557=CARTESIAN_POINT('Ctrl Pts',(-11.4583345328788,18.8839875075812,3.37697311326332));
#89558=CARTESIAN_POINT('Ctrl Pts',(-11.4600523568521,18.8851332574215,3.39848578774896));
#89559=CARTESIAN_POINT('Ctrl Pts',(-11.4610176633964,18.885923903218,3.41348162672928));
#89560=CARTESIAN_POINT('Ctrl Pts',(-11.4629170959972,18.8879521529579,3.45230837672371));
#89561=CARTESIAN_POINT('Ctrl Pts',(-11.4635,18.8891793096102,3.47615209647377));
#89562=CARTESIAN_POINT('Ctrl Pts',(-11.4635,18.8903920399481,3.49999999999848));
#89563=CARTESIAN_POINT('Origin',(-10.,13.2,3.5));
#89564=CARTESIAN_POINT('',(-11.4635,19.4617257853095,3.50000000002413));
#89565=CARTESIAN_POINT('',(-11.4635,19.3881255777082,3.49999999999758));
#89566=CARTESIAN_POINT('',(-11.4635,13.2,3.5));
#89567=CARTESIAN_POINT('',(-11.4634997839299,18.9595020917114,3.50079525917368));
#89568=CARTESIAN_POINT('Ctrl Pts',(-11.4635,19.4617257853095,3.50000000002413));
#89569=CARTESIAN_POINT('Ctrl Pts',(-11.4635000000026,19.4524485230724,3.3412217020481));
#89570=CARTESIAN_POINT('Ctrl Pts',(-11.4376650484514,19.4425861276583,3.18348540399603));
#89571=CARTESIAN_POINT('Ctrl Pts',(-11.3783221719652,19.4320345915534,3.00725738649133));
#89572=CARTESIAN_POINT('Ctrl Pts',(-11.3689573148942,19.4305183273054,2.98180766057932));
#89573=CARTESIAN_POINT('Ctrl Pts',(-11.3556309158342,19.4285418047488,2.94848015531596));
#89574=CARTESIAN_POINT('Ctrl Pts',(-11.3522981584465,19.4280608332659,2.94035813735574));
#89575=CARTESIAN_POINT('Ctrl Pts',(-11.3467735026669,19.42728457902,2.92723196774772));
#89576=CARTESIAN_POINT('Ctrl Pts',(-11.3446263481021,19.426987802169,2.92220931872042));
#89577=CARTESIAN_POINT('Ctrl Pts',(-11.3404513020567,19.4264200030463,2.91259232618528));
#89578=CARTESIAN_POINT('Ctrl Pts',(-11.3384277875086,19.4261488379691,2.90799617658701));
#89579=CARTESIAN_POINT('Ctrl Pts',(-11.3337052068178,19.4255251255251,2.89741743638549));
#89580=CARTESIAN_POINT('Ctrl Pts',(-11.330989462413,19.425173150328,2.89144237945448));
#89581=CARTESIAN_POINT('Ctrl Pts',(-11.3223227572006,19.4240704968521,2.87270984642012));
#89582=CARTESIAN_POINT('Ctrl Pts',(-11.3162277773467,19.4233247416354,2.86001963517606));
#89583=CARTESIAN_POINT('Ctrl Pts',(-11.2854568896411,19.4196983183261,2.79825206581243));
#89584=CARTESIAN_POINT('Ctrl Pts',(-11.2582133820865,19.4169077474748,2.75050050609355));
#89585=CARTESIAN_POINT('Ctrl Pts',(-11.1709614261774,19.4089267219041,2.61579165080753));
#89586=CARTESIAN_POINT('Ctrl Pts',(-11.104162486679,19.4039360201529,2.533667497967));
#89587=CARTESIAN_POINT('Ctrl Pts',(-11.0219259393998,19.3981646355012,2.45233504232117));
#89588=CARTESIAN_POINT('Ctrl Pts',(-11.0146633423629,19.3976575064748,2.44529967053531));
#89589=CARTESIAN_POINT('Ctrl Pts',(-10.9907607225171,19.3959945233693,2.4226202853351));
#89590=CARTESIAN_POINT('Ctrl Pts',(-10.9738279133202,19.3948258907295,2.40729099817625));
#89591=CARTESIAN_POINT('Ctrl Pts',(-10.9443044568649,19.3927904753356,2.38179479541691));
#89592=CARTESIAN_POINT('Ctrl Pts',(-10.9318909066807,19.3919352733111,2.37142874323844));
#89593=CARTESIAN_POINT('Ctrl Pts',(-10.9153873143281,19.3907953094447,2.35810520901328));
#89594=CARTESIAN_POINT('Ctrl Pts',(-10.9114496992113,19.3905231053712,2.35495978532642));
#89595=CARTESIAN_POINT('Ctrl Pts',(-10.905085867791,19.3900826875053,2.34992988941526));
#89596=CARTESIAN_POINT('Ctrl Pts',(-10.9026697915969,19.3899153665694,2.34803258105276));
#89597=CARTESIAN_POINT('Ctrl Pts',(-10.8980167565477,19.3895928744069,2.3444022489014));
#89598=CARTESIAN_POINT('Ctrl Pts',(-10.8957807317323,19.3894377844098,2.34266809534273));
#89599=CARTESIAN_POINT('Ctrl Pts',(-10.8904696340765,19.3890691566503,2.33857367523647));
#89600=CARTESIAN_POINT('Ctrl Pts',(-10.8873901956392,19.3888552246634,2.33621912842635));
#89601=CARTESIAN_POINT('Ctrl Pts',(-10.8770896045394,19.3881390797345,2.32840792248312));
#89602=CARTESIAN_POINT('Ctrl Pts',(-10.8698273382458,19.3876332749473,2.32300613268513));
#89603=CARTESIAN_POINT('Ctrl Pts',(-10.8296007985981,19.3848288110455,2.29366061717046));
#89604=CARTESIAN_POINT('Ctrl Pts',(-10.7957001677799,19.3824556870078,2.27103584444739));
#89605=CARTESIAN_POINT('Ctrl Pts',(-10.680352843892,19.3744595974338,2.20082939784806));
#89606=CARTESIAN_POINT('Ctrl Pts',(-10.5952523625627,19.3687001125254,2.15970152865512));
#89607=CARTESIAN_POINT('Ctrl Pts',(-10.4393901202397,19.3588591008574,2.10216979943314));
#89608=CARTESIAN_POINT('Ctrl Pts',(-10.3702500096279,19.3547139126427,2.08228696008173));
#89609=CARTESIAN_POINT('Ctrl Pts',(-10.2896331116339,19.3501511161827,2.06540759108002));
#89610=CARTESIAN_POINT('Ctrl Pts',(-10.2793226725288,19.349572366234,2.06336449584378));
#89611=CARTESIAN_POINT('Ctrl Pts',(-10.262689972495,19.3486462973541,2.06025442578539));
#89612=CARTESIAN_POINT('Ctrl Pts',(-10.2563812790387,19.3482967877577,2.05911763779681));
#89613=CARTESIAN_POINT('Ctrl Pts',(-10.2451233704981,19.347676136775,2.05716531096991));
#89614=CARTESIAN_POINT('Ctrl Pts',(-10.2401770770362,19.3474044932385,2.05633370228128));
#89615=CARTESIAN_POINT('Ctrl Pts',(-10.2298145000246,19.3468375495628,2.05464619807104));
#89616=CARTESIAN_POINT('Ctrl Pts',(-10.2243974771326,19.3465424097218,2.05379528055222));
#89617=CARTESIAN_POINT('Ctrl Pts',(-10.2102011380848,19.345772091221,2.05164697379681));
#89618=CARTESIAN_POINT('Ctrl Pts',(-10.2014145054314,19.34529846393,2.05039894845542));
#89619=CARTESIAN_POINT('Ctrl Pts',(-10.1617971925706,19.3431765931866,2.0451390037453));
#89620=CARTESIAN_POINT('Ctrl Pts',(-10.1308536167949,19.3415566083917,2.0420300541232));
#89621=CARTESIAN_POINT('Ctrl Pts',(-10.0457844723548,19.3371853026616,2.03621349773804));
#89622=CARTESIAN_POINT('Ctrl Pts',(-9.99157003237367,19.334491790305,2.03552170208954));
#89623=CARTESIAN_POINT('Ctrl Pts',(-9.84606763351743,19.327350877629,2.04174722922775));
#89624=CARTESIAN_POINT('Ctrl Pts',(-9.75526945254689,19.3229954474432,2.05421250553614));
#89625=CARTESIAN_POINT('Ctrl Pts',(-9.62850193768208,19.3164453316802,2.08390563547147));
#89626=CARTESIAN_POINT('Ctrl Pts',(-9.5911389195793,19.3144523968771,2.09423821785307));
#89627=CARTESIAN_POINT('Ctrl Pts',(-9.54848556310275,19.3120593214827,2.10787810299123));
#89628=CARTESIAN_POINT('Ctrl Pts',(-9.54274950552511,19.3117349894782,2.10975158850731));
#89629=CARTESIAN_POINT('Ctrl Pts',(-9.53359123633073,19.311212893273,2.11280563028858));
#89630=CARTESIAN_POINT('Ctrl Pts',(-9.53016147366375,19.3110164077606,2.11396352400709));
#89631=CARTESIAN_POINT('Ctrl Pts',(-9.52408498371202,19.3106665310475,2.11604010304071));
#89632=CARTESIAN_POINT('Ctrl Pts',(-9.52143655692601,19.3105134396495,2.11695367757221));
#89633=CARTESIAN_POINT('Ctrl Pts',(-9.51579965186166,19.3101863049149,2.11891625747655));
#89634=CARTESIAN_POINT('Ctrl Pts',(-9.51281199829518,19.3100121453022,2.11996734400902));
#89635=CARTESIAN_POINT('Ctrl Pts',(-9.50467564682918,19.3095357894121,2.12285950827203));
#89636=CARTESIAN_POINT('Ctrl Pts',(-9.49953387137099,19.3092324982303,2.12471973730548));
#89637=CARTESIAN_POINT('Ctrl Pts',(-9.4727914080038,19.3076437406707,2.13456464942518));
#89638=CARTESIAN_POINT('Ctrl Pts',(-9.45137210010414,19.3063326011449,2.14302914507264));
#89639=CARTESIAN_POINT('Ctrl Pts',(-9.38707003955389,19.3022973956454,2.17021132186913));
#89640=CARTESIAN_POINT('Ctrl Pts',(-9.34487815567612,19.2995141595237,2.19048256889337));
#89641=CARTESIAN_POINT('Ctrl Pts',(-9.26719040448947,19.2942146194269,2.23250312849887));
#89642=CARTESIAN_POINT('Ctrl Pts',(-9.23150672551661,19.2917055362684,2.25381529490041));
#89643=CARTESIAN_POINT('Ctrl Pts',(-9.11231676879165,19.2831434999268,2.3320703966411));
#89644=CARTESIAN_POINT('Ctrl Pts',(-9.03381295054377,19.2772076913192,2.39612953280818));
#89645=CARTESIAN_POINT('Ctrl Pts',(-8.95504591408695,19.2710198370259,2.47529725484498));
#89646=CARTESIAN_POINT('Ctrl Pts',(-8.94764654684068,19.2704356845538,2.48289775560714));
#89647=CARTESIAN_POINT('Ctrl Pts',(-8.93588943315622,19.2695026889125,2.49524012478654));
#89648=CARTESIAN_POINT('Ctrl Pts',(-8.93147930777664,19.2691516022992,2.49993138362786));
#89649=CARTESIAN_POINT('Ctrl Pts',(-8.92368628174116,19.2685291501771,2.50833159424205));
#89650=CARTESIAN_POINT('Ctrl Pts',(-8.92029125487751,19.2682572722157,2.51202911294484));
#89651=CARTESIAN_POINT('Ctrl Pts',(-8.91323696348129,19.2676908354403,2.51979172308752));
#89652=CARTESIAN_POINT('Ctrl Pts',(-8.90958132329648,19.2673964307516,2.52386001296781));
#89653=CARTESIAN_POINT('Ctrl Pts',(-8.90009630243397,19.2666302150475,2.53453547971394));
#89654=CARTESIAN_POINT('Ctrl Pts',(-8.89430358326092,19.2661599246375,2.54117503034391));
#89655=CARTESIAN_POINT('Ctrl Pts',(-8.86876223180642,19.2640752308194,2.57098954588913));
#89656=CARTESIAN_POINT('Ctrl Pts',(-8.84967898401814,19.2624878547055,2.59472598410348));
#89657=CARTESIAN_POINT('Ctrl Pts',(-8.79973351710246,19.2582307599563,2.66098202371571));
#89658=CARTESIAN_POINT('Ctrl Pts',(-8.77039700663102,19.2556149532308,2.70459579877185));
#89659=CARTESIAN_POINT('Ctrl Pts',(-8.68913403800723,19.2478329577494,2.84068649317437));
#89660=CARTESIAN_POINT('Ctrl Pts',(-8.64485016577919,19.2428200578731,2.93730197707057));
#89661=CARTESIAN_POINT('Ctrl Pts',(-8.60263873539193,19.2359892470634,3.06413137353829));
#89662=CARTESIAN_POINT('Ctrl Pts',(-8.59463785285838,19.2345459040571,3.09066272712875));
#89663=CARTESIAN_POINT('Ctrl Pts',(-8.58596164926306,19.2327688523476,3.12269658637106));
#89664=CARTESIAN_POINT('Ctrl Pts',(-8.58455779865475,19.2324736600671,3.12799772037629));
#89665=CARTESIAN_POINT('Ctrl Pts',(-8.58230852278426,19.2319877130592,3.13668838656857));
#89666=CARTESIAN_POINT('Ctrl Pts',(-8.58144536897563,19.2317979435292,3.14007332509899));
#89667=CARTESIAN_POINT('Ctrl Pts',(-8.57991601569942,19.2314556609791,3.14616178783846));
#89668=CARTESIAN_POINT('Ctrl Pts',(-8.57924540527199,19.2313034021861,3.14886415132922));
#89669=CARTESIAN_POINT('Ctrl Pts',(-8.57779804676516,19.2309699834298,3.15476861290011));
#89670=CARTESIAN_POINT('Ctrl Pts',(-8.57702440897239,19.2307886541447,3.15797138522856));
#89671=CARTESIAN_POINT('Ctrl Pts',(-8.57486018795554,19.230272497008,3.16706546068466));
#89672=CARTESIAN_POINT('Ctrl Pts',(-8.57349534783142,19.2299362558809,3.17296274512755));
#89673=CARTESIAN_POINT('Ctrl Pts',(-8.56499619218746,19.227772651871,3.21075213362819));
#89674=CARTESIAN_POINT('Ctrl Pts',(-8.55889572602779,19.2258932815956,3.24286500192575));
#89675=CARTESIAN_POINT('Ctrl Pts',(-8.54132305107115,19.2191989107634,3.35588505618728));
#89676=CARTESIAN_POINT('Ctrl Pts',(-8.53555341202188,19.2142297614304,3.43752451107034));
#89677=CARTESIAN_POINT('Ctrl Pts',(-8.5378977806997,19.2035218500461,3.61605195314118));
#89678=CARTESIAN_POINT('Ctrl Pts',(-8.54877797047256,19.1978466268146,3.71253515469245));
#89679=CARTESIAN_POINT('Ctrl Pts',(-8.571360226001,19.1918855814505,3.81770263479479));
#89680=CARTESIAN_POINT('Ctrl Pts',(-8.5737194396154,19.191296671026,3.82813158886203));
#89681=CARTESIAN_POINT('Ctrl Pts',(-8.57768790715829,19.1903575797684,3.84482218291235));
#89682=CARTESIAN_POINT('Ctrl Pts',(-8.5792246970207,19.1900051085473,3.85110050924547));
#89683=CARTESIAN_POINT('Ctrl Pts',(-8.58202967401712,19.1893810704679,3.86223975230408));
#89684=CARTESIAN_POINT('Ctrl Pts',(-8.58328138306868,19.1891089820984,3.86710467830216));
#89685=CARTESIAN_POINT('Ctrl Pts',(-8.58594517343029,19.1885429674895,3.87724127615743));
#89686=CARTESIAN_POINT('Ctrl Pts',(-8.58736174575787,19.1882491900568,3.88251169490943));
#89687=CARTESIAN_POINT('Ctrl Pts',(-8.59112800416835,19.1874864777828,3.89621790774856));
#89688=CARTESIAN_POINT('Ctrl Pts',(-8.5935239999163,19.1870190374626,3.90464082436167));
#89689=CARTESIAN_POINT('Ctrl Pts',(-8.60443687727148,19.1849655295444,3.94173568266471));
#89690=CARTESIAN_POINT('Ctrl Pts',(-8.61375624750092,19.1834054797222,3.97016514612553));
#89691=CARTESIAN_POINT('Ctrl Pts',(-8.64136026491014,19.1792429169887,4.04639531394243));
#89692=CARTESIAN_POINT('Ctrl Pts',(-8.66129102499622,19.176691217273,4.09355588507725));
#89693=CARTESIAN_POINT('Ctrl Pts',(-8.72434143447789,19.1696000335026,4.22332311603181));
#89694=CARTESIAN_POINT('Ctrl Pts',(-8.77292702672683,19.1651715642419,4.30298900748788));
#89695=CARTESIAN_POINT('Ctrl Pts',(-8.85354707607167,19.1584286167577,4.41059800253315));
#89696=CARTESIAN_POINT('Ctrl Pts',(-8.8797370631283,19.1563077281068,4.4426311048685));
#89697=CARTESIAN_POINT('Ctrl Pts',(-8.91171439053565,19.1537396173159,4.47852532434047));
#89698=CARTESIAN_POINT('Ctrl Pts',(-8.91621738480605,19.1533784387528,4.48351035464096));
#89699=CARTESIAN_POINT('Ctrl Pts',(-8.92310438865228,19.1528264175971,4.49102986714121));
#89700=CARTESIAN_POINT('Ctrl Pts',(-8.92546344206393,19.1526373957696,4.4935872082774));
#89701=CARTESIAN_POINT('Ctrl Pts',(-8.92972627462679,19.152295897515,4.49817541120781));
#89702=CARTESIAN_POINT('Ctrl Pts',(-8.93162674771857,19.1521436699795,4.50020927428896));
#89703=CARTESIAN_POINT('Ctrl Pts',(-8.93579729643342,19.1518096454743,4.50464709607204));
#89704=CARTESIAN_POINT('Ctrl Pts',(-8.93806969200833,19.1516276745681,4.50704875872401));
#89705=CARTESIAN_POINT('Ctrl Pts',(-8.94456210899373,19.1511079040361,4.51386409220888));
#89706=CARTESIAN_POINT('Ctrl Pts',(-8.94880159119083,19.1507686604302,4.5182590249448));
#89707=CARTESIAN_POINT('Ctrl Pts',(-8.97668493832947,19.1485392716742,4.54680506536336));
#89708=CARTESIAN_POINT('Ctrl Pts',(-9.001130224203,19.1465934988796,4.5701557736849));
#89709=CARTESIAN_POINT('Ctrl Pts',(-9.09645481502427,19.1391112196426,4.65509872569979));
#89710=CARTESIAN_POINT('Ctrl Pts',(-9.17239646759694,19.1333745877624,4.71066900008591));
#89711=CARTESIAN_POINT('Ctrl Pts',(-9.3249163251688,19.1227978244221,4.80117668905939));
#89712=CARTESIAN_POINT('Ctrl Pts',(-9.400215424835,19.1179466887933,4.83755780285789));
#89713=CARTESIAN_POINT('Ctrl Pts',(-9.48819707202169,19.112728041925,4.87113242719118));
#89714=CARTESIAN_POINT('Ctrl Pts',(-9.49821931849686,19.1121396501248,4.87483181741007));
#89715=CARTESIAN_POINT('Ctrl Pts',(-9.51436658934363,19.1112012230839,4.88059196818485));
#89716=CARTESIAN_POINT('Ctrl Pts',(-9.52046618965083,19.1108489025931,4.882722430124));
#89717=CARTESIAN_POINT('Ctrl Pts',(-9.53133260169763,19.1102250373651,4.88643728645773));
#89718=CARTESIAN_POINT('Ctrl Pts',(-9.53609380961473,19.1099529721035,4.88803765327444));
#89719=CARTESIAN_POINT('Ctrl Pts',(-9.54604628235298,19.1093869125499,4.89132601113578));
#89720=CARTESIAN_POINT('Ctrl Pts',(-9.55123894862432,19.1090930676393,4.89300953582749));
#89721=CARTESIAN_POINT('Ctrl Pts',(-9.56479141957688,19.108329978341,4.89731976470854));
#89722=CARTESIAN_POINT('Ctrl Pts',(-9.57316567954627,19.1078622312734,4.89990053243183));
#89723=CARTESIAN_POINT('Ctrl Pts',(-9.61027892796517,19.1058053915191,4.91097404920086));
#89724=CARTESIAN_POINT('Ctrl Pts',(-9.63925266202821,19.1042424234472,4.91865845208204));
#89725=CARTESIAN_POINT('Ctrl Pts',(-9.71841524391045,19.1000698153711,4.93707152551713));
#89726=CARTESIAN_POINT('Ctrl Pts',(-9.76896607511278,19.0975113124651,4.94605961588683));
#89727=CARTESIAN_POINT('Ctrl Pts',(-9.91584444952054,19.090237691633,4.96427439282175));
#89728=CARTESIAN_POINT('Ctrl Pts',(-10.0127380826137,19.0856460104106,4.96663467823313));
#89729=CARTESIAN_POINT('Ctrl Pts',(-10.1468527378634,19.0788719116609,4.95660425529117));
#89730=CARTESIAN_POINT('Ctrl Pts',(-10.1844289326779,19.0769255190811,4.9523247553457));
#89731=CARTESIAN_POINT('Ctrl Pts',(-10.2277217809414,19.0745846396972,4.94568703522324));
#89732=CARTESIAN_POINT('Ctrl Pts',(-10.2336437132274,19.0742622841533,4.94474178528179));
#89733=CARTESIAN_POINT('Ctrl Pts',(-10.243119913875,19.0737427682739,4.94316942267513));
#89734=CARTESIAN_POINT('Ctrl Pts',(-10.2466780244964,19.0735468667013,4.9425655017117));
#89735=CARTESIAN_POINT('Ctrl Pts',(-10.2529928539392,19.0731976463438,4.94146963455314));
#89736=CARTESIAN_POINT('Ctrl Pts',(-10.255750436706,19.0730446233236,4.94098293033323));
#89737=CARTESIAN_POINT('Ctrl Pts',(-10.2616304624845,19.0727171926923,4.93992771469341));
#89738=CARTESIAN_POINT('Ctrl Pts',(-10.264752408592,19.0725426660079,4.93935696899386));
#89739=CARTESIAN_POINT('Ctrl Pts',(-10.2732771284898,19.0720642940924,4.93776983005245));
#89740=CARTESIAN_POINT('Ctrl Pts',(-10.2786760139853,19.0717593386902,4.93673315212822));
#89741=CARTESIAN_POINT('Ctrl Pts',(-10.3070503523027,19.0701465902986,4.93111884847474));
#89742=CARTESIAN_POINT('Ctrl Pts',(-10.3299180609175,19.0688122148497,4.92602069479193));
#89743=CARTESIAN_POINT('Ctrl Pts',(-10.3993143190696,19.0646768191767,4.90879093602591));
#89744=CARTESIAN_POINT('Ctrl Pts',(-10.4453745519343,19.0618134842561,4.89491389567479));
#89745=CARTESIAN_POINT('Ctrl Pts',(-10.6015533422794,19.0518610518198,4.83933534920191));
#89746=CARTESIAN_POINT('Ctrl Pts',(-10.7072956744309,19.0447358639228,4.78663373496802));
#89747=CARTESIAN_POINT('Ctrl Pts',(-10.8292061074749,19.0364373843041,4.70625445152632));
#89748=CARTESIAN_POINT('Ctrl Pts',(-10.8523689734237,19.0348536701358,4.68999994114569));
#89749=CARTESIAN_POINT('Ctrl Pts',(-10.882197461977,19.0328038014142,4.66774974224451));
#89750=CARTESIAN_POINT('Ctrl Pts',(-10.8892988438916,19.0323149617858,4.66235080489159));
#89751=CARTESIAN_POINT('Ctrl Pts',(-10.9006930869062,19.0315291687146,4.6535226011869));
#89752=CARTESIAN_POINT('Ctrl Pts',(-10.9050167034869,19.0312306527563,4.65013355563903));
#89753=CARTESIAN_POINT('Ctrl Pts',(-10.9131080895021,19.0306713149452,4.64371728376321));
#89754=CARTESIAN_POINT('Ctrl Pts',(-10.9168801345462,19.03041028001,4.64069558951642));
#89755=CARTESIAN_POINT('Ctrl Pts',(-10.9255125347198,19.0298122083475,4.63370989805401));
#89756=CARTESIAN_POINT('Ctrl Pts',(-10.9303625348391,19.0294756835999,4.62973321643136));
#89757=CARTESIAN_POINT('Ctrl Pts',(-10.9404648942874,19.0287735690889,4.62134076687125));
#89758=CARTESIAN_POINT('Ctrl Pts',(-10.9457120712773,19.0284082311885,4.61691898238927));
#89759=CARTESIAN_POINT('Ctrl Pts',(-10.9594608528606,19.0274490641185,4.60516656268905));
#89760=CARTESIAN_POINT('Ctrl Pts',(-10.9679096354125,19.0268577074367,4.5977746609398));
#89761=CARTESIAN_POINT('Ctrl Pts',(-10.9931424155635,19.0250847871176,4.57518052432145));
#89762=CARTESIAN_POINT('Ctrl Pts',(-11.0096597861465,19.0239150240216,4.55968495370579));
#89763=CARTESIAN_POINT('Ctrl Pts',(-11.0707156452118,19.0195438407297,4.49968198920872));
#89764=CARTESIAN_POINT('Ctrl Pts',(-11.1127274369591,19.0164407865026,4.45269854547398));
#89765=CARTESIAN_POINT('Ctrl Pts',(-11.2162224705601,19.008261125164,4.32073501696944));
#89766=CARTESIAN_POINT('Ctrl Pts',(-11.271818271681,19.0032752039734,4.23162581080527));
#89767=CARTESIAN_POINT('Ctrl Pts',(-11.324354224812,18.9969774402849,4.12303404272962));
#89768=CARTESIAN_POINT('Ctrl Pts',(-11.331050762151,18.9961355313254,4.108596219519));
#89769=CARTESIAN_POINT('Ctrl Pts',(-11.3395433659732,18.9950109244557,4.08947511250625));
#89770=CARTESIAN_POINT('Ctrl Pts',(-11.3415529367248,18.9947403690034,4.08488721483336));
#89771=CARTESIAN_POINT('Ctrl Pts',(-11.3447542327214,18.9943019813114,4.0774752796125));
#89772=CARTESIAN_POINT('Ctrl Pts',(-11.3459607238252,18.994135027147,4.07465761506311));
#89773=CARTESIAN_POINT('Ctrl Pts',(-11.3482650872044,18.9938127460461,4.06922888860492));
#89774=CARTESIAN_POINT('Ctrl Pts',(-11.3493642377146,18.9936574970333,4.06661841345753));
#89775=CARTESIAN_POINT('Ctrl Pts',(-11.3519561614253,18.9932877782613,4.06041229886672));
#89776=CARTESIAN_POINT('Ctrl Pts',(-11.3534421735571,18.9930729078479,4.0568138730817));
#89777=CARTESIAN_POINT('Ctrl Pts',(-11.3583717677595,18.9923504038943,4.04474037484503));
#89778=CARTESIAN_POINT('Ctrl Pts',(-11.3617501698118,18.9918390926783,4.0362391273953));
#89779=CARTESIAN_POINT('Ctrl Pts',(-11.3800447281281,18.9889807957476,3.98891559194911));
#89780=CARTESIAN_POINT('Ctrl Pts',(-11.3933793656938,18.9865563240167,3.94950559920582));
#89781=CARTESIAN_POINT('Ctrl Pts',(-11.4437290608436,18.9758948947297,3.7767888706231));
#89782=CARTESIAN_POINT('Ctrl Pts',(-11.463424603677,18.9673935543336,3.63914799684217));
#89783=CARTESIAN_POINT('Ctrl Pts',(-11.4634997839299,18.9595020917114,3.50079525917368));
#89784=CARTESIAN_POINT('Ctrl Pts',(-11.463499784802,18.9595020000746,3.50079365260118));
#89785=CARTESIAN_POINT('Ctrl Pts',(-11.4634999282675,18.9594869104204,3.50052910137612));
#89786=CARTESIAN_POINT('Ctrl Pts',(-11.4635,18.9594718228119,3.50026455050034));
#89787=CARTESIAN_POINT('Ctrl Pts',(-11.4635,18.9594567372512,3.50000000000276));
#89788=CARTESIAN_POINT('',(-11.4634994779773,18.8904305419548,3.50076815470882));
#89789=CARTESIAN_POINT('Ctrl Pts',(-11.4635,18.8903920399481,3.49999999999848));
#89790=CARTESIAN_POINT('Ctrl Pts',(-11.4635,18.8904050895196,3.50025661510164));
#89791=CARTESIAN_POINT('Ctrl Pts',(-11.4634999325063,18.8904181374306,3.50051323068873));
#89792=CARTESIAN_POINT('Ctrl Pts',(-11.4634997975183,18.8904311836853,3.50076984673329));
#89793=CARTESIAN_POINT('Ctrl Pts',(-11.4634997984221,18.890431096239,3.50076812669027));
#89794=CARTESIAN_POINT('Ctrl Pts',(-11.4634937883446,18.8910132559842,3.51221903341649));
#89795=CARTESIAN_POINT('Ctrl Pts',(-11.4633533849326,18.8915920540778,3.52366969261506));
#89796=CARTESIAN_POINT('Ctrl Pts',(-11.4597985251028,18.8990413693994,3.67177255314227));
#89797=CARTESIAN_POINT('Ctrl Pts',(-11.4373908907185,18.9053791212155,3.80727533817238));
#89798=CARTESIAN_POINT('Ctrl Pts',(-11.387649115658,18.9138592895339,3.96598437396818));
#89799=CARTESIAN_POINT('Ctrl Pts',(-11.3779237119127,18.9154017383441,3.99400152961883));
#89800=CARTESIAN_POINT('Ctrl Pts',(-11.3652526854024,18.9173062261339,4.02721165613559));
#89801=CARTESIAN_POINT('Ctrl Pts',(-11.3631172800626,18.9176239920481,4.03270846040276));
#89802=CARTESIAN_POINT('Ctrl Pts',(-11.3597492183937,18.9181205272658,4.04122541780645));
#89803=CARTESIAN_POINT('Ctrl Pts',(-11.3585395619885,18.918297956365,4.04425467190385));
#89804=CARTESIAN_POINT('Ctrl Pts',(-11.3562771197782,18.9186281866594,4.04986580073081));
#89805=CARTESIAN_POINT('Ctrl Pts',(-11.3552270771593,18.918780824336,4.05244872467638));
#89806=CARTESIAN_POINT('Ctrl Pts',(-11.3528275386992,18.9191282071699,4.05830316529903));
#89807=CARTESIAN_POINT('Ctrl Pts',(-11.3514735598145,18.919323217104,4.06157278283855));
#89808=CARTESIAN_POINT('Ctrl Pts',(-11.3473178487401,18.9199186452004,4.07150600877889));
#89809=CARTESIAN_POINT('Ctrl Pts',(-11.3444786363621,18.9203212209716,4.07815369547151));
#89810=CARTESIAN_POINT('Ctrl Pts',(-11.3119708262875,18.9248815707213,4.15273245892959));
#89811=CARTESIAN_POINT('Ctrl Pts',(-11.2772342277427,18.9292997755313,4.21832970371251));
#89812=CARTESIAN_POINT('Ctrl Pts',(-11.1869509978999,18.9394720120493,4.36140421947868));
#89813=CARTESIAN_POINT('Ctrl Pts',(-11.1284992205411,18.9452158305324,4.4366765185587));
#89814=CARTESIAN_POINT('Ctrl Pts',(-11.0434421340565,18.952368274697,4.52658830911708));
#89815=CARTESIAN_POINT('Ctrl Pts',(-11.0231203673566,18.9540035229907,4.54684283129346));
#89816=CARTESIAN_POINT('Ctrl Pts',(-10.9925357526582,18.9563592854659,4.57558424463029));
#89817=CARTESIAN_POINT('Ctrl Pts',(-10.9827325184723,18.9570994036766,4.58454852404956));
#89818=CARTESIAN_POINT('Ctrl Pts',(-10.9648557884184,18.9584226203781,4.60045393613906));
#89819=CARTESIAN_POINT('Ctrl Pts',(-10.9568261076936,18.9590076642827,4.60744271457308));
#89820=CARTESIAN_POINT('Ctrl Pts',(-10.9443106959637,18.9599054731251,4.61809798537478));
#89821=CARTESIAN_POINT('Ctrl Pts',(-10.9398783596608,18.9602207615261,4.62182639735366));
#89822=CARTESIAN_POINT('Ctrl Pts',(-10.9319542137566,18.9607797477126,4.62841213584912));
#89823=CARTESIAN_POINT('Ctrl Pts',(-10.9284711232963,18.9610238615502,4.63127979682628));
#89824=CARTESIAN_POINT('Ctrl Pts',(-10.9205854667354,18.9615729843872,4.63771118041038));
#89825=CARTESIAN_POINT('Ctrl Pts',(-10.916175346408,18.9618776168836,4.64126555519157));
#89826=CARTESIAN_POINT('Ctrl Pts',(-10.9041665594707,18.9627005464271,4.65082967305957));
#89827=CARTESIAN_POINT('Ctrl Pts',(-10.8965286005457,18.9632168771588,4.65678977265509));
#89828=CARTESIAN_POINT('Ctrl Pts',(-10.8605850313518,18.9656146365331,4.68426763776586));
#89829=CARTESIAN_POINT('Ctrl Pts',(-10.8315593563729,18.9674587825877,4.70482601898135));
#89830=CARTESIAN_POINT('Ctrl Pts',(-10.6768666882513,18.9768794888153,4.80613585849699));
#89831=CARTESIAN_POINT('Ctrl Pts',(-10.5401525374523,18.9837566537663,4.8683442937853));
#89832=CARTESIAN_POINT('Ctrl Pts',(-10.3670465804022,18.9929137665057,4.91705305941306));
#89833=CARTESIAN_POINT('Ctrl Pts',(-10.3374365873845,18.994498786133,4.92439420731395));
#89834=CARTESIAN_POINT('Ctrl Pts',(-10.3018105211813,18.9964509132998,4.93205376371408));
#89835=CARTESIAN_POINT('Ctrl Pts',(-10.2959925379804,18.9967711333796,4.93326759116886));
#89836=CARTESIAN_POINT('Ctrl Pts',(-10.2869604908855,18.9972706829159,4.93509464214676));
#89837=CARTESIAN_POINT('Ctrl Pts',(-10.283751424121,18.9974486458808,4.93573259492423));
#89838=CARTESIAN_POINT('Ctrl Pts',(-10.2778046587712,18.9977793533087,4.93689407774314));
#89839=CARTESIAN_POINT('Ctrl Pts',(-10.2750675889424,18.9979319301875,4.93742055092653));
#89840=CARTESIAN_POINT('Ctrl Pts',(-10.2688650878725,18.9982785068563,4.93859523278231));
#89841=CARTESIAN_POINT('Ctrl Pts',(-10.2653988252634,18.9984727662671,4.93923873706635));
#89842=CARTESIAN_POINT('Ctrl Pts',(-10.256432914147,18.9989766672973,4.94086974844446));
#89843=CARTESIAN_POINT('Ctrl Pts',(-10.2509299264486,18.9992873297414,4.94183828545735));
#89844=CARTESIAN_POINT('Ctrl Pts',(-10.2163927309197,19.0012451604467,4.94771319515197));
#89845=CARTESIAN_POINT('Ctrl Pts',(-10.1872233581509,19.0029344011007,4.95177356486003));
#89846=CARTESIAN_POINT('Ctrl Pts',(-10.0535486374856,19.0107787775643,4.9662856637501));
#89847=CARTESIAN_POINT('Ctrl Pts',(-9.94822832933526,19.0172197176339,4.96634968180547));
#89848=CARTESIAN_POINT('Ctrl Pts',(-9.79225596596759,19.0265398495859,4.94960780672466));
#89849=CARTESIAN_POINT('Ctrl Pts',(-9.74103198219931,19.0295698839666,4.94133852745841));
#89850=CARTESIAN_POINT('Ctrl Pts',(-9.66085017601027,19.034239965734,4.92398059414231));
#89851=CARTESIAN_POINT('Ctrl Pts',(-9.63155259575886,19.0359310381326,4.91668275754192));
#89852=CARTESIAN_POINT('Ctrl Pts',(-9.59404390717099,19.0380772404299,4.90609711711246));
#89853=CARTESIAN_POINT('Ctrl Pts',(-9.58560927897287,19.0385586326944,4.90363449199275));
#89854=CARTESIAN_POINT('Ctrl Pts',(-9.57196510455479,19.0393354629141,4.89951714745544));
#89855=CARTESIAN_POINT('Ctrl Pts',(-9.56674183718933,19.0396323981674,4.89790896814791));
#89856=CARTESIAN_POINT('Ctrl Pts',(-9.55673517191959,19.0402004335404,4.8947665664988));
#89857=CARTESIAN_POINT('Ctrl Pts',(-9.55195043284844,19.0404716770047,4.89323690343059));
#89858=CARTESIAN_POINT('Ctrl Pts',(-9.54103686331703,19.0410895632117,4.88968584079911));
#89859=CARTESIAN_POINT('Ctrl Pts',(-9.53491331329074,19.0414356797211,4.88764846867514));
#89860=CARTESIAN_POINT('Ctrl Pts',(-9.51871695434973,19.0423497153297,4.88214050717547));
#89861=CARTESIAN_POINT('Ctrl Pts',(-9.50866812255637,19.0429153539751,4.87860028499092));
#89862=CARTESIAN_POINT('Ctrl Pts',(-9.40731908370013,19.0486076081573,4.84164589325476));
#89863=CARTESIAN_POINT('Ctrl Pts',(-9.3195223628312,19.0534120451214,4.79932197213555));
#89864=CARTESIAN_POINT('Ctrl Pts',(-9.16706909048235,19.0621159110974,4.70610666531665));
#89865=CARTESIAN_POINT('Ctrl Pts',(-9.10124840789684,19.0660277432525,4.6578907662122));
#89866=CARTESIAN_POINT('Ctrl Pts',(-9.01515863151058,19.071818597797,4.58304412866461));
#89867=CARTESIAN_POINT('Ctrl Pts',(-8.99125698261388,19.0735101552157,4.56081776065816));
#89868=CARTESIAN_POINT('Ctrl Pts',(-8.96382802089867,19.0755814937634,4.53354560137138));
#89869=CARTESIAN_POINT('Ctrl Pts',(-8.95956273294129,19.0759074976781,4.52925175304407));
#89870=CARTESIAN_POINT('Ctrl Pts',(-8.95301641303678,19.0764141471231,4.52257932615369));
#89871=CARTESIAN_POINT('Ctrl Pts',(-8.95071652498853,19.0765933633167,4.52021924029947));
#89872=CARTESIAN_POINT('Ctrl Pts',(-8.94648741532887,19.0769252113112,4.51585000984714));
#89873=CARTESIAN_POINT('Ctrl Pts',(-8.94455594716732,19.0770776660609,4.51384311387529));
#89874=CARTESIAN_POINT('Ctrl Pts',(-8.94021358505153,19.0774224431619,4.50930531674216));
#89875=CARTESIAN_POINT('Ctrl Pts',(-8.93780603636744,19.0776150135029,4.50677130015311));
#89876=CARTESIAN_POINT('Ctrl Pts',(-8.93164132279362,19.0781116951501,4.50023602879445));
#89877=CARTESIAN_POINT('Ctrl Pts',(-8.92789758245441,19.0784167803251,4.4962222547278));
#89878=CARTESIAN_POINT('Ctrl Pts',(-8.90535140255819,19.0802746575577,4.47177555831482));
#89879=CARTESIAN_POINT('Ctrl Pts',(-8.88711217990929,19.0818648600866,4.45083320471266));
#89880=CARTESIAN_POINT('Ctrl Pts',(-8.8635321302407,19.0840265088872,4.42215008601664));
#89881=CARTESIAN_POINT('Ctrl Pts',(-8.85765306791184,19.0845747830171,4.4148570822684));
#89882=CARTESIAN_POINT('Ctrl Pts',(-8.8512751973173,19.0851795038228,4.40678796896942));
#89883=CARTESIAN_POINT('Ctrl Pts',(-8.85070654763207,19.0852335085463,4.4060671350983));
#89884=CARTESIAN_POINT('Ctrl Pts',(-8.78803853945861,19.0911947704695,4.32647376028324));
#89885=CARTESIAN_POINT('Ctrl Pts',(-8.73421800636294,19.0973404764065,4.24142191718636));
#89886=CARTESIAN_POINT('Ctrl Pts',(-8.65971860638031,19.1072603280742,4.09157493574746));
#89887=CARTESIAN_POINT('Ctrl Pts',(-8.6340581858006,19.1111365537407,4.02964136141409));
#89888=CARTESIAN_POINT('Ctrl Pts',(-8.60775159136329,19.1157433380274,3.95135420443804));
#89889=CARTESIAN_POINT('Ctrl Pts',(-8.60301333184552,19.1166069801966,3.9364682403135));
#89890=CARTESIAN_POINT('Ctrl Pts',(-8.59654270853897,19.1178379467534,3.91495389520153));
#89891=CARTESIAN_POINT('Ctrl Pts',(-8.59461723860037,19.1182114996025,3.90838511271655));
#89892=CARTESIAN_POINT('Ctrl Pts',(-8.59134680292386,19.1188589687067,3.89693084194802));
#89893=CARTESIAN_POINT('Ctrl Pts',(-8.58998100329481,19.1191335535903,3.89205146696607));
#89894=CARTESIAN_POINT('Ctrl Pts',(-8.58739436163082,19.1196618462301,3.88262220393595));
#89895=CARTESIAN_POINT('Ctrl Pts',(-8.58617009497762,19.1199156613013,3.87807332737975));
#89896=CARTESIAN_POINT('Ctrl Pts',(-8.58299832183356,19.120583404227,3.86605742954535));
#89897=CARTESIAN_POINT('Ctrl Pts',(-8.58108785826273,19.1209961414884,3.85858072281213));
#89898=CARTESIAN_POINT('Ctrl Pts',(-8.57454284315463,19.1224487940204,3.83209480668695));
#89899=CARTESIAN_POINT('Ctrl Pts',(-8.57023033370002,19.12347846433,3.81300769267559));
#89900=CARTESIAN_POINT('Ctrl Pts',(-8.54092946320679,19.1310750692854,3.67004308906951));
#89901=CARTESIAN_POINT('Ctrl Pts',(-8.53169769971814,19.1370953083661,3.54348802515119));
#89902=CARTESIAN_POINT('Ctrl Pts',(-8.54166438968115,19.1457266435962,3.36736227577759));
#89903=CARTESIAN_POINT('Ctrl Pts',(-8.54705071643975,19.148202546586,3.31759045860735));
#89904=CARTESIAN_POINT('Ctrl Pts',(-8.55877824828366,19.1520121436158,3.24448312088082));
#89905=CARTESIAN_POINT('Ctrl Pts',(-8.5631650262296,19.153269944864,3.22086895784399));
#89906=CARTESIAN_POINT('Ctrl Pts',(-8.56927640379195,19.154855427326,3.19195300619819));
#89907=CARTESIAN_POINT('Ctrl Pts',(-8.57045306931451,19.1551543153173,3.18653783302719));
#89908=CARTESIAN_POINT('Ctrl Pts',(-8.57235419992102,19.1556276343702,3.17802196037888));
#89909=CARTESIAN_POINT('Ctrl Pts',(-8.57305809094665,19.1558009199294,3.17491666257417));
#89910=CARTESIAN_POINT('Ctrl Pts',(-8.57439986899663,19.1561276532861,3.16908558009046));
#89911=CARTESIAN_POINT('Ctrl Pts',(-8.57503544610246,19.1562809699356,3.16635931527085));
#89912=CARTESIAN_POINT('Ctrl Pts',(-8.57650513764595,19.1566322088916,3.16013598000003));
#89913=CARTESIAN_POINT('Ctrl Pts',(-8.57734431823989,19.1568304159127,3.15664015111482));
#89914=CARTESIAN_POINT('Ctrl Pts',(-8.57960595807513,19.1573583946805,3.14736932954402));
#89915=CARTESIAN_POINT('Ctrl Pts',(-8.58105074023388,19.1576893814363,3.1415999165177));
#89916=CARTESIAN_POINT('Ctrl Pts',(-8.59163331127443,19.1600690277061,3.10040798792131));
#89917=CARTESIAN_POINT('Ctrl Pts',(-8.60206059883461,19.1621824920263,3.06533287829992));
#89918=CARTESIAN_POINT('Ctrl Pts',(-8.61648311195782,19.1648275370238,3.02273297786068));
#89919=CARTESIAN_POINT('Ctrl Pts',(-8.61924481892797,19.1653234336311,3.01480115795194));
#89920=CARTESIAN_POINT('Ctrl Pts',(-8.65469549692082,19.1715562243935,2.91573857354387));
#89921=CARTESIAN_POINT('Ctrl Pts',(-8.69628123895668,19.1774723926981,2.82804431797812));
#89922=CARTESIAN_POINT('Ctrl Pts',(-8.77891485928773,19.1869427957533,2.69080306282505));
#89923=CARTESIAN_POINT('Ctrl Pts',(-8.81509969616742,19.1906019529537,2.63868618083177));
#89924=CARTESIAN_POINT('Ctrl Pts',(-8.86400209389244,19.1949812342604,2.57719372387759));
#89925=CARTESIAN_POINT('Ctrl Pts',(-8.87363474025282,19.195820083828,2.56546054552569));
#89926=CARTESIAN_POINT('Ctrl Pts',(-8.88782299585406,19.197022309762,2.548716472269));
#89927=CARTESIAN_POINT('Ctrl Pts',(-8.8922333446231,19.197391519909,2.54358425458789));
#89928=CARTESIAN_POINT('Ctrl Pts',(-8.89999963880857,19.1980339402669,2.53467259539743));
#89929=CARTESIAN_POINT('Ctrl Pts',(-8.90333983768092,19.1983077894451,2.53087963494174));
#89930=CARTESIAN_POINT('Ctrl Pts',(-8.90984485028935,19.1988364275771,2.52356957022177));
#89931=CARTESIAN_POINT('Ctrl Pts',(-8.91300719940275,19.1990913135192,2.52005036516622));
#89932=CARTESIAN_POINT('Ctrl Pts',(-8.92144544953346,19.1997659187328,2.51075100433232));
#89933=CARTESIAN_POINT('Ctrl Pts',(-8.9267507830111,19.2001843997546,2.50499768079893));
#89934=CARTESIAN_POINT('Ctrl Pts',(-8.94597537156872,19.2016809536736,2.48448240777051));
#89935=CARTESIAN_POINT('Ctrl Pts',(-8.960155438753,19.2027479213745,2.46996736024903));
#89936=CARTESIAN_POINT('Ctrl Pts',(-9.09416318526745,19.212513616109,2.33838270915207));
#89937=CARTESIAN_POINT('Ctrl Pts',(-9.23293114521216,19.2201624705963,2.24242743545717));
#89938=CARTESIAN_POINT('Ctrl Pts',(-9.41337924357198,19.2302757766424,2.1588463684646));
#89939=CARTESIAN_POINT('Ctrl Pts',(-9.44226829587132,19.2319048116769,2.14657765513481));
#89940=CARTESIAN_POINT('Ctrl Pts',(-9.47711248687387,19.2339061901083,2.13308494326703));
#89941=CARTESIAN_POINT('Ctrl Pts',(-9.48271094969269,19.2342288598946,2.13095647999957));
#89942=CARTESIAN_POINT('Ctrl Pts',(-9.49139696378548,19.2347314172632,2.12771505430884));
#89943=CARTESIAN_POINT('Ctrl Pts',(-9.49447552512786,19.2349099118896,2.12657798711041));
#89944=CARTESIAN_POINT('Ctrl Pts',(-9.50017494028386,19.2352410997588,2.12449466596413));
#89945=CARTESIAN_POINT('Ctrl Pts',(-9.50279468647932,19.2353936213885,2.12354553648829));
#89946=CARTESIAN_POINT('Ctrl Pts',(-9.50872299227258,19.235739419123,2.12141685435759));
#89947=CARTESIAN_POINT('Ctrl Pts',(-9.51203307970919,19.2359329498355,2.12024173423697));
#89948=CARTESIAN_POINT('Ctrl Pts',(-9.52057935936852,19.2364337326745,2.11724230420256));
#89949=CARTESIAN_POINT('Ctrl Pts',(-9.52582169825958,19.2367419852226,2.11543583315469));
#89950=CARTESIAN_POINT('Ctrl Pts',(-9.55827193135465,19.2386561109895,2.10445963208981));
#89951=CARTESIAN_POINT('Ctrl Pts',(-9.58573282842601,19.2403019849419,2.09606300294355));
#89952=CARTESIAN_POINT('Ctrl Pts',(-9.75525735872894,19.2505468179804,2.04963458489905));
#89953=CARTESIAN_POINT('Ctrl Pts',(-9.90214634706315,19.2596741607257,2.03238455393682));
#89954=CARTESIAN_POINT('Ctrl Pts',(-10.0885523410539,19.2704053424228,2.03864992541802));
#89955=CARTESIAN_POINT('Ctrl Pts',(-10.1278748760657,19.2726288003457,2.04156454008032));
#89956=CARTESIAN_POINT('Ctrl Pts',(-10.1765625422358,19.2753323780346,2.04715799267027));
#89957=CARTESIAN_POINT('Ctrl Pts',(-10.1860796339814,19.2758585277891,2.04834625149376));
#89958=CARTESIAN_POINT('Ctrl Pts',(-10.2011765746972,19.2766895919647,2.05038209326492));
#89959=CARTESIAN_POINT('Ctrl Pts',(-10.2067642747135,19.276996408987,2.05116853095995));
#89960=CARTESIAN_POINT('Ctrl Pts',(-10.2172800088412,19.2775723958659,2.05271063632221));
#89961=CARTESIAN_POINT('Ctrl Pts',(-10.2222089888003,19.2778417837619,2.0534592053439));
#89962=CARTESIAN_POINT('Ctrl Pts',(-10.2332996623311,19.2784466382635,2.05520158150741));
#89963=CARTESIAN_POINT('Ctrl Pts',(-10.2394590390122,19.2787816522177,2.05620965067414));
#89964=CARTESIAN_POINT('Ctrl Pts',(-10.2551924009508,19.2796351936729,2.05888809050786));
#89965=CARTESIAN_POINT('Ctrl Pts',(-10.2647566218842,19.2801519574655,2.06061449416049));
#89966=CARTESIAN_POINT('Ctrl Pts',(-10.3235700280896,19.2833177802144,2.07183674237607));
#89967=CARTESIAN_POINT('Ctrl Pts',(-10.3723237665449,19.2858888397729,2.08376430349396));
#89968=CARTESIAN_POINT('Ctrl Pts',(-10.5485961943378,19.2951170768274,2.13662394302789));
#89969=CARTESIAN_POINT('Ctrl Pts',(-10.6709215073448,19.3013339623607,2.19247949114761));
#89970=CARTESIAN_POINT('Ctrl Pts',(-10.8087960320802,19.3096615597938,2.27993951042481));
#89971=CARTESIAN_POINT('Ctrl Pts',(-10.8331682471934,19.3111930592952,2.29645147229864));
#89972=CARTESIAN_POINT('Ctrl Pts',(-10.8617947014911,19.3130852928861,2.31713197074493));
#89973=CARTESIAN_POINT('Ctrl Pts',(-10.8665441021854,19.3134024136174,2.32060685148671));
#89974=CARTESIAN_POINT('Ctrl Pts',(-10.8738910568082,19.3138981562282,2.32605055754707));
#89975=CARTESIAN_POINT('Ctrl Pts',(-10.8765032636626,19.3140754447768,2.32799961562743));
#89976=CARTESIAN_POINT('Ctrl Pts',(-10.88133830005,19.3144055503658,2.3316324093787));
#89977=CARTESIAN_POINT('Ctrl Pts',(-10.8835628398947,19.3145582049613,2.33331378103655));
#89978=CARTESIAN_POINT('Ctrl Pts',(-10.8886025084914,19.314905804154,2.33714558902756));
#89979=CARTESIAN_POINT('Ctrl Pts',(-10.8914146307227,19.3151010149067,2.33929988592921));
#89980=CARTESIAN_POINT('Ctrl Pts',(-10.8999555181905,19.315697651573,2.3458921929956));
#89981=CARTESIAN_POINT('Ctrl Pts',(-10.9056590770935,19.3161012476319,2.3503624934034));
#89982=CARTESIAN_POINT('Ctrl Pts',(-10.9604902932024,19.3200295040541,2.39399901880944));
#89983=CARTESIAN_POINT('Ctrl Pts',(-11.0070762572335,19.3237421819597,2.43624459523901));
#89984=CARTESIAN_POINT('Ctrl Pts',(-11.1311819647378,19.3344240649125,2.56426674279092));
#89985=CARTESIAN_POINT('Ctrl Pts',(-11.2014805075467,19.3414422403673,2.65642386488544));
#89986=CARTESIAN_POINT('Ctrl Pts',(-11.2721345744582,19.3494031036046,2.77608315948565));
#89987=CARTESIAN_POINT('Ctrl Pts',(-11.2835691043462,19.3507305312622,2.796556747927));
#89988=CARTESIAN_POINT('Ctrl Pts',(-11.3023707265818,19.3529831670557,2.83220744705339));
#89989=CARTESIAN_POINT('Ctrl Pts',(-11.3099762370591,19.3539164019355,2.84725296249905));
#89990=CARTESIAN_POINT('Ctrl Pts',(-11.3203946098345,19.3552275371098,2.86877886449836));
#89991=CARTESIAN_POINT('Ctrl Pts',(-11.3234229301527,19.3556128386323,2.87515298034299));
#89992=CARTESIAN_POINT('Ctrl Pts',(-11.3285619102496,19.3562740849912,2.88617465766563));
#89993=CARTESIAN_POINT('Ctrl Pts',(-11.3306945591667,19.3565507798328,2.89081177672277));
#89994=CARTESIAN_POINT('Ctrl Pts',(-11.3347288783223,19.3570786491562,2.8997060638848));
#89995=CARTESIAN_POINT('Ctrl Pts',(-11.3366345449189,19.3573299573574,2.90396134153322));
#89996=CARTESIAN_POINT('Ctrl Pts',(-11.341054118556,19.3579174673861,2.91395786716575));
#89997=CARTESIAN_POINT('Ctrl Pts',(-11.3435515561416,19.3582531088152,2.91970632607008));
#89998=CARTESIAN_POINT('Ctrl Pts',(-11.3520025916107,19.3594017330883,2.93950548259117));
#89999=CARTESIAN_POINT('Ctrl Pts',(-11.3577734314809,19.360208581783,2.95363341647211));
#90000=CARTESIAN_POINT('Ctrl Pts',(-11.4107130486128,19.3678399690638,3.08925999274087));
#90001=CARTESIAN_POINT('Ctrl Pts',(-11.4416727951722,19.3740590932737,3.21645087969917));
#90002=CARTESIAN_POINT('Ctrl Pts',(-11.4607906234388,19.382943268054,3.39720327065946));
#90003=CARTESIAN_POINT('Ctrl Pts',(-11.4635,19.385483219807,3.44858563713104));
#90004=CARTESIAN_POINT('Ctrl Pts',(-11.4635,19.3881255777082,3.49999999999758));
#90005=CARTESIAN_POINT('Origin',(-10.,13.2,3.5));
#90006=CARTESIAN_POINT('',(-11.4635,19.9607369088795,3.50000000007519));
#90007=CARTESIAN_POINT('',(-11.4635,19.889530718258,3.4999999999448));
#90008=CARTESIAN_POINT('',(-11.4635,13.2,3.5));
#90009=CARTESIAN_POINT('',(-11.4634994221272,19.9606728854432,3.49868359318153));
#90010=CARTESIAN_POINT('Ctrl Pts',(-11.4635,19.9607369088795,3.50000000007519));
#90011=CARTESIAN_POINT('Ctrl Pts',(-11.4635,19.9607155759167,3.49956121929246));
#90012=CARTESIAN_POINT('Ctrl Pts',(-11.4634998026698,19.9606942428785,3.49912243308542));
#90013=CARTESIAN_POINT('Ctrl Pts',(-11.4634994079946,19.9606729097263,3.49868364158582));
#90014=CARTESIAN_POINT('Ctrl Pts',(-11.4634994079501,19.9606729073219,3.49868359213058));
#90015=CARTESIAN_POINT('Ctrl Pts',(-11.4634137445551,19.956042766607,3.40344842169157));
#90016=CARTESIAN_POINT('Ctrl Pts',(-11.4540323528043,19.9514432767397,3.30845726190788));
#90017=CARTESIAN_POINT('Ctrl Pts',(-11.4341658037668,19.9460401280826,3.20837143954945));
#90018=CARTESIAN_POINT('Ctrl Pts',(-11.4327911374842,19.9456767153169,3.20169089370002));
#90019=CARTESIAN_POINT('Ctrl Pts',(-11.4302108123229,19.945012514577,3.18958057969233));
#90020=CARTESIAN_POINT('Ctrl Pts',(-11.4290207932211,19.9447125498405,3.18414757444547));
#90021=CARTESIAN_POINT('Ctrl Pts',(-11.4271000238858,19.9442379420016,3.17561144520711));
#90022=CARTESIAN_POINT('Ctrl Pts',(-11.4263900407649,19.9440644553884,3.17250364297565));
#90023=CARTESIAN_POINT('Ctrl Pts',(-11.4250379589305,19.9437376275442,3.1666729956909));
#90024=CARTESIAN_POINT('Ctrl Pts',(-11.4243982041104,19.9435844194613,3.16394965871794));
#90025=CARTESIAN_POINT('Ctrl Pts',(-11.4229205617866,19.9432337999986,3.15773959600882));
#90026=CARTESIAN_POINT('Ctrl Pts',(-11.4220776655418,19.9430361070718,3.15425410790757));
#90027=CARTESIAN_POINT('Ctrl Pts',(-11.4198096605747,19.9425102691521,3.14502421632571));
#90028=CARTESIAN_POINT('Ctrl Pts',(-11.4183625154802,19.9421809238922,3.13928535998554));
#90029=CARTESIAN_POINT('Ctrl Pts',(-11.4079209669034,19.9398478477394,3.09891245365048));
#90030=CARTESIAN_POINT('Ctrl Pts',(-11.3976944448366,19.9377821047575,3.06461223919841));
#90031=CARTESIAN_POINT('Ctrl Pts',(-11.38183488504,19.9348756600818,3.01776372784465));
#90032=CARTESIAN_POINT('Ctrl Pts',(-11.3772659615998,19.9340663509738,3.00486574745594));
#90033=CARTESIAN_POINT('Ctrl Pts',(-11.3597237666308,19.9310626316199,2.95746698529145));
#90034=CARTESIAN_POINT('Ctrl Pts',(-11.3456295550546,19.9288454497048,2.92339634274777));
#90035=CARTESIAN_POINT('Ctrl Pts',(-11.310057537937,19.9237069969352,2.84583561283726));
#90036=CARTESIAN_POINT('Ctrl Pts',(-11.2876733885248,19.9207877383682,2.80280611264914));
#90037=CARTESIAN_POINT('Ctrl Pts',(-11.2361885363111,19.9147338877698,2.71480560047531));
#90038=CARTESIAN_POINT('Ctrl Pts',(-11.2066706959746,19.9116131402043,2.67015719906115));
#90039=CARTESIAN_POINT('Ctrl Pts',(-11.1581488717457,19.90699428837,2.60484614158327));
#90040=CARTESIAN_POINT('Ctrl Pts',(-11.1408889258023,19.9054352779286,2.58294937543069));
#90041=CARTESIAN_POINT('Ctrl Pts',(-11.1189225181921,19.9035496118399,2.55666265585356));
#90042=CARTESIAN_POINT('Ctrl Pts',(-11.1147998470305,19.9031997514125,2.55179419457049));
#90043=CARTESIAN_POINT('Ctrl Pts',(-11.1067320421034,19.9025228395713,2.54239227767872));
#90044=CARTESIAN_POINT('Ctrl Pts',(-11.1027905640002,19.9021956490416,2.53785586509849));
#90045=CARTESIAN_POINT('Ctrl Pts',(-11.0955700654623,19.9016025554382,2.52964815168607));
#90046=CARTESIAN_POINT('Ctrl Pts',(-11.0923002658052,19.901336278605,2.52596888755771));
#90047=CARTESIAN_POINT('Ctrl Pts',(-11.0851397353979,19.9007581160934,2.51799307471616));
#90048=CARTESIAN_POINT('Ctrl Pts',(-11.081241906057,19.9004465325133,2.51370299171305));
#90049=CARTESIAN_POINT('Ctrl Pts',(-11.0705330424237,19.8995989211419,2.50205623276338));
#90050=CARTESIAN_POINT('Ctrl Pts',(-11.0636716705296,19.8990650220827,2.49474613082253));
#90051=CARTESIAN_POINT('Ctrl Pts',(-11.0284196591286,19.8963672211087,2.45795372319157));
#90052=CARTESIAN_POINT('Ctrl Pts',(-10.9988750550461,19.8942536648422,2.42959986209388));
#90053=CARTESIAN_POINT('Ctrl Pts',(-10.9580828980211,19.8914994527891,2.39361369338931));
#90054=CARTESIAN_POINT('Ctrl Pts',(-10.9478645134338,19.8908222990557,2.38484692783403));
#90055=CARTESIAN_POINT('Ctrl Pts',(-10.878613658334,19.8863120066616,2.32707348482156));
#90056=CARTESIAN_POINT('Ctrl Pts',(-10.8159256284579,19.8826145921874,2.28263220323446));
#90057=CARTESIAN_POINT('Ctrl Pts',(-10.7006323312488,19.8760710428404,2.21382052309578));
#90058=CARTESIAN_POINT('Ctrl Pts',(-10.6495288245896,19.8732464083486,2.18727202957116));
#90059=CARTESIAN_POINT('Ctrl Pts',(-10.5731768054225,19.8689588293042,2.15315873190921));
#90060=CARTESIAN_POINT('Ctrl Pts',(-10.5490753068879,19.8675958605482,2.14315469114894));
#90061=CARTESIAN_POINT('Ctrl Pts',(-10.519523059989,19.8658985816823,2.13180445748483));
#90062=CARTESIAN_POINT('Ctrl Pts',(-10.5143139991395,19.8655984397398,2.12983783415813));
#90063=CARTESIAN_POINT('Ctrl Pts',(-10.5060393396881,19.8651199401288,2.12676766289083));
#90064=CARTESIAN_POINT('Ctrl Pts',(-10.5029810063627,19.8649427147344,2.12564452494672));
#90065=CARTESIAN_POINT('Ctrl Pts',(-10.4972990851735,19.8646127254945,2.12357941005239));
#90066=CARTESIAN_POINT('Ctrl Pts',(-10.4946765425452,19.8644601239696,2.12263471133655));
#90067=CARTESIAN_POINT('Ctrl Pts',(-10.4887162388068,19.8641126474312,2.12050689445962));
#90068=CARTESIAN_POINT('Ctrl Pts',(-10.4853768872018,19.863917506455,2.1193283999687));
#90069=CARTESIAN_POINT('Ctrl Pts',(-10.4751935299055,19.863321091338,2.11577608936369));
#90070=CARTESIAN_POINT('Ctrl Pts',(-10.4683362538154,19.8629176486511,2.11344099491087));
#90071=CARTESIAN_POINT('Ctrl Pts',(-10.4019544400507,19.8589964636457,2.09138473063548));
#90072=CARTESIAN_POINT('Ctrl Pts',(-10.341243309482,19.8552914177431,2.07545946536196));
#90073=CARTESIAN_POINT('Ctrl Pts',(-10.1662376355533,19.8446107443839,2.04138409722124));
#90074=CARTESIAN_POINT('Ctrl Pts',(-10.0505327944258,19.8375852254356,2.03280931865867));
#90075=CARTESIAN_POINT('Ctrl Pts',(-9.91158568035819,19.8296172167755,2.03898481855261));
#90076=CARTESIAN_POINT('Ctrl Pts',(-9.88817999193968,19.8282891892406,2.04058956244162));
#90077=CARTESIAN_POINT('Ctrl Pts',(-9.848032610309,19.826035703083,2.04431374517357));
#90078=CARTESIAN_POINT('Ctrl Pts',(-9.83127090189589,19.8251022078473,2.04616125897734));
#90079=CARTESIAN_POINT('Ctrl Pts',(-9.8075451563331,19.82379085329,2.04919223485169));
#90080=CARTESIAN_POINT('Ctrl Pts',(-9.80055243369569,19.8234055874896,2.05013700336749));
#90081=CARTESIAN_POINT('Ctrl Pts',(-9.78851523630969,19.8227444542812,2.05185205164295));
#90082=CARTESIAN_POINT('Ctrl Pts',(-9.78346749742927,19.822467836695,2.05259820303716));
#90083=CARTESIAN_POINT('Ctrl Pts',(-9.7738169798387,19.8219401503499,2.05407634665203));
#90084=CARTESIAN_POINT('Ctrl Pts',(-9.76921360123617,19.8216889477474,2.05480395490498));
#90085=CARTESIAN_POINT('Ctrl Pts',(-9.75843155802166,19.8211017384344,2.05656099118922));
#90086=CARTESIAN_POINT('Ctrl Pts',(-9.75225584398058,19.8207662912435,2.0576081256702));
#90087=CARTESIAN_POINT('Ctrl Pts',(-9.73107243551469,19.819618601982,2.06133998177758));
#90088=CARTESIAN_POINT('Ctrl Pts',(-9.71609979308382,19.8188124819635,2.06421959252592));
#90089=CARTESIAN_POINT('Ctrl Pts',(-9.57352180475279,19.8111780721326,2.09395848544571));
#90090=CARTESIAN_POINT('Ctrl Pts',(-9.45000568237654,19.8049559802393,2.13752264926429));
#90091=CARTESIAN_POINT('Ctrl Pts',(-9.28793193910559,19.7960589220608,2.22036909480593));
#90092=CARTESIAN_POINT('Ctrl Pts',(-9.24325251606778,19.7935092898169,2.24627406565687));
#90093=CARTESIAN_POINT('Ctrl Pts',(-9.17954064616634,19.7895976833154,2.28786227981394));
#90094=CARTESIAN_POINT('Ctrl Pts',(-9.15938345317736,19.7883164287226,2.30175332866223));
#90095=CARTESIAN_POINT('Ctrl Pts',(-9.13507714125785,19.7867046767838,2.31941889017696));
#90096=CARTESIAN_POINT('Ctrl Pts',(-9.13058783459079,19.7864041191722,2.32272102156282));
#90097=CARTESIAN_POINT('Ctrl Pts',(-9.12355842121665,19.7859287816161,2.32795367527048));
#90098=CARTESIAN_POINT('Ctrl Pts',(-9.12100553274142,19.7857551640983,2.329867035563));
#90099=CARTESIAN_POINT('Ctrl Pts',(-9.116226226158,19.7854282311601,2.33347353636971));
#90100=CARTESIAN_POINT('Ctrl Pts',(-9.11399839475503,19.7852750499323,2.33516472034014));
#90101=CARTESIAN_POINT('Ctrl Pts',(-9.10892851882197,19.7849246743868,2.33903630686234));
#90102=CARTESIAN_POINT('Ctrl Pts',(-9.10608962539454,19.7847271999829,2.34122076176553));
#90103=CARTESIAN_POINT('Ctrl Pts',(-9.09859191401106,19.7842023209756,2.34703400511823));
#90104=CARTESIAN_POINT('Ctrl Pts',(-9.09394703981038,19.783873722902,2.35068056930586));
#90105=CARTESIAN_POINT('Ctrl Pts',(-9.06144994665411,19.7815512663168,2.37651257704863));
#90106=CARTESIAN_POINT('Ctrl Pts',(-9.03439550496941,19.7794959846328,2.39967834202384));
#90107=CARTESIAN_POINT('Ctrl Pts',(-8.93277701436523,19.7713770799739,2.49332656360102));
#90108=CARTESIAN_POINT('Ctrl Pts',(-8.86485773304225,19.7650917927627,2.57058649450229));
#90109=CARTESIAN_POINT('Ctrl Pts',(-8.76714163505637,19.7550710224111,2.70859861163956));
#90110=CARTESIAN_POINT('Ctrl Pts',(-8.73245005455498,19.7512217740035,2.76544237865106));
#90111=CARTESIAN_POINT('Ctrl Pts',(-8.69455815663255,19.7466432912847,2.8382628181346));
#90112=CARTESIAN_POINT('Ctrl Pts',(-8.68759418546321,19.745782796896,2.85218404731595));
#90113=CARTESIAN_POINT('Ctrl Pts',(-8.67789397716318,19.7445555504022,2.87237382561336));
#90114=CARTESIAN_POINT('Ctrl Pts',(-8.67497767910233,19.7441826199879,2.87855426484827));
#90115=CARTESIAN_POINT('Ctrl Pts',(-8.66997603532699,19.7435359490749,2.88934940957531));
#90116=CARTESIAN_POINT('Ctrl Pts',(-8.66787116848844,19.7432615437805,2.89395489661097));
#90117=CARTESIAN_POINT('Ctrl Pts',(-8.66385410917567,19.7427333999446,2.90286634263372));
#90118=CARTESIAN_POINT('Ctrl Pts',(-8.66193872644397,19.7424795553122,2.90717078745172));
#90119=CARTESIAN_POINT('Ctrl Pts',(-8.65744415039595,19.7418790130687,2.9174042186559));
#90120=CARTESIAN_POINT('Ctrl Pts',(-8.65488338383103,19.7415329413859,2.92334122353582));
#90121=CARTESIAN_POINT('Ctrl Pts',(-8.64595508593005,19.7403121028983,2.94442412070779));
#90122=CARTESIAN_POINT('Ctrl Pts',(-8.63980321477142,19.7394445631679,2.95966036508148));
#90123=CARTESIAN_POINT('Ctrl Pts',(-8.59140912326885,19.732387321404,3.08558494065421));
#90124=CARTESIAN_POINT('Ctrl Pts',(-8.56249427169595,19.7266807330681,3.20092154506376));
#90125=CARTESIAN_POINT('Ctrl Pts',(-8.54043625200066,19.718018778119,3.37740081448873));
#90126=CARTESIAN_POINT('Ctrl Pts',(-8.53666505748933,19.715109854666,3.43670081049282));
#90127=CARTESIAN_POINT('Ctrl Pts',(-8.53643367992204,19.7107054397737,3.52267295556827));
#90128=CARTESIAN_POINT('Ctrl Pts',(-8.53708792427982,19.7093161068906,3.54928000082999));
#90129=CARTESIAN_POINT('Ctrl Pts',(-8.53876325220548,19.7075831411918,3.58156029283086));
#90130=CARTESIAN_POINT('Ctrl Pts',(-8.53909290005057,19.7072750264397,3.58726601642025));
#90131=CARTESIAN_POINT('Ctrl Pts',(-8.53966060707512,19.7067903910223,3.5961846457714));
#90132=CARTESIAN_POINT('Ctrl Pts',(-8.53987587326326,19.7066151096075,3.59939900764801));
#90133=CARTESIAN_POINT('Ctrl Pts',(-8.54029751129362,19.7062868036667,3.60539777016742));
#90134=CARTESIAN_POINT('Ctrl Pts',(-8.5405012387892,19.7061339264532,3.60818230491921));
#90135=CARTESIAN_POINT('Ctrl Pts',(-8.5409853945846,19.7057832689559,3.61454930745263));
#90136=CARTESIAN_POINT('Ctrl Pts',(-8.54127104922889,19.7055852026814,3.61813132636036));
#90137=CARTESIAN_POINT('Ctrl Pts',(-8.54205344756484,19.705064803885,3.62750650098825));
#90138=CARTESIAN_POINT('Ctrl Pts',(-8.54257152351526,19.7047413389941,3.63329775388379));
#90139=CARTESIAN_POINT('Ctrl Pts',(-8.54633798821459,19.7025248119698,3.67275021392144));
#90140=CARTESIAN_POINT('Ctrl Pts',(-8.55071754288131,19.7005762988811,3.70629079347159));
#90141=CARTESIAN_POINT('Ctrl Pts',(-8.57274777077938,19.6926873348225,3.83901128282558));
#90142=CARTESIAN_POINT('Ctrl Pts',(-8.59945464158742,19.6865190039527,3.93640689355828));
#90143=CARTESIAN_POINT('Ctrl Pts',(-8.66123117777454,19.6763924792935,4.09531280814216));
#90144=CARTESIAN_POINT('Ctrl Pts',(-8.69112913346795,19.6723451386725,4.1584515761339));
#90145=CARTESIAN_POINT('Ctrl Pts',(-8.73326238610005,19.6675603275407,4.23311842180967));
#90146=CARTESIAN_POINT('Ctrl Pts',(-8.7413300823713,19.6666778858602,4.24688477668963));
#90147=CARTESIAN_POINT('Ctrl Pts',(-8.75320814921338,19.6654252674149,4.26641370531577));
#90148=CARTESIAN_POINT('Ctrl Pts',(-8.75683650109319,19.6650485541611,4.2722851831776));
#90149=CARTESIAN_POINT('Ctrl Pts',(-8.76320472565336,19.6643974671863,4.28242920238383));
#90150=CARTESIAN_POINT('Ctrl Pts',(-8.76592551748704,19.6641224026863,4.28671353102732));
#90151=CARTESIAN_POINT('Ctrl Pts',(-8.7712058238074,19.6635944820704,4.29493343177462));
#90152=CARTESIAN_POINT('Ctrl Pts',(-8.77376209275742,19.6633415111051,4.29887100582407));
#90153=CARTESIAN_POINT('Ctrl Pts',(-8.77984790768838,19.6627453224624,4.30814731333391));
#90154=CARTESIAN_POINT('Ctrl Pts',(-8.78339363028139,19.662402708906,4.31347535386647));
#90155=CARTESIAN_POINT('Ctrl Pts',(-8.79594833690625,19.6612058817682,4.33207520032044));
#90156=CARTESIAN_POINT('Ctrl Pts',(-8.8051406373841,19.6603585221528,4.34522226464615));
#90157=CARTESIAN_POINT('Ctrl Pts',(-8.88672891227969,19.6530754119513,4.45792004475657));
#90158=CARTESIAN_POINT('Ctrl Pts',(-8.9711972824844,19.6471681364316,4.54811767146009));
#90159=CARTESIAN_POINT('Ctrl Pts',(-9.10927710602421,19.6384223693583,4.66258765575071));
#90160=CARTESIAN_POINT('Ctrl Pts',(-9.15461998962888,19.6356570423598,4.69596367807828));
#90161=CARTESIAN_POINT('Ctrl Pts',(-9.22337796836966,19.6314486811779,4.74070755531096));
#90162=CARTESIAN_POINT('Ctrl Pts',(-9.24535484239603,19.6301012552783,4.75419597445641));
#90163=CARTESIAN_POINT('Ctrl Pts',(-9.27257698301564,19.6284152641202,4.76992915519647));
#90164=CARTESIAN_POINT('Ctrl Pts',(-9.27749519327278,19.62810999518,4.77273371409891));
#90165=CARTESIAN_POINT('Ctrl Pts',(-9.28522700281274,19.6276288602635,4.77708344112295));
#90166=CARTESIAN_POINT('Ctrl Pts',(-9.28802967658596,19.6274542043595,4.77864804042013));
#90167=CARTESIAN_POINT('Ctrl Pts',(-9.29328133325388,19.6271264224067,4.78155717054276));
#90168=CARTESIAN_POINT('Ctrl Pts',(-9.29572903096472,19.6269734387705,4.78290391574854));
#90169=CARTESIAN_POINT('Ctrl Pts',(-9.30134956332321,19.626621677513,4.78597545041253));
#90170=CARTESIAN_POINT('Ctrl Pts',(-9.30452492844998,19.6264226070416,4.78769550593635));
#90171=CARTESIAN_POINT('Ctrl Pts',(-9.312882000565,19.6258978590131,4.7921824991193));
#90172=CARTESIAN_POINT('Ctrl Pts',(-9.31807400404919,19.6255710189273,4.79492999419432));
#90173=CARTESIAN_POINT('Ctrl Pts',(-9.35435626943737,19.6232820160773,4.81385106239168));
#90174=CARTESIAN_POINT('Ctrl Pts',(-9.38599995462256,19.6212603318344,4.82893340745466));
#90175=CARTESIAN_POINT('Ctrl Pts',(-9.42647382145323,19.6186703599349,4.84647028659164));
#90176=CARTESIAN_POINT('Ctrl Pts',(-9.43482917189611,19.6181354607806,4.84999868171311));
#90177=CARTESIAN_POINT('Ctrl Pts',(-9.53192056583963,19.6119211107036,4.88994024236719));
#90178=CARTESIAN_POINT('Ctrl Pts',(-9.62399757590105,19.6060601650186,4.91762324028468));
#90179=CARTESIAN_POINT('Ctrl Pts',(-9.78189222149721,19.5965359725163,4.94861458435281));
#90180=CARTESIAN_POINT('Ctrl Pts',(-9.8464282850424,19.5927793476797,4.95687085410545));
#90181=CARTESIAN_POINT('Ctrl Pts',(-9.92665579746746,19.5882978209831,4.96174188744806));
#90182=CARTESIAN_POINT('Ctrl Pts',(-9.94201915791696,19.587447841252,4.9624318667499));
#90183=CARTESIAN_POINT('Ctrl Pts',(-9.96418876775474,19.5862327767526,4.96307759704093));
#90184=CARTESIAN_POINT('Ctrl Pts',(-9.97098794581049,19.5858616818992,4.96322821262309));
#90185=CARTESIAN_POINT('Ctrl Pts',(-9.98284556306865,19.5852171469707,4.96340820007504));
#90186=CARTESIAN_POINT('Ctrl Pts',(-9.98790352509332,19.5849430546479,4.96345874931301));
#90187=CARTESIAN_POINT('Ctrl Pts',(-9.9976815048502,19.5844147732169,4.96350577440856));
#90188=CARTESIAN_POINT('Ctrl Pts',(-10.0024014371083,19.5841604823555,4.96350564090653));
#90189=CARTESIAN_POINT('Ctrl Pts',(-10.0136200536952,19.5835577342547,4.96345105098093));
#90190=CARTESIAN_POINT('Ctrl Pts',(-10.0201185694611,19.5832099140434,4.96337614080986));
#90191=CARTESIAN_POINT('Ctrl Pts',(-10.0432431867641,19.5819767828504,4.96295550748489));
#90192=CARTESIAN_POINT('Ctrl Pts',(-10.0598639858717,19.5810988942023,4.9623696943485));
#90193=CARTESIAN_POINT('Ctrl Pts',(-10.1918530276353,19.5741869576191,4.95546349157989));
#90194=CARTESIAN_POINT('Ctrl Pts',(-10.3061122785802,19.5686086371621,4.93578530808741));
#90195=CARTESIAN_POINT('Ctrl Pts',(-10.4757500310807,19.5599949949133,4.88537590617138));
#90196=CARTESIAN_POINT('Ctrl Pts',(-10.5334606689696,19.5569917345533,4.86419323565645));
#90197=CARTESIAN_POINT('Ctrl Pts',(-10.6145044553621,19.5524591462504,4.82851535953255));
#90198=CARTESIAN_POINT('Ctrl Pts',(-10.6390327584642,19.5510431795133,4.81689245328271));
#90199=CARTESIAN_POINT('Ctrl Pts',(-10.6683463656569,19.5492803730599,4.80199018009279));
#90200=CARTESIAN_POINT('Ctrl Pts',(-10.6734550912476,19.5489705023101,4.79935504440227));
#90201=CARTESIAN_POINT('Ctrl Pts',(-10.6814088694462,19.54848370746,4.79519289215716));
#90202=CARTESIAN_POINT('Ctrl Pts',(-10.6842646741082,19.5483080407645,4.7936864112331));
#90203=CARTESIAN_POINT('Ctrl Pts',(-10.6895797389374,19.5479794076285,4.79086010998411));
#90204=CARTESIAN_POINT('Ctrl Pts',(-10.6920402213336,19.5478265915004,4.78954269861279));
#90205=CARTESIAN_POINT('Ctrl Pts',(-10.6976504905862,19.5474765936178,4.78651812209661));
#90206=CARTESIAN_POINT('Ctrl Pts',(-10.7007977770161,19.5472791299922,4.7848064292587));
#90207=CARTESIAN_POINT('Ctrl Pts',(-10.7090049861787,19.5467613357898,4.78030370318974));
#90208=CARTESIAN_POINT('Ctrl Pts',(-10.7140546686712,19.5464398907297,4.77749425467367));
#90209=CARTESIAN_POINT('Ctrl Pts',(-10.7479026614091,19.5442666412832,4.75839915218622));
#90210=CARTESIAN_POINT('Ctrl Pts',(-10.7761562413337,19.5423617532052,4.74117201757062));
#90211=CARTESIAN_POINT('Ctrl Pts',(-10.8193709285459,19.5393318979977,4.71276985944076));
#90212=CARTESIAN_POINT('Ctrl Pts',(-10.8347449692665,19.5382298450131,4.70223968055702));
#90213=CARTESIAN_POINT('Ctrl Pts',(-10.9129777569391,19.5325109077971,4.64643137033179));
#90214=CARTESIAN_POINT('Ctrl Pts',(-10.972370871376,19.5278002291315,4.59650743157249));
#90215=CARTESIAN_POINT('Ctrl Pts',(-11.0860126013559,19.518292613268,4.48445584413692));
#90216=CARTESIAN_POINT('Ctrl Pts',(-11.1395405602359,19.5135267088618,4.42196936214456));
#90217=CARTESIAN_POINT('Ctrl Pts',(-11.1942331072658,19.5083448190035,4.34603211461871));
#90218=CARTESIAN_POINT('Ctrl Pts',(-11.2008083000543,19.5077156784156,4.33667346702114));
#90219=CARTESIAN_POINT('Ctrl Pts',(-11.2106867920785,19.5067606859864,4.32225677950704));
#90220=CARTESIAN_POINT('Ctrl Pts',(-11.2140695043242,19.5064318503367,4.31725391412741));
#90221=CARTESIAN_POINT('Ctrl Pts',(-11.2199122772675,19.5058606321388,4.30849640230696));
#90222=CARTESIAN_POINT('Ctrl Pts',(-11.2223861941975,19.5056177340641,4.30475113521458));
#90223=CARTESIAN_POINT('Ctrl Pts',(-11.2279167792504,19.5050723460416,4.29629402661117));
#90224=CARTESIAN_POINT('Ctrl Pts',(-11.2309636427519,19.5047702220696,4.29157583655084));
#90225=CARTESIAN_POINT('Ctrl Pts',(-11.2390783965571,19.5039609896041,4.27884965535902));
#90226=CARTESIAN_POINT('Ctrl Pts',(-11.2440958382738,19.5034557362017,4.27080971019543));
#90227=CARTESIAN_POINT('Ctrl Pts',(-11.2664278807289,19.5011837549075,4.23423869191108));
#90228=CARTESIAN_POINT('Ctrl Pts',(-11.2828422439138,19.4994496066057,4.2051680883371));
#90229=CARTESIAN_POINT('Ctrl Pts',(-11.3076118965672,19.4967086028152,4.15756731916387));
#90230=CARTESIAN_POINT('Ctrl Pts',(-11.316599815457,19.4956835424412,4.13938143373197));
#90231=CARTESIAN_POINT('Ctrl Pts',(-11.3815681658965,19.4880135176368,4.00074285838403));
#90232=CARTESIAN_POINT('Ctrl Pts',(-11.4212877154875,19.481841213713,3.87337494196798));
#90233=CARTESIAN_POINT('Ctrl Pts',(-11.4481455384831,19.4735699988697,3.71346696718282));
#90234=CARTESIAN_POINT('Ctrl Pts',(-11.4521348330697,19.4720427424521,3.68438503750852));
#90235=CARTESIAN_POINT('Ctrl Pts',(-11.4558703979341,19.4701553302202,3.64935927968659));
#90236=CARTESIAN_POINT('Ctrl Pts',(-11.4564586066254,19.4698385350959,3.64351005136787));
#90237=CARTESIAN_POINT('Ctrl Pts',(-11.457317924449,19.4693432293857,3.63441475582111));
#90238=CARTESIAN_POINT('Ctrl Pts',(-11.4576134706745,19.4691660489122,3.63117099217267));
#90239=CARTESIAN_POINT('Ctrl Pts',(-11.4581418553068,19.4688360994474,3.62514931416747));
#90240=CARTESIAN_POINT('Ctrl Pts',(-11.4583775869423,19.4686834924334,3.62237170649832));
#90241=CARTESIAN_POINT('Ctrl Pts',(-11.4588948555638,19.4683359463758,3.61606290907804));
#90242=CARTESIAN_POINT('Ctrl Pts',(-11.4591715072062,19.4681407409272,3.61253137547976));
#90243=CARTESIAN_POINT('Ctrl Pts',(-11.4598557787738,19.4676326704406,3.6033693563878));
#90244=CARTESIAN_POINT('Ctrl Pts',(-11.4602436426691,19.4673187565338,3.59773750866249));
#90245=CARTESIAN_POINT('Ctrl Pts',(-11.462518878454,19.4652979615535,3.56165634540871));
#90246=CARTESIAN_POINT('Ctrl Pts',(-11.4634862001066,19.4635459198122,3.53115852443362));
#90247=CARTESIAN_POINT('Ctrl Pts',(-11.4634999512113,19.4617513002721,3.50043670964679));
#90248=CARTESIAN_POINT('Ctrl Pts',(-11.4635,19.4617385435116,3.50021835384036));
#90249=CARTESIAN_POINT('Ctrl Pts',(-11.4635,19.4617257853095,3.50000000002413));
#90250=CARTESIAN_POINT('',(-11.4634993701123,19.8894511250131,3.49867606424249));
#90251=CARTESIAN_POINT('Ctrl Pts',(-11.4635,19.3881255777082,3.49999999999758));
#90252=CARTESIAN_POINT('Ctrl Pts',(-11.4635,19.3881370392299,3.50022301552205));
#90253=CARTESIAN_POINT('Ctrl Pts',(-11.4634999490457,19.3881485027067,3.50044603164707));
#90254=CARTESIAN_POINT('Ctrl Pts',(-11.4634888518949,19.3893964453504,3.52472008708722));
#90255=CARTESIAN_POINT('Ctrl Pts',(-11.4628849790811,19.3906549537311,3.54876585650265));
#90256=CARTESIAN_POINT('Ctrl Pts',(-11.461402976112,19.3922519923169,3.57852810566533));
#90257=CARTESIAN_POINT('Ctrl Pts',(-11.4610831222154,19.3925619190849,3.58426998126322));
#90258=CARTESIAN_POINT('Ctrl Pts',(-11.4605286576543,19.3930506651495,3.59326815002381));
#90259=CARTESIAN_POINT('Ctrl Pts',(-11.4603169743387,19.393228239904,3.59652586011211));
#90260=CARTESIAN_POINT('Ctrl Pts',(-11.4599233417494,19.3935433614148,3.60228577791062));
#90261=CARTESIAN_POINT('Ctrl Pts',(-11.4597458567251,19.3936806582384,3.60478825160784));
#90262=CARTESIAN_POINT('Ctrl Pts',(-11.4593129048901,19.3940047119826,3.61067806849549));
#90263=CARTESIAN_POINT('Ctrl Pts',(-11.4590520806128,19.3941917631619,3.61406495869504));
#90264=CARTESIAN_POINT('Ctrl Pts',(-11.4582552911372,19.3947403259567,3.62396135268497));
#90265=CARTESIAN_POINT('Ctrl Pts',(-11.4576875440557,19.3951035365753,3.63046812535771));
#90266=CARTESIAN_POINT('Ctrl Pts',(-11.4528571950243,19.3979907279391,3.68185272219291));
#90267=CARTESIAN_POINT('Ctrl Pts',(-11.4465669915753,19.4006133688458,3.72651188545727));
#90268=CARTESIAN_POINT('Ctrl Pts',(-11.4204208431472,19.4089837066789,3.86537225020693));
#90269=CARTESIAN_POINT('Ctrl Pts',(-11.3933312749514,19.4148632640615,3.9579536784888));
#90270=CARTESIAN_POINT('Ctrl Pts',(-11.3313501279308,19.4246668279097,4.11169738273552));
#90271=CARTESIAN_POINT('Ctrl Pts',(-11.3007869957119,19.4286730746124,4.17425678720106));
#90272=CARTESIAN_POINT('Ctrl Pts',(-11.2606401269891,19.4331044912688,4.24345681886297));
#90273=CARTESIAN_POINT('Ctrl Pts',(-11.2552964014634,19.4336801780356,4.25244436587787));
#90274=CARTESIAN_POINT('Ctrl Pts',(-11.2465297059245,19.4346023787075,4.26683560160738));
#90275=CARTESIAN_POINT('Ctrl Pts',(-11.2431668941995,19.4349510531361,4.2722753541504));
#90276=CARTESIAN_POINT('Ctrl Pts',(-11.2371035750247,19.4355708292823,4.28194126675532));
#90277=CARTESIAN_POINT('Ctrl Pts',(-11.2344168122376,19.43584242725,4.28617589286897));
#90278=CARTESIAN_POINT('Ctrl Pts',(-11.2287411675719,19.4364098883857,4.29502048830991));
#90279=CARTESIAN_POINT('Ctrl Pts',(-11.225747982341,19.436705587331,4.29962761247738));
#90280=CARTESIAN_POINT('Ctrl Pts',(-11.2178287923076,19.4374787240333,4.3116679108839));
#90281=CARTESIAN_POINT('Ctrl Pts',(-11.2128606297635,19.4379545900671,4.31907317282511));
#90282=CARTESIAN_POINT('Ctrl Pts',(-11.1900319996136,19.4401007504995,4.35243704071685));
#90283=CARTESIAN_POINT('Ctrl Pts',(-11.1714030771434,19.4417419697623,4.37786108729252));
#90284=CARTESIAN_POINT('Ctrl Pts',(-11.1178811024405,19.446188223003,4.44616497784161));
#90285=CARTESIAN_POINT('Ctrl Pts',(-11.0813571785017,19.4489328075118,4.4877011737487));
#90286=CARTESIAN_POINT('Ctrl Pts',(-11.0052302764448,19.4542473850178,4.5649766023865));
#90287=CARTESIAN_POINT('Ctrl Pts',(-10.9658521475789,19.4568164309644,4.6008145560141));
#90288=CARTESIAN_POINT('Ctrl Pts',(-10.8668395090666,19.4630566640221,4.68151429231231));
#90289=CARTESIAN_POINT('Ctrl Pts',(-10.8055630945377,19.466746884936,4.72411281085682));
#90290=CARTESIAN_POINT('Ctrl Pts',(-10.7350818208191,19.4711080266872,4.76551937648137));
#90291=CARTESIAN_POINT('Ctrl Pts',(-10.7288178976457,19.4714965995947,4.76913712550046));
#90292=CARTESIAN_POINT('Ctrl Pts',(-10.7194491340016,19.4720796198084,4.77445585424689));
#90293=CARTESIAN_POINT('Ctrl Pts',(-10.7163644282492,19.4722718768891,4.77619229986725));
#90294=CARTESIAN_POINT('Ctrl Pts',(-10.7108387369449,19.4726168515441,4.77927648100102));
#90295=CARTESIAN_POINT('Ctrl Pts',(-10.708400170501,19.4727692974872,4.78062844848033));
#90296=CARTESIAN_POINT('Ctrl Pts',(-10.703101075647,19.4731010220007,4.78354655640935));
#90297=CARTESIAN_POINT('Ctrl Pts',(-10.700239211046,19.4732804557987,4.78511008553037));
#90298=CARTESIAN_POINT('Ctrl Pts',(-10.6921906114133,19.4737858221446,4.78947242824774));
#90299=CARTESIAN_POINT('Ctrl Pts',(-10.6869922212927,19.4741130775286,4.79224946167871));
#90300=CARTESIAN_POINT('Ctrl Pts',(-10.6555926743018,19.4760942360078,4.80878041241338));
#90301=CARTESIAN_POINT('Ctrl Pts',(-10.6289977319239,19.4777907523757,4.82176757816664));
#90302=CARTESIAN_POINT('Ctrl Pts',(-10.4781876306072,19.4874393587972,4.88983076120671));
#90303=CARTESIAN_POINT('Ctrl Pts',(-10.3471619700783,19.495850140819,4.92820822716175));
#90304=CARTESIAN_POINT('Ctrl Pts',(-10.1650416887877,19.5065454620465,4.95496207001341));
#90305=CARTESIAN_POINT('Ctrl Pts',(-10.1170551277985,19.5092828107653,4.95960687560147));
#90306=CARTESIAN_POINT('Ctrl Pts',(-10.0593274835243,19.512478084001,4.96232854438822));
#90307=CARTESIAN_POINT('Ctrl Pts',(-10.0497279317456,19.5130062565214,4.96268645342303));
#90308=CARTESIAN_POINT('Ctrl Pts',(-10.0339210232831,19.51387087085,4.96312000098184));
#90309=CARTESIAN_POINT('Ctrl Pts',(-10.0277155739982,19.5142090097267,4.96325070364289));
#90310=CARTESIAN_POINT('Ctrl Pts',(-10.0165275235296,19.5148163776531,4.96341515488704));
#90311=CARTESIAN_POINT('Ctrl Pts',(-10.0115452504418,19.5150860379272,4.96346294200809));
#90312=CARTESIAN_POINT('Ctrl Pts',(-10.0008970811179,19.5156606557286,4.96351069217716));
#90313=CARTESIAN_POINT('Ctrl Pts',(-9.99523122172534,19.5159653776625,4.96350319810504));
#90314=CARTESIAN_POINT('Ctrl Pts',(-9.97987019197919,19.5167888067918,4.96339367378582));
#90315=CARTESIAN_POINT('Ctrl Pts',(-9.9701756660977,19.5173055435273,4.96322820121313));
#90316=CARTESIAN_POINT('Ctrl Pts',(-9.9196596332674,19.5199836623755,4.96186369627595));
#90317=CARTESIAN_POINT('Ctrl Pts',(-9.87889797126392,19.5220946326705,4.95905268307079));
#90318=CARTESIAN_POINT('Ctrl Pts',(-9.71378303553656,19.5305137133052,4.94069751926143));
#90319=CARTESIAN_POINT('Ctrl Pts',(-9.59156494624521,19.5363916492481,4.91092450988107));
#90320=CARTESIAN_POINT('Ctrl Pts',(-9.46399590928774,19.5432002307963,4.86185969258435));
#90321=CARTESIAN_POINT('Ctrl Pts',(-9.45340420836556,19.5437712795273,4.85764326680083));
#90322=CARTESIAN_POINT('Ctrl Pts',(-9.4089914721531,19.5461941632612,4.83935913776671));
#90323=CARTESIAN_POINT('Ctrl Pts',(-9.37565795690693,19.5480824121372,4.82414899976603));
#90324=CARTESIAN_POINT('Ctrl Pts',(-9.33761651227905,19.550358185318,4.80503477470672));
#90325=CARTESIAN_POINT('Ctrl Pts',(-9.33231667434938,19.5506780372347,4.80233122601178));
#90326=CARTESIAN_POINT('Ctrl Pts',(-9.32384050553403,19.5511943171159,4.79794203165456));
#90327=CARTESIAN_POINT('Ctrl Pts',(-9.32065359130019,19.5513895116015,4.79627683614106));
#90328=CARTESIAN_POINT('Ctrl Pts',(-9.31499648272897,19.5517379850783,4.79329434717067));
#90329=CARTESIAN_POINT('Ctrl Pts',(-9.31252389492118,19.5518909734596,4.79198169179796));
#90330=CARTESIAN_POINT('Ctrl Pts',(-9.30724730966148,19.5522189273376,4.78916100475393));
#90331=CARTESIAN_POINT('Ctrl Pts',(-9.30444450638144,19.5523940157872,4.78765093913189));
#90332=CARTESIAN_POINT('Ctrl Pts',(-9.29677816670136,19.5528753111136,4.78348821338989));
#90333=CARTESIAN_POINT('Ctrl Pts',(-9.29192478180408,19.5531826499434,4.78081709236763));
#90334=CARTESIAN_POINT('Ctrl Pts',(-9.26613317293796,19.5548295370464,4.76643096221526));
#90335=CARTESIAN_POINT('Ctrl Pts',(-9.24547137530858,19.5561969856439,4.75423056858856));
#90336=CARTESIAN_POINT('Ctrl Pts',(-9.18274248956905,19.5604770492784,4.71507935363373));
#90337=CARTESIAN_POINT('Ctrl Pts',(-9.14174932372667,19.5634566331956,4.68647918343862));
#90338=CARTESIAN_POINT('Ctrl Pts',(-9.00281137922814,19.5740262052301,4.57857127997811));
#90339=CARTESIAN_POINT('Ctrl Pts',(-8.913694079542,19.5816308322526,4.48876256262639));
#90340=CARTESIAN_POINT('Ctrl Pts',(-8.82508023407212,19.5898300087594,4.37280739379337));
#90341=CARTESIAN_POINT('Ctrl Pts',(-8.81330670353822,19.590937076438,4.35673115864341));
#90342=CARTESIAN_POINT('Ctrl Pts',(-8.79740260013003,19.5924584405785,4.33405762417671));
#90343=CARTESIAN_POINT('Ctrl Pts',(-8.79299119237502,19.5928833510243,4.32766078087798));
#90344=CARTESIAN_POINT('Ctrl Pts',(-8.7859818838541,19.5935633217146,4.31732157013319));
#90345=CARTESIAN_POINT('Ctrl Pts',(-8.78335178913591,19.5938195881298,4.31340129521907));
#90346=CARTESIAN_POINT('Ctrl Pts',(-8.77794177869087,19.5943490871375,4.30525248276169));
#90347=CARTESIAN_POINT('Ctrl Pts',(-8.77516473087381,19.5946222105868,4.30102211059117));
#90348=CARTESIAN_POINT('Ctrl Pts',(-8.76870427074262,19.5952607680451,4.29106851671943));
#90349=CARTESIAN_POINT('Ctrl Pts',(-8.76503871221338,19.5956255390292,4.28533380853693));
#90350=CARTESIAN_POINT('Ctrl Pts',(-8.7532103196746,19.5968109109581,4.26654085692686));
#90351=CARTESIAN_POINT('Ctrl Pts',(-8.74521341125689,19.597625456764,4.25337907639385));
#90352=CARTESIAN_POINT('Ctrl Pts',(-8.70448043466346,19.6018487188167,4.18388996682947));
#90353=CARTESIAN_POINT('Ctrl Pts',(-8.6753231438874,19.6051283561073,4.12554688264944));
#90354=CARTESIAN_POINT('Ctrl Pts',(-8.61451511102962,19.6128869849944,3.98038489203253));
#90355=CARTESIAN_POINT('Ctrl Pts',(-8.58700399490199,19.617274622955,3.89214672512127));
#90356=CARTESIAN_POINT('Ctrl Pts',(-8.56575899711584,19.6224075666015,3.79137753656668));
#90357=CARTESIAN_POINT('Ctrl Pts',(-8.56365467278365,19.6229469505714,3.78082061390514));
#90358=CARTESIAN_POINT('Ctrl Pts',(-8.55488996320356,19.6253411738116,3.73417135393701));
#90359=CARTESIAN_POINT('Ctrl Pts',(-8.54947265648821,19.6272329671384,3.69786168250997));
#90360=CARTESIAN_POINT('Ctrl Pts',(-8.54476954666823,19.6295127124965,3.65547350828073));
#90361=CARTESIAN_POINT('Ctrl Pts',(-8.54414922163953,19.6298327248091,3.64955331097293));
#90362=CARTESIAN_POINT('Ctrl Pts',(-8.54321206155058,19.6303492142427,3.64005030628945));
#90363=CARTESIAN_POINT('Ctrl Pts',(-8.54287228152534,19.6305444562879,3.63646976732252));
#90364=CARTESIAN_POINT('Ctrl Pts',(-8.5422915002884,19.6308929829265,3.6301000290468));
#90365=CARTESIAN_POINT('Ctrl Pts',(-8.54204529980753,19.6310459765809,3.62731134974793));
#90366=CARTESIAN_POINT('Ctrl Pts',(-8.54153625737361,19.6313739050152,3.62135029494992));
#90367=CARTESIAN_POINT('Ctrl Pts',(-8.54127576742497,19.6315489625135,3.61817781322907));
#90368=CARTESIAN_POINT('Ctrl Pts',(-8.54059049117699,19.6320300875497,3.60948423908685));
#90369=CARTESIAN_POINT('Ctrl Pts',(-8.54018669145509,19.6323372857366,3.60396160461855));
#90370=CARTESIAN_POINT('Ctrl Pts',(-8.53820280922318,19.6339820770236,3.57453324519177));
#90371=CARTESIAN_POINT('Ctrl Pts',(-8.53717867091092,19.6353474883183,3.55059500034907));
#90372=CARTESIAN_POINT('Ctrl Pts',(-8.53583524222462,19.639618535893,3.47681521411126));
#90373=CARTESIAN_POINT('Ctrl Pts',(-8.53747382767058,19.642590846011,3.42697553874008));
#90374=CARTESIAN_POINT('Ctrl Pts',(-8.55216402382087,19.6531194160634,3.25234704689363));
#90375=CARTESIAN_POINT('Ctrl Pts',(-8.57870044642372,19.6606919054296,3.12921815587786));
#90376=CARTESIAN_POINT('Ctrl Pts',(-8.62745632911001,19.6688958815603,2.99169449324787));
#90377=CARTESIAN_POINT('Ctrl Pts',(-8.63469464575175,19.6700329964928,2.97256093634037));
#90378=CARTESIAN_POINT('Ctrl Pts',(-8.64526378429456,19.671588346472,2.94629999243609));
#90379=CARTESIAN_POINT('Ctrl Pts',(-8.64825424920253,19.6720178284821,2.93903891303143));
#90380=CARTESIAN_POINT('Ctrl Pts',(-8.65314190456953,19.6727032078373,2.92743738037344));
#90381=CARTESIAN_POINT('Ctrl Pts',(-8.65500194937244,19.6729603474446,2.92308152468217));
#90382=CARTESIAN_POINT('Ctrl Pts',(-8.65888926558614,19.6734902370097,2.91409918844373));
#90383=CARTESIAN_POINT('Ctrl Pts',(-8.66091941059574,19.6737628855044,2.90947401504536));
#90384=CARTESIAN_POINT('Ctrl Pts',(-8.66571773557392,19.6743979113802,2.89869422989448));
#90385=CARTESIAN_POINT('Ctrl Pts',(-8.66850463347723,19.6747596475565,2.89254804195705));
#90386=CARTESIAN_POINT('Ctrl Pts',(-8.67765512759769,19.6759249468962,2.87273322402547));
#90387=CARTESIAN_POINT('Ctrl Pts',(-8.68418757119051,19.6767227413814,2.85914335120469));
#90388=CARTESIAN_POINT('Ctrl Pts',(-8.71890115548597,19.6807957758188,2.78969581140663));
#90389=CARTESIAN_POINT('Ctrl Pts',(-8.7504341805923,19.683952514362,2.73558343377593));
#90390=CARTESIAN_POINT('Ctrl Pts',(-8.83560972332474,19.6914952616717,2.60884892028306));
#90391=CARTESIAN_POINT('Ctrl Pts',(-8.89268249415985,19.6957880909552,2.5388537987157));
#90392=CARTESIAN_POINT('Ctrl Pts',(-8.99212286210712,19.7028272091799,2.43759752579814));
#90393=CARTESIAN_POINT('Ctrl Pts',(-9.03035017278664,19.7054532030893,2.40259692823344));
#90394=CARTESIAN_POINT('Ctrl Pts',(-9.07584518979355,19.7085970225304,2.36517807434153));
#90395=CARTESIAN_POINT('Ctrl Pts',(-9.0813754294384,19.7089794808208,2.36069678731107));
#90396=CARTESIAN_POINT('Ctrl Pts',(-9.08968648324077,19.7095550756271,2.35406199147379));
#90397=CARTESIAN_POINT('Ctrl Pts',(-9.09244281079923,19.7097461028654,2.35187780877597));
#90398=CARTESIAN_POINT('Ctrl Pts',(-9.0973972836655,19.7100897646473,2.34798075005767));
#90399=CARTESIAN_POINT('Ctrl Pts',(-9.0995924731048,19.710242136298,2.34626419787403));
#90400=CARTESIAN_POINT('Ctrl Pts',(-9.10438099917312,19.7105747542419,2.34254174847796));
#90401=CARTESIAN_POINT('Ctrl Pts',(-9.10697614331696,19.7107551628563,2.34053831903817));
#90402=CARTESIAN_POINT('Ctrl Pts',(-9.11431900084161,19.7112659798729,2.33490897095393));
#90403=CARTESIAN_POINT('Ctrl Pts',(-9.11908215842843,19.7115977561718,2.33130342170295));
#90404=CARTESIAN_POINT('Ctrl Pts',(-9.14876356574491,19.7136670950381,2.30912014208308));
#90405=CARTESIAN_POINT('Ctrl Pts',(-9.17424466770942,19.7154516879571,2.29131221813473));
#90406=CARTESIAN_POINT('Ctrl Pts',(-9.33457789607275,19.7266358461978,2.18669750910278));
#90407=CARTESIAN_POINT('Ctrl Pts',(-9.48238553957991,19.7365995753722,2.12172398753755));
#90408=CARTESIAN_POINT('Ctrl Pts',(-9.6629788467985,19.7471601878114,2.07559729912238));
#90409=CARTESIAN_POINT('Ctrl Pts',(-9.68830152301704,19.7486107833966,2.06984249380475));
#90410=CARTESIAN_POINT('Ctrl Pts',(-9.72223535808229,19.7505155864279,2.06307493148943));
#90411=CARTESIAN_POINT('Ctrl Pts',(-9.73072052486733,19.7509886690149,2.06146066526613));
#90412=CARTESIAN_POINT('Ctrl Pts',(-9.74456490866533,19.7517554262881,2.05895361863814));
#90413=CARTESIAN_POINT('Ctrl Pts',(-9.74991559927502,19.7520505272024,2.05801541175204));
#90414=CARTESIAN_POINT('Ctrl Pts',(-9.76023446564596,19.752617280279,2.05626523255056));
#90415=CARTESIAN_POINT('Ctrl Pts',(-9.76520184284659,19.752889060973,2.05544906061482));
#90416=CARTESIAN_POINT('Ctrl Pts',(-9.77672822323623,19.7535173202494,2.05361622792713));
#90417=CARTESIAN_POINT('Ctrl Pts',(-9.78329015722995,19.7538731994404,2.05261852007167));
#90418=CARTESIAN_POINT('Ctrl Pts',(-9.80417626518422,19.7550004063593,2.04958811980506));
#90419=CARTESIAN_POINT('Ctrl Pts',(-9.81852413989434,19.755766488904,2.04772313614655));
#90420=CARTESIAN_POINT('Ctrl Pts',(-9.89035499686071,19.7595635307535,2.03946750216789));
#90421=CARTESIAN_POINT('Ctrl Pts',(-9.94815623199775,19.7624940727064,2.03627517345835));
#90422=CARTESIAN_POINT('Ctrl Pts',(-10.1262541280899,19.7713268299521,2.03700527146272));
#90423=CARTESIAN_POINT('Ctrl Pts',(-10.2459761815924,19.7769596538143,2.05231754779553));
#90424=CARTESIAN_POINT('Ctrl Pts',(-10.3904950169908,19.7845676826105,2.08926157923564));
#90425=CARTESIAN_POINT('Ctrl Pts',(-10.4183041668185,19.7860725025643,2.09725602705258));
#90426=CARTESIAN_POINT('Ctrl Pts',(-10.4511554702649,19.7879187716305,2.10776368868606));
#90427=CARTESIAN_POINT('Ctrl Pts',(-10.4564449131565,19.7882181921252,2.10948885507311));
#90428=CARTESIAN_POINT('Ctrl Pts',(-10.4650628657661,19.7887097380655,2.11235409454352));
#90429=CARTESIAN_POINT('Ctrl Pts',(-10.4683973768328,19.7889008401202,2.11347610013684));
#90430=CARTESIAN_POINT('Ctrl Pts',(-10.4743658418246,19.7892445814191,2.11550837330259));
#90431=CARTESIAN_POINT('Ctrl Pts',(-10.4770012714212,19.789396957238,2.11641415041444));
#90432=CARTESIAN_POINT('Ctrl Pts',(-10.4827305618842,19.7897295192493,2.11840157925402));
#90433=CARTESIAN_POINT('Ctrl Pts',(-10.4858233404175,19.7899098673236,2.11948608371518));
#90434=CARTESIAN_POINT('Ctrl Pts',(-10.4945384575337,19.7904203452318,2.12257501380342));
#90435=CARTESIAN_POINT('Ctrl Pts',(-10.5001521463365,19.7907518401392,2.12460343660886));
#90436=CARTESIAN_POINT('Ctrl Pts',(-10.5344870476136,19.7927951232602,2.13724783812309));
#90437=CARTESIAN_POINT('Ctrl Pts',(-10.5628797707166,19.7945525210164,2.1487280238192));
#90438=CARTESIAN_POINT('Ctrl Pts',(-10.6610882482114,19.8008204992774,2.19206948588274));
#90439=CARTESIAN_POINT('Ctrl Pts',(-10.7287392971688,19.8054753552094,2.2285212655474));
#90440=CARTESIAN_POINT('Ctrl Pts',(-10.8645873012179,19.8151904104543,2.31613627882895));
#90441=CARTESIAN_POINT('Ctrl Pts',(-10.9318223407228,19.8202184239716,2.36829552523978));
#90442=CARTESIAN_POINT('Ctrl Pts',(-11.0125920698612,19.8264473289293,2.44306083109441));
#90443=CARTESIAN_POINT('Ctrl Pts',(-11.0305827273165,19.8278496410744,2.46059514210448));
#90444=CARTESIAN_POINT('Ctrl Pts',(-11.0540655613569,19.8297013682571,2.48469179009598));
#90445=CARTESIAN_POINT('Ctrl Pts',(-11.0599637430919,19.8301683602617,2.49085093450522));
#90446=CARTESIAN_POINT('Ctrl Pts',(-11.069514070692,19.8309277364672,2.5009999244755));
#90447=CARTESIAN_POINT('Ctrl Pts',(-11.0731984714005,19.8312214956212,2.50495902577625));
#90448=CARTESIAN_POINT('Ctrl Pts',(-11.0802756890719,19.831787360392,2.51264894088238));
#90449=CARTESIAN_POINT('Ctrl Pts',(-11.0836713308142,19.832059583447,2.51637704073608));
#90450=CARTESIAN_POINT('Ctrl Pts',(-11.0915302243543,19.8326913494294,2.52509547051751));
#90451=CARTESIAN_POINT('Ctrl Pts',(-11.0959786566836,19.8330502712902,2.53009904711472));
#90452=CARTESIAN_POINT('Ctrl Pts',(-11.1097075710606,19.8341622704137,2.545756331416));
#90453=CARTESIAN_POINT('Ctrl Pts',(-11.1188683708862,19.834910435979,2.55651419759801));
#90454=CARTESIAN_POINT('Ctrl Pts',(-11.1683195161835,19.8389866024002,2.6163198669558));
#90455=CARTESIAN_POINT('Ctrl Pts',(-11.2055438973363,19.8421909595547,2.66781842694425));
#90456=CARTESIAN_POINT('Ctrl Pts',(-11.2664674218612,19.8478496029484,2.76481327483067));
#90457=CARTESIAN_POINT('Ctrl Pts',(-11.2913443219007,19.8503251223025,2.80944280029376));
#90458=CARTESIAN_POINT('Ctrl Pts',(-11.3511495750143,19.8569277173582,2.93131679114062));
#90459=CARTESIAN_POINT('Ctrl Pts',(-11.3817860003093,19.861052370121,3.01043908276629));
#90460=CARTESIAN_POINT('Ctrl Pts',(-11.408564591399,19.8661158509983,3.10262587747066));
#90461=CARTESIAN_POINT('Ctrl Pts',(-11.4115960946363,19.8667189906883,3.11353285858365));
#90462=CARTESIAN_POINT('Ctrl Pts',(-11.4156228675866,19.8675647257246,3.12870056083994));
#90463=CARTESIAN_POINT('Ctrl Pts',(-11.4167260951719,19.8678014440579,3.13293250345685));
#90464=CARTESIAN_POINT('Ctrl Pts',(-11.4184635892592,19.868182513626,3.13972199746729));
#90465=CARTESIAN_POINT('Ctrl Pts',(-11.4191099545004,19.8683261786957,3.14227646153254));
#90466=CARTESIAN_POINT('Ctrl Pts',(-11.420445710445,19.8686271163107,3.14761602510535));
#90467=CARTESIAN_POINT('Ctrl Pts',(-11.4211338110559,19.8687844639743,3.15040141206348));
#90468=CARTESIAN_POINT('Ctrl Pts',(-11.4227836461558,19.8691674054795,3.15716520154111));
#90469=CARTESIAN_POINT('Ctrl Pts',(-11.4237368868074,19.8693934771686,3.16114563730735));
#90470=CARTESIAN_POINT('Ctrl Pts',(-11.4257351832887,19.8698777726327,3.16964720387249));
#90471=CARTESIAN_POINT('Ctrl Pts',(-11.4267754564191,19.8701362499985,3.17416940202215));
#90472=CARTESIAN_POINT('Ctrl Pts',(-11.4317038490203,19.871391970386,3.1960699675285));
#90473=CARTESIAN_POINT('Ctrl Pts',(-11.4352959031073,19.8724040590828,3.21351267192146));
#90474=CARTESIAN_POINT('Ctrl Pts',(-11.4550740134502,19.8785960252534,3.31928901210277));
#90475=CARTESIAN_POINT('Ctrl Pts',(-11.4634181561964,19.8840564920709,3.40888654081214));
#90476=CARTESIAN_POINT('Ctrl Pts',(-11.4634994008935,19.8894511611806,3.49867577028773));
#90477=CARTESIAN_POINT('Ctrl Pts',(-11.4634994011565,19.8894511786466,3.49867606099216));
#90478=CARTESIAN_POINT('Ctrl Pts',(-11.4634998003887,19.889477693589,3.49911737745962));
#90479=CARTESIAN_POINT('Ctrl Pts',(-11.4635,19.8895042068034,3.49955869048854));
#90480=CARTESIAN_POINT('Ctrl Pts',(-11.4635,19.889530718258,3.4999999999448));
#90481=CARTESIAN_POINT('Origin',(-10.,13.2,3.5));
#90482=CARTESIAN_POINT('',(-11.4635,20.459317028952,3.50000000000019));
#90483=CARTESIAN_POINT('',(-11.4635,20.390600218991,3.49999999999975));
#90484=CARTESIAN_POINT('',(-11.4635,13.2,3.5));
#90485=CARTESIAN_POINT('Ctrl Pts',(-11.4635,20.459317028952,3.5000000000001));
#90486=CARTESIAN_POINT('Ctrl Pts',(-11.4635,20.4585861607261,3.48684366450097));
#90487=CARTESIAN_POINT('Ctrl Pts',(-11.4633225942004,20.457860760563,3.47368763253133));
#90488=CARTESIAN_POINT('Ctrl Pts',(-11.4627948065494,20.4567898065315,3.45412231023958));
#90489=CARTESIAN_POINT('Ctrl Pts',(-11.4625796377616,20.4564400819949,3.44771029236232));
#90490=CARTESIAN_POINT('Ctrl Pts',(-11.4621216643936,20.4558199937918,3.43630138831388));
#90491=CARTESIAN_POINT('Ctrl Pts',(-11.4618953899615,20.4555491216085,3.43130397179102));
#90492=CARTESIAN_POINT('Ctrl Pts',(-11.4613647468365,20.4549801729395,3.42077896701188));
#90493=CARTESIAN_POINT('Ctrl Pts',(-11.4610546289448,20.4546822793544,3.41525173889905));
#90494=CARTESIAN_POINT('Ctrl Pts',(-11.4601510936625,20.4538966131438,3.40063168220289));
#90495=CARTESIAN_POINT('Ctrl Pts',(-11.4595040997807,20.4534105090671,3.39154232769414));
#90496=CARTESIAN_POINT('Ctrl Pts',(-11.4560719320678,20.4511428547768,3.34894637463714));
#90497=CARTESIAN_POINT('Ctrl Pts',(-11.4522174412442,20.4493946878353,3.31553482727249));
#90498=CARTESIAN_POINT('Ctrl Pts',(-11.438138932602,20.4445582981249,3.22195134093262));
#90499=CARTESIAN_POINT('Ctrl Pts',(-11.4252983366242,20.4415455503876,3.16224261081665));
#90500=CARTESIAN_POINT('Ctrl Pts',(-11.3822214179042,20.433783059304,3.00918732932115));
#90501=CARTESIAN_POINT('Ctrl Pts',(-11.3462729364702,20.4291146075255,2.91778108706047));
#90502=CARTESIAN_POINT('Ctrl Pts',(-11.2905274834118,20.4228469200063,2.80938922834438));
#90503=CARTESIAN_POINT('Ctrl Pts',(-11.2790682285419,20.4215950503575,2.78839002263734));
#90504=CARTESIAN_POINT('Ctrl Pts',(-11.2642284884675,20.42000559209,2.76271341011662));
#90505=CARTESIAN_POINT('Ctrl Pts',(-11.2613275828113,20.4196962904609,2.75776155224647));
#90506=CARTESIAN_POINT('Ctrl Pts',(-11.2567326861606,20.4192083558283,2.75002277285764));
#90507=CARTESIAN_POINT('Ctrl Pts',(-11.2550583449591,20.4190309611882,2.74722417943978));
#90508=CARTESIAN_POINT('Ctrl Pts',(-11.2519356941978,20.4187008217362,2.74204417256937));
#90509=CARTESIAN_POINT('Ctrl Pts',(-11.2504899281503,20.4185482405374,2.73966128735058));
#90510=CARTESIAN_POINT('Ctrl Pts',(-11.2471940631138,20.418201024319,2.73426393011264));
#90511=CARTESIAN_POINT('Ctrl Pts',(-11.2453398462278,20.4180061249949,2.73125203958135));
#90512=CARTESIAN_POINT('Ctrl Pts',(-11.2396661928984,20.4174111640023,2.72211045666386));
#90513=CARTESIAN_POINT('Ctrl Pts',(-11.2358123425125,20.4170089488611,2.71600238446182));
#90514=CARTESIAN_POINT('Ctrl Pts',(-11.1836711101133,20.4115950902546,2.63470207207895));
#90515=CARTESIAN_POINT('Ctrl Pts',(-11.1286450767361,20.4062093218945,2.56406460363401));
#90516=CARTESIAN_POINT('Ctrl Pts',(-10.9909043473901,20.3940826678966,2.41718499056907));
#90517=CARTESIAN_POINT('Ctrl Pts',(-10.9051396337102,20.3874055017354,2.34453036920985));
#90518=CARTESIAN_POINT('Ctrl Pts',(-10.7979156082569,20.3801990584344,2.27303384144496));
#90519=CARTESIAN_POINT('Ctrl Pts',(-10.7837583681777,20.3792671828579,2.2639425071447));
#90520=CARTESIAN_POINT('Ctrl Pts',(-10.7638920337555,20.3779860184665,2.25166356376414));
#90521=CARTESIAN_POINT('Ctrl Pts',(-10.7583139976357,20.3776291379109,2.24826728883624));
#90522=CARTESIAN_POINT('Ctrl Pts',(-10.7486585644598,20.3770162174819,2.24247665681609));
#90523=CARTESIAN_POINT('Ctrl Pts',(-10.7445919847818,20.3767595362859,2.24006453271567));
#90524=CARTESIAN_POINT('Ctrl Pts',(-10.7361552218653,20.3762300004168,2.23511531218163));
#90525=CARTESIAN_POINT('Ctrl Pts',(-10.7317834402164,20.3759572503516,2.23258105518874));
#90526=CARTESIAN_POINT('Ctrl Pts',(-10.721524047013,20.3753209769279,2.22670461715346));
#90527=CARTESIAN_POINT('Ctrl Pts',(-10.7156261688355,20.3749581033805,2.22338053008284));
#90528=CARTESIAN_POINT('Ctrl Pts',(-10.6964076928092,20.3737848954022,2.2127238940706));
#90529=CARTESIAN_POINT('Ctrl Pts',(-10.6829956023699,20.3729804432523,2.20555785084485));
#90530=CARTESIAN_POINT('Ctrl Pts',(-10.6129199208088,20.3688472271292,2.16950904821246));
#90531=CARTESIAN_POINT('Ctrl Pts',(-10.5545268275638,20.3656411487338,2.14413194679851));
#90532=CARTESIAN_POINT('Ctrl Pts',(-10.40210321424,20.3576476321263,2.08939108164212));
#90533=CARTESIAN_POINT('Ctrl Pts',(-10.3064346172044,20.3529829476257,2.06556611554445));
#90534=CARTESIAN_POINT('Ctrl Pts',(-10.1996502540447,20.3475813911027,2.05015060114662));
#90535=CARTESIAN_POINT('Ctrl Pts',(-10.190182601987,20.3471006733265,2.04887833867582));
#90536=CARTESIAN_POINT('Ctrl Pts',(-10.1470890727483,20.3449018132879,2.04351640419182));
#90537=CARTESIAN_POINT('Ctrl Pts',(-10.1133421801772,20.3431501199156,2.04050252794203));
#90538=CARTESIAN_POINT('Ctrl Pts',(-10.0737069406151,20.3410273455869,2.03834563840073));
#90539=CARTESIAN_POINT('Ctrl Pts',(-10.0678883553571,20.3407140648319,2.03806383353461));
#90540=CARTESIAN_POINT('Ctrl Pts',(-10.0584748490325,20.3402043410197,2.03766423880226));
#90541=CARTESIAN_POINT('Ctrl Pts',(-10.0548808469425,20.340009052094,2.03752494772663));
#90542=CARTESIAN_POINT('Ctrl Pts',(-10.0484957827406,20.3396608388582,2.03730105414115));
#90543=CARTESIAN_POINT('Ctrl Pts',(-10.0457049527783,20.3395082079309,2.0372111894317));
#90544=CARTESIAN_POINT('Ctrl Pts',(-10.0396958335017,20.3391786240388,2.03703490976044));
#90545=CARTESIAN_POINT('Ctrl Pts',(-10.0364775593377,20.3390015327322,2.0369511280516));
#90546=CARTESIAN_POINT('Ctrl Pts',(-10.0275552941409,20.3385090174946,2.03674831091788));
#90547=CARTESIAN_POINT('Ctrl Pts',(-10.0218509073033,20.3381923737394,2.03665201148477));
#90548=CARTESIAN_POINT('Ctrl Pts',(-9.98969365549149,20.3363980144065,2.03629721200639));
#90549=CARTESIAN_POINT('Ctrl Pts',(-9.96323970265074,20.334886298025,2.03672266032551));
#90550=CARTESIAN_POINT('Ctrl Pts',(-9.87810227136302,20.3299369259874,2.04040188642371));
#90551=CARTESIAN_POINT('Ctrl Pts',(-9.81960017659495,20.3264088661178,2.04647296012052));
#90552=CARTESIAN_POINT('Ctrl Pts',(-9.6438861012254,20.3156861790243,2.07548063515102));
#90553=CARTESIAN_POINT('Ctrl Pts',(-9.52894419341959,20.3085432518702,2.10924889192518));
#90554=CARTESIAN_POINT('Ctrl Pts',(-9.40434830473908,20.3009587714688,2.16310096173804));
#90555=CARTESIAN_POINT('Ctrl Pts',(-9.38943821841819,20.3000528708883,2.16984424897268));
#90556=CARTESIAN_POINT('Ctrl Pts',(-9.36880853794113,20.2988014639674,2.17959428735803));
#90557=CARTESIAN_POINT('Ctrl Pts',(-9.36299140740488,20.29844881634,2.18239081568749));
#90558=CARTESIAN_POINT('Ctrl Pts',(-9.35296298884173,20.2978412077954,2.18729381612792));
#90559=CARTESIAN_POINT('Ctrl Pts',(-9.34874304742762,20.2975856310286,2.18938228249713));
#90560=CARTESIAN_POINT('Ctrl Pts',(-9.34000415353803,20.2970565573425,2.19375982596258));
#90561=CARTESIAN_POINT('Ctrl Pts',(-9.33548685441311,20.2967831749257,2.19605207548404));
#90562=CARTESIAN_POINT('Ctrl Pts',(-9.32489338302851,20.2961422748894,2.20149695307174));
#90563=CARTESIAN_POINT('Ctrl Pts',(-9.31882721871617,20.2957754356686,2.20466886420272));
#90564=CARTESIAN_POINT('Ctrl Pts',(-9.29898410424006,20.2945758233606,2.21522248989186));
#90565=CARTESIAN_POINT('Ctrl Pts',(-9.28530287418127,20.2937493147883,2.22278248535166));
#90566=CARTESIAN_POINT('Ctrl Pts',(-9.21358644135855,20.2894159200497,2.26392493071262));
#90567=CARTESIAN_POINT('Ctrl Pts',(-9.15778651145136,20.2860462143296,2.30124830370249));
#90568=CARTESIAN_POINT('Ctrl Pts',(-9.02608012585929,20.2778500202053,2.4030956614309));
#90569=CARTESIAN_POINT('Ctrl Pts',(-8.9538313725829,20.273135691026,2.47177433908668));
#90570=CARTESIAN_POINT('Ctrl Pts',(-8.86439788531536,20.2662175017211,2.57605160217889));
#90571=CARTESIAN_POINT('Ctrl Pts',(-8.8408209205691,20.2642638759563,2.60580974911267));
#90572=CARTESIAN_POINT('Ctrl Pts',(-8.81488697556333,20.2619148859655,2.64129434408914));
#90573=CARTESIAN_POINT('Ctrl Pts',(-8.81137485014706,20.2615922180586,2.64616246577292));
#90574=CARTESIAN_POINT('Ctrl Pts',(-8.80579830310663,20.2610722943105,2.65399314736641));
#90575=CARTESIAN_POINT('Ctrl Pts',(-8.80371468763766,20.260876300372,2.65694203139851));
#90576=CARTESIAN_POINT('Ctrl Pts',(-8.80003445426928,20.2605269763263,2.66219167959683));
#90577=CARTESIAN_POINT('Ctrl Pts',(-8.79843350266798,20.2603739426225,2.66448935071331));
#90578=CARTESIAN_POINT('Ctrl Pts',(-8.79503284550171,20.2600465593963,2.66939993233331));
#90579=CARTESIAN_POINT('Ctrl Pts',(-8.79323506723848,20.2598720912459,2.67201406262575));
#90580=CARTESIAN_POINT('Ctrl Pts',(-8.78834803912353,20.2593940409363,2.67916996460683));
#90581=CARTESIAN_POINT('Ctrl Pts',(-8.78527586851363,20.2590893510475,2.68372326768473));
#90582=CARTESIAN_POINT('Ctrl Pts',(-8.76927150352025,20.2574804591513,2.70773397682981));
#90583=CARTESIAN_POINT('Ctrl Pts',(-8.7567816584149,20.2561498219653,2.72748067258661));
#90584=CARTESIAN_POINT('Ctrl Pts',(-8.72015780539824,20.2520306381704,2.78857350248166));
#90585=CARTESIAN_POINT('Ctrl Pts',(-8.6975756914836,20.2491802905592,2.83081088587004));
#90586=CARTESIAN_POINT('Ctrl Pts',(-8.63407573749567,20.2402673835883,2.96501845979466));
#90587=CARTESIAN_POINT('Ctrl Pts',(-8.60053390658912,20.2341704435879,3.06016707201283));
#90588=CARTESIAN_POINT('Ctrl Pts',(-8.56696162203014,20.2258660540496,3.19985729705873));
#90589=CARTESIAN_POINT('Ctrl Pts',(-8.55875445129622,20.2234295009587,3.2421309587808));
#90590=CARTESIAN_POINT('Ctrl Pts',(-8.55092430309774,20.220488760785,3.29477928035595));
#90591=CARTESIAN_POINT('Ctrl Pts',(-8.54953159768786,20.2199295246279,3.30486584004043));
#90592=CARTESIAN_POINT('Ctrl Pts',(-8.5475068873743,20.2190551502944,3.32075151269132));
#90593=CARTESIAN_POINT('Ctrl Pts',(-8.54680411210141,20.2187378088219,3.32654114263757));
#90594=CARTESIAN_POINT('Ctrl Pts',(-8.54562367785358,20.2181790684193,3.33677696801069));
#90595=CARTESIAN_POINT('Ctrl Pts',(-8.5451317563247,20.21793722717,3.34122141595275));
#90596=CARTESIAN_POINT('Ctrl Pts',(-8.54405002705769,20.2173838976553,3.35142205156006));
#90597=CARTESIAN_POINT('Ctrl Pts',(-8.54347396949103,20.2170728417907,3.35717964346401));
#90598=CARTESIAN_POINT('Ctrl Pts',(-8.54197193984876,20.2162135830915,3.37314760006469));
#90599=CARTESIAN_POINT('Ctrl Pts',(-8.54111907612931,20.2156676589603,3.38336461650375));
#90600=CARTESIAN_POINT('Ctrl Pts',(-8.5367643629416,20.2124973751532,3.44309819412834));
#90601=CARTESIAN_POINT('Ctrl Pts',(-8.53567605865511,20.2099491778866,3.49276067483508));
#90602=CARTESIAN_POINT('Ctrl Pts',(-8.54056124353831,20.201479750471,3.66136423339364));
#90603=CARTESIAN_POINT('Ctrl Pts',(-8.55850935500589,20.1958884282564,3.77946747108423));
#90604=CARTESIAN_POINT('Ctrl Pts',(-8.5927282984786,20.1895349614457,3.90185017331306));
#90605=CARTESIAN_POINT('Ctrl Pts',(-8.59496256707478,20.1891303024943,3.90959371669516));
#90606=CARTESIAN_POINT('Ctrl Pts',(-8.60764490262973,20.1868860310935,3.9522230724931));
#90607=CARTESIAN_POINT('Ctrl Pts',(-8.61932756751662,20.1850082975208,3.98672543146744));
#90608=CARTESIAN_POINT('Ctrl Pts',(-8.63439694046938,20.182744377329,4.02630391238361));
#90609=CARTESIAN_POINT('Ctrl Pts',(-8.63654401192042,20.1824250754662,4.03184141486891));
#90610=CARTESIAN_POINT('Ctrl Pts',(-8.64004362442416,20.1819095483078,4.04070676851005));
#90611=CARTESIAN_POINT('Ctrl Pts',(-8.64137483797195,20.1817145512693,4.0440430327879));
#90612=CARTESIAN_POINT('Ctrl Pts',(-8.64376489016373,20.1813663436337,4.04996945997589));
#90613=CARTESIAN_POINT('Ctrl Pts',(-8.64481888990078,20.1812134225456,4.0525615248878));
#90614=CARTESIAN_POINT('Ctrl Pts',(-8.64708815847951,20.1808855154591,4.05809670980613));
#90615=CARTESIAN_POINT('Ctrl Pts',(-8.64830558101838,20.1807104059678,4.06103884510556));
#90616=CARTESIAN_POINT('Ctrl Pts',(-8.65166925793434,20.1802288291927,4.06909331619036));
#90617=CARTESIAN_POINT('Ctrl Pts',(-8.65383495637173,20.1799212272831,4.07419741015248));
#90618=CARTESIAN_POINT('Ctrl Pts',(-8.66555934888172,20.178269422689,4.10139840502714));
#90619=CARTESIAN_POINT('Ctrl Pts',(-8.67563270323871,20.176897121994,4.12326801426323));
#90620=CARTESIAN_POINT('Ctrl Pts',(-8.70837821347617,20.1725951849505,4.18997791047985));
#90621=CARTESIAN_POINT('Ctrl Pts',(-8.73282264425357,20.1695978494516,4.23390551272138));
#90622=CARTESIAN_POINT('Ctrl Pts',(-8.82701899972409,20.1589299200293,4.38439481185877));
#90623=CARTESIAN_POINT('Ctrl Pts',(-8.90836851306369,20.1512486618383,4.48305168894253));
#90624=CARTESIAN_POINT('Ctrl Pts',(-9.01512649082637,20.1430598075018,4.58268430628366));
#90625=CARTESIAN_POINT('Ctrl Pts',(-9.02902516341687,20.1420232106957,4.59516621946138));
#90626=CARTESIAN_POINT('Ctrl Pts',(-9.0488836785362,20.1405822959859,4.61232514292157));
#90627=CARTESIAN_POINT('Ctrl Pts',(-9.05464625160571,20.1401687770694,4.61722682295983));
#90628=CARTESIAN_POINT('Ctrl Pts',(-9.06403595145289,20.1395023146433,4.62508909225015));
#90629=CARTESIAN_POINT('Ctrl Pts',(-9.06763968120551,20.1392482529777,4.62807730334386));
#90630=CARTESIAN_POINT('Ctrl Pts',(-9.07518761168055,20.138719682142,4.63427516671551));
#90631=CARTESIAN_POINT('Ctrl Pts',(-9.0791343320648,20.1384453018159,4.6374816613624));
#90632=CARTESIAN_POINT('Ctrl Pts',(-9.08852124092305,20.1377973932307,4.64502713607102));
#90633=CARTESIAN_POINT('Ctrl Pts',(-9.0939758484807,20.1374245867772,4.64934803681316));
#90634=CARTESIAN_POINT('Ctrl Pts',(-9.11229675865478,20.1361844614468,4.66364958310356));
#90635=CARTESIAN_POINT('Ctrl Pts',(-9.12529903177867,20.1353240185402,4.67345457564422));
#90636=CARTESIAN_POINT('Ctrl Pts',(-9.19713585962409,20.1306713734026,4.72576901378889));
#90637=CARTESIAN_POINT('Ctrl Pts',(-9.25890914353523,20.1270414561978,4.76407532114117));
#90638=CARTESIAN_POINT('Ctrl Pts',(-9.41089829175372,20.1186337239025,4.84333808502662));
#90639=CARTESIAN_POINT('Ctrl Pts',(-9.50291668369698,20.1139425395583,4.88003750392223));
#90640=CARTESIAN_POINT('Ctrl Pts',(-9.62922331045825,20.1072785057017,4.91612732635012));
#90641=CARTESIAN_POINT('Ctrl Pts',(-9.66081129649352,20.105592463459,4.9240234115604));
#90642=CARTESIAN_POINT('Ctrl Pts',(-9.69825775149512,20.1035436591159,4.93206737039526));
#90643=CARTESIAN_POINT('Ctrl Pts',(-9.70388864685603,20.1032342557305,4.93324226920779));
#90644=CARTESIAN_POINT('Ctrl Pts',(-9.71302981526673,20.1027296215998,4.93509342608285));
#90645=CARTESIAN_POINT('Ctrl Pts',(-9.71653595140138,20.1025355077801,4.93579008253647));
#90646=CARTESIAN_POINT('Ctrl Pts',(-9.7227833465373,20.1021885762415,4.93700764189391));
#90647=CARTESIAN_POINT('Ctrl Pts',(-9.7255235791595,20.102036043593,4.93753355789755));
#90648=CARTESIAN_POINT('Ctrl Pts',(-9.73144336653739,20.1017057291804,4.938652162645));
#90649=CARTESIAN_POINT('Ctrl Pts',(-9.73462334065085,20.101527802894,4.93924214040401));
#90650=CARTESIAN_POINT('Ctrl Pts',(-9.74348510040362,20.101030658394,4.94085588704509));
#90651=CARTESIAN_POINT('Ctrl Pts',(-9.74917096292433,20.1007101834854,4.94185657151965));
#90652=CARTESIAN_POINT('Ctrl Pts',(-9.78201888808637,20.0988507152992,4.94743747443672));
#90653=CARTESIAN_POINT('Ctrl Pts',(-9.80929839007174,20.0972748311089,4.95128346721581));
#90654=CARTESIAN_POINT('Ctrl Pts',(-9.89931083282583,20.0920064859197,4.96139232572001));
#90655=CARTESIAN_POINT('Ctrl Pts',(-9.96233935506856,20.0882114704415,4.96437246090669));
#90656=CARTESIAN_POINT('Ctrl Pts',(-10.1386103983788,20.0775941531258,4.96131753616541));
#90657=CARTESIAN_POINT('Ctrl Pts',(-10.2512695827667,20.0708375309667,4.94621357288375));
#90658=CARTESIAN_POINT('Ctrl Pts',(-10.3773087313069,20.063565625763,4.91412556522857));
#90659=CARTESIAN_POINT('Ctrl Pts',(-10.3934744215156,20.0626375772524,4.90971305781014));
#90660=CARTESIAN_POINT('Ctrl Pts',(-10.4158202280936,20.0613607852006,4.90319930561471));
#90661=CARTESIAN_POINT('Ctrl Pts',(-10.4220670027975,20.0610045171669,4.90133300840579));
#90662=CARTESIAN_POINT('Ctrl Pts',(-10.4328195102951,20.0603923662041,4.89804214858246));
#90663=CARTESIAN_POINT('Ctrl Pts',(-10.437331163193,20.0601358456546,4.89663740181011));
#90664=CARTESIAN_POINT('Ctrl Pts',(-10.4466549548152,20.0596063815475,4.89368473940844));
#90665=CARTESIAN_POINT('Ctrl Pts',(-10.4514660409754,20.0593335440106,4.89213369194642));
#90666=CARTESIAN_POINT('Ctrl Pts',(-10.4627116529755,20.058696620408,4.88844378794382));
#90667=CARTESIAN_POINT('Ctrl Pts',(-10.4691395721417,20.0583331881689,4.88628506809995));
#90668=CARTESIAN_POINT('Ctrl Pts',(-10.4895091464893,20.0571833440202,4.87928634947637));
#90669=CARTESIAN_POINT('Ctrl Pts',(-10.5033929463999,20.0564023830972,4.87428002997463));
#90670=CARTESIAN_POINT('Ctrl Pts',(-10.5359550749984,20.0545758419502,4.86197885583329));
#90671=CARTESIAN_POINT('Ctrl Pts',(-10.5545640838046,20.0535359986684,4.8545083872159));
#90672=CARTESIAN_POINT('Ctrl Pts',(-10.6209758989012,20.0498321984615,4.82624959486688));
#90673=CARTESIAN_POINT('Ctrl Pts',(-10.6678152016703,20.0472351762392,4.80329293425981));
#90674=CARTESIAN_POINT('Ctrl Pts',(-10.78354775598,20.0407257828274,4.73868949579091));
#90675=CARTESIAN_POINT('Ctrl Pts',(-10.8504108399234,20.0368799263507,4.69377529215694));
#90676=CARTESIAN_POINT('Ctrl Pts',(-10.9539521411974,20.0303095640824,4.61109020932959));
#90677=CARTESIAN_POINT('Ctrl Pts',(-10.9928912584495,20.027669381724,4.5764348661828));
#90678=CARTESIAN_POINT('Ctrl Pts',(-11.0349584116525,20.0245094367286,4.53476765629012));
#90679=CARTESIAN_POINT('Ctrl Pts',(-11.0399838036904,20.0241266062625,4.52971680587639));
#90680=CARTESIAN_POINT('Ctrl Pts',(-11.0474347170704,20.0235505979442,4.52211796604934));
#90681=CARTESIAN_POINT('Ctrl Pts',(-11.0498883331428,20.0233595345351,4.51959752375482));
#90682=CARTESIAN_POINT('Ctrl Pts',(-11.0542688719603,20.0230158831839,4.51506509973609));
#90683=CARTESIAN_POINT('Ctrl Pts',(-11.056199158364,20.0228635586798,4.51305643909112));
#90684=CARTESIAN_POINT('Ctrl Pts',(-11.0603868069784,20.0225311359013,4.50867378312491));
#90685=CARTESIAN_POINT('Ctrl Pts',(-11.062641907428,20.0223508760369,4.50629774784673));
#90686=CARTESIAN_POINT('Ctrl Pts',(-11.0672777317011,20.0219777739256,4.50138035720402));
#90687=CARTESIAN_POINT('Ctrl Pts',(-11.069657398808,20.02178485598,4.49883803744669));
#90688=CARTESIAN_POINT('Ctrl Pts',(-11.081242878703,20.0208388876541,4.48637179552282));
#90689=CARTESIAN_POINT('Ctrl Pts',(-11.0903194693153,20.020076852143,4.4763293038851));
#90690=CARTESIAN_POINT('Ctrl Pts',(-11.136606263325,20.0160875150725,4.42366633833537));
#90691=CARTESIAN_POINT('Ctrl Pts',(-11.1714587202384,20.0127314832471,4.37904306255321));
#90692=CARTESIAN_POINT('Ctrl Pts',(-11.232974669029,20.0062460173592,4.29010463783038));
#90693=CARTESIAN_POINT('Ctrl Pts',(-11.2600493420596,20.0031271227852,4.24616862571327));
#90694=CARTESIAN_POINT('Ctrl Pts',(-11.2866954006238,19.9997960348885,4.19732612616028));
#90695=CARTESIAN_POINT('Ctrl Pts',(-11.2886276758864,19.9995528138799,4.19374886908338));
#90696=CARTESIAN_POINT('Ctrl Pts',(-11.3320445888902,19.9940502250727,4.1125630727733));
#90697=CARTESIAN_POINT('Ctrl Pts',(-11.3664655914831,19.9889209772329,4.03136838411564));
#90698=CARTESIAN_POINT('Ctrl Pts',(-11.3966664999606,19.9834476899926,3.93734435758537));
#90699=CARTESIAN_POINT('Ctrl Pts',(-11.3998357262746,19.9828566074109,3.92709173171027));
#90700=CARTESIAN_POINT('Ctrl Pts',(-11.4047360157333,19.9819147347835,3.91059822267615));
#90701=CARTESIAN_POINT('Ctrl Pts',(-11.4065388782858,19.9815616327746,3.90437922810142));
#90702=CARTESIAN_POINT('Ctrl Pts',(-11.4096674852493,19.9809368708083,3.89331295607356));
#90703=CARTESIAN_POINT('Ctrl Pts',(-11.4110096396259,19.9806646852084,3.88847045980617));
#90704=CARTESIAN_POINT('Ctrl Pts',(-11.4137559568959,19.980098856048,3.87835970849104));
#90705=CARTESIAN_POINT('Ctrl Pts',(-11.4151556766407,19.9798053589016,3.87309031968845));
#90706=CARTESIAN_POINT('Ctrl Pts',(-11.4187206257387,19.9790442130742,3.85936095086765));
#90707=CARTESIAN_POINT('Ctrl Pts',(-11.4208396576202,19.9785780473065,3.85088912592739));
#90708=CARTESIAN_POINT('Ctrl Pts',(-11.4252784582874,19.9775703981376,3.83244310763236));
#90709=CARTESIAN_POINT('Ctrl Pts',(-11.4275696356019,19.9770298293959,3.82246247210452));
#90710=CARTESIAN_POINT('Ctrl Pts',(-11.4521868986626,19.970978501996,3.7098181246165));
#90711=CARTESIAN_POINT('Ctrl Pts',(-11.4634999999946,19.9658450492175,3.60506528518567));
#90712=CARTESIAN_POINT('Ctrl Pts',(-11.4635,19.9607369088795,3.50000000007519));
#90713=CARTESIAN_POINT('Ctrl Pts',(-11.4635,19.889530718258,3.4999999999448));
#90714=CARTESIAN_POINT('Ctrl Pts',(-11.4635000000029,19.894098071368,3.57602812264237));
#90715=CARTESIAN_POINT('Ctrl Pts',(-11.4575756192878,19.8986041100056,3.65195075480961));
#90716=CARTESIAN_POINT('Ctrl Pts',(-11.4415950904616,19.9044771054825,3.75369629780065));
#90717=CARTESIAN_POINT('Ctrl Pts',(-11.4366800211121,19.905992131755,3.78019433863034));
#90718=CARTESIAN_POINT('Ctrl Pts',(-11.4293252597365,19.9079367146872,3.81452861641016));
#90719=CARTESIAN_POINT('Ctrl Pts',(-11.4275477866545,19.908386892226,3.82250002989647));
#90720=CARTESIAN_POINT('Ctrl Pts',(-11.424440649886,19.9091418242089,3.83590530237781));
#90721=CARTESIAN_POINT('Ctrl Pts',(-11.4231464049553,19.9094476949911,3.84134710851949));
#90722=CARTESIAN_POINT('Ctrl Pts',(-11.4205283073341,19.9100499139078,3.85208143847751));
#90723=CARTESIAN_POINT('Ctrl Pts',(-11.4192059975401,19.910346305761,3.85737424211584));
#90724=CARTESIAN_POINT('Ctrl Pts',(-11.4166085922903,19.9109139535609,3.86752905926711));
#90725=CARTESIAN_POINT('Ctrl Pts',(-11.4153379857553,19.9111853485035,3.87239213217479));
#90726=CARTESIAN_POINT('Ctrl Pts',(-11.4123735237005,19.9118044773777,3.88350383624424));
#90727=CARTESIAN_POINT('Ctrl Pts',(-11.4106632012984,19.9121516775848,3.88974799191676));
#90728=CARTESIAN_POINT('Ctrl Pts',(-11.4060099170788,19.9130704975451,3.90630452154103));
#90729=CARTESIAN_POINT('Ctrl Pts',(-11.4029949176656,19.9136397978806,3.91659635172702));
#90730=CARTESIAN_POINT('Ctrl Pts',(-11.374848167005,19.9187311807119,4.00890351104174));
#90731=CARTESIAN_POINT('Ctrl Pts',(-11.3426634352935,19.923008432776,4.08859800525403));
#90732=CARTESIAN_POINT('Ctrl Pts',(-11.2813697121994,19.929604024528,4.20875538506209));
#90733=CARTESIAN_POINT('Ctrl Pts',(-11.2568745027884,19.9319766159394,4.25133813497436));
#90734=CARTESIAN_POINT('Ctrl Pts',(-11.2043916657069,19.9367111976816,4.33280185036871));
#90735=CARTESIAN_POINT('Ctrl Pts',(-11.1765449435219,19.9390692419126,4.37169930642364));
#90736=CARTESIAN_POINT('Ctrl Pts',(-11.1289817042751,19.9429781042925,4.43169713660158));
#90737=CARTESIAN_POINT('Ctrl Pts',(-11.1104576700371,19.9444754915997,4.45369952685649));
#90738=CARTESIAN_POINT('Ctrl Pts',(-11.0873876803285,19.946330771025,4.47951760536667));
#90739=CARTESIAN_POINT('Ctrl Pts',(-11.0834502446072,19.9466470988143,4.48387106455671));
#90740=CARTESIAN_POINT('Ctrl Pts',(-11.0772882471084,19.9471418672051,4.49060228352051));
#90741=CARTESIAN_POINT('Ctrl Pts',(-11.0750817145551,19.9473189829016,4.49299655491857));
#90742=CARTESIAN_POINT('Ctrl Pts',(-11.070970406837,19.9476489356556,4.49742789991519));
#90743=CARTESIAN_POINT('Ctrl Pts',(-11.0690677888058,19.9478016115908,4.49946690310272));
#90744=CARTESIAN_POINT('Ctrl Pts',(-11.0647321257125,19.9481494792712,4.50408681455575));
#90745=CARTESIAN_POINT('Ctrl Pts',(-11.0622955292365,19.9483449388795,4.50666431282053));
#90746=CARTESIAN_POINT('Ctrl Pts',(-11.0548368119417,19.9489430750938,4.51449711201356));
#90747=CARTESIAN_POINT('Ctrl Pts',(-11.0497849638866,19.9493479374495,4.51972379360995));
#90748=CARTESIAN_POINT('Ctrl Pts',(-10.9973166870003,19.9535480618291,4.57320476829084));
#90749=CARTESIAN_POINT('Ctrl Pts',(-10.9466519623634,19.9575607837162,4.61814901091992));
#90750=CARTESIAN_POINT('Ctrl Pts',(-10.8155309465143,19.9674944744758,4.71914738886183));
#90751=CARTESIAN_POINT('Ctrl Pts',(-10.7321900783782,19.9734276613691,4.77094935954187));
#90752=CARTESIAN_POINT('Ctrl Pts',(-10.6035892678925,19.981731678141,4.83400441758086));
#90753=CARTESIAN_POINT('Ctrl Pts',(-10.5619730248338,19.9843046070277,4.85206314072622));
#90754=CARTESIAN_POINT('Ctrl Pts',(-10.5098115728236,19.9873909470546,4.87187231149635));
#90755=CARTESIAN_POINT('Ctrl Pts',(-10.5000015117888,19.9879655865824,4.87547808961509));
#90756=CARTESIAN_POINT('Ctrl Pts',(-10.4844409418412,19.9888680814775,4.88100904412464));
#90757=CARTESIAN_POINT('Ctrl Pts',(-10.4787157788796,19.9891982280175,4.88300405302513));
#90758=CARTESIAN_POINT('Ctrl Pts',(-10.4682723614392,19.9897970412564,4.8865705804098));
#90759=CARTESIAN_POINT('Ctrl Pts',(-10.4635581995058,19.9900660861239,4.88815372904553));
#90760=CARTESIAN_POINT('Ctrl Pts',(-10.4533538328366,19.9906457840905,4.89152286464655));
#90761=CARTESIAN_POINT('Ctrl Pts',(-10.4478609314645,19.9909561594179,4.89330045860854));
#90762=CARTESIAN_POINT('Ctrl Pts',(-10.4329018083687,19.9917969707834,4.89804387500847));
#90763=CARTESIAN_POINT('Ctrl Pts',(-10.4234156256785,19.9923253363793,4.9009460612596));
#90764=CARTESIAN_POINT('Ctrl Pts',(-10.3759981773585,19.9949433026962,4.9149272425878));
#90765=CARTESIAN_POINT('Ctrl Pts',(-10.3376569643441,19.9969861760379,4.92456374435216));
#90766=CARTESIAN_POINT('Ctrl Pts',(-10.1933314996131,20.0044628337437,4.95468234666377));
#90767=CARTESIAN_POINT('Ctrl Pts',(-10.085582600919,20.0095961482466,4.96497560605187));
#90768=CARTESIAN_POINT('Ctrl Pts',(-9.93223798521164,20.0171259017573,4.96263666909413));
#90769=CARTESIAN_POINT('Ctrl Pts',(-9.88685558545205,20.0193869070532,4.95982722601458));
#90770=CARTESIAN_POINT('Ctrl Pts',(-9.81920132561252,20.0228969208704,4.95246528142579));
#90771=CARTESIAN_POINT('Ctrl Pts',(-9.79678290986956,20.0240832829943,4.94949862250487));
#90772=CARTESIAN_POINT('Ctrl Pts',(-9.76907088632763,20.0255884524901,4.94517596216321));
#90773=CARTESIAN_POINT('Ctrl Pts',(-9.76370308324525,20.025881813155,4.9443079943049));
#90774=CARTESIAN_POINT('Ctrl Pts',(-9.75522259962754,20.0263483268957,4.94288816855444));
#90775=CARTESIAN_POINT('Ctrl Pts',(-9.75210660161655,20.0265203889804,4.94235609519179));
#90776=CARTESIAN_POINT('Ctrl Pts',(-9.74622973931599,20.0268461714822,4.94133298314577));
#90777=CARTESIAN_POINT('Ctrl Pts',(-9.74346854891021,20.0269997706503,4.94084410247839));
#90778=CARTESIAN_POINT('Ctrl Pts',(-9.73713274226629,20.0273534286572,4.93970353108384));
#90779=CARTESIAN_POINT('Ctrl Pts',(-9.7335591358612,20.0275537865757,4.93904646135372));
#90780=CARTESIAN_POINT('Ctrl Pts',(-9.72401383756117,20.0280912465118,4.9372546180525));
#90781=CARTESIAN_POINT('Ctrl Pts',(-9.71804677158459,20.0284296321021,4.93609594851646));
#90782=CARTESIAN_POINT('Ctrl Pts',(-9.67297060853479,20.0310031405718,4.92705141391336));
#90783=CARTESIAN_POINT('Ctrl Pts',(-9.6341944705975,20.0333152283376,4.91760704557434));
#90784=CARTESIAN_POINT('Ctrl Pts',(-9.51498865217206,20.0406331690028,4.88335665986826));
#90785=CARTESIAN_POINT('Ctrl Pts',(-9.43627649046886,20.0457596692194,4.8531916083317));
#90786=CARTESIAN_POINT('Ctrl Pts',(-9.30808656344019,20.054269218602,4.79092806692027));
#90787=CARTESIAN_POINT('Ctrl Pts',(-9.257149914964,20.0577005568928,4.76230516518392));
#90788=CARTESIAN_POINT('Ctrl Pts',(-9.18058141997299,20.0628992716039,4.7130345388412));
#90789=CARTESIAN_POINT('Ctrl Pts',(-9.15370597226154,20.0647331819932,4.69443972641523));
#90790=CARTESIAN_POINT('Ctrl Pts',(-9.1202265976167,20.067030823902,4.66957791442647));
#90791=CARTESIAN_POINT('Ctrl Pts',(-9.11302914614311,20.0675256000719,4.66412905083237));
#90792=CARTESIAN_POINT('Ctrl Pts',(-9.10151379913323,20.0683186557842,4.65524250614175));
#90793=CARTESIAN_POINT('Ctrl Pts',(-9.09716420560889,20.0686185498206,4.65184644405158));
#90794=CARTESIAN_POINT('Ctrl Pts',(-9.08890345856685,20.0691887985716,4.64532110333304));
#90795=CARTESIAN_POINT('Ctrl Pts',(-9.0849889663023,20.0694593197919,4.64219619445404));
#90796=CARTESIAN_POINT('Ctrl Pts',(-9.0760668757816,20.0700766320864,4.63499845563891));
#90797=CARTESIAN_POINT('Ctrl Pts',(-9.07107000477661,20.0704228917358,4.63091245378506));
#90798=CARTESIAN_POINT('Ctrl Pts',(-9.05807529974231,20.0713248685701,4.62014228900869));
#90799=CARTESIAN_POINT('Ctrl Pts',(-9.05012147631755,20.0718784591431,4.61340544560104));
#90800=CARTESIAN_POINT('Ctrl Pts',(-8.99060649724521,20.0760338106523,4.56189462289946));
#90801=CARTESIAN_POINT('Ctrl Pts',(-8.94216107780299,20.0794856497431,4.51364379344618));
#90802=CARTESIAN_POINT('Ctrl Pts',(-8.82090775052224,20.088594213038,4.37467711684604));
#90803=CARTESIAN_POINT('Ctrl Pts',(-8.75525199999838,20.0940493923356,4.27840623879632));
#90804=CARTESIAN_POINT('Ctrl Pts',(-8.68883131744937,20.101408550492,4.15072465069198));
#90805=CARTESIAN_POINT('Ctrl Pts',(-8.67670198426008,20.1028585582181,4.12569005688965));
#90806=CARTESIAN_POINT('Ctrl Pts',(-8.66291862210883,20.1046595622595,4.09504552216817));
#90807=CARTESIAN_POINT('Ctrl Pts',(-8.66057460421397,20.1049716924913,4.08975027887022));
#90808=CARTESIAN_POINT('Ctrl Pts',(-8.65696872266202,20.1054613020736,4.08147203527022));
#90809=CARTESIAN_POINT('Ctrl Pts',(-8.65568520457998,20.1056375007327,4.07849846162943));
#90810=CARTESIAN_POINT('Ctrl Pts',(-8.65331407255141,20.105966652738,4.07295466815457));
#90811=CARTESIAN_POINT('Ctrl Pts',(-8.65222393429799,20.1061194520176,4.07038558472665));
#90812=CARTESIAN_POINT('Ctrl Pts',(-8.64975561755191,20.1064687898988,4.06452201956107));
#90813=CARTESIAN_POINT('Ctrl Pts',(-8.64838214960475,20.1066656056578,4.06122561313357));
#90814=CARTESIAN_POINT('Ctrl Pts',(-8.64483321232762,20.1071804903288,4.05261935804939));
#90815=CARTESIAN_POINT('Ctrl Pts',(-8.64267690451335,20.1074996534187,4.04730173538273));
#90816=CARTESIAN_POINT('Ctrl Pts',(-8.62860841617458,20.1096237828037,4.01201321328187));
#90817=CARTESIAN_POINT('Ctrl Pts',(-8.61765928472868,20.1114792022709,3.98167026739948));
#90818=CARTESIAN_POINT('Ctrl Pts',(-8.60155070411231,20.1145390255567,3.93194083336622));
#90819=CARTESIAN_POINT('Ctrl Pts',(-8.59577116960505,20.1157234148815,3.91276465707285));
#90820=CARTESIAN_POINT('Ctrl Pts',(-8.56598398722431,20.1223187691706,3.80605334431026));
#90821=CARTESIAN_POINT('Ctrl Pts',(-8.54976519530505,20.1278518134404,3.71654317708157));
#90822=CARTESIAN_POINT('Ctrl Pts',(-8.5365463112622,20.1369153886528,3.56370697262953));
#90823=CARTESIAN_POINT('Ctrl Pts',(-8.53516014243279,20.1405297619297,3.50101843937636));
#90824=CARTESIAN_POINT('Ctrl Pts',(-8.53843054103904,20.1448618922449,3.42335428389944));
#90825=CARTESIAN_POINT('Ctrl Pts',(-8.53929830524962,20.145695511967,3.40829159212638));
#90826=CARTESIAN_POINT('Ctrl Pts',(-8.54089122637371,20.1468916628035,3.3865125576196));
#90827=CARTESIAN_POINT('Ctrl Pts',(-8.54143018333722,20.1472599459972,3.37978392408118));
#90828=CARTESIAN_POINT('Ctrl Pts',(-8.54245381853221,20.1479012922292,3.36802691743868));
#90829=CARTESIAN_POINT('Ctrl Pts',(-8.54291801159393,20.1481749879302,3.36299691396326));
#90830=CARTESIAN_POINT('Ctrl Pts',(-8.54386784882309,20.1487037147638,3.35325588076138));
#90831=CARTESIAN_POINT('Ctrl Pts',(-8.54435033592137,20.1489588406352,3.34854461245758));
#90832=CARTESIAN_POINT('Ctrl Pts',(-8.54569334081858,20.149634973573,3.33603044422757));
#90833=CARTESIAN_POINT('Ctrl Pts',(-8.54659379200469,20.1500547317036,3.32823192388808));
#90834=CARTESIAN_POINT('Ctrl Pts',(-8.55006476100666,20.151560509562,3.30015545562132));
#90835=CARTESIAN_POINT('Ctrl Pts',(-8.55299733502293,20.1526352414854,3.27992414731093));
#90836=CARTESIAN_POINT('Ctrl Pts',(-8.57694637552225,20.1602196344993,3.13600974533993));
#90837=CARTESIAN_POINT('Ctrl Pts',(-8.61336381114822,20.1661953764286,3.01542606630461));
#90838=CARTESIAN_POINT('Ctrl Pts',(-8.68511682441223,20.1747735245407,2.85548579061879));
#90839=CARTESIAN_POINT('Ctrl Pts',(-8.70782597164135,20.1772404552128,2.81108639091288));
#90840=CARTESIAN_POINT('Ctrl Pts',(-8.74473829586202,20.1810376048559,2.74718904692318));
#90841=CARTESIAN_POINT('Ctrl Pts',(-8.75722984462729,20.1822925080247,2.72674164333686));
#90842=CARTESIAN_POINT('Ctrl Pts',(-8.77321883862008,20.1838747351751,2.70195808637215));
#90843=CARTESIAN_POINT('Ctrl Pts',(-8.77624714639873,20.1841734058537,2.69732206636208));
#90844=CARTESIAN_POINT('Ctrl Pts',(-8.78105755855642,20.1846464574002,2.69004833033907));
#90845=CARTESIAN_POINT('Ctrl Pts',(-8.78282211547801,20.1848196949302,2.68739900333979));
#90846=CARTESIAN_POINT('Ctrl Pts',(-8.7861548079016,20.1851463901751,2.6824304693737));
#90847=CARTESIAN_POINT('Ctrl Pts',(-8.78772096234364,20.1852997171273,2.68010999384232));
#90848=CARTESIAN_POINT('Ctrl Pts',(-8.79131437112047,20.1856510475614,2.67481866461764));
#90849=CARTESIAN_POINT('Ctrl Pts',(-8.79334592384373,20.1858493363044,2.67185078298052));
#90850=CARTESIAN_POINT('Ctrl Pts',(-8.79876878814064,20.1863776742684,2.66399087401409));
#90851=CARTESIAN_POINT('Ctrl Pts',(-8.80217900562572,20.1867089410639,2.65911204904806));
#90852=CARTESIAN_POINT('Ctrl Pts',(-8.82682714070199,20.1890954623381,2.62430339839722));
#90853=CARTESIAN_POINT('Ctrl Pts',(-8.84915291529124,20.1912159345142,2.59516319161518));
#90854=CARTESIAN_POINT('Ctrl Pts',(-8.87972668534691,20.1940364214541,2.55822151439551));
#90855=CARTESIAN_POINT('Ctrl Pts',(-8.88700499943113,20.194702149994,2.54963105271912));
#90856=CARTESIAN_POINT('Ctrl Pts',(-8.95147161846621,20.2005438771801,2.47529860735073));
#90857=CARTESIAN_POINT('Ctrl Pts',(-9.01432657908907,20.20585512046,2.41470124228506));
#90858=CARTESIAN_POINT('Ctrl Pts',(-9.14150650408248,20.2155483707541,2.31230548975715));
#90859=CARTESIAN_POINT('Ctrl Pts',(-9.20445396068216,20.2199500440195,2.26925280390683));
#90860=CARTESIAN_POINT('Ctrl Pts',(-9.2802683397965,20.2247912977481,2.22565851654451));
#90861=CARTESIAN_POINT('Ctrl Pts',(-9.29012705390789,20.22541263905,2.22014051957886));
#90862=CARTESIAN_POINT('Ctrl Pts',(-9.30532780934558,20.2263583645299,2.21186222408904));
#90863=CARTESIAN_POINT('Ctrl Pts',(-9.31062446141557,20.2266856428689,2.20901984891106));
#90864=CARTESIAN_POINT('Ctrl Pts',(-9.32029141185334,20.2272789147652,2.20390867235254));
#90865=CARTESIAN_POINT('Ctrl Pts',(-9.32465591580488,20.2275452821668,2.20162915037062));
#90866=CARTESIAN_POINT('Ctrl Pts',(-9.33418522465892,20.2281236643144,2.1967131706401));
#90867=CARTESIAN_POINT('Ctrl Pts',(-9.33935437557597,20.2284353765932,2.19408528804474));
#90868=CARTESIAN_POINT('Ctrl Pts',(-9.35350744191571,20.229283397555,2.18699572113506));
#90869=CARTESIAN_POINT('Ctrl Pts',(-9.36252191641759,20.229817575014,2.1825955201098));
#90870=CARTESIAN_POINT('Ctrl Pts',(-9.40858284789632,20.2325178573159,2.16069546385885));
#90871=CARTESIAN_POINT('Ctrl Pts',(-9.44630887479806,20.2346335084292,2.14466335553089));
#90872=CARTESIAN_POINT('Ctrl Pts',(-9.49715144604226,20.237383787494,2.12553512524404));
#90873=CARTESIAN_POINT('Ctrl Pts',(-9.50970634464722,20.238055059588,2.12100670681927));
#90874=CARTESIAN_POINT('Ctrl Pts',(-9.61741858922705,20.2437543062467,2.08381305978538));
#90875=CARTESIAN_POINT('Ctrl Pts',(-9.71564390338453,20.2485335490283,2.06087005775287));
#90876=CARTESIAN_POINT('Ctrl Pts',(-9.86780638118246,20.2561052832374,2.04152711392916));
#90877=CARTESIAN_POINT('Ctrl Pts',(-9.92048533613664,20.2587614331918,2.03770909016852));
#90878=CARTESIAN_POINT('Ctrl Pts',(-9.98358392284736,20.2621000305162,2.03655557374408));
#90879=CARTESIAN_POINT('Ctrl Pts',(-9.99391929905978,20.2626519388117,2.03647613981034));
#90880=CARTESIAN_POINT('Ctrl Pts',(-10.0083440081236,20.263430325154,2.03651807222002));
#90881=CARTESIAN_POINT('Ctrl Pts',(-10.0124335441541,20.2636519144459,2.03654710305693));
#90882=CARTESIAN_POINT('Ctrl Pts',(-10.019391160707,20.2640305366273,2.03662565926711));
#90883=CARTESIAN_POINT('Ctrl Pts',(-10.0222593511513,20.2641870898066,2.03666647704751));
#90884=CARTESIAN_POINT('Ctrl Pts',(-10.0277627432949,20.2644884120598,2.03676098084255));
#90885=CARTESIAN_POINT('Ctrl Pts',(-10.0303979413271,20.2646331031827,2.03681335365757));
#90886=CARTESIAN_POINT('Ctrl Pts',(-10.0374091493145,20.265019129146,2.03697164541255));
#90887=CARTESIAN_POINT('Ctrl Pts',(-10.041784814132,20.2652611459357,2.03709007827683));
#90888=CARTESIAN_POINT('Ctrl Pts',(-10.0574987389489,20.2661340674989,2.03758595327695));
#90889=CARTESIAN_POINT('Ctrl Pts',(-10.0688327591201,20.2667707669853,2.03807558877922));
#90890=CARTESIAN_POINT('Ctrl Pts',(-10.1604276562741,20.271967304551,2.04310001409775));
#90891=CARTESIAN_POINT('Ctrl Pts',(-10.2401898155471,20.2768026957063,2.05410883386141));
#90892=CARTESIAN_POINT('Ctrl Pts',(-10.3896838983912,20.2860268533023,2.08745705147466));
#90893=CARTESIAN_POINT('Ctrl Pts',(-10.4594546316017,20.2904020272699,2.10858559824966));
#90894=CARTESIAN_POINT('Ctrl Pts',(-10.5596304521911,20.296661804801,2.14728337512537));
#90895=CARTESIAN_POINT('Ctrl Pts',(-10.591443492704,20.2986475688073,2.16088709546936));
#90896=CARTESIAN_POINT('Ctrl Pts',(-10.6364614171583,20.3014516181678,2.18205508334331));
#90897=CARTESIAN_POINT('Ctrl Pts',(-10.6500757115573,20.302298871294,2.18871683751952));
#90898=CARTESIAN_POINT('Ctrl Pts',(-10.6742420256568,20.3038016939787,2.20101080816636));
#90899=CARTESIAN_POINT('Ctrl Pts',(-10.6848329770508,20.3044599242566,2.20656309193725));
#90900=CARTESIAN_POINT('Ctrl Pts',(-10.7007647087862,20.3054497143361,2.21516581931488));
#90901=CARTESIAN_POINT('Ctrl Pts',(-10.7061560943078,20.305784600662,2.21812105835928));
#90902=CARTESIAN_POINT('Ctrl Pts',(-10.7158787468092,20.3063884557543,2.22353039614543));
#90903=CARTESIAN_POINT('Ctrl Pts',(-10.7202163984983,20.3066578341839,2.22597277506286));
#90904=CARTESIAN_POINT('Ctrl Pts',(-10.7295002775941,20.3072343671388,2.23126276655002));
#90905=CARTESIAN_POINT('Ctrl Pts',(-10.7344424899993,20.3075412696311,2.23411728319668));
#90906=CARTESIAN_POINT('Ctrl Pts',(-10.7476810766338,20.30836340778,2.24186723688362));
#90907=CARTESIAN_POINT('Ctrl Pts',(-10.755946104479,20.3088767267961,2.24681584152321));
#90908=CARTESIAN_POINT('Ctrl Pts',(-10.7950240835078,20.3113047345628,2.27074068856318));
#90909=CARTESIAN_POINT('Ctrl Pts',(-10.8251763487629,20.3131806510007,2.29077461979789));
#90910=CARTESIAN_POINT('Ctrl Pts',(-10.8651413145503,20.3156867944579,2.31952011808858));
#90911=CARTESIAN_POINT('Ctrl Pts',(-10.8756239216902,20.3163461281453,2.3272745400654));
#90912=CARTESIAN_POINT('Ctrl Pts',(-10.9946079416295,20.3238613759719,2.4177769071366));
#90913=CARTESIAN_POINT('Ctrl Pts',(-11.0911133593024,20.3301888480836,2.515156556385));
#90914=CARTESIAN_POINT('Ctrl Pts',(-11.1904582184754,20.338656052466,2.64822558186085));
#90915=CARTESIAN_POINT('Ctrl Pts',(-11.2074599293953,20.340197590524,2.67250334696458));
#90916=CARTESIAN_POINT('Ctrl Pts',(-11.226945813418,20.3421010590452,2.7022086836613));
#90917=CARTESIAN_POINT('Ctrl Pts',(-11.2301498895593,20.3424187715151,2.7071581113905));
#90918=CARTESIAN_POINT('Ctrl Pts',(-11.2350798223213,20.3429152410791,2.71487534692116));
#90919=CARTESIAN_POINT('Ctrl Pts',(-11.2368265174964,20.3430926585387,2.71762984874807));
#90920=CARTESIAN_POINT('Ctrl Pts',(-11.2400493021347,20.3434228784913,2.72274987755209));
#90921=CARTESIAN_POINT('Ctrl Pts',(-11.2415278473529,20.3435755175543,2.72511379646284));
#90922=CARTESIAN_POINT('Ctrl Pts',(-11.2448678190451,20.3439229182395,2.7304878889549));
#90923=CARTESIAN_POINT('Ctrl Pts',(-11.2467250788109,20.3441179447524,2.7335005849578));
#90924=CARTESIAN_POINT('Ctrl Pts',(-11.2523432060185,20.3447134725718,2.74268829437434));
#90925=CARTESIAN_POINT('Ctrl Pts',(-11.2560691993536,20.3451161325203,2.74888437162551));
#90926=CARTESIAN_POINT('Ctrl Pts',(-11.2908077781177,20.3489419413125,2.80763365642851));
#90927=CARTESIAN_POINT('Ctrl Pts',(-11.3185479375074,20.3525426105373,2.86204570177406));
#90928=CARTESIAN_POINT('Ctrl Pts',(-11.3893517097413,20.363200834911,3.02541299193128));
#90929=CARTESIAN_POINT('Ctrl Pts',(-11.4228513669856,20.3703211528115,3.13801665847732));
#90930=CARTESIAN_POINT('Ctrl Pts',(-11.4465537972481,20.3783824205192,3.27668071001339));
#90931=CARTESIAN_POINT('Ctrl Pts',(-11.4499675176857,20.3797190755843,3.30004080417767));
#90932=CARTESIAN_POINT('Ctrl Pts',(-11.454858658206,20.3819857504721,3.34029510375796));
#90933=CARTESIAN_POINT('Ctrl Pts',(-11.456610268367,20.3829239293748,3.35715067641398));
#90934=CARTESIAN_POINT('Ctrl Pts',(-11.4586774587503,20.384240732325,3.3810784909363));
#90935=CARTESIAN_POINT('Ctrl Pts',(-11.4592350435477,20.3846268445503,3.38812800115375));
#90936=CARTESIAN_POINT('Ctrl Pts',(-11.4601072646536,20.3852890471085,3.4002748617643));
#90937=CARTESIAN_POINT('Ctrl Pts',(-11.4604463513216,20.3855658931273,3.40537028309883));
#90938=CARTESIAN_POINT('Ctrl Pts',(-11.461043816564,20.386093757596,3.41511816026283));
#90939=CARTESIAN_POINT('Ctrl Pts',(-11.4613066591182,20.3863449115146,3.41977027143469));
#90940=CARTESIAN_POINT('Ctrl Pts',(-11.4619313921308,20.3869952065732,3.43185177820457));
#90941=CARTESIAN_POINT('Ctrl Pts',(-11.4622588719079,20.3873932758838,3.4392828712037));
#90942=CARTESIAN_POINT('Ctrl Pts',(-11.4631764913181,20.3887362282574,3.46446963435414));
#90943=CARTESIAN_POINT('Ctrl Pts',(-11.4635,20.3896728624995,3.48223381506111));
#90944=CARTESIAN_POINT('Ctrl Pts',(-11.4635,20.390600218991,3.49999999999975));
#90945=CARTESIAN_POINT('Origin',(-10.,13.2,3.5));
#90946=CARTESIAN_POINT('',(-11.4635,20.9613838610471,3.50000000002865));
#90947=CARTESIAN_POINT('',(-11.4635,20.8884018418444,3.49999999996669));
#90948=CARTESIAN_POINT('',(-11.4635,13.2,3.5));
#90949=CARTESIAN_POINT('Ctrl Pts',(-11.4635,20.9613838610471,3.50000000002865));
#90950=CARTESIAN_POINT('Ctrl Pts',(-11.4635000000015,20.9566884958894,3.42124724916301));
#90951=CARTESIAN_POINT('Ctrl Pts',(-11.4571434721348,20.9518997548335,3.34261904798223));
#90952=CARTESIAN_POINT('Ctrl Pts',(-11.4331286661958,20.9430155565538,3.19508157007876));
#90953=CARTESIAN_POINT('Ctrl Pts',(-11.4167227184934,20.9389100987044,3.12619260529468));
#90954=CARTESIAN_POINT('Ctrl Pts',(-11.3905528339483,20.9340650164995,3.04343324048439));
#90955=CARTESIAN_POINT('Ctrl Pts',(-11.3854566224749,20.9331762716414,3.02819456757604));
#90956=CARTESIAN_POINT('Ctrl Pts',(-11.3778073980026,20.9319163802089,3.00651552347577));
#90957=CARTESIAN_POINT('Ctrl Pts',(-11.3754581361996,20.9315385925182,3.0000049275953));
#90958=CARTESIAN_POINT('Ctrl Pts',(-11.3713051704093,20.9308862479867,2.9887464709405));
#90959=CARTESIAN_POINT('Ctrl Pts',(-11.3695227892526,20.9306109929557,2.98399091869568));
#90960=CARTESIAN_POINT('Ctrl Pts',(-11.3660468584145,20.9300831216393,2.97486170757454));
#90961=CARTESIAN_POINT('Ctrl Pts',(-11.3643569703184,20.9298303880588,2.97048672934046));
#90962=CARTESIAN_POINT('Ctrl Pts',(-11.360317984819,20.9292353909773,2.96017784564874));
#90963=CARTESIAN_POINT('Ctrl Pts',(-11.3579510357184,20.9288937256505,2.95425100596183));
#90964=CARTESIAN_POINT('Ctrl Pts',(-11.3495391842833,20.9277034784807,2.93358131525659));
#90965=CARTESIAN_POINT('Ctrl Pts',(-11.3432922327071,20.92686165002,2.91892157149693));
#90966=CARTESIAN_POINT('Ctrl Pts',(-11.2862567703959,20.919524474884,2.79091435411472));
#90967=CARTESIAN_POINT('Ctrl Pts',(-11.2214726632592,20.9135689753299,2.68436174290968));
#90968=CARTESIAN_POINT('Ctrl Pts',(-11.1374322571354,20.9069960955733,2.57902704816759));
#90969=CARTESIAN_POINT('Ctrl Pts',(-11.1307707738241,20.9064810956157,2.57086019777578));
#90970=CARTESIAN_POINT('Ctrl Pts',(-11.093548450587,20.9036322660254,2.52621958308996));
#90971=CARTESIAN_POINT('Ctrl Pts',(-11.0613127912209,20.9012709048846,2.49118332353302));
#90972=CARTESIAN_POINT('Ctrl Pts',(-11.0164020946423,20.8980219838253,2.44690985430923));
#90973=CARTESIAN_POINT('Ctrl Pts',(-11.0052022405265,20.897214819632,2.43621407474553));
#90974=CARTESIAN_POINT('Ctrl Pts',(-10.9885461216265,20.8960151428804,2.42080551798409));
#90975=CARTESIAN_POINT('Ctrl Pts',(-10.9832211047394,20.8956317058716,2.41595183695281));
#90976=CARTESIAN_POINT('Ctrl Pts',(-10.9736336167589,20.8949410688944,2.40734172433269));
#90977=CARTESIAN_POINT('Ctrl Pts',(-10.969384666537,20.894634900307,2.40357038838521));
#90978=CARTESIAN_POINT('Ctrl Pts',(-10.9626836765125,20.8941516993163,2.39769203931977));
#90979=CARTESIAN_POINT('Ctrl Pts',(-10.9602463840394,20.8939758780837,2.39556820820464));
#90980=CARTESIAN_POINT('Ctrl Pts',(-10.9577922516998,20.8937987479549,2.39344396763952));
#90981=CARTESIAN_POINT('Ctrl Pts',(-10.9577824043896,20.8937980372112,2.39343544426394));
#90982=CARTESIAN_POINT('Ctrl Pts',(-10.9577625910322,20.8937966071508,2.39341829520226));
#90983=CARTESIAN_POINT('Ctrl Pts',(-10.9577526250649,20.8937958878398,2.39340966959089));
#90984=CARTESIAN_POINT('Ctrl Pts',(-10.9577325723636,20.8937944404981,2.39339231431746));
#90985=CARTESIAN_POINT('Ctrl Pts',(-10.9577224855433,20.8937937124611,2.39338358458646));
#90986=CARTESIAN_POINT('Ctrl Pts',(-10.9577021890507,20.8937922475169,2.39336601928647));
#90987=CARTESIAN_POINT('Ctrl Pts',(-10.9576919792924,20.8937915106034,2.39335718364902));
#90988=CARTESIAN_POINT('Ctrl Pts',(-10.9576714346564,20.8937900277423,2.39333940459143));
#90989=CARTESIAN_POINT('Ctrl Pts',(-10.9576610998094,20.8937892817969,2.39333046120418));
#90990=CARTESIAN_POINT('Ctrl Pts',(-10.955543813586,20.8936364606164,2.39149829332148));
#90991=CARTESIAN_POINT('Ctrl Pts',(-10.9534317135231,20.8934839401861,2.38968113558982));
#90992=CARTESIAN_POINT('Ctrl Pts',(-10.9486368968294,20.8931375324251,2.38557965608107));
#90993=CARTESIAN_POINT('Ctrl Pts',(-10.9459511253157,20.8929433859604,2.38329899572709));
#90994=CARTESIAN_POINT('Ctrl Pts',(-10.9389884904475,20.8924398564311,2.37742971949755));
#90995=CARTESIAN_POINT('Ctrl Pts',(-10.9346993211786,20.8921294545162,2.37385587209659));
#90996=CARTESIAN_POINT('Ctrl Pts',(-10.9077062966974,20.8901752461793,2.35162502672633));
#90997=CARTESIAN_POINT('Ctrl Pts',(-10.8844666890242,20.8884895356405,2.3336320316125));
#90998=CARTESIAN_POINT('Ctrl Pts',(-10.7739230435552,20.8805162809182,2.25324897094252));
#90999=CARTESIAN_POINT('Ctrl Pts',(-10.6804677286658,20.8739303276766,2.19988095798401));
#91000=CARTESIAN_POINT('Ctrl Pts',(-10.5193331488387,20.8635097544077,2.13003916366665));
#91001=CARTESIAN_POINT('Ctrl Pts',(-10.4548186481774,20.8595505648093,2.10728983163349));
#91002=CARTESIAN_POINT('Ctrl Pts',(-10.3737281073614,20.854857397976,2.08493510917998));
#91003=CARTESIAN_POINT('Ctrl Pts',(-10.3584457304731,20.8539846334208,2.08098695242332));
#91004=CARTESIAN_POINT('Ctrl Pts',(-10.3364215302781,20.8527431929175,2.07567558864699));
#91005=CARTESIAN_POINT('Ctrl Pts',(-10.3297296752626,20.8523681395848,2.07411156876902));
#91006=CARTESIAN_POINT('Ctrl Pts',(-10.3180819573915,20.8517189926481,2.07147564813582));
#91007=CARTESIAN_POINT('Ctrl Pts',(-10.3131311194847,20.8514442196876,2.07038226843804));
#91008=CARTESIAN_POINT('Ctrl Pts',(-10.3035783435721,20.8509162108358,2.06832456694155));
#91009=CARTESIAN_POINT('Ctrl Pts',(-10.2989772505817,20.8506628639093,2.06735665266818));
#91010=CARTESIAN_POINT('Ctrl Pts',(-10.2880746531643,20.8500647958731,2.06511792583211));
#91011=CARTESIAN_POINT('Ctrl Pts',(-10.2817692534615,20.8497206882825,2.0638664191107));
#91012=CARTESIAN_POINT('Ctrl Pts',(-10.2595367102829,20.8485134826897,2.05960572454648));
#91013=CARTESIAN_POINT('Ctrl Pts',(-10.243567702511,20.8476573987832,2.05681956271455));
#91014=CARTESIAN_POINT('Ctrl Pts',(-10.1078104846959,20.8404654213748,2.03545119233245));
#91015=CARTESIAN_POINT('Ctrl Pts',(-9.98619094863813,20.8346392857349,2.03155249908111));
#91016=CARTESIAN_POINT('Ctrl Pts',(-9.80821563139624,20.8259285765369,2.04798154784805));
#91017=CARTESIAN_POINT('Ctrl Pts',(-9.75132118218259,20.8231057413387,2.0566369880701));
#91018=CARTESIAN_POINT('Ctrl Pts',(-9.66954216945178,20.818818723098,2.07405748298735));
#91019=CARTESIAN_POINT('Ctrl Pts',(-9.64414836847395,20.8174543131188,2.08018174105154));
#91020=CARTESIAN_POINT('Ctrl Pts',(-9.61344604106461,20.8157492806381,2.08846162265551));
#91021=CARTESIAN_POINT('Ctrl Pts',(-9.60796719937263,20.8154428458867,2.08997346302112));
#91022=CARTESIAN_POINT('Ctrl Pts',(-9.59940358505597,20.8149602768334,2.09239028976283));
#91023=CARTESIAN_POINT('Ctrl Pts',(-9.5963126919099,20.8147853645206,2.09327360837324));
#91024=CARTESIAN_POINT('Ctrl Pts',(-9.59054176420462,20.8144573688773,2.09494341597724));
#91025=CARTESIAN_POINT('Ctrl Pts',(-9.58786105753331,20.8143044299725,2.0957273972463));
#91026=CARTESIAN_POINT('Ctrl Pts',(-9.58172649798214,20.8139531261873,2.09754054755735));
#91027=CARTESIAN_POINT('Ctrl Pts',(-9.57827420040487,20.8137544712946,2.09857480127582));
#91028=CARTESIAN_POINT('Ctrl Pts',(-9.56922865056005,20.8132315245625,2.10132115537344));
#91029=CARTESIAN_POINT('Ctrl Pts',(-9.56364183803928,20.8129060827301,2.1030540389614));
#91030=CARTESIAN_POINT('Ctrl Pts',(-9.52513661950051,20.8106468455845,2.11525087553652));
#91031=CARTESIAN_POINT('Ctrl Pts',(-9.49258960908891,20.8086552152174,2.12684316490263));
#91032=CARTESIAN_POINT('Ctrl Pts',(-9.43313310578712,20.8049016749588,2.15042228365196));
#91033=CARTESIAN_POINT('Ctrl Pts',(-9.40611468908789,20.8031501745572,2.16209185516065));
#91034=CARTESIAN_POINT('Ctrl Pts',(-9.30617271356306,20.7965392716831,2.20888205228234));
#91035=CARTESIAN_POINT('Ctrl Pts',(-9.23584606064211,20.7916267791755,2.24921951193989));
#91036=CARTESIAN_POINT('Ctrl Pts',(-9.11908595498904,20.7832592713526,2.3297306721709));
#91037=CARTESIAN_POINT('Ctrl Pts',(-9.07115966331733,20.7797501902482,2.3673937441244));
#91038=CARTESIAN_POINT('Ctrl Pts',(-9.01462412332571,20.7755293273988,2.4178320225422));
#91039=CARTESIAN_POINT('Ctrl Pts',(-9.00368468848392,20.7747082759455,2.42789507383177));
#91040=CARTESIAN_POINT('Ctrl Pts',(-8.98803283551275,20.7735268174833,2.44273952670517));
#91041=CARTESIAN_POINT('Ctrl Pts',(-8.98319726108917,20.7731608519179,2.44738922548098));
#91042=CARTESIAN_POINT('Ctrl Pts',(-8.97478253016123,20.7725222597703,2.45559259637408));
#91043=CARTESIAN_POINT('Ctrl Pts',(-8.97118948139539,20.7722490158112,2.45913180329861));
#91044=CARTESIAN_POINT('Ctrl Pts',(-8.96425129159652,20.7717202398729,2.46603705007871));
#91045=CARTESIAN_POINT('Ctrl Pts',(-8.96090408995374,20.7714646185943,2.46940092216979));
#91046=CARTESIAN_POINT('Ctrl Pts',(-8.95202405150034,20.7707850189206,2.47841242772935));
#91047=CARTESIAN_POINT('Ctrl Pts',(-8.94652047382456,20.7703623145763,2.48408875992992));
#91048=CARTESIAN_POINT('Ctrl Pts',(-8.92671803572117,20.7688355584821,2.50484675792464));
#91049=CARTESIAN_POINT('Ctrl Pts',(-8.91269447507775,20.7677432137784,2.52018833319449));
#91050=CARTESIAN_POINT('Ctrl Pts',(-8.8165888678351,20.760163670269,2.62993186321281));
#91051=CARTESIAN_POINT('Ctrl Pts',(-8.74658411849937,20.7542053861851,2.73421258703406));
#91052=CARTESIAN_POINT('Ctrl Pts',(-8.66845912207229,20.7456481831522,2.89064997688716));
#91053=CARTESIAN_POINT('Ctrl Pts',(-8.64851249880959,20.7431848872761,2.93627183374724));
#91054=CARTESIAN_POINT('Ctrl Pts',(-8.62247140949482,20.7393928630961,3.00520704998095));
#91055=CARTESIAN_POINT('Ctrl Pts',(-8.61456445921144,20.7381392244046,3.02779950017673));
#91056=CARTESIAN_POINT('Ctrl Pts',(-8.605515885078,20.7365584842016,3.05584131981198));
#91057=CARTESIAN_POINT('Ctrl Pts',(-8.60384623578679,20.7362599762067,3.0611178465059));
#91058=CARTESIAN_POINT('Ctrl Pts',(-8.60126388452743,20.7357871614945,3.06944262469));
#91059=CARTESIAN_POINT('Ctrl Pts',(-8.60033110935933,20.7356139967324,3.07248465485085));
#91060=CARTESIAN_POINT('Ctrl Pts',(-8.59859655005347,20.7352874253576,3.07820804530214));
#91061=CARTESIAN_POINT('Ctrl Pts',(-8.59779253292075,20.7351341493173,3.08088867661833));
#91062=CARTESIAN_POINT('Ctrl Pts',(-8.59597308611298,20.7347829216217,3.08701863957445));
#91063=CARTESIAN_POINT('Ctrl Pts',(-8.59496267701831,20.7345846847845,3.09046941574758));
#91064=CARTESIAN_POINT('Ctrl Pts',(-8.59231364197492,20.7340564576069,3.09964167543322));
#91065=CARTESIAN_POINT('Ctrl Pts',(-8.59069720017489,20.733725249986,3.10536943026507));
#91066=CARTESIAN_POINT('Ctrl Pts',(-8.57936178000041,20.7313383910769,3.14649374141286));
#91067=CARTESIAN_POINT('Ctrl Pts',(-8.57094333208066,20.7292174935674,3.18223242306017));
#91068=CARTESIAN_POINT('Ctrl Pts',(-8.56183881258576,20.7264358883531,3.22863897155574));
#91069=CARTESIAN_POINT('Ctrl Pts',(-8.55991282253501,20.7258098789813,3.23905302617854));
#91070=CARTESIAN_POINT('Ctrl Pts',(-8.54307715898259,20.7199732890585,3.33595551281808));
#91071=CARTESIAN_POINT('Ctrl Pts',(-8.5358624844121,20.7146225471786,3.42360058363659));
#91072=CARTESIAN_POINT('Ctrl Pts',(-8.53713576986994,20.704889451098,3.5875411182641));
#91073=CARTESIAN_POINT('Ctrl Pts',(-8.54367389731852,20.700485462885,3.66356136209694));
#91074=CARTESIAN_POINT('Ctrl Pts',(-8.55794609596348,20.6956421867867,3.74988072813913));
#91075=CARTESIAN_POINT('Ctrl Pts',(-8.55991770669952,20.6950209413873,3.76100352300825));
#91076=CARTESIAN_POINT('Ctrl Pts',(-8.56313523722941,20.6940753987287,3.77800722371377));
#91077=CARTESIAN_POINT('Ctrl Pts',(-8.56428891014575,20.6937482079167,3.78390496808598));
#91078=CARTESIAN_POINT('Ctrl Pts',(-8.56645355672026,20.6931551140177,3.79462021795071));
#91079=CARTESIAN_POINT('Ctrl Pts',(-8.56745256653365,20.6928888371694,3.79944002664116));
#91080=CARTESIAN_POINT('Ctrl Pts',(-8.56968089652382,20.6923106748737,3.80992435984508));
#91081=CARTESIAN_POINT('Ctrl Pts',(-8.57091959411294,20.6919990915232,3.81558682074617));
#91082=CARTESIAN_POINT('Ctrl Pts',(-8.57439249473232,20.6911514813904,3.83102265485876));
#91083=CARTESIAN_POINT('Ctrl Pts',(-8.57669355626136,20.6906175833299,3.84078076678931));
#91084=CARTESIAN_POINT('Ctrl Pts',(-8.58889737310922,20.68791979675,3.89025221820011));
#91085=CARTESIAN_POINT('Ctrl Pts',(-8.60036311749825,20.6858062532142,3.92956304204687));
#91086=CARTESIAN_POINT('Ctrl Pts',(-8.61777109271493,20.6830520201436,3.98109953692637));
#91087=CARTESIAN_POINT('Ctrl Pts',(-8.62225551825075,20.6823748335203,3.9937951709245));
#91088=CARTESIAN_POINT('Ctrl Pts',(-8.67225012357295,20.6751493674886,4.12934643792311));
#91089=CARTESIAN_POINT('Ctrl Pts',(-8.73387908575262,20.6690544698455,4.24560600476089));
#91090=CARTESIAN_POINT('Ctrl Pts',(-8.82714833275273,20.6608812035185,4.37584471751621));
#91091=CARTESIAN_POINT('Ctrl Pts',(-8.84485643189269,20.6593613638933,4.39907069331645));
#91092=CARTESIAN_POINT('Ctrl Pts',(-8.86694345872554,20.6574822527619,4.42630966016178));
#91093=CARTESIAN_POINT('Ctrl Pts',(-8.87066816095837,20.6571658993751,4.43084709121206));
#91094=CARTESIAN_POINT('Ctrl Pts',(-8.87650062091459,20.6566711363923,4.4378656582528));
#91095=CARTESIAN_POINT('Ctrl Pts',(-8.87858957183165,20.6564940522166,4.44036242954924));
#91096=CARTESIAN_POINT('Ctrl Pts',(-8.88248287099121,20.6561641878848,4.44498438530276));
#91097=CARTESIAN_POINT('Ctrl Pts',(-8.8842849705884,20.6560115689693,4.44711139516433));
#91098=CARTESIAN_POINT('Ctrl Pts',(-8.888392346421,20.6556638732756,4.45193132131147));
#91099=CARTESIAN_POINT('Ctrl Pts',(-8.89070132633105,20.6554685291409,4.45462100754157));
#91100=CARTESIAN_POINT('Ctrl Pts',(-8.89777042974374,20.6548708900156,4.46279539122287));
#91101=CARTESIAN_POINT('Ctrl Pts',(-8.90256155219291,20.6544664137501,4.46825298333638));
#91102=CARTESIAN_POINT('Ctrl Pts',(-8.95554832763693,20.6500016622017,4.5277119891248));
#91103=CARTESIAN_POINT('Ctrl Pts',(-9.0076414177821,20.6456930284718,4.57809716581572));
#91104=CARTESIAN_POINT('Ctrl Pts',(-9.10628639507191,20.6379762913093,4.66027895616951));
#91105=CARTESIAN_POINT('Ctrl Pts',(-9.15135727437918,20.634589900873,4.69364026220984));
#91106=CARTESIAN_POINT('Ctrl Pts',(-9.26645628537517,20.6263961081862,4.76901410465484));
#91107=CARTESIAN_POINT('Ctrl Pts',(-9.3383047623977,20.6216650822126,4.80791667775934));
#91108=CARTESIAN_POINT('Ctrl Pts',(-9.42349604610924,20.6165156476931,4.84521595332661));
#91109=CARTESIAN_POINT('Ctrl Pts',(-9.4340149421953,20.6158871999292,4.84967540345245));
#91110=CARTESIAN_POINT('Ctrl Pts',(-9.45017003179515,20.6149330363354,4.85630221363035));
#91111=CARTESIAN_POINT('Ctrl Pts',(-9.45576904773861,20.6146043446668,4.8585585599309));
#91112=CARTESIAN_POINT('Ctrl Pts',(-9.46600310121169,20.6140071459131,4.86260935821819));
#91113=CARTESIAN_POINT('Ctrl Pts',(-9.47063360558834,20.6137382698475,4.8644149560642));
#91114=CARTESIAN_POINT('Ctrl Pts',(-9.48067947328153,20.6131577882854,4.86827335688927));
#91115=CARTESIAN_POINT('Ctrl Pts',(-9.48609801795175,20.6128464680661,4.87031767952266));
#91116=CARTESIAN_POINT('Ctrl Pts',(-9.5009089159111,20.6120002778584,4.87580536758673));
#91117=CARTESIAN_POINT('Ctrl Pts',(-9.51032476145337,20.6114675245657,4.87918471826834));
#91118=CARTESIAN_POINT('Ctrl Pts',(-9.55816219279598,20.6087861884441,4.89580192552832));
#91119=CARTESIAN_POINT('Ctrl Pts',(-9.59709031072738,20.6066871940358,4.90753253259805));
#91120=CARTESIAN_POINT('Ctrl Pts',(-9.64964362236174,20.6039393299958,4.92100947640338));
#91121=CARTESIAN_POINT('Ctrl Pts',(-9.66287522881874,20.603254541555,4.92420659445815));
#91122=CARTESIAN_POINT('Ctrl Pts',(-9.80407915310314,20.5960121157417,4.95624718476087));
#91123=CARTESIAN_POINT('Ctrl Pts',(-9.93531412083742,20.5899100079538,4.96794086071377));
#91124=CARTESIAN_POINT('Ctrl Pts',(-10.0955230028228,20.5817276127359,4.96067148000949));
#91125=CARTESIAN_POINT('Ctrl Pts',(-10.1246607228169,20.5802070729755,4.95847361732146));
#91126=CARTESIAN_POINT('Ctrl Pts',(-10.1595498760166,20.5783271782173,4.95478883641113));
#91127=CARTESIAN_POINT('Ctrl Pts',(-10.1653847818272,20.5780107830154,4.95413706131149));
#91128=CARTESIAN_POINT('Ctrl Pts',(-10.174448739469,20.5775159686562,4.95306933287671));
#91129=CARTESIAN_POINT('Ctrl Pts',(-10.1776806587125,20.5773388753632,4.95267767654967));
#91130=CARTESIAN_POINT('Ctrl Pts',(-10.1836776592562,20.577009002979,4.95193062488643));
#91131=CARTESIAN_POINT('Ctrl Pts',(-10.1864430465042,20.5768563851983,4.95157811088977));
#91132=CARTESIAN_POINT('Ctrl Pts',(-10.192722281388,20.5765087037073,4.95075943442791));
#91133=CARTESIAN_POINT('Ctrl Pts',(-10.1962354381214,20.576313372731,4.95028840807772));
#91134=CARTESIAN_POINT('Ctrl Pts',(-10.2053465379557,20.5758047631845,4.94903312643694));
#91135=CARTESIAN_POINT('Ctrl Pts',(-10.2109416565452,20.5754904321555,4.94822920063906));
#91136=CARTESIAN_POINT('Ctrl Pts',(-10.2468386063077,20.5734615595297,4.94285896966273));
#91137=CARTESIAN_POINT('Ctrl Pts',(-10.2769933771252,20.5717014538664,4.93737458772868));
#91138=CARTESIAN_POINT('Ctrl Pts',(-10.4488422888724,20.5614328355315,4.90051142392588));
#91139=CARTESIAN_POINT('Ctrl Pts',(-10.5854259286604,20.5524375547913,4.84914025540655));
#91140=CARTESIAN_POINT('Ctrl Pts',(-10.7465100432677,20.5418302924739,4.75940242629095));
#91141=CARTESIAN_POINT('Ctrl Pts',(-10.7800064589469,20.5396170533657,4.73893585454775));
#91142=CARTESIAN_POINT('Ctrl Pts',(-10.8206055595114,20.5369241247869,4.71182938158522));
#91143=CARTESIAN_POINT('Ctrl Pts',(-10.828516701172,20.5363988326869,4.70643442274162));
#91144=CARTESIAN_POINT('Ctrl Pts',(-10.8410011135454,20.5355688725945,4.69774002388942));
#91145=CARTESIAN_POINT('Ctrl Pts',(-10.8456091523379,20.5352623096942,4.69449118897344));
#91146=CARTESIAN_POINT('Ctrl Pts',(-10.8542551316687,20.5346866513018,4.68832035284328));
#91147=CARTESIAN_POINT('Ctrl Pts',(-10.8582971328054,20.5344173389875,4.68540420263811));
#91148=CARTESIAN_POINT('Ctrl Pts',(-10.8673684293265,20.5338124608504,4.67878888435012));
#91149=CARTESIAN_POINT('Ctrl Pts',(-10.8723891279557,20.5334773488524,4.67507805576253));
#91150=CARTESIAN_POINT('Ctrl Pts',(-10.8851720995358,20.5326231910664,4.66550299960771));
#91151=CARTESIAN_POINT('Ctrl Pts',(-10.8928999931483,20.5321059142689,4.65959324601958));
#91152=CARTESIAN_POINT('Ctrl Pts',(-10.9402818909444,20.5289277042012,4.62260434650245));
#91153=CARTESIAN_POINT('Ctrl Pts',(-10.9783700193084,20.5263455139822,4.58957025861108));
#91154=CARTESIAN_POINT('Ctrl Pts',(-11.1109874611881,20.5171190844727,4.4619768639741));
#91155=CARTESIAN_POINT('Ctrl Pts',(-11.194136314116,20.5109117001381,4.35657726243979));
#91156=CARTESIAN_POINT('Ctrl Pts',(-11.2767249500379,20.5025961367532,4.21601040281057));
#91157=CARTESIAN_POINT('Ctrl Pts',(-11.2908568794953,20.501065591186,4.19020705515303));
#91158=CARTESIAN_POINT('Ctrl Pts',(-11.3068697369986,20.4991744977396,4.15875514703171));
#91159=CARTESIAN_POINT('Ctrl Pts',(-11.3095069588764,20.4988575075804,4.15349703558725));
#91160=CARTESIAN_POINT('Ctrl Pts',(-11.313555429092,20.4983619622567,4.14530225429773));
#91161=CARTESIAN_POINT('Ctrl Pts',(-11.3149887210578,20.4981847392783,4.14237646887631));
#91162=CARTESIAN_POINT('Ctrl Pts',(-11.31763019005,20.4978547521786,4.13693853929639));
#91163=CARTESIAN_POINT('Ctrl Pts',(-11.3188409658966,20.4977021503595,4.1344277160232));
#91164=CARTESIAN_POINT('Ctrl Pts',(-11.3215736284869,20.4973546700867,4.12871928174073));
#91165=CARTESIAN_POINT('Ctrl Pts',(-11.3230910803971,20.4971595256465,4.1255196105431));
#91166=CARTESIAN_POINT('Ctrl Pts',(-11.326995846302,20.4966517170909,4.11720831331439));
#91167=CARTESIAN_POINT('Ctrl Pts',(-11.3293652196803,20.4963380058488,4.11208838310404));
#91168=CARTESIAN_POINT('Ctrl Pts',(-11.3443299348688,20.4943211291711,4.0792546713723));
#91169=CARTESIAN_POINT('Ctrl Pts',(-11.3560867670352,20.4925729981713,4.05116908989277));
#91170=CARTESIAN_POINT('Ctrl Pts',(-11.4034028041339,20.4848353898071,3.92743813517331));
#91171=CARTESIAN_POINT('Ctrl Pts',(-11.4297807441703,20.478584085687,3.82858823475624));
#91172=CARTESIAN_POINT('Ctrl Pts',(-11.4575117149778,20.4679876099714,3.65260042666487));
#91173=CARTESIAN_POINT('Ctrl Pts',(-11.4634769354391,20.4635722569285,3.57658548729573));
#91174=CARTESIAN_POINT('Ctrl Pts',(-11.4634999778476,20.4593334002854,3.50029468859335));
#91175=CARTESIAN_POINT('Ctrl Pts',(-11.4635,20.459325214305,3.50014734427607));
#91176=CARTESIAN_POINT('Ctrl Pts',(-11.4635,20.459317028952,3.5000000000001));
#91177=CARTESIAN_POINT('Ctrl Pts',(-11.4635,20.390600218991,3.49999999999975));
#91178=CARTESIAN_POINT('Ctrl Pts',(-11.4635,20.390607428758,3.50013812385499));
#91179=CARTESIAN_POINT('Ctrl Pts',(-11.4634999805033,20.3906146379989,3.50027624782956));
#91180=CARTESIAN_POINT('Ctrl Pts',(-11.4634741169183,20.3953818886303,3.59162099111268));
#91181=CARTESIAN_POINT('Ctrl Pts',(-11.4549227392133,20.3998676312033,3.68262807373579));
#91182=CARTESIAN_POINT('Ctrl Pts',(-11.4187105930484,20.4093415908848,3.87388767578039));
#91183=CARTESIAN_POINT('Ctrl Pts',(-11.3887498446853,20.4142928448941,3.97318077703706));
#91184=CARTESIAN_POINT('Ctrl Pts',(-11.3444555861568,20.4203180210045,4.07825967081919));
#91185=CARTESIAN_POINT('Ctrl Pts',(-11.3402234602025,20.4208846136783,4.08800181442585));
#91186=CARTESIAN_POINT('Ctrl Pts',(-11.3341467485738,20.4216868979981,4.10158360618573));
#91187=CARTESIAN_POINT('Ctrl Pts',(-11.3323907713043,20.4219174723696,4.10546280941432));
#91188=CARTESIAN_POINT('Ctrl Pts',(-11.3295298988873,20.4222911999234,4.11171016563223));
#91189=CARTESIAN_POINT('Ctrl Pts',(-11.3284355327981,20.4224337156073,4.11408314889006));
#91190=CARTESIAN_POINT('Ctrl Pts',(-11.3261174822221,20.4227346799665,4.11907432974894));
#91191=CARTESIAN_POINT('Ctrl Pts',(-11.3248923929248,20.4228932169853,4.12169184420796));
#91192=CARTESIAN_POINT('Ctrl Pts',(-11.3218682669134,20.4232832599149,4.12810362848368));
#91193=CARTESIAN_POINT('Ctrl Pts',(-11.3200606450264,20.423515285491,4.13189380100151));
#91194=CARTESIAN_POINT('Ctrl Pts',(-11.3134381352104,20.4243611882083,4.1456272667948));
#91195=CARTESIAN_POINT('Ctrl Pts',(-11.3085271303932,20.4249806170377,4.15552348290582));
#91196=CARTESIAN_POINT('Ctrl Pts',(-11.2760832204036,20.4290186013033,4.21908397511318));
#91197=CARTESIAN_POINT('Ctrl Pts',(-11.245369281037,20.4325946070711,4.27105394129202));
#91198=CARTESIAN_POINT('Ctrl Pts',(-11.1793753163977,20.4396507046261,4.36844336828949));
#91199=CARTESIAN_POINT('Ctrl Pts',(-11.1444473983025,20.4431207221245,4.41398050987996));
#91200=CARTESIAN_POINT('Ctrl Pts',(-11.0506532432454,20.4516826729866,4.52243007014784));
#91201=CARTESIAN_POINT('Ctrl Pts',(-10.9887326843839,20.4566917543782,4.58242651751467));
#91202=CARTESIAN_POINT('Ctrl Pts',(-10.9135597045607,20.4620560648074,4.64339666730071));
#91203=CARTESIAN_POINT('Ctrl Pts',(-10.9051559833319,20.4626468172799,4.65006083623498));
#91204=CARTESIAN_POINT('Ctrl Pts',(-10.891562833795,20.4635883294865,4.66059893161671));
#91205=CARTESIAN_POINT('Ctrl Pts',(-10.8864197407251,20.4639413974254,4.66453175646391));
#91206=CARTESIAN_POINT('Ctrl Pts',(-10.8772377663721,20.4645661957537,4.67145696243838));
#91207=CARTESIAN_POINT('Ctrl Pts',(-10.8732092729814,20.4648384511188,4.67446289002655));
#91208=CARTESIAN_POINT('Ctrl Pts',(-10.8647763577664,20.4654045215651,4.68068787611257));
#91209=CARTESIAN_POINT('Ctrl Pts',(-10.860369256452,20.4656981895318,4.68390318582672));
#91210=CARTESIAN_POINT('Ctrl Pts',(-10.8488536213085,20.4664599885719,4.69220643994294));
#91211=CARTESIAN_POINT('Ctrl Pts',(-10.8417172389066,20.466926632797,4.69725551159592));
#91212=CARTESIAN_POINT('Ctrl Pts',(-10.8101027530645,20.4689705427825,4.71920072681514));
#91213=CARTESIAN_POINT('Ctrl Pts',(-10.7851572419888,20.4705221013258,4.73541294661557));
#91214=CARTESIAN_POINT('Ctrl Pts',(-10.7163672564936,20.4746552512933,4.77719404635434));
#91215=CARTESIAN_POINT('Ctrl Pts',(-10.6716583565793,20.4771869779718,4.80126179547164));
#91216=CARTESIAN_POINT('Ctrl Pts',(-10.5646561713394,20.4830070221092,4.85187603736339));
#91217=CARTESIAN_POINT('Ctrl Pts',(-10.501595306771,20.4862581184921,4.87652004682003));
#91218=CARTESIAN_POINT('Ctrl Pts',(-10.3734075435223,20.4928459924698,4.91663227259763));
#91219=CARTESIAN_POINT('Ctrl Pts',(-10.3084779367331,20.4961747805824,4.93217300959891));
#91220=CARTESIAN_POINT('Ctrl Pts',(-10.2355561858,20.5001194633601,4.94443703883215));
#91221=CARTESIAN_POINT('Ctrl Pts',(-10.2283799741315,20.5005098602532,4.94558903526506));
#91222=CARTESIAN_POINT('Ctrl Pts',(-10.2176896406082,20.5010950938128,4.94722356589499));
#91223=CARTESIAN_POINT('Ctrl Pts',(-10.2141817533489,20.5012877158291,4.94774687197062));
#91224=CARTESIAN_POINT('Ctrl Pts',(-10.2079122320455,20.5016330823566,4.9486588733908));
#91225=CARTESIAN_POINT('Ctrl Pts',(-10.2051513554318,20.5017855526473,4.94905243138268));
#91226=CARTESIAN_POINT('Ctrl Pts',(-10.1991644832941,20.5021170224225,4.94988839604609));
#91227=CARTESIAN_POINT('Ctrl Pts',(-10.1959381761234,20.50229617508,4.95032792261136));
#91228=CARTESIAN_POINT('Ctrl Pts',(-10.1868909573308,20.5027999731771,4.95152970492334));
#91229=CARTESIAN_POINT('Ctrl Pts',(-10.1810669544135,20.503125928615,4.95226769909673));
#91230=CARTESIAN_POINT('Ctrl Pts',(-10.1462682291114,20.505082690734,4.95646467718328));
#91231=CARTESIAN_POINT('Ctrl Pts',(-10.1172015960127,20.50675492819,4.95909125854797));
#91232=CARTESIAN_POINT('Ctrl Pts',(-9.95760060590718,20.5160741420751,4.96871399136899));
#91233=CARTESIAN_POINT('Ctrl Pts',(-9.82665405767403,20.524156189074,4.95906653258119));
#91234=CARTESIAN_POINT('Ctrl Pts',(-9.68508252089366,20.5326020000613,4.92928423180258));
#91235=CARTESIAN_POINT('Ctrl Pts',(-9.67148740649836,20.5334108003078,4.92622085454221));
#91236=CARTESIAN_POINT('Ctrl Pts',(-9.61829535026342,20.5365654978466,4.91343416850989));
#91237=CARTESIAN_POINT('Ctrl Pts',(-9.57906601780826,20.5388699583677,4.9022516289793));
#91238=CARTESIAN_POINT('Ctrl Pts',(-9.5308430606685,20.5416752396865,4.88629878870084));
#91239=CARTESIAN_POINT('Ctrl Pts',(-9.52136650552922,20.5422252158763,4.88305551235554));
#91240=CARTESIAN_POINT('Ctrl Pts',(-9.50646033397564,20.5430883796072,4.87778243317299));
#91241=CARTESIAN_POINT('Ctrl Pts',(-9.50100832000851,20.5434036778963,4.87581726248366));
#91242=CARTESIAN_POINT('Ctrl Pts',(-9.49090108904287,20.5439874763804,4.872106142382));
#91243=CARTESIAN_POINT('Ctrl Pts',(-9.48624283371902,20.5442562544251,4.87036876133388));
#91244=CARTESIAN_POINT('Ctrl Pts',(-9.47594870545084,20.5448496231285,4.86646951150331));
#91245=CARTESIAN_POINT('Ctrl Pts',(-9.470317154656,20.5451738368501,4.86429643773945));
#91246=CARTESIAN_POINT('Ctrl Pts',(-9.45407307548177,20.5461079710779,4.85791251409775));
#91247=CARTESIAN_POINT('Ctrl Pts',(-9.44349603986617,20.5467149063497,4.853612187833));
#91248=CARTESIAN_POINT('Ctrl Pts',(-9.35820410394262,20.5516007166158,4.8177661434215));
#91249=CARTESIAN_POINT('Ctrl Pts',(-9.28617553206794,20.5556628084855,4.78018218264892));
#91250=CARTESIAN_POINT('Ctrl Pts',(-9.14259423546236,20.563991602126,4.68935691419776));
#91251=CARTESIAN_POINT('Ctrl Pts',(-9.07204243519726,20.5682245567197,4.63516859086689));
#91252=CARTESIAN_POINT('Ctrl Pts',(-8.97681467810198,20.5747301381891,4.54718435638437));
#91253=CARTESIAN_POINT('Ctrl Pts',(-8.94796796888357,20.5768273590472,4.51820003992412));
#91254=CARTESIAN_POINT('Ctrl Pts',(-8.91624730916446,20.5793374981187,4.48353938825117));
#91255=CARTESIAN_POINT('Ctrl Pts',(-8.91214838315707,20.5796660108317,4.47900382035431));
#91256=CARTESIAN_POINT('Ctrl Pts',(-8.90565199038369,20.5801935959356,4.47172422028032));
#91257=CARTESIAN_POINT('Ctrl Pts',(-8.90323610286555,20.5803913472762,4.46899663559176));
#91258=CARTESIAN_POINT('Ctrl Pts',(-8.89897815009931,20.5807426975999,4.46415299972927));
#91259=CARTESIAN_POINT('Ctrl Pts',(-8.8971319526628,20.5808959882856,4.46204063891472));
#91260=CARTESIAN_POINT('Ctrl Pts',(-8.893222217744,20.5812226597567,4.45754119839523));
#91261=CARTESIAN_POINT('Ctrl Pts',(-8.89116035575976,20.5813961513067,4.45515278824485));
#91262=CARTESIAN_POINT('Ctrl Pts',(-8.88558344190604,20.5818686783726,4.44865023425726));
#91263=CARTESIAN_POINT('Ctrl Pts',(-8.88208349447449,20.5821687795416,4.44452327483412));
#91264=CARTESIAN_POINT('Ctrl Pts',(-8.86429567523937,20.5837118523578,4.42331141813337));
#91265=CARTESIAN_POINT('Ctrl Pts',(-8.85037698899982,20.5849788071226,4.40592224239126));
#91266=CARTESIAN_POINT('Ctrl Pts',(-8.80992673116005,20.5888268944151,4.35295216074447));
#91267=CARTESIAN_POINT('Ctrl Pts',(-8.78461201156551,20.591461509597,4.31647616686375));
#91268=CARTESIAN_POINT('Ctrl Pts',(-8.72302006781919,20.5983965824194,4.21850232022926));
#91269=CARTESIAN_POINT('Ctrl Pts',(-8.68951184208899,20.6027228860264,4.15539663854157));
#91270=CARTESIAN_POINT('Ctrl Pts',(-8.63068859801709,20.6113792753365,4.02189406395155));
#91271=CARTESIAN_POINT('Ctrl Pts',(-8.60588773625279,20.6156872215042,3.95148729461855));
#91272=CARTESIAN_POINT('Ctrl Pts',(-8.58381486465399,20.6204035137354,3.86927462819662));
#91273=CARTESIAN_POINT('Ctrl Pts',(-8.58118338850067,20.6209858988318,3.85903136324673));
#91274=CARTESIAN_POINT('Ctrl Pts',(-8.57713071825249,20.6219166910244,3.8425151199075));
#91275=CARTESIAN_POINT('Ctrl Pts',(-8.57563947342048,20.6222673237693,3.83625985855487));
#91276=CARTESIAN_POINT('Ctrl Pts',(-8.5730575804616,20.6228893330799,3.82510426156666));
#91277=CARTESIAN_POINT('Ctrl Pts',(-8.57195083346964,20.6231612186845,3.82020778942869));
#91278=CARTESIAN_POINT('Ctrl Pts',(-8.56968944184591,20.6237280330903,3.8099579764735));
#91279=CARTESIAN_POINT('Ctrl Pts',(-8.56853960607608,20.6240228054133,3.80460364688229));
#91280=CARTESIAN_POINT('Ctrl Pts',(-8.56561291148635,20.6247907725627,3.79059254065567));
#91281=CARTESIAN_POINT('Ctrl Pts',(-8.56388434474194,20.6252624345873,3.7819258301705));
#91282=CARTESIAN_POINT('Ctrl Pts',(-8.55650421227616,20.6273612969774,3.74309274992734));
#91283=CARTESIAN_POINT('Ctrl Pts',(-8.55172368249318,20.6289610086887,3.71276761492174));
#91284=CARTESIAN_POINT('Ctrl Pts',(-8.54128046593888,20.6332608611351,3.62958874739014));
#91285=CARTESIAN_POINT('Ctrl Pts',(-8.53753699533784,20.6359056589259,3.57654061958454));
#91286=CARTESIAN_POINT('Ctrl Pts',(-8.53505787753058,20.6435130477447,3.42153402450689));
#91287=CARTESIAN_POINT('Ctrl Pts',(-8.54407055202662,20.6483421366308,3.31978159020635));
#91288=CARTESIAN_POINT('Ctrl Pts',(-8.56942674510398,20.6550802002476,3.18979546212704));
#91289=CARTESIAN_POINT('Ctrl Pts',(-8.57621761619831,20.6566671421376,3.15998505918496));
#91290=CARTESIAN_POINT('Ctrl Pts',(-8.5853630790576,20.6586050550509,3.1249446011584));
#91291=CARTESIAN_POINT('Ctrl Pts',(-8.58682148787257,20.6589090358855,3.1194863194484));
#91292=CARTESIAN_POINT('Ctrl Pts',(-8.58924618989976,20.6594065793754,3.11061779702304));
#91293=CARTESIAN_POINT('Ctrl Pts',(-8.59019334570668,20.6595990764697,3.10720232984749));
#91294=CARTESIAN_POINT('Ctrl Pts',(-8.59190785862227,20.6599443087391,3.10110584352167));
#91295=CARTESIAN_POINT('Ctrl Pts',(-8.59267048041607,20.6600967705797,3.09842354422595));
#91296=CARTESIAN_POINT('Ctrl Pts',(-8.59434067521794,20.6604283270342,3.09261231465354));
#91297=CARTESIAN_POINT('Ctrl Pts',(-8.59525101833033,20.6606075755217,3.08948427363875));
#91298=CARTESIAN_POINT('Ctrl Pts',(-8.5978332724912,20.6611119079906,3.08072052891734));
#91299=CARTESIAN_POINT('Ctrl Pts',(-8.59952868664254,20.6614383063382,3.07509188679085));
#91300=CARTESIAN_POINT('Ctrl Pts',(-8.60988310904659,20.6634033344892,3.04145127872989));
#91301=CARTESIAN_POINT('Ctrl Pts',(-8.61934786459483,20.6650837938046,3.01369624477323));
#91302=CARTESIAN_POINT('Ctrl Pts',(-8.67612115789244,20.6745116480617,2.86226201702805));
#91303=CARTESIAN_POINT('Ctrl Pts',(-8.73921435087696,20.6827019219361,2.74515532452553));
#91304=CARTESIAN_POINT('Ctrl Pts',(-8.82807916098557,20.6914976447893,2.62320204860877));
#91305=CARTESIAN_POINT('Ctrl Pts',(-8.83923344717261,20.6925653345078,2.6084877180643));
#91306=CARTESIAN_POINT('Ctrl Pts',(-8.87249719250457,20.6956448575536,2.56629044576023));
#91307=CARTESIAN_POINT('Ctrl Pts',(-8.89532612903876,20.6976301705083,2.53938975045291));
#91308=CARTESIAN_POINT('Ctrl Pts',(-8.92561928826648,20.7001093439909,2.50620340853799));
#91309=CARTESIAN_POINT('Ctrl Pts',(-8.93220292176351,20.7006393978413,2.49913288347314));
#91310=CARTESIAN_POINT('Ctrl Pts',(-8.94275277289437,20.7014751867949,2.4880254129426));
#91311=CARTESIAN_POINT('Ctrl Pts',(-8.94667314485928,20.7017828616776,2.48394547313304));
#91312=CARTESIAN_POINT('Ctrl Pts',(-8.95374333634529,20.7023325946614,2.47667240868098));
#91313=CARTESIAN_POINT('Ctrl Pts',(-8.95688434492712,20.7025750277356,2.47347084982523));
#91314=CARTESIAN_POINT('Ctrl Pts',(-8.96425265302893,20.7031396020369,2.46602924113074));
#91315=CARTESIAN_POINT('Ctrl Pts',(-8.96849137052845,20.703461239446,2.46180057516005));
#91316=CARTESIAN_POINT('Ctrl Pts',(-8.98072226529886,20.7043804699136,2.44974753450614));
#91317=CARTESIAN_POINT('Ctrl Pts',(-8.98877844041387,20.7049752258136,2.44198851215169));
#91318=CARTESIAN_POINT('Ctrl Pts',(-9.04941482937833,20.7093747666153,2.38491405071674));
#91319=CARTESIAN_POINT('Ctrl Pts',(-9.10548822072992,20.7130112826272,2.33944874008731));
#91320=CARTESIAN_POINT('Ctrl Pts',(-9.23322487295998,20.720678567297,2.25065831475121));
#91321=CARTESIAN_POINT('Ctrl Pts',(-9.30570694708112,20.7246657501089,2.20897122993276));
#91322=CARTESIAN_POINT('Ctrl Pts',(-9.43116367535788,20.7315127742817,2.15045215543675));
#91323=CARTESIAN_POINT('Ctrl Pts',(-9.4822472535904,20.7342903161352,2.1300419667088));
#91324=CARTESIAN_POINT('Ctrl Pts',(-9.54114592350192,20.7376055436466,2.11027465027035));
#91325=CARTESIAN_POINT('Ctrl Pts',(-9.54795667965244,20.7379905752628,2.10804438161724));
#91326=CARTESIAN_POINT('Ctrl Pts',(-9.55814282197562,20.738569296075,2.10479144179286));
#91327=CARTESIAN_POINT('Ctrl Pts',(-9.56150607290425,20.7387608421014,2.10373077021889));
#91328=CARTESIAN_POINT('Ctrl Pts',(-9.56753440712326,20.7391050562114,2.10185353757106));
#91329=CARTESIAN_POINT('Ctrl Pts',(-9.57019802028452,20.7392574577136,2.10103242443278));
#91330=CARTESIAN_POINT('Ctrl Pts',(-9.5759926749828,20.7395896920806,2.09926421535745));
#91331=CARTESIAN_POINT('Ctrl Pts',(-9.57912450888576,20.7397696842417,2.09832001848));
#91332=CARTESIAN_POINT('Ctrl Pts',(-9.58795197318773,20.7402781701645,2.09569093401207));
#91333=CARTESIAN_POINT('Ctrl Pts',(-9.59365466579339,20.7406080124679,2.09403022930265));
#91334=CARTESIAN_POINT('Ctrl Pts',(-9.62863724511608,20.7426389753466,2.08407341532358));
#91335=CARTESIAN_POINT('Ctrl Pts',(-9.65815800719362,20.7443851764392,2.0766580957713));
#91336=CARTESIAN_POINT('Ctrl Pts',(-9.8326517368111,20.7548110116127,2.03856834994767));
#91337=CARTESIAN_POINT('Ctrl Pts',(-9.98138562376467,20.7640040227649,2.02913157191114));
#91338=CARTESIAN_POINT('Ctrl Pts',(-10.1654734906761,20.7746119914218,2.04542457667391));
#91339=CARTESIAN_POINT('Ctrl Pts',(-10.2017900367449,20.7766738084385,2.05001646427287));
#91340=CARTESIAN_POINT('Ctrl Pts',(-10.2474402060859,20.7792271579078,2.05753713884985));
#91341=CARTESIAN_POINT('Ctrl Pts',(-10.2569660585743,20.7797578687801,2.05920361867682));
#91342=CARTESIAN_POINT('Ctrl Pts',(-10.2720951432256,20.7805975396543,2.06200516211635));
#91343=CARTESIAN_POINT('Ctrl Pts',(-10.2777093373958,20.7809084241285,2.06307883098469));
#91344=CARTESIAN_POINT('Ctrl Pts',(-10.2882001191804,20.7814880679398,2.06514888820618));
#91345=CARTESIAN_POINT('Ctrl Pts',(-10.2930781787321,20.7817570743469,2.0661373135095));
#91346=CARTESIAN_POINT('Ctrl Pts',(-10.3039590643816,20.7823559902763,2.06839991860104));
#91347=CARTESIAN_POINT('Ctrl Pts',(-10.3099591297369,20.782685485763,2.06968701140548));
#91348=CARTESIAN_POINT('Ctrl Pts',(-10.3275710386278,20.7836505010516,2.07358102539579));
#91349=CARTESIAN_POINT('Ctrl Pts',(-10.339159539298,20.7842827170908,2.07629192090537));
#91350=CARTESIAN_POINT('Ctrl Pts',(-10.4588240031204,20.7907856780798,2.10582903841884));
#91351=CARTESIAN_POINT('Ctrl Pts',(-10.5635364984254,20.7962222471104,2.14476489767079));
#91352=CARTESIAN_POINT('Ctrl Pts',(-10.7449222954545,20.8061132140168,2.23690800791843));
#91353=CARTESIAN_POINT('Ctrl Pts',(-10.8228865963402,20.8105666921341,2.2862602645948));
#91354=CARTESIAN_POINT('Ctrl Pts',(-10.9044833827044,20.8160115108662,2.3494063526567));
#91355=CARTESIAN_POINT('Ctrl Pts',(-10.9132003774872,20.8166042377049,2.35631254854431));
#91356=CARTESIAN_POINT('Ctrl Pts',(-10.9252092026642,20.8174376134264,2.36605157696715));
#91357=CARTESIAN_POINT('Ctrl Pts',(-10.9285686244638,20.8176726070618,2.36880090015919));
#91358=CARTESIAN_POINT('Ctrl Pts',(-10.9339426610799,20.8180516113993,2.37323903759915));
#91359=CARTESIAN_POINT('Ctrl Pts',(-10.9359650706279,20.8181949497142,2.3749184265511));
#91360=CARTESIAN_POINT('Ctrl Pts',(-10.9400062855384,20.8184828163387,2.37829264902925));
#91361=CARTESIAN_POINT('Ctrl Pts',(-10.9420250465688,20.8186273472463,2.37998749589648));
#91362=CARTESIAN_POINT('Ctrl Pts',(-10.9469971891729,20.8189851032353,2.38418480086848));
#91363=CARTESIAN_POINT('Ctrl Pts',(-10.9499452310026,20.8191987802106,2.38669353172425));
#91364=CARTESIAN_POINT('Ctrl Pts',(-10.9596720352538,20.8199088649679,2.39503763041493));
#91365=CARTESIAN_POINT('Ctrl Pts',(-10.9664071176315,20.8204087596367,2.4009233291967));
#91366=CARTESIAN_POINT('Ctrl Pts',(-10.9825368114719,20.8216250210738,2.41528173979945));
#91367=CARTESIAN_POINT('Ctrl Pts',(-10.991876214188,20.8223451929125,2.42381514348535));
#91368=CARTESIAN_POINT('Ctrl Pts',(-11.0265092178773,20.8250723718442,2.45629307432812));
#91369=CARTESIAN_POINT('Ctrl Pts',(-11.0510549080209,20.8271206907293,2.48101588986008));
#91370=CARTESIAN_POINT('Ctrl Pts',(-11.1684397018811,20.8374108297976,2.60800534651693));
#91371=CARTESIAN_POINT('Ctrl Pts',(-11.2473802239159,20.8458690277799,2.72220760261087));
#91372=CARTESIAN_POINT('Ctrl Pts',(-11.3210755620005,20.855218854551,2.86967875371017));
#91373=CARTESIAN_POINT('Ctrl Pts',(-11.3323584045408,20.8567119818949,2.89389214853392));
#91374=CARTESIAN_POINT('Ctrl Pts',(-11.3464424278588,20.8586633473753,2.92641368162881));
#91375=CARTESIAN_POINT('Ctrl Pts',(-11.3498403391074,20.8591416409647,2.93445642102651));
#91376=CARTESIAN_POINT('Ctrl Pts',(-11.3552432092668,20.859914714751,2.94757097524141));
#91377=CARTESIAN_POINT('Ctrl Pts',(-11.3572921162346,20.860210965593,2.95262435568503));
#91378=CARTESIAN_POINT('Ctrl Pts',(-11.3611755624191,20.8607785138527,2.96235828891635));
#91379=CARTESIAN_POINT('Ctrl Pts',(-11.3630143189916,20.8610499491327,2.96703706665562));
#91380=CARTESIAN_POINT('Ctrl Pts',(-11.3672077934773,20.8616753694391,2.97787115544829));
#91381=CARTESIAN_POINT('Ctrl Pts',(-11.3695451253283,20.8620287726436,2.98403310911999));
#91382=CARTESIAN_POINT('Ctrl Pts',(-11.3767921804142,20.8631401235808,3.00353490312667));
#91383=CARTESIAN_POINT('Ctrl Pts',(-11.3815493058924,20.8638930363262,3.01693081798758));
#91384=CARTESIAN_POINT('Ctrl Pts',(-11.4040587939898,20.8675785694212,3.08337088947177));
#91385=CARTESIAN_POINT('Ctrl Pts',(-11.4189560792206,20.8704175947892,3.13733565928366));
#91386=CARTESIAN_POINT('Ctrl Pts',(-11.4525167466992,20.8783406135788,3.29324514767279));
#91387=CARTESIAN_POINT('Ctrl Pts',(-11.4634999999976,20.8832405801403,3.39647993126226));
#91388=CARTESIAN_POINT('Ctrl Pts',(-11.4635,20.8884018418444,3.4999999999667));
#91389=CARTESIAN_POINT('Origin',(-10.,13.2,3.5));
#91390=CARTESIAN_POINT('',(-11.4635,21.4611504451332,3.50000000000115));
#91391=CARTESIAN_POINT('',(-11.4635,21.3891087006547,3.49999999989906));
#91392=CARTESIAN_POINT('',(-11.4635,13.2,3.5));
#91393=CARTESIAN_POINT('',(-11.4634996681794,20.9614426132404,3.50098551447728));
#91394=CARTESIAN_POINT('Ctrl Pts',(-11.4635,21.4611504451332,3.50000000000115));
#91395=CARTESIAN_POINT('Ctrl Pts',(-11.4635,21.4611301311275,3.49958402536292));
#91396=CARTESIAN_POINT('Ctrl Pts',(-11.463499822648,21.4611098150822,3.49916804479857));
#91397=CARTESIAN_POINT('Ctrl Pts',(-11.4634800403263,21.45997668514,3.47596872626212));
#91398=CARTESIAN_POINT('Ctrl Pts',(-11.4629285888914,21.4588587293667,3.453189353351));
#91399=CARTESIAN_POINT('Ctrl Pts',(-11.459355687562,21.4551326182292,3.37811065493419));
#91400=CARTESIAN_POINT('Ctrl Pts',(-11.4540587307172,21.4524786967789,3.32596506512405));
#91401=CARTESIAN_POINT('Ctrl Pts',(-11.4448804648682,21.4493035845956,3.26718370650074));
#91402=CARTESIAN_POINT('Ctrl Pts',(-11.443730267838,21.448920873213,3.2601544374043));
#91403=CARTESIAN_POINT('Ctrl Pts',(-11.4419355603834,21.4483450095766,3.24966730221917));
#91404=CARTESIAN_POINT('Ctrl Pts',(-11.4413298034892,21.4481539702018,3.24620280355885));
#91405=CARTESIAN_POINT('Ctrl Pts',(-11.4402218649907,21.4478103444058,3.23999809515392));
#91406=CARTESIAN_POINT('Ctrl Pts',(-11.4397243422751,21.4476580212517,3.2372571047446));
#91407=CARTESIAN_POINT('Ctrl Pts',(-11.438624679679,21.4473255805546,3.23129567464895));
#91408=CARTESIAN_POINT('Ctrl Pts',(-11.4380195591897,21.4471453012809,3.22807587382141));
#91409=CARTESIAN_POINT('Ctrl Pts',(-11.4362819450198,21.4466350371026,3.21899818148236));
#91410=CARTESIAN_POINT('Ctrl Pts',(-11.435124446602,21.4463036883464,3.21314521467631));
#91411=CARTESIAN_POINT('Ctrl Pts',(-11.4277385215497,21.4442414116689,3.17696177174206));
#91412=CARTESIAN_POINT('Ctrl Pts',(-11.4205850262114,21.4424638086071,3.14683022659087));
#91413=CARTESIAN_POINT('Ctrl Pts',(-11.3711499059412,21.4314313603784,2.96453989002991));
#91414=CARTESIAN_POINT('Ctrl Pts',(-11.3054224331949,21.4216221630225,2.81980899491061));
#91415=CARTESIAN_POINT('Ctrl Pts',(-11.2022685113024,21.4110553934255,2.66503399632583));
#91416=CARTESIAN_POINT('Ctrl Pts',(-11.1860571767917,21.4094867014405,2.64216182996881));
#91417=CARTESIAN_POINT('Ctrl Pts',(-11.1638515592825,21.4074531325712,2.61266645594961));
#91418=CARTESIAN_POINT('Ctrl Pts',(-11.1584403306633,21.4069660172414,2.60561346408241));
#91419=CARTESIAN_POINT('Ctrl Pts',(-11.1495858000748,21.4061823146069,2.59428766080702));
#91420=CARTESIAN_POINT('Ctrl Pts',(-11.1461821974204,21.4058841798824,2.58998421741162));
#91421=CARTESIAN_POINT('Ctrl Pts',(-11.1396215634412,21.40531538727,2.58178429023885));
#91422=CARTESIAN_POINT('Ctrl Pts',(-11.1364685535956,21.4050445758402,2.57788470077436));
#91423=CARTESIAN_POINT('Ctrl Pts',(-11.1291754280711,21.4044239488897,2.56895891380048));
#91424=CARTESIAN_POINT('Ctrl Pts',(-11.1250216691297,21.4040746863901,2.56394396673649));
#91425=CARTESIAN_POINT('Ctrl Pts',(-11.111958169909,21.4029891611793,2.54838461530554));
#91426=CARTESIAN_POINT('Ctrl Pts',(-11.1029324795768,21.4022576021341,2.53793826875781));
#91427=CARTESIAN_POINT('Ctrl Pts',(-11.0211719566985,21.3957878290582,2.44597166437074));
#91428=CARTESIAN_POINT('Ctrl Pts',(-10.939669528071,21.3904603760823,2.37270579807588));
#91429=CARTESIAN_POINT('Ctrl Pts',(-10.7888294885497,21.3814477690091,2.26493966676558));
#91430=CARTESIAN_POINT('Ctrl Pts',(-10.7235426742755,21.3777575031556,2.22559421903429));
#91431=CARTESIAN_POINT('Ctrl Pts',(-10.6346165643394,21.3726380238458,2.18104602627489));
#91432=CARTESIAN_POINT('Ctrl Pts',(-10.6134877345626,21.3714147880386,2.17108674239387));
#91433=CARTESIAN_POINT('Ctrl Pts',(-10.5869246875783,21.3698577586546,2.15933446708396));
#91434=CARTESIAN_POINT('Ctrl Pts',(-10.5817051795276,21.3695509025321,2.1570615270948));
#91435=CARTESIAN_POINT('Ctrl Pts',(-10.573484749764,21.3690660008817,2.15353869021256));
#91436=CARTESIAN_POINT('Ctrl Pts',(-10.5704926419175,21.3688891687441,2.15226821582951));
#91437=CARTESIAN_POINT('Ctrl Pts',(-10.5649261633307,21.3685595263574,2.1499265001712));
#91438=CARTESIAN_POINT('Ctrl Pts',(-10.5623529504834,21.3684068754176,2.14885264177258));
#91439=CARTESIAN_POINT('Ctrl Pts',(-10.5564953513437,21.3680587841313,2.14642776836013));
#91440=CARTESIAN_POINT('Ctrl Pts',(-10.5532091197796,21.3678630739183,2.14508135610378));
#91441=CARTESIAN_POINT('Ctrl Pts',(-10.5431573578577,21.367263225692,2.14100568209325));
#91442=CARTESIAN_POINT('Ctrl Pts',(-10.5363763988116,21.3668568833374,2.1383150783701));
#91443=CARTESIAN_POINT('Ctrl Pts',(-10.453761427734,21.361888389703,2.10624728187323));
#91444=CARTESIAN_POINT('Ctrl Pts',(-10.3756334230676,21.3570148277561,2.08319269281859));
#91445=CARTESIAN_POINT('Ctrl Pts',(-10.177714277955,21.3448484532469,2.04231712190961));
#91446=CARTESIAN_POINT('Ctrl Pts',(-10.056831455609,21.3376126476002,2.03262071543825));
#91447=CARTESIAN_POINT('Ctrl Pts',(-9.91988968774703,21.329954948038,2.03860393723804));
#91448=CARTESIAN_POINT('Ctrl Pts',(-9.90367376392719,21.3290557290481,2.0395831415249));
#91449=CARTESIAN_POINT('Ctrl Pts',(-9.88106183320187,21.3278120032122,2.04132684883454));
#91450=CARTESIAN_POINT('Ctrl Pts',(-9.87464990082434,21.3274604687251,2.04186385959931));
#91451=CARTESIAN_POINT('Ctrl Pts',(-9.8635574831246,21.3268542547662,2.04286657774157));
#91452=CARTESIAN_POINT('Ctrl Pts',(-9.85887535159832,21.3265989661006,2.04331259186927));
#91453=CARTESIAN_POINT('Ctrl Pts',(-9.84915162785144,21.3260700003851,2.04428618422934));
#91454=CARTESIAN_POINT('Ctrl Pts',(-9.84411045747146,21.3257964404922,2.04481740107011));
#91455=CARTESIAN_POINT('Ctrl Pts',(-9.83224791779711,21.3251542701545,2.04612977593453));
#91456=CARTESIAN_POINT('Ctrl Pts',(-9.8254290512644,21.3247863459649,2.04693276977572));
#91457=CARTESIAN_POINT('Ctrl Pts',(-9.80299025317935,21.3235794384284,2.0497354093413));
#91458=CARTESIAN_POINT('Ctrl Pts',(-9.78739664094299,21.3227468274616,2.05193920696695));
#91459=CARTESIAN_POINT('Ctrl Pts',(-9.70464902013932,21.3183570517546,2.064999197121));
#91460=CARTESIAN_POINT('Ctrl Pts',(-9.63827461380241,21.3149413213872,2.08027621668749));
#91461=CARTESIAN_POINT('Ctrl Pts',(-9.48633342006634,21.3071268913126,2.12660066633379));
#91462=CARTESIAN_POINT('Ctrl Pts',(-9.40212707427342,21.3028035137062,2.16111027112437));
#91463=CARTESIAN_POINT('Ctrl Pts',(-9.31338696659663,21.2978019485107,2.20752869420937));
#91464=CARTESIAN_POINT('Ctrl Pts',(-9.30515030113056,21.2973331095202,2.21193811280459));
#91465=CARTESIAN_POINT('Ctrl Pts',(-9.26521347672998,21.2950347291572,2.23381244510653));
#91466=CARTESIAN_POINT('Ctrl Pts',(-9.2341286938692,21.2931680878775,2.25236908693119));
#91467=CARTESIAN_POINT('Ctrl Pts',(-9.19878816219192,21.2909164287371,2.27528491478045));
#91468=CARTESIAN_POINT('Ctrl Pts',(-9.19382996878516,21.2905974628379,2.27854294901673));
#91469=CARTESIAN_POINT('Ctrl Pts',(-9.18590343993438,21.2900823746668,2.28382076549076));
#91470=CARTESIAN_POINT('Ctrl Pts',(-9.18292243759883,21.2898874773167,2.28582151393529));
#91471=CARTESIAN_POINT('Ctrl Pts',(-9.17763136852044,21.2895393809886,2.28940101074344));
#91472=CARTESIAN_POINT('Ctrl Pts',(-9.17531843361537,21.28938647083,2.29097543747345));
#91473=CARTESIAN_POINT('Ctrl Pts',(-9.17038203307026,21.2890585098531,2.2943564271401));
#91474=CARTESIAN_POINT('Ctrl Pts',(-9.16775998719448,21.2888833350482,2.29616489645935));
#91475=CARTESIAN_POINT('Ctrl Pts',(-9.16058560982151,21.2884013987963,2.30114782703011));
#91476=CARTESIAN_POINT('Ctrl Pts',(-9.15604544768949,21.2880934999663,2.30433961231346));
#91477=CARTESIAN_POINT('Ctrl Pts',(-9.13184662829229,21.2864372422295,2.32155815284345));
#91478=CARTESIAN_POINT('Ctrl Pts',(-9.11252034471343,21.2850606097371,2.3360433059577));
#91479=CARTESIAN_POINT('Ctrl Pts',(-9.05392142794344,21.2807394058507,2.38227151457293));
#91480=CARTESIAN_POINT('Ctrl Pts',(-9.01592757424103,21.277726499898,2.41557273939989));
#91481=CARTESIAN_POINT('Ctrl Pts',(-8.88752373856033,21.2669636947059,2.5404319031459));
#91482=CARTESIAN_POINT('Ctrl Pts',(-8.80751698747826,21.2592069482765,2.64187969540345));
#91483=CARTESIAN_POINT('Ctrl Pts',(-8.73286767803188,21.2510259388926,2.76752897205724));
#91484=CARTESIAN_POINT('Ctrl Pts',(-8.72420467963364,21.2500564955394,2.78272427479796));
#91485=CARTESIAN_POINT('Ctrl Pts',(-8.71228119170046,21.2486923203827,2.80453840291927));
#91486=CARTESIAN_POINT('Ctrl Pts',(-8.70879537338103,21.2482896493729,2.81103180244253));
#91487=CARTESIAN_POINT('Ctrl Pts',(-8.70319217737001,21.2476359411706,2.82166136237208));
#91488=CARTESIAN_POINT('Ctrl Pts',(-8.70104521444083,21.2473838679045,2.82578171049791));
#91489=CARTESIAN_POINT('Ctrl Pts',(-8.69657548545385,21.2468556751731,2.8344604012811));
#91490=CARTESIAN_POINT('Ctrl Pts',(-8.69425692330766,21.2465797050502,2.83902084664508));
#91491=CARTESIAN_POINT('Ctrl Pts',(-8.68876489988419,21.2459211681037,2.84996493775974));
#91492=CARTESIAN_POINT('Ctrl Pts',(-8.68561405781701,21.2455393893209,2.85635983084253));
#91493=CARTESIAN_POINT('Ctrl Pts',(-8.67497665685648,21.244236482752,2.87835320145688));
#91494=CARTESIAN_POINT('Ctrl Pts',(-8.66771988757726,21.2433232389886,2.89406160589563));
#91495=CARTESIAN_POINT('Ctrl Pts',(-8.65096439207781,21.2411512086961,2.93208861657945));
#91496=CARTESIAN_POINT('Ctrl Pts',(-8.64173847558102,21.2399013469183,2.95452211441172));
#91497=CARTESIAN_POINT('Ctrl Pts',(-8.60792953137675,21.2350830696333,3.04291566124165));
#91498=CARTESIAN_POINT('Ctrl Pts',(-8.5875591847026,21.231638108814,3.11038719020647));
#91499=CARTESIAN_POINT('Ctrl Pts',(-8.54994242726977,21.2232925582005,3.27774861985359));
#91500=CARTESIAN_POINT('Ctrl Pts',(-8.53805481268909,21.2184409491678,3.37845303050966));
#91501=CARTESIAN_POINT('Ctrl Pts',(-8.53649275767327,21.2125324444674,3.49029938558661));
#91502=CARTESIAN_POINT('Ctrl Pts',(-8.53646098064527,21.2119597726167,3.50103714852257));
#91503=CARTESIAN_POINT('Ctrl Pts',(-8.53658176970697,21.2111502896338,3.51605069394901));
#91504=CARTESIAN_POINT('Ctrl Pts',(-8.53663492389504,21.2109187189398,3.52032718952413));
#91505=CARTESIAN_POINT('Ctrl Pts',(-8.53675080086115,21.2105438379702,3.52721901810856));
#91506=CARTESIAN_POINT('Ctrl Pts',(-8.53680179307397,21.2104011731885,3.52983455635806));
#91507=CARTESIAN_POINT('Ctrl Pts',(-8.53692376803546,21.210100337392,3.53533430662061));
#91508=CARTESIAN_POINT('Ctrl Pts',(-8.53699626693786,21.2099420804834,3.53821845596389));
#91509=CARTESIAN_POINT('Ctrl Pts',(-8.53719463090444,21.209553498555,3.54527866660649));
#91510=CARTESIAN_POINT('Ctrl Pts',(-8.53732985103437,21.209322662046,3.54945442292691));
#91511=CARTESIAN_POINT('Ctrl Pts',(-8.53788283967565,21.2084855062561,3.56453484454326));
#91512=CARTESIAN_POINT('Ctrl Pts',(-8.53840468178118,21.2078737801958,3.57543505765787));
#91513=CARTESIAN_POINT('Ctrl Pts',(-8.54251979034078,21.2039274914821,3.64507607018328));
#91514=CARTESIAN_POINT('Ctrl Pts',(-8.54953136508475,21.2004425896762,3.70355615661841));
#91515=CARTESIAN_POINT('Ctrl Pts',(-8.57247777543465,21.1927434247547,3.82993566542132));
#91516=CARTESIAN_POINT('Ctrl Pts',(-8.58978333102514,21.1885242647581,3.89745032580979));
#91517=CARTESIAN_POINT('Ctrl Pts',(-8.63578567597808,21.179899157694,4.03523297328383));
#91518=CARTESIAN_POINT('Ctrl Pts',(-8.66527299870249,21.1755235017651,4.10503029413225));
#91519=CARTESIAN_POINT('Ctrl Pts',(-8.70489812915807,21.1707437526348,4.1816565936542));
#91520=CARTESIAN_POINT('Ctrl Pts',(-8.70986840195684,21.1701601018389,4.19101739165575));
#91521=CARTESIAN_POINT('Ctrl Pts',(-8.71801978183778,21.1692277491744,4.20597478114955));
#91522=CARTESIAN_POINT('Ctrl Pts',(-8.72113682998956,21.1688768087861,4.21160569532669));
#91523=CARTESIAN_POINT('Ctrl Pts',(-8.72675075627993,21.1682545239069,4.22159116309641));
#91524=CARTESIAN_POINT('Ctrl Pts',(-8.72923306840958,21.1679826679192,4.22595375179171));
#91525=CARTESIAN_POINT('Ctrl Pts',(-8.73446770029021,21.167416185326,4.23504433613493));
#91526=CARTESIAN_POINT('Ctrl Pts',(-8.7372241892471,21.1671217134128,4.23976984974173));
#91527=CARTESIAN_POINT('Ctrl Pts',(-8.74449223529763,21.1663551223996,4.25207063433728));
#91528=CARTESIAN_POINT('Ctrl Pts',(-8.7490459024572,21.1658845267094,4.25962085061249));
#91529=CARTESIAN_POINT('Ctrl Pts',(-8.76965800893085,21.1637964618045,4.29310872199924));
#91530=CARTESIAN_POINT('Ctrl Pts',(-8.78645744700883,21.1622061302865,4.3185826192565));
#91531=CARTESIAN_POINT('Ctrl Pts',(-8.83439914582753,21.1579387481391,4.38655572799235));
#91532=CARTESIAN_POINT('Ctrl Pts',(-8.86705939512393,21.155315953508,4.42792918338761));
#91533=CARTESIAN_POINT('Ctrl Pts',(-8.97150478951151,21.1475598476947,4.54648107798513));
#91534=CARTESIAN_POINT('Ctrl Pts',(-9.04944928307729,21.142576261814,4.61775433219206));
#91535=CARTESIAN_POINT('Ctrl Pts',(-9.15701541301805,21.1357631857022,4.696661533193));
#91536=CARTESIAN_POINT('Ctrl Pts',(-9.1801450907161,21.1343001148797,4.7126250711233));
#91537=CARTESIAN_POINT('Ctrl Pts',(-9.20833925665923,21.1325009723191,4.73090854663575));
#91538=CARTESIAN_POINT('Ctrl Pts',(-9.21297700116117,21.132204529286,4.73387899735192));
#91539=CARTESIAN_POINT('Ctrl Pts',(-9.22058963991437,21.1317169355873,4.73869447162572));
#91540=CARTESIAN_POINT('Ctrl Pts',(-9.22355462487179,21.1315267814213,4.74055515087622));
#91541=CARTESIAN_POINT('Ctrl Pts',(-9.22889032387238,21.1311840934668,4.74387695232787));
#91542=CARTESIAN_POINT('Ctrl Pts',(-9.23125855815697,21.1310318166463,4.74534196129335));
#91543=CARTESIAN_POINT('Ctrl Pts',(-9.23643311676034,21.1306987007447,4.74852260024066));
#91544=CARTESIAN_POINT('Ctrl Pts',(-9.23924101195282,21.1305176946732,4.75023550987749));
#91545=CARTESIAN_POINT('Ctrl Pts',(-9.24720989044726,21.1300033541549,4.75506000607419));
#91546=CARTESIAN_POINT('Ctrl Pts',(-9.25238429011887,21.1296686217544,4.75814916271871));
#91547=CARTESIAN_POINT('Ctrl Pts',(-9.28527290352683,21.1275370110273,4.77750939525265));
#91548=CARTESIAN_POINT('Ctrl Pts',(-9.31349580790314,21.1256898408835,4.79289472304763));
#91549=CARTESIAN_POINT('Ctrl Pts',(-9.41280254116626,21.1191873398328,4.84286190880665));
#91550=CARTESIAN_POINT('Ctrl Pts',(-9.48616447510012,21.1143860494115,4.8726075059821));
#91551=CARTESIAN_POINT('Ctrl Pts',(-9.65715228174409,21.103626519623,4.92629770037979));
#91552=CARTESIAN_POINT('Ctrl Pts',(-9.75558075408761,21.0977435122032,4.94642148469233));
#91553=CARTESIAN_POINT('Ctrl Pts',(-9.86590099355165,21.0916002502656,4.9573822535575));
#91554=CARTESIAN_POINT('Ctrl Pts',(-9.8765056875752,21.0910139409771,4.95831914879267));
#91555=CARTESIAN_POINT('Ctrl Pts',(-9.89355054844842,21.0900781815977,4.9596377514581));
#91556=CARTESIAN_POINT('Ctrl Pts',(-9.89998452372124,21.089726466836,4.96009272225645));
#91557=CARTESIAN_POINT('Ctrl Pts',(-9.91143240019448,21.0891032957391,4.96082621956821));
#91558=CARTESIAN_POINT('Ctrl Pts',(-9.91644509249127,21.0888313228433,4.96112150138762));
#91559=CARTESIAN_POINT('Ctrl Pts',(-9.92691524917671,21.0882650801918,4.961684207726));
#91560=CARTESIAN_POINT('Ctrl Pts',(-9.93237289838305,21.0879709621372,4.96194688007399));
#91561=CARTESIAN_POINT('Ctrl Pts',(-9.94661024148069,21.0872063470297,4.96255221497409));
#91562=CARTESIAN_POINT('Ctrl Pts',(-9.95539184863972,21.0867373586443,4.96284639152908));
#91563=CARTESIAN_POINT('Ctrl Pts',(-9.99436737631881,21.0846669755442,4.96380074024291));
#91564=CARTESIAN_POINT('Ctrl Pts',(-10.0245759197325,21.0830921422266,4.96360531750974));
#91565=CARTESIAN_POINT('Ctrl Pts',(-10.1066166978932,21.0788785685528,4.96053353149635));
#91566=CARTESIAN_POINT('Ctrl Pts',(-10.1583375172939,21.0762922994023,4.95583484762467));
#91567=CARTESIAN_POINT('Ctrl Pts',(-10.3009254274818,21.0692152413394,4.93519067490057));
#91568=CARTESIAN_POINT('Ctrl Pts',(-10.390691461434,21.0648288500034,4.91339552729158));
#91569=CARTESIAN_POINT('Ctrl Pts',(-10.5167660368826,21.0581387069485,4.86984818063788));
#91570=CARTESIAN_POINT('Ctrl Pts',(-10.5551363567249,21.0560248424622,4.8547524586733));
#91571=CARTESIAN_POINT('Ctrl Pts',(-10.5989521988299,21.0534646371539,4.83534024533925));
#91572=CARTESIAN_POINT('Ctrl Pts',(-10.6050704310159,21.0531037377691,4.83257910735675));
#91573=CARTESIAN_POINT('Ctrl Pts',(-10.6143296561969,21.0525520600224,4.82832353773122));
#91574=CARTESIAN_POINT('Ctrl Pts',(-10.6174847566823,21.0523630990202,4.82685979746426));
#91575=CARTESIAN_POINT('Ctrl Pts',(-10.6231554827871,21.0520216643432,4.82420438102518));
#91576=CARTESIAN_POINT('Ctrl Pts',(-10.6256729518529,21.0518694391256,4.82301676314877));
#91577=CARTESIAN_POINT('Ctrl Pts',(-10.6311141252355,21.0515390106314,4.82043088186607));
#91578=CARTESIAN_POINT('Ctrl Pts',(-10.6340365431695,21.0513606578538,4.81903010366078));
#91579=CARTESIAN_POINT('Ctrl Pts',(-10.642225513315,21.0508584641722,4.8150714503419));
#91580=CARTESIAN_POINT('Ctrl Pts',(-10.6474813424692,21.0505333196409,4.81249169073426));
#91581=CARTESIAN_POINT('Ctrl Pts',(-10.6593300903672,21.0497941432116,4.80658738727821));
#91582=CARTESIAN_POINT('Ctrl Pts',(-10.6659135729145,21.0493790838802,4.80324436605426));
#91583=CARTESIAN_POINT('Ctrl Pts',(-10.6867078973027,21.0480549089188,4.79248653360897));
#91584=CARTESIAN_POINT('Ctrl Pts',(-10.7008219654322,21.0471364632001,4.78488820900658));
#91585=CARTESIAN_POINT('Ctrl Pts',(-10.7586895583269,21.0432974234315,4.75249802229644));
#91586=CARTESIAN_POINT('Ctrl Pts',(-10.8012736386547,21.0402971342469,4.72569208732945));
#91587=CARTESIAN_POINT('Ctrl Pts',(-10.9467350795945,21.0296082615991,4.62330193253106));
#91588=CARTESIAN_POINT('Ctrl Pts',(-11.0410474002814,21.0219097677028,4.53650676924113));
#91589=CARTESIAN_POINT('Ctrl Pts',(-11.1347214881851,21.0137220141372,4.4244342244136));
#91590=CARTESIAN_POINT('Ctrl Pts',(-11.1462660878363,21.0127001152032,4.41007999121677));
#91591=CARTESIAN_POINT('Ctrl Pts',(-11.1621392883171,21.0112760471716,4.38956230495059));
#91592=CARTESIAN_POINT('Ctrl Pts',(-11.1666956752425,21.0108649597493,4.38357796722822));
#91593=CARTESIAN_POINT('Ctrl Pts',(-11.1740080984009,21.0102013610263,4.37381867430217));
#91594=CARTESIAN_POINT('Ctrl Pts',(-11.1767925016566,21.009947750139,4.37006522710676));
#91595=CARTESIAN_POINT('Ctrl Pts',(-11.1825727109988,21.0094192956094,4.36219484805808));
#91596=CARTESIAN_POINT('Ctrl Pts',(-11.1855651121342,21.009144585275,4.35807548538071));
#91597=CARTESIAN_POINT('Ctrl Pts',(-11.1926173576315,21.008494422858,4.34825999238966));
#91598=CARTESIAN_POINT('Ctrl Pts',(-11.196658003029,21.0081197065789,4.3425501780368));
#91599=CARTESIAN_POINT('Ctrl Pts',(-11.2100900803685,21.0068664097011,4.32327782704935));
#91600=CARTESIAN_POINT('Ctrl Pts',(-11.2192932903751,21.0059949104353,4.30958525443937));
#91601=CARTESIAN_POINT('Ctrl Pts',(-11.2687421622212,21.0012351319294,4.2332584867474));
#91602=CARTESIAN_POINT('Ctrl Pts',(-11.3043964994631,20.9975181250561,4.16777699043187));
#91603=CARTESIAN_POINT('Ctrl Pts',(-11.3597744263522,20.9908985377333,4.04454020773095));
#91604=CARTESIAN_POINT('Ctrl Pts',(-11.3811700748043,20.9879770697163,3.98772906042544));
#91605=CARTESIAN_POINT('Ctrl Pts',(-11.406670838702,20.983718731574,3.90471654848577));
#91606=CARTESIAN_POINT('Ctrl Pts',(-11.4136886518874,20.9824249091658,3.87947681474044));
#91607=CARTESIAN_POINT('Ctrl Pts',(-11.4239200913853,20.9803046684768,3.83844203636619));
#91608=CARTESIAN_POINT('Ctrl Pts',(-11.4275568608422,20.9794903835435,3.82275814532188));
#91609=CARTESIAN_POINT('Ctrl Pts',(-11.4365579543222,20.9772946049564,3.78080628546527));
#91610=CARTESIAN_POINT('Ctrl Pts',(-11.4414602383561,20.9758965958273,3.75444671073171));
#91611=CARTESIAN_POINT('Ctrl Pts',(-11.4464811884678,20.9741703166208,3.72260702659757));
#91612=CARTESIAN_POINT('Ctrl Pts',(-11.4472969071363,20.9738780694586,3.71724036833512));
#91613=CARTESIAN_POINT('Ctrl Pts',(-11.4485859946034,20.9733960013297,3.70842972611474));
#91614=CARTESIAN_POINT('Ctrl Pts',(-11.4490769890527,20.9732071391678,3.70498832595111));
#91615=CARTESIAN_POINT('Ctrl Pts',(-11.4499390431667,20.9728658077306,3.69878825181068));
#91616=CARTESIAN_POINT('Ctrl Pts',(-11.4503144977457,20.9727135862063,3.69603024099272));
#91617=CARTESIAN_POINT('Ctrl Pts',(-11.4510316633044,20.9724157252554,3.69064723748581));
#91618=CARTESIAN_POINT('Ctrl Pts',(-11.4513741176792,20.9722701355862,3.68802241189453));
#91619=CARTESIAN_POINT('Ctrl Pts',(-11.4521235011009,20.9719439083484,3.6821545241073));
#91620=CARTESIAN_POINT('Ctrl Pts',(-11.4525266894804,20.9717630680335,3.67891100868824));
#91621=CARTESIAN_POINT('Ctrl Pts',(-11.4535106169903,20.9713080933837,3.67077303471594));
#91622=CARTESIAN_POINT('Ctrl Pts',(-11.454077497768,20.9710332367512,3.66587697910149));
#91623=CARTESIAN_POINT('Ctrl Pts',(-11.4604998930407,20.9677627007257,3.60784340154265));
#91624=CARTESIAN_POINT('Ctrl Pts',(-11.4634636773972,20.9646285659503,3.55443221564043));
#91625=CARTESIAN_POINT('Ctrl Pts',(-11.4634996681794,20.9614426132404,3.50098551447728));
#91626=CARTESIAN_POINT('Ctrl Pts',(-11.4634996668985,20.9614427265142,3.50098741472866));
#91627=CARTESIAN_POINT('Ctrl Pts',(-11.4634998889677,20.9614231064952,3.50065827434728));
#91628=CARTESIAN_POINT('Ctrl Pts',(-11.4635,20.9614034846666,3.50032913609544));
#91629=CARTESIAN_POINT('Ctrl Pts',(-11.4635,20.9613838610471,3.50000000002865));
#91630=CARTESIAN_POINT('',(-11.4634999217228,20.8884519212361,3.50099524440106));
#91631=CARTESIAN_POINT('Ctrl Pts',(-11.4635,20.8884018418444,3.49999999996669));
#91632=CARTESIAN_POINT('Ctrl Pts',(-11.4635,20.8884183486207,3.5003310784354));
#91633=CARTESIAN_POINT('Ctrl Pts',(-11.4634998876533,20.8884348582932,3.500662159811));
#91634=CARTESIAN_POINT('Ctrl Pts',(-11.4634996629539,20.8884513708823,3.50099324403673));
#91635=CARTESIAN_POINT('Ctrl Pts',(-11.4634996615798,20.888451471758,3.50099526663525));
#91636=CARTESIAN_POINT('Ctrl Pts',(-11.4634678874633,20.8907817278273,3.54771783037357));
#91637=CARTESIAN_POINT('Ctrl Pts',(-11.4611986803181,20.8931652632148,3.59440894044376));
#91638=CARTESIAN_POINT('Ctrl Pts',(-11.4562447091829,20.8959151118543,3.6456229266027));
#91639=CARTESIAN_POINT('Ctrl Pts',(-11.4557657341047,20.8961694278967,3.65033567767033));
#91640=CARTESIAN_POINT('Ctrl Pts',(-11.4549259326783,20.8965970411513,3.6582180676293));
#91641=CARTESIAN_POINT('Ctrl Pts',(-11.4545776038289,20.8967696743937,3.6613890348129));
#91642=CARTESIAN_POINT('Ctrl Pts',(-11.4539232260965,20.8970856552067,3.66717182145757));
#91643=CARTESIAN_POINT('Ctrl Pts',(-11.4536204986812,20.8972288200656,3.6697840123862));
#91644=CARTESIAN_POINT('Ctrl Pts',(-11.4529817754272,20.8975248391498,3.67516851580173));
#91645=CARTESIAN_POINT('Ctrl Pts',(-11.4526448872473,20.8976777448881,3.67794066367647));
#91646=CARTESIAN_POINT('Ctrl Pts',(-11.4518567276296,20.8980282625831,3.68427474981859));
#91647=CARTESIAN_POINT('Ctrl Pts',(-11.4514002826456,20.8982261590924,3.68783599216815));
#91648=CARTESIAN_POINT('Ctrl Pts',(-11.4501719242579,20.8987457089006,3.69714793074098));
#91649=CARTESIAN_POINT('Ctrl Pts',(-11.4493789153753,20.8990684882368,3.70289572170898));
#91650=CARTESIAN_POINT('Ctrl Pts',(-11.4437702057706,20.9012687394216,3.74183630248317));
#91651=CARTESIAN_POINT('Ctrl Pts',(-11.4378491708847,20.9032007589316,3.77485746259861));
#91652=CARTESIAN_POINT('Ctrl Pts',(-11.4259168023662,20.9065282709584,3.83035297819525));
#91653=CARTESIAN_POINT('Ctrl Pts',(-11.4204940730595,20.9079057618472,3.85294240121919));
#91654=CARTESIAN_POINT('Ctrl Pts',(-11.3927160293921,20.9143703607978,3.95761432554385));
#91655=CARTESIAN_POINT('Ctrl Pts',(-11.3637668996709,20.9195462862548,4.03778230505363));
#91656=CARTESIAN_POINT('Ctrl Pts',(-11.3013152328085,20.9283333467417,4.17264315021601));
#91657=CARTESIAN_POINT('Ctrl Pts',(-11.2708837150819,20.9320027716621,4.22850968341083));
#91658=CARTESIAN_POINT('Ctrl Pts',(-11.2287883436083,20.936392852964,4.29507390705955));
#91659=CARTESIAN_POINT('Ctrl Pts',(-11.2204638517342,20.937232895955,4.30779410878638));
#91660=CARTESIAN_POINT('Ctrl Pts',(-11.208147160853,20.9384365075832,4.32598942359285));
#91661=CARTESIAN_POINT('Ctrl Pts',(-11.2043129491904,20.9388059287207,4.33156984837963));
#91662=CARTESIAN_POINT('Ctrl Pts',(-11.1975488724475,20.9394485937481,4.34126957450956));
#91663=CARTESIAN_POINT('Ctrl Pts',(-11.1946361562558,20.9397224780415,4.34540064700281));
#91664=CARTESIAN_POINT('Ctrl Pts',(-11.1889563335281,20.940251096742,4.35336830371731));
#91665=CARTESIAN_POINT('Ctrl Pts',(-11.1861919168658,20.9405059286469,4.3572067206404));
#91666=CARTESIAN_POINT('Ctrl Pts',(-11.1795643542736,20.9411111150987,4.36631569616052));
#91667=CARTESIAN_POINT('Ctrl Pts',(-11.1756844038229,20.9414608209053,4.37157394165595));
#91668=CARTESIAN_POINT('Ctrl Pts',(-11.1616796932645,20.9427069939652,4.390289927458));
#91669=CARTESIAN_POINT('Ctrl Pts',(-11.1513578176559,20.9435958298475,4.40359895483992));
#91670=CARTESIAN_POINT('Ctrl Pts',(-11.070888843521,20.9503116358383,4.50373743085783));
#91671=CARTESIAN_POINT('Ctrl Pts',(-10.9912456297667,20.9557177734446,4.58246317407575));
#91672=CARTESIAN_POINT('Ctrl Pts',(-10.8860507497717,20.9622218769823,4.66500375730469));
#91673=CARTESIAN_POINT('Ctrl Pts',(-10.8683754197174,20.9632972820162,4.67823758108123));
#91674=CARTESIAN_POINT('Ctrl Pts',(-10.8118772216963,20.9667004905346,4.71857664482065));
#91675=CARTESIAN_POINT('Ctrl Pts',(-10.7720369123503,20.9690505551201,4.74419937652244));
#91676=CARTESIAN_POINT('Ctrl Pts',(-10.7176537447061,20.9722849988975,4.77555622806802));
#91677=CARTESIAN_POINT('Ctrl Pts',(-10.7041587521399,20.9730897400513,4.78305534039246));
#91678=CARTESIAN_POINT('Ctrl Pts',(-10.6842089226722,20.9742861424566,4.79373184827651));
#91679=CARTESIAN_POINT('Ctrl Pts',(-10.6778449078585,20.9746687859607,4.79707756978428));
#91680=CARTESIAN_POINT('Ctrl Pts',(-10.6663603756657,20.9753615358747,4.8030076730888));
#91681=CARTESIAN_POINT('Ctrl Pts',(-10.6612487890496,20.9756706543867,4.80560912342843));
#91682=CARTESIAN_POINT('Ctrl Pts',(-10.6532502686896,20.976155782314,4.80962080724145));
#91683=CARTESIAN_POINT('Ctrl Pts',(-10.6503737019194,20.9763305381653,4.81105172275856));
#91684=CARTESIAN_POINT('Ctrl Pts',(-10.6449933449511,20.9766579782372,4.81370605566845));
#91685=CARTESIAN_POINT('Ctrl Pts',(-10.6424907621754,20.9768105166132,4.81493179894655));
#91686=CARTESIAN_POINT('Ctrl Pts',(-10.6368221945154,20.9771565557812,4.81768816823731));
#91687=CARTESIAN_POINT('Ctrl Pts',(-10.633654201036,20.9773503127382,4.81921452732917));
#91688=CARTESIAN_POINT('Ctrl Pts',(-10.6240584517716,20.9779382304224,4.8237952803805));
#91689=CARTESIAN_POINT('Ctrl Pts',(-10.6176139865872,20.978334471661,4.82681417499587));
#91690=CARTESIAN_POINT('Ctrl Pts',(-10.5361922965864,20.9833558613795,4.86423425519794));
#91691=CARTESIAN_POINT('Ctrl Pts',(-10.4584655685125,20.9883025126594,4.89228009642619));
#91692=CARTESIAN_POINT('Ctrl Pts',(-10.3179515557337,20.9970608168189,4.92993267866941));
#91693=CARTESIAN_POINT('Ctrl Pts',(-10.2561106916181,21.0008570900837,4.94229286519773));
#91694=CARTESIAN_POINT('Ctrl Pts',(-10.1346290331164,21.0080797808981,4.95851104418175));
#91695=CARTESIAN_POINT('Ctrl Pts',(-10.0751636212557,21.0115086470748,4.96278201794068));
#91696=CARTESIAN_POINT('Ctrl Pts',(-10.0009051341905,21.0156446676167,4.96357347421454));
#91697=CARTESIAN_POINT('Ctrl Pts',(-9.98621110586287,21.0164561883048,4.96350880497));
#91698=CARTESIAN_POINT('Ctrl Pts',(-9.96484275948789,21.0176266199279,4.96309289620649));
#91699=CARTESIAN_POINT('Ctrl Pts',(-9.95816625717915,21.017990943691,4.96291722066639));
#91700=CARTESIAN_POINT('Ctrl Pts',(-9.94645373087873,21.0186277170247,4.96252878610567));
#91701=CARTESIAN_POINT('Ctrl Pts',(-9.94141720272888,21.0189007724277,4.96233570354803));
#91702=CARTESIAN_POINT('Ctrl Pts',(-9.93097202981078,21.0194655051952,4.96188122279942));
#91703=CARTESIAN_POINT('Ctrl Pts',(-9.92556363038191,21.0197570538729,4.96161581758119));
#91704=CARTESIAN_POINT('Ctrl Pts',(-9.91161170355261,21.0205069859648,4.96085351604024));
#91705=CARTESIAN_POINT('Ctrl Pts',(-9.90307077020996,21.0209639694783,4.96031168415693));
#91706=CARTESIAN_POINT('Ctrl Pts',(-9.86925255558547,21.0227655107959,4.95786826988807));
#91707=CARTESIAN_POINT('Ctrl Pts',(-9.84402098433956,21.0240920134794,4.95538497804692));
#91708=CARTESIAN_POINT('Ctrl Pts',(-9.68033566857496,21.0326066645846,4.93496900683278));
#91709=CARTESIAN_POINT('Ctrl Pts',(-9.54500415439845,21.0391377933756,4.89796201794667));
#91710=CARTESIAN_POINT('Ctrl Pts',(-9.37405280195013,21.0483917719569,4.82371114732454));
#91711=CARTESIAN_POINT('Ctrl Pts',(-9.33206261267229,21.0507626284908,4.80302723947746));
#91712=CARTESIAN_POINT('Ctrl Pts',(-9.28263427905847,21.053756157782,4.77566185559158));
#91713=CARTESIAN_POINT('Ctrl Pts',(-9.27417705092004,21.0542758057067,4.77086890900552));
#91714=CARTESIAN_POINT('Ctrl Pts',(-9.26231644351195,21.055016027925,4.76399016799674));
#91715=CARTESIAN_POINT('Ctrl Pts',(-9.25887270545364,21.055232328876,4.76197405156413));
#91716=CARTESIAN_POINT('Ctrl Pts',(-9.25298365166132,21.0556046601951,4.75849392057858));
#91717=CARTESIAN_POINT('Ctrl Pts',(-9.25053425935228,21.0557602497611,4.75703678400076));
#91718=CARTESIAN_POINT('Ctrl Pts',(-9.24580739955322,21.0560619460629,4.75420606158851));
#91719=CARTESIAN_POINT('Ctrl Pts',(-9.24352940794893,21.0562079873464,4.75283341535161));
#91720=CARTESIAN_POINT('Ctrl Pts',(-9.23805000757893,21.0565608051909,4.74951130788908));
#91721=CARTESIAN_POINT('Ctrl Pts',(-9.23485233910362,21.0567679704366,4.74755575261467));
#91722=CARTESIAN_POINT('Ctrl Pts',(-9.22311419028167,21.0575330142122,4.74031510553916));
#91723=CARTESIAN_POINT('Ctrl Pts',(-9.21462086916275,21.0580955155457,4.73495454646749));
#91724=CARTESIAN_POINT('Ctrl Pts',(-9.11464645272156,21.0648169833118,4.6704072784527));
#91725=CARTESIAN_POINT('Ctrl Pts',(-9.03000131371245,21.0714836212155,4.60127390049134));
#91726=CARTESIAN_POINT('Ctrl Pts',(-8.9080712291999,21.0819379462725,4.47662860940969));
#91727=CARTESIAN_POINT('Ctrl Pts',(-8.86550869595354,21.0858063642649,4.42684563549367));
#91728=CARTESIAN_POINT('Ctrl Pts',(-8.80541468862294,21.091566023651,4.34618787342835));
#91729=CARTESIAN_POINT('Ctrl Pts',(-8.78543365341597,21.0935430123415,4.31724957676257));
#91730=CARTESIAN_POINT('Ctrl Pts',(-8.76153559450679,21.0959908875846,4.27982286610712));
#91731=CARTESIAN_POINT('Ctrl Pts',(-8.75663217437518,21.0964979933706,4.27198072637484));
#91732=CARTESIAN_POINT('Ctrl Pts',(-8.7488967042639,21.0973059929001,4.25934431402223));
#91733=CARTESIAN_POINT('Ctrl Pts',(-8.74601715621876,21.0976086121102,4.2545795336059));
#91734=CARTESIAN_POINT('Ctrl Pts',(-8.74060421071949,21.0981810357783,4.24550618761535));
#91735=CARTESIAN_POINT('Ctrl Pts',(-8.73806556517226,21.0984510274128,4.24120085866339));
#91736=CARTESIAN_POINT('Ctrl Pts',(-8.73234441442198,21.099063029358,4.23138367062301));
#91737=CARTESIAN_POINT('Ctrl Pts',(-8.72917569749857,21.099404541552,4.22586386548708));
#91738=CARTESIAN_POINT('Ctrl Pts',(-8.72106022233904,21.1002859795838,4.21151091729666));
#91739=CARTESIAN_POINT('Ctrl Pts',(-8.71616888545164,21.100823936604,4.2026467223897));
#91740=CARTESIAN_POINT('Ctrl Pts',(-8.68366004952092,21.1044468437323,4.14226051228089));
#91741=CARTESIAN_POINT('Ctrl Pts',(-8.65905745898278,21.1074240550001,4.08917191774264));
#91742=CARTESIAN_POINT('Ctrl Pts',(-8.6036309159947,21.1149730806284,3.94796951901581));
#91743=CARTESIAN_POINT('Ctrl Pts',(-8.57793780684316,21.1194139252313,3.85813677922145));
#91744=CARTESIAN_POINT('Ctrl Pts',(-8.55113998458815,21.1266717584984,3.71341964542923));
#91745=CARTESIAN_POINT('Ctrl Pts',(-8.54425828471586,21.1293831836728,3.6598695230222));
#91746=CARTESIAN_POINT('Ctrl Pts',(-8.53959128084539,21.1327888041901,3.59564432388117));
#91747=CARTESIAN_POINT('Ctrl Pts',(-8.53894556319771,21.1333467344117,3.5852137543083));
#91748=CARTESIAN_POINT('Ctrl Pts',(-8.5382017406495,21.1341322243204,3.57067511772246));
#91749=CARTESIAN_POINT('Ctrl Pts',(-8.53800913229654,21.1343547758547,3.56657195526271));
#91750=CARTESIAN_POINT('Ctrl Pts',(-8.5377112159965,21.1347345493512,3.55959874438));
#91751=CARTESIAN_POINT('Ctrl Pts',(-8.5375970761848,21.1348912844461,3.55672906172041));
#91752=CARTESIAN_POINT('Ctrl Pts',(-8.53739453182035,21.1351925653286,3.55122909891772));
#91753=CARTESIAN_POINT('Ctrl Pts',(-8.53730477424594,21.1353370309784,3.54859889354514));
#91754=CARTESIAN_POINT('Ctrl Pts',(-8.53708527353023,21.1357216754216,3.54161409050566));
#91755=CARTESIAN_POINT('Ctrl Pts',(-8.53696788040713,21.1359625274059,3.53725916656505));
#91756=CARTESIAN_POINT('Ctrl Pts',(-8.53661775649572,21.1368271055657,3.52169026017909));
#91757=CARTESIAN_POINT('Ctrl Pts',(-8.53649450725721,21.137456486465,3.51047449483913));
#91758=CARTESIAN_POINT('Ctrl Pts',(-8.53654515516309,21.1431198413276,3.41047310841816));
#91759=CARTESIAN_POINT('Ctrl Pts',(-8.5446694720475,21.1484889986286,3.32188275367972));
#91760=CARTESIAN_POINT('Ctrl Pts',(-8.57920590428533,21.1599541336159,3.13460802694218));
#91761=CARTESIAN_POINT('Ctrl Pts',(-8.60801224365818,21.1660005059439,3.03681198907617));
#91762=CARTESIAN_POINT('Ctrl Pts',(-8.65463390940712,21.1728843656703,2.92358584571164));
#91763=CARTESIAN_POINT('Ctrl Pts',(-8.6629456441163,21.174038080151,2.90455990508909));
#91764=CARTESIAN_POINT('Ctrl Pts',(-8.67487389436709,21.1755987136269,2.87876598986451));
#91765=CARTESIAN_POINT('Ctrl Pts',(-8.67814267310525,21.1760173772424,2.87184070361112));
#91766=CARTESIAN_POINT('Ctrl Pts',(-8.68373156924583,21.1767183812838,2.86023681370671));
#91767=CARTESIAN_POINT('Ctrl Pts',(-8.68602261885863,21.1770017134976,2.85554444748383));
#91768=CARTESIAN_POINT('Ctrl Pts',(-8.69059633297172,21.1775595060649,2.84630267495011));
#91769=CARTESIAN_POINT('Ctrl Pts',(-8.69287771301283,21.1778340057171,2.84175271837361));
#91770=CARTESIAN_POINT('Ctrl Pts',(-8.69795460357751,21.1784367805802,2.83175790666896));
#91771=CARTESIAN_POINT('Ctrl Pts',(-8.70076063566251,21.1787646846549,2.82631848374136));
#91772=CARTESIAN_POINT('Ctrl Pts',(-8.71073046053708,21.1799116385908,2.80728621738846));
#91773=CARTESIAN_POINT('Ctrl Pts',(-8.71807424922285,21.1807243901212,2.79378847143435));
#91774=CARTESIAN_POINT('Ctrl Pts',(-8.79051892301356,21.1884500206363,2.66549156394738));
#91775=CARTESIAN_POINT('Ctrl Pts',(-8.87064920523814,21.1947393068515,2.5598843986068));
#91776=CARTESIAN_POINT('Ctrl Pts',(-8.99962658011907,21.2036714996917,2.43058386451901));
#91777=CARTESIAN_POINT('Ctrl Pts',(-9.03723330910315,21.2061762982343,2.3966063830991));
#91778=CARTESIAN_POINT('Ctrl Pts',(-9.09529543359107,21.21002594748,2.3493795271473));
#91779=CARTESIAN_POINT('Ctrl Pts',(-9.11444297778402,21.2112930331554,2.33457885294272));
#91780=CARTESIAN_POINT('Ctrl Pts',(-9.13842508106681,21.2128889430654,2.31697347333036));
#91781=CARTESIAN_POINT('Ctrl Pts',(-9.14292130662893,21.2131885234483,2.31371200161458));
#91782=CARTESIAN_POINT('Ctrl Pts',(-9.1500262668751,21.2136626947862,2.3086196829808));
#91783=CARTESIAN_POINT('Ctrl Pts',(-9.15262264918451,21.213836133331,2.30677159281626));
#91784=CARTESIAN_POINT('Ctrl Pts',(-9.15751054449196,21.2141629884947,2.3033164156148));
#91785=CARTESIAN_POINT('Ctrl Pts',(-9.15980064230863,21.2143162727403,2.3017074135811));
#91786=CARTESIAN_POINT('Ctrl Pts',(-9.16503915312032,21.2146672221375,2.29804928294395));
#91787=CARTESIAN_POINT('Ctrl Pts',(-9.16799049834818,21.2148651702731,2.2960044308019));
#91788=CARTESIAN_POINT('Ctrl Pts',(-9.17583763242447,21.2153920116797,2.29061014164183));
#91789=CARTESIAN_POINT('Ctrl Pts',(-9.18074626022775,21.215722111854,2.28727960969383));
#91790=CARTESIAN_POINT('Ctrl Pts',(-9.2157394062011,21.2180784270235,2.26384596979193));
#91791=CARTESIAN_POINT('Ctrl Pts',(-9.24653791983643,21.2201680476056,2.24483628898403));
#91792=CARTESIAN_POINT('Ctrl Pts',(-9.28646677278156,21.2228666019121,2.22219047365839));
#91793=CARTESIAN_POINT('Ctrl Pts',(-9.29497465069798,21.2234410277182,2.21747666558154));
#91794=CARTESIAN_POINT('Ctrl Pts',(-9.31156780052904,21.2245594294929,2.20849819803641));
#91795=CARTESIAN_POINT('Ctrl Pts',(-9.31964733547032,21.2251031336573,2.20422376699748));
#91796=CARTESIAN_POINT('Ctrl Pts',(-9.41270439937898,21.2313516085068,2.15610275540327));
#91797=CARTESIAN_POINT('Ctrl Pts',(-9.50175063296573,21.2371801747724,2.12060678763121));
#91798=CARTESIAN_POINT('Ctrl Pts',(-9.63273521958418,21.2451899228687,2.0827469005947));
#91799=CARTESIAN_POINT('Ctrl Pts',(-9.67230370284899,21.2475431890549,2.07307837528896));
#91800=CARTESIAN_POINT('Ctrl Pts',(-9.72886736455619,21.2508075846401,2.06173458678877));
#91801=CARTESIAN_POINT('Ctrl Pts',(-9.74556544783553,21.251759264722,2.05868691909391));
#91802=CARTESIAN_POINT('Ctrl Pts',(-9.77522327567962,21.2534286327248,2.05380538734197));
#91803=CARTESIAN_POINT('Ctrl Pts',(-9.78816147435961,21.2541498958856,2.05185363717459));
#91804=CARTESIAN_POINT('Ctrl Pts',(-9.80743919165336,21.2552144475472,2.04920945282567));
#91805=CARTESIAN_POINT('Ctrl Pts',(-9.81375963213919,21.2555618639238,2.0483845537268));
#91806=CARTESIAN_POINT('Ctrl Pts',(-9.825046456361,21.2561794494475,2.04698640818088));
#91807=CARTESIAN_POINT('Ctrl Pts',(-9.83001073990744,21.2564501113165,2.04639727134377));
#91808=CARTESIAN_POINT('Ctrl Pts',(-9.84050440907031,21.2570202306539,2.04520642662856));
#91809=CARTESIAN_POINT('Ctrl Pts',(-9.84603441178467,21.257319494923,2.04461077939027));
#91810=CARTESIAN_POINT('Ctrl Pts',(-9.86074466905555,21.2581124958157,2.04311109059864));
#91811=CARTESIAN_POINT('Ctrl Pts',(-9.86993038601583,21.2586045076349,2.04226228618085));
#91812=CARTESIAN_POINT('Ctrl Pts',(-9.9099888736827,21.2607369351497,2.03894235154316));
#91813=CARTESIAN_POINT('Ctrl Pts',(-9.94092877728684,21.2623495723929,2.03736463017295));
#91814=CARTESIAN_POINT('Ctrl Pts',(-10.1263967790424,21.2718538287936,2.03380250583381));
#91815=CARTESIAN_POINT('Ctrl Pts',(-10.28036568849,21.2789508668227,2.05532114542294));
#91816=CARTESIAN_POINT('Ctrl Pts',(-10.457549551469,21.2883819563988,2.10952212768218));
#91817=CARTESIAN_POINT('Ctrl Pts',(-10.4866996657552,21.2899814742456,2.11945536942276));
#91818=CARTESIAN_POINT('Ctrl Pts',(-10.521089499703,21.2919498245786,2.132398636556));
#91819=CARTESIAN_POINT('Ctrl Pts',(-10.5266533148601,21.2922708612208,2.13453156774136));
#91820=CARTESIAN_POINT('Ctrl Pts',(-10.5352548308002,21.2927714134737,2.13788941596586));
#91821=CARTESIAN_POINT('Ctrl Pts',(-10.538301771078,21.2929495537965,2.139090679047));
#91822=CARTESIAN_POINT('Ctrl Pts',(-10.5439339579229,21.2932804209201,2.14133305521722));
#91823=CARTESIAN_POINT('Ctrl Pts',(-10.5465202772114,21.2934329787906,2.14237133072001));
#91824=CARTESIAN_POINT('Ctrl Pts',(-10.5523675219553,21.2937792930083,2.1447381178771));
#91825=CARTESIAN_POINT('Ctrl Pts',(-10.5556266116033,21.2939733072907,2.14607100762659));
#91826=CARTESIAN_POINT('Ctrl Pts',(-10.5654792519445,21.2945627631698,2.15014206735476));
#91827=CARTESIAN_POINT('Ctrl Pts',(-10.5720575049815,21.2949603009552,2.15291669542205));
#91828=CARTESIAN_POINT('Ctrl Pts',(-10.627314126559,21.2983315791153,2.17670100511284));
#91829=CARTESIAN_POINT('Ctrl Pts',(-10.6748336414272,21.3014397674838,2.20029168682407));
#91830=CARTESIAN_POINT('Ctrl Pts',(-10.8052601675048,21.3103728172256,2.27412426202323));
#91831=CARTESIAN_POINT('Ctrl Pts',(-10.8846184461138,21.31628014391,2.33009928968929));
#91832=CARTESIAN_POINT('Ctrl Pts',(-11.0001032064973,21.32525259741,2.43007146471581));
#91833=CARTESIAN_POINT('Ctrl Pts',(-11.0402177048261,21.3284599070218,2.46902873282656));
#91834=CARTESIAN_POINT('Ctrl Pts',(-11.087617682278,21.3323599827721,2.52065234540852));
#91835=CARTESIAN_POINT('Ctrl Pts',(-11.0970727983884,21.3331441487931,2.53125578897215));
#91836=CARTESIAN_POINT('Ctrl Pts',(-11.1106851418213,21.3342826344654,2.54697629879894));
#91837=CARTESIAN_POINT('Ctrl Pts',(-11.1149643751268,21.3346419604253,2.5519862324318));
#91838=CARTESIAN_POINT('Ctrl Pts',(-11.1224486011826,21.3352729999617,2.56086920156233));
#91839=CARTESIAN_POINT('Ctrl Pts',(-11.1256677222223,21.3355452857153,2.56473014648532));
#91840=CARTESIAN_POINT('Ctrl Pts',(-11.1323376596818,21.3361112989426,2.57281424938419));
#91841=CARTESIAN_POINT('Ctrl Pts',(-11.1357848957104,21.3364048800448,2.57704026985936));
#91842=CARTESIAN_POINT('Ctrl Pts',(-11.1446913057284,21.3371661935363,2.5880842423434));
#91843=CARTESIAN_POINT('Ctrl Pts',(-11.1501132559022,21.3376324426726,2.59493202601757));
#91844=CARTESIAN_POINT('Ctrl Pts',(-11.1718807051539,21.3395161900734,2.62293525407937));
#91845=CARTESIAN_POINT('Ctrl Pts',(-11.1877069256551,21.3409134331606,2.64448884740441));
#91846=CARTESIAN_POINT('Ctrl Pts',(-11.2937703485707,21.3505078083649,2.79755659716515));
#91847=CARTESIAN_POINT('Ctrl Pts',(-11.3625535910143,21.3578155085845,2.94258992024518));
#91848=CARTESIAN_POINT('Ctrl Pts',(-11.4151597132442,21.3675079728895,3.12567579722264));
#91849=CARTESIAN_POINT('Ctrl Pts',(-11.4227793757136,21.3691198930767,3.15577013325147));
#91850=CARTESIAN_POINT('Ctrl Pts',(-11.430717017823,21.3711021210456,3.19191441734161));
#91851=CARTESIAN_POINT('Ctrl Pts',(-11.4319622057151,21.3714238486354,3.19775481762025));
#91852=CARTESIAN_POINT('Ctrl Pts',(-11.4338354806062,21.3719252492649,3.20681267076338));
#91853=CARTESIAN_POINT('Ctrl Pts',(-11.4344885742218,21.3721035395539,3.21002495716689));
#91854=CARTESIAN_POINT('Ctrl Pts',(-11.435676907326,21.3724345421612,3.21597212489187));
#91855=CARTESIAN_POINT('Ctrl Pts',(-11.4362151306475,21.3725870844127,3.21870635592564));
#91856=CARTESIAN_POINT('Ctrl Pts',(-11.4374150468531,21.3729331787579,3.22489528229714));
#91857=CARTESIAN_POINT('Ctrl Pts',(-11.438072092779,21.3731269873723,3.22835081804142));
#91858=CARTESIAN_POINT('Ctrl Pts',(-11.4400216473243,21.3737152136708,3.23880923377225));
#91859=CARTESIAN_POINT('Ctrl Pts',(-11.4412754868841,21.374111715007,3.24581910410662));
#91860=CARTESIAN_POINT('Ctrl Pts',(-11.4563984470665,21.3791296586784,3.33407908000419));
#91861=CARTESIAN_POINT('Ctrl Pts',(-11.4634291991323,21.38407206109,3.41634335699287));
#91862=CARTESIAN_POINT('Ctrl Pts',(-11.4634998226655,21.3890586118033,3.49916806716909));
#91863=CARTESIAN_POINT('Ctrl Pts',(-11.4635,21.38908365615,3.49958403613083));
#91864=CARTESIAN_POINT('Ctrl Pts',(-11.4635,21.3891087006547,3.49999999989906));
#91865=CARTESIAN_POINT('Origin',(-10.,13.2,3.5));
#91866=CARTESIAN_POINT('',(-11.4634999989655,21.95929037674,3.50005409278718));
#91867=CARTESIAN_POINT('',(-11.4634995977471,21.8907054572846,3.50002669594524));
#91868=CARTESIAN_POINT('',(-11.4635,13.2,3.5));
#91869=CARTESIAN_POINT('Ctrl Pts',(-11.4634999989303,21.9592903521363,3.50005595443291));
#91870=CARTESIAN_POINT('Ctrl Pts',(-11.4635000837772,21.9591704883509,3.49783676651995));
#91871=CARTESIAN_POINT('Ctrl Pts',(-11.4634951210042,21.9590507810711,3.49561757043241));
#91872=CARTESIAN_POINT('Ctrl Pts',(-11.4634633356496,21.9586711814159,3.48857120664378));
#91873=CARTESIAN_POINT('Ctrl Pts',(-11.4634176777367,21.9584118738391,3.48374412844848));
#91874=CARTESIAN_POINT('Ctrl Pts',(-11.4632041962147,21.957618078178,3.46892637974804));
#91875=CARTESIAN_POINT('Ctrl Pts',(-11.4629579376394,21.9570860205732,3.45893701153549));
#91876=CARTESIAN_POINT('Ctrl Pts',(-11.4611625807412,21.954361214927,3.40749830568833));
#91877=CARTESIAN_POINT('Ctrl Pts',(-11.4579541439654,21.9522202978012,3.36612404212276));
#91878=CARTESIAN_POINT('Ctrl Pts',(-11.4410054772692,21.9450506786003,3.225451272886));
#91879=CARTESIAN_POINT('Ctrl Pts',(-11.4188333281464,21.9402629521516,3.12745979366409));
#91880=CARTESIAN_POINT('Ctrl Pts',(-11.3710145863942,21.9329358614462,2.98560701919107));
#91881=CARTESIAN_POINT('Ctrl Pts',(-11.3528394360572,21.9304854775702,2.93954843727851));
#91882=CARTESIAN_POINT('Ctrl Pts',(-11.3224999054142,21.9267113782372,2.87278779961937));
#91883=CARTESIAN_POINT('Ctrl Pts',(-11.3121029516317,21.925461926811,2.85131913981528));
#91884=CARTESIAN_POINT('Ctrl Pts',(-11.2986561562204,21.9238858904358,2.82520002798487));
#91885=CARTESIAN_POINT('Ctrl Pts',(-11.2960978165354,21.9235876976811,2.82029913761618));
#91886=CARTESIAN_POINT('Ctrl Pts',(-11.2920240379942,21.9231152710309,2.81260182493634));
#91887=CARTESIAN_POINT('Ctrl Pts',(-11.2905271190604,21.9229421759555,2.80979559519673));
#91888=CARTESIAN_POINT('Ctrl Pts',(-11.2876957141098,21.9226156597463,2.80452905750818));
#91889=CARTESIAN_POINT('Ctrl Pts',(-11.2863633113951,21.9224623686253,2.80206768620966));
#91890=CARTESIAN_POINT('Ctrl Pts',(-11.2833020514056,21.9221110076161,2.79645111107296));
#91891=CARTESIAN_POINT('Ctrl Pts',(-11.2815686155178,21.9219126517508,2.79329845238403));
#91892=CARTESIAN_POINT('Ctrl Pts',(-11.276933395061,21.9213839012366,2.78494135818655));
#91893=CARTESIAN_POINT('Ctrl Pts',(-11.2740114506032,21.9210522855656,2.77974825378787));
#91894=CARTESIAN_POINT('Ctrl Pts',(-11.252777994898,21.9186553468001,2.74254401312974));
#91895=CARTESIAN_POINT('Ctrl Pts',(-11.233295347001,21.9165241695375,2.7112196602872));
#91896=CARTESIAN_POINT('Ctrl Pts',(-11.2018455469214,21.9132194012611,2.66467242925011));
#91897=CARTESIAN_POINT('Ctrl Pts',(-11.1907235363588,21.9120736448428,2.64889348971784));
#91898=CARTESIAN_POINT('Ctrl Pts',(-11.1300698314428,21.9059605524687,2.56636002406667));
#91899=CARTESIAN_POINT('Ctrl Pts',(-11.0752268583977,21.9009041594141,2.50369200737933));
#91900=CARTESIAN_POINT('Ctrl Pts',(-10.9807191466828,21.893133951048,2.41264729949082));
#91901=CARTESIAN_POINT('Ctrl Pts',(-10.9444516243821,21.8903328228964,2.38100146087094));
#91902=CARTESIAN_POINT('Ctrl Pts',(-10.8841848114728,21.8859705980108,2.33343609705836));
#91903=CARTESIAN_POINT('Ctrl Pts',(-10.8611630631068,21.8843664054587,2.31633938058716));
#91904=CARTESIAN_POINT('Ctrl Pts',(-10.8305779474961,21.8823131895614,2.29499088734407));
#91905=CARTESIAN_POINT('Ctrl Pts',(-10.823459536086,21.8818406230474,2.29011525947487));
#91906=CARTESIAN_POINT('Ctrl Pts',(-10.8124149750886,21.8811154420045,2.28269311634664));
#91907=CARTESIAN_POINT('Ctrl Pts',(-10.8085191111315,21.8808611626428,2.28010205821046));
#91908=CARTESIAN_POINT('Ctrl Pts',(-10.8007541020377,21.8803573363245,2.27499125048678));
#91909=CARTESIAN_POINT('Ctrl Pts',(-10.7968853260594,21.8801077740617,2.27247104062598));
#91910=CARTESIAN_POINT('Ctrl Pts',(-10.7880757159549,21.8795427685242,2.26679145795087));
#91911=CARTESIAN_POINT('Ctrl Pts',(-10.7831276708928,21.8792277445854,2.26364337882923));
#91912=CARTESIAN_POINT('Ctrl Pts',(-10.7691422429803,21.87834376245,2.25486311910358));
#91913=CARTESIAN_POINT('Ctrl Pts',(-10.7600620194861,21.8777773151768,2.24929964554339));
#91914=CARTESIAN_POINT('Ctrl Pts',(-10.7071689109668,21.874519490189,2.21768070598441));
#91915=CARTESIAN_POINT('Ctrl Pts',(-10.6620771828199,21.8719082550391,2.19382805272781));
#91916=CARTESIAN_POINT('Ctrl Pts',(-10.4951779325324,21.8626900088065,2.11641052490169));
#91917=CARTESIAN_POINT('Ctrl Pts',(-10.3674773134903,21.8565101415634,2.07715951881793));
#91918=CARTESIAN_POINT('Ctrl Pts',(-10.2072676110131,21.8482293629933,2.05095389394188));
#91919=CARTESIAN_POINT('Ctrl Pts',(-10.1781547784743,21.8467013936436,2.04708736552379));
#91920=CARTESIAN_POINT('Ctrl Pts',(-10.1430983756158,21.8448131834933,2.0435008842159));
#91921=CARTESIAN_POINT('Ctrl Pts',(-10.1372458786108,21.8444963460496,2.04293775498961));
#91922=CARTESIAN_POINT('Ctrl Pts',(-10.1281460052437,21.8440009883469,2.0421174731926));
#91923=CARTESIAN_POINT('Ctrl Pts',(-10.1249008281039,21.8438237986499,2.0418358654302));
#91924=CARTESIAN_POINT('Ctrl Pts',(-10.1188767787523,21.8434938410214,2.04133337173733));
#91925=CARTESIAN_POINT('Ctrl Pts',(-10.11609820089,21.8433412351377,2.04110959003202));
#91926=CARTESIAN_POINT('Ctrl Pts',(-10.1097874907034,21.842993703369,2.04061947948288));
#91927=CARTESIAN_POINT('Ctrl Pts',(-10.1062550356974,21.8427985111697,2.0403580358101));
#91928=CARTESIAN_POINT('Ctrl Pts',(-10.0954909666558,21.8422017875704,2.03960064786574));
#91929=CARTESIAN_POINT('Ctrl Pts',(-10.0882566989605,21.8417980844197,2.03914561194563));
#91930=CARTESIAN_POINT('Ctrl Pts',(-10.0178409584893,21.8378446863776,2.03524140234865));
#91931=CARTESIAN_POINT('Ctrl Pts',(-9.95450786348122,21.8341043296183,2.03583987735351));
#91932=CARTESIAN_POINT('Ctrl Pts',(-9.77662597607295,21.8234162117968,2.04907380399863));
#91933=CARTESIAN_POINT('Ctrl Pts',(-9.66322180877623,21.8164226908135,2.071129844737));
#91934=CARTESIAN_POINT('Ctrl Pts',(-9.5197804533306,21.8077945664898,2.11707546265889));
#91935=CARTESIAN_POINT('Ctrl Pts',(-9.48639429982574,21.8057987001517,2.12912415599765));
#91936=CARTESIAN_POINT('Ctrl Pts',(-9.44487345930459,21.8033312202667,2.14583871379558));
#91937=CARTESIAN_POINT('Ctrl Pts',(-9.43630295065719,21.8028226744916,2.14938387860799));
#91938=CARTESIAN_POINT('Ctrl Pts',(-9.42263843260034,21.8020129959342,2.15518889263071));
#91939=CARTESIAN_POINT('Ctrl Pts',(-9.41752271992285,21.8017101241068,2.15739674013288));
#91940=CARTESIAN_POINT('Ctrl Pts',(-9.4078449461099,21.801137604408,2.16163921446936));
#91941=CARTESIAN_POINT('Ctrl Pts',(-9.40328046015303,21.8008677668167,2.16366808325395));
#91942=CARTESIAN_POINT('Ctrl Pts',(-9.39293606278555,21.8002566312356,2.16832963429322));
#91943=CARTESIAN_POINT('Ctrl Pts',(-9.38716270035744,21.79991582688,2.17097666210453));
#91944=CARTESIAN_POINT('Ctrl Pts',(-9.37226854095461,21.7990372387027,2.17792317343375));
#91945=CARTESIAN_POINT('Ctrl Pts',(-9.36317453618332,21.7985014031581,2.18227952303064));
#91946=CARTESIAN_POINT('Ctrl Pts',(-9.30256201159752,21.794932829543,2.21208910806198));
#91947=CARTESIAN_POINT('Ctrl Pts',(-9.25253335444661,21.7920039920107,2.2404648478235));
#91948=CARTESIAN_POINT('Ctrl Pts',(-9.12479569959115,21.7844232288834,2.32321496626206));
#91949=CARTESIAN_POINT('Ctrl Pts',(-9.05048359323231,21.7799135396216,2.38231325186151));
#91950=CARTESIAN_POINT('Ctrl Pts',(-8.94389758331957,21.772597821708,2.48543085389492));
#91951=CARTESIAN_POINT('Ctrl Pts',(-8.90746900772402,21.7699041182703,2.5247678055725));
#91952=CARTESIAN_POINT('Ctrl Pts',(-8.86663719053606,21.7665200602163,2.57402515624088));
#91953=CARTESIAN_POINT('Ctrl Pts',(-8.86007799601037,21.7659641256341,2.58211194492431));
#91954=CARTESIAN_POINT('Ctrl Pts',(-8.85105665554726,21.7651810341626,2.59348013883958));
#91955=CARTESIAN_POINT('Ctrl Pts',(-8.84852101844007,21.7649588460993,2.59670313758938));
#91956=CARTESIAN_POINT('Ctrl Pts',(-8.84423396366924,21.7645795469579,2.6021997127614));
#91957=CARTESIAN_POINT('Ctrl Pts',(-8.84247560453653,21.7644229202751,2.60446788986445));
#91958=CARTESIAN_POINT('Ctrl Pts',(-8.83911747621278,21.7641217335744,2.60882608692546));
#91959=CARTESIAN_POINT('Ctrl Pts',(-8.83751665971492,21.7639772529974,2.61091526797984));
#91960=CARTESIAN_POINT('Ctrl Pts',(-8.83327839690617,21.7635923442451,2.61647752188809));
#91961=CARTESIAN_POINT('Ctrl Pts',(-8.83065084553238,21.7633512408194,2.61995805645383));
#91962=CARTESIAN_POINT('Ctrl Pts',(-8.82130131040381,21.7624845753519,2.63245853469706));
#91963=CARTESIAN_POINT('Ctrl Pts',(-8.81466799124114,21.7618533224432,2.64154393933367));
#91964=CARTESIAN_POINT('Ctrl Pts',(-8.75731012902373,21.7562554192069,2.72203716607972));
#91965=CARTESIAN_POINT('Ctrl Pts',(-8.71299048644277,21.750962485745,2.79778323833706));
#91966=CARTESIAN_POINT('Ctrl Pts',(-8.63190202096214,21.7394924479113,2.97015808004315));
#91967=CARTESIAN_POINT('Ctrl Pts',(-8.59803190595747,21.7333671077691,3.06766204631052));
#91968=CARTESIAN_POINT('Ctrl Pts',(-8.56997984079086,21.726417681113,3.18806684238377));
#91969=CARTESIAN_POINT('Ctrl Pts',(-8.56571455021362,21.7252684047315,3.20830622112898));
#91970=CARTESIAN_POINT('Ctrl Pts',(-8.56046192414569,21.7237128192393,3.23614241599987));
#91971=CARTESIAN_POINT('Ctrl Pts',(-8.5591032104751,21.7232948614451,3.24366595716492));
#91972=CARTESIAN_POINT('Ctrl Pts',(-8.55691644360918,21.7225947730186,3.25634178628154));
#91973=CARTESIAN_POINT('Ctrl Pts',(-8.55605689004874,21.7223116554813,3.26148842366885));
#91974=CARTESIAN_POINT('Ctrl Pts',(-8.55441330065208,21.7217540848904,3.2716641734089));
#91975=CARTESIAN_POINT('Ctrl Pts',(-8.55362793958215,21.7214795937914,3.27669299432882));
#91976=CARTESIAN_POINT('Ctrl Pts',(-8.55195534342973,21.7208765989605,3.28778210446067));
#91977=CARTESIAN_POINT('Ctrl Pts',(-8.55107988310235,21.7205484680752,3.2938440905297));
#91978=CARTESIAN_POINT('Ctrl Pts',(-8.54813705709081,21.7193994443028,3.31516657127676));
#91979=CARTESIAN_POINT('Ctrl Pts',(-8.54627248442591,21.7185848820045,3.33045432602311));
#91980=CARTESIAN_POINT('Ctrl Pts',(-8.5307696184011,21.7108717779644,3.47674211733177));
#91981=CARTESIAN_POINT('Ctrl Pts',(-8.5346320052955,21.7045938192308,3.6089828561549));
#91982=CARTESIAN_POINT('Ctrl Pts',(-8.56443145441309,21.6956674857378,3.78906307213894));
#91983=CARTESIAN_POINT('Ctrl Pts',(-8.57533260239597,21.6931550187792,3.83872796592656));
#91984=CARTESIAN_POINT('Ctrl Pts',(-8.59521657054554,21.689294831275,3.91110046235463));
#91985=CARTESIAN_POINT('Ctrl Pts',(-8.60221936241023,21.6880253834705,3.93431466339828));
#91986=CARTESIAN_POINT('Ctrl Pts',(-8.61153150120847,21.6864268878782,3.96262117768541));
#91987=CARTESIAN_POINT('Ctrl Pts',(-8.61329796498304,21.6861272003435,3.96788950646745));
#91988=CARTESIAN_POINT('Ctrl Pts',(-8.61612462857936,21.6856529337003,3.97616316710048));
#91989=CARTESIAN_POINT('Ctrl Pts',(-8.617164734898,21.6854795083092,3.9791753692756));
#91990=CARTESIAN_POINT('Ctrl Pts',(-8.61913644347883,21.6851527294618,3.98482565490848));
#91991=CARTESIAN_POINT('Ctrl Pts',(-8.62006577670157,21.6849995086646,3.9874644769713));
#91992=CARTESIAN_POINT('Ctrl Pts',(-8.62220416428847,21.6846487744428,3.99348126361423));
#91993=CARTESIAN_POINT('Ctrl Pts',(-8.62341807661731,21.6844509787846,3.9968574545014));
#91994=CARTESIAN_POINT('Ctrl Pts',(-8.62666948528854,21.6839246898652,4.00579704458868));
#91995=CARTESIAN_POINT('Ctrl Pts',(-8.62872835079242,21.6835949931343,4.01135253456713));
#91996=CARTESIAN_POINT('Ctrl Pts',(-8.64348347251496,21.6812576560782,4.05043667013636));
#91997=CARTESIAN_POINT('Ctrl Pts',(-8.65737337855474,21.6791877722604,4.08349889889475));
#91998=CARTESIAN_POINT('Ctrl Pts',(-8.67815530924446,21.6762862395431,4.12828482984927));
#91999=CARTESIAN_POINT('Ctrl Pts',(-8.6840185595466,21.6754861918268,4.14047486141506));
#92000=CARTESIAN_POINT('Ctrl Pts',(-8.69247062771171,21.6743597327681,4.15744099693509));
#92001=CARTESIAN_POINT('Ctrl Pts',(-8.6949184427733,21.6740364957301,4.16228683522756));
#92002=CARTESIAN_POINT('Ctrl Pts',(-8.73762558518917,21.6684493261555,4.24567619112539));
#92003=CARTESIAN_POINT('Ctrl Pts',(-8.78488496736626,21.6630745406304,4.32043825290269));
#92004=CARTESIAN_POINT('Ctrl Pts',(-8.87651407117109,21.6541795756184,4.43994456728132));
#92005=CARTESIAN_POINT('Ctrl Pts',(-8.91755911770016,21.6505840065092,4.48693449851202));
#92006=CARTESIAN_POINT('Ctrl Pts',(-8.97208079597778,21.6462718136731,4.54184486128887));
#92007=CARTESIAN_POINT('Ctrl Pts',(-8.98284569741638,21.6454405151886,4.5523572366306));
#92008=CARTESIAN_POINT('Ctrl Pts',(-8.99866613351974,21.6442471374244,4.56733695801184));
#92009=CARTESIAN_POINT('Ctrl Pts',(-9.00359320981006,21.6438793415426,4.57193806010005));
#92010=CARTESIAN_POINT('Ctrl Pts',(-9.01226549975239,21.643238633391,4.57992513381734));
#92011=CARTESIAN_POINT('Ctrl Pts',(-9.0159967433852,21.642965091333,4.58332604948312));
#92012=CARTESIAN_POINT('Ctrl Pts',(-9.02374566792692,21.642401339232,4.59031589447885));
#92013=CARTESIAN_POINT('Ctrl Pts',(-9.02776572087343,21.6421112456479,4.59390208803307));
#92014=CARTESIAN_POINT('Ctrl Pts',(-9.03813221076957,21.6413691870973,4.60304749932841));
#92015=CARTESIAN_POINT('Ctrl Pts',(-9.04450713301085,21.6409185662689,4.60857422615282));
#92016=CARTESIAN_POINT('Ctrl Pts',(-9.06953990125163,21.6391707844506,4.62989997787011));
#92017=CARTESIAN_POINT('Ctrl Pts',(-9.0885452128395,21.6378903185369,4.64528608538948));
#92018=CARTESIAN_POINT('Ctrl Pts',(-9.23656008033713,21.6282404858106,4.75909503520879));
#92019=CARTESIAN_POINT('Ctrl Pts',(-9.38071950345847,21.6208150097395,4.83590486910357));
#92020=CARTESIAN_POINT('Ctrl Pts',(-9.56406785634892,21.6109769154887,4.89741423471858));
#92021=CARTESIAN_POINT('Ctrl Pts',(-9.59391954024016,21.6093587502289,4.90637895491126));
#92022=CARTESIAN_POINT('Ctrl Pts',(-9.62980857046062,21.6073696085137,4.91591888097632));
#92023=CARTESIAN_POINT('Ctrl Pts',(-9.6355940244763,21.6070476114953,4.91741887053334));
#92024=CARTESIAN_POINT('Ctrl Pts',(-9.64456689962912,21.6065459170461,4.91968669408182));
#92025=CARTESIAN_POINT('Ctrl Pts',(-9.64774805421934,21.6063676055274,4.9204793431988));
#92026=CARTESIAN_POINT('Ctrl Pts',(-9.65363707854226,21.6060366428554,4.92192571414978));
#92027=CARTESIAN_POINT('Ctrl Pts',(-9.65634416634114,21.6058841622806,4.92258239745361));
#92028=CARTESIAN_POINT('Ctrl Pts',(-9.66247058688416,21.605538313492,4.92405003234557));
#92029=CARTESIAN_POINT('Ctrl Pts',(-9.66589095760961,21.6053446897388,4.92485639508078));
#92030=CARTESIAN_POINT('Ctrl Pts',(-9.67472291917828,21.6048433972554,4.92690500711366));
#92031=CARTESIAN_POINT('Ctrl Pts',(-9.68013868450348,21.6045347243183,4.92812878112535));
#92032=CARTESIAN_POINT('Ctrl Pts',(-9.71366088548042,21.6026167781016,4.9355033847289));
#92033=CARTESIAN_POINT('Ctrl Pts',(-9.74193492165365,21.6009673426565,4.9408546929518));
#92034=CARTESIAN_POINT('Ctrl Pts',(-9.87335681296835,21.5932105017247,4.96173623535843));
#92035=CARTESIAN_POINT('Ctrl Pts',(-9.97782037657912,21.5868151459587,4.96704458156094));
#92036=CARTESIAN_POINT('Ctrl Pts',(-10.1347183405296,21.5774708125399,4.95824389699694));
#92037=CARTESIAN_POINT('Ctrl Pts',(-10.1872797823016,21.5743799517944,4.95242949126771));
#92038=CARTESIAN_POINT('Ctrl Pts',(-10.2695763298698,21.5696289932391,4.93878265627349));
#92039=CARTESIAN_POINT('Ctrl Pts',(-10.2995742953442,21.5679156448625,4.93283717432106));
#92040=CARTESIAN_POINT('Ctrl Pts',(-10.3379627827179,21.5657458300829,4.92397024585101));
#92041=CARTESIAN_POINT('Ctrl Pts',(-10.3465418902986,21.5652623794568,4.92190675736069));
#92042=CARTESIAN_POINT('Ctrl Pts',(-10.3604105106826,21.5644831196977,4.91843803443896));
#92043=CARTESIAN_POINT('Ctrl Pts',(-10.3657116359412,21.5641857950418,4.91708051790469));
#92044=CARTESIAN_POINT('Ctrl Pts',(-10.375859988453,21.563617599588,4.91442097978208));
#92045=CARTESIAN_POINT('Ctrl Pts',(-10.3807083675487,21.5633465816307,4.91312369547515));
#92046=CARTESIAN_POINT('Ctrl Pts',(-10.3917557101348,21.5627300095916,4.9101067676736));
#92047=CARTESIAN_POINT('Ctrl Pts',(-10.3979502253396,21.5623849747295,4.90837113454388));
#92048=CARTESIAN_POINT('Ctrl Pts',(-10.4143092511725,21.5614754990796,4.90367097117169));
#92049=CARTESIAN_POINT('Ctrl Pts',(-10.4244534816599,21.5609133028475,4.90063685537803));
#92050=CARTESIAN_POINT('Ctrl Pts',(-10.5063542370379,21.5563869209241,4.87516901454287));
#92051=CARTESIAN_POINT('Ctrl Pts',(-10.576321264917,21.5526068965931,4.84734557270202));
#92052=CARTESIAN_POINT('Ctrl Pts',(-10.7069695619628,21.5454541244459,4.78334211235957));
#92053=CARTESIAN_POINT('Ctrl Pts',(-10.7677810567725,21.5420785078132,4.74791225350963));
#92054=CARTESIAN_POINT('Ctrl Pts',(-10.8626912784255,21.5364304167027,4.683043357448));
#92055=CARTESIAN_POINT('Ctrl Pts',(-10.8983962151186,21.5342059077369,4.65616242828577));
#92056=CARTESIAN_POINT('Ctrl Pts',(-10.9500459305302,21.5307471609263,4.61343842373267));
#92057=CARTESIAN_POINT('Ctrl Pts',(-10.9669483947721,21.5295734454881,4.59879164848176));
#92058=CARTESIAN_POINT('Ctrl Pts',(-10.9875193033697,21.5280825743114,4.58012370661639));
#92059=CARTESIAN_POINT('Ctrl Pts',(-10.9915105942422,21.5277902961085,4.57646102380593));
#92060=CARTESIAN_POINT('Ctrl Pts',(-10.9977947669935,21.5273251518988,4.57062963387479));
#92061=CARTESIAN_POINT('Ctrl Pts',(-11.0001011667095,21.527153366573,4.56847548681762));
#92062=CARTESIAN_POINT('Ctrl Pts',(-11.0044436706111,21.5268278618063,4.56439326650314));
#92063=CARTESIAN_POINT('Ctrl Pts',(-11.0064812111677,21.526674261757,4.5624667920955));
#92064=CARTESIAN_POINT('Ctrl Pts',(-11.0111504217753,21.5263202823811,4.55802661542949));
#92065=CARTESIAN_POINT('Ctrl Pts',(-11.0137782615063,21.5261196015584,4.55550894374324));
#92066=CARTESIAN_POINT('Ctrl Pts',(-11.0207859005637,21.5255805939359,4.54874477863558));
#92067=CARTESIAN_POINT('Ctrl Pts',(-11.0251485363479,21.5252409716897,4.54448070412508));
#92068=CARTESIAN_POINT('Ctrl Pts',(-11.0583035737339,21.5226296032565,4.51166688618668));
#92069=CARTESIAN_POINT('Ctrl Pts',(-11.0859226772531,21.5202783802973,4.48196115951001));
#92070=CARTESIAN_POINT('Ctrl Pts',(-11.1690659715518,21.5127257572951,4.38473377712412));
#92071=CARTESIAN_POINT('Ctrl Pts',(-11.2197981970836,21.5073961710961,4.31336446490505));
#92072=CARTESIAN_POINT('Ctrl Pts',(-11.3016584975888,21.49772045675,4.17315479174647));
#92073=CARTESIAN_POINT('Ctrl Pts',(-11.3344301351383,21.493354600281,4.10559972713085));
#92074=CARTESIAN_POINT('Ctrl Pts',(-11.3679448482733,21.4882409043851,4.02041639713847));
#92075=CARTESIAN_POINT('Ctrl Pts',(-11.3737445244045,21.4873246453876,4.00490825665599));
#92076=CARTESIAN_POINT('Ctrl Pts',(-11.3816219359288,21.4860330771165,3.98270295460613));
#92077=CARTESIAN_POINT('Ctrl Pts',(-11.3839164890509,21.4856506608306,3.97608451975304));
#92078=CARTESIAN_POINT('Ctrl Pts',(-11.3877972302376,21.4849928836044,3.96462569746802));
#92079=CARTESIAN_POINT('Ctrl Pts',(-11.3894058160064,21.4847167923813,3.95979307341665));
#92080=CARTESIAN_POINT('Ctrl Pts',(-11.3924412842639,21.4841890668592,3.95051230878689));
#92081=CARTESIAN_POINT('Ctrl Pts',(-11.3938721597778,21.4839373049291,3.94606554830478));
#92082=CARTESIAN_POINT('Ctrl Pts',(-11.397184965174,21.4833472282806,3.93559867447005));
#92083=CARTESIAN_POINT('Ctrl Pts',(-11.3990493246379,21.4830094872735,3.92957306832552));
#92084=CARTESIAN_POINT('Ctrl Pts',(-11.40535960199,21.4818462163973,3.90870136534874));
#92085=CARTESIAN_POINT('Ctrl Pts',(-11.4096087122984,21.4810270358764,3.89379654555211));
#92086=CARTESIAN_POINT('Ctrl Pts',(-11.4467308269554,21.4735129762302,3.75527256097526));
#92087=CARTESIAN_POINT('Ctrl Pts',(-11.4634999999999,21.4673972845276,3.62791798927615));
#92088=CARTESIAN_POINT('Ctrl Pts',(-11.4635,21.4611504451332,3.50000000000115));
#92089=CARTESIAN_POINT('Ctrl Pts',(-11.4635,21.3891087006547,3.49999999989906));
#92090=CARTESIAN_POINT('Ctrl Pts',(-11.4635000000082,21.396299059564,3.61942455324135));
#92091=CARTESIAN_POINT('Ctrl Pts',(-11.4488819064457,21.4034476858667,3.73842431250034));
#92092=CARTESIAN_POINT('Ctrl Pts',(-11.4160045137088,21.4110348061065,3.87017551169755));
#92093=CARTESIAN_POINT('Ctrl Pts',(-11.4117876336054,21.411938487072,3.88594611052557));
#92094=CARTESIAN_POINT('Ctrl Pts',(-11.4055378386873,21.4131874124851,3.90784460544997));
#92095=CARTESIAN_POINT('Ctrl Pts',(-11.4037270149434,21.4135397598175,3.91403418646385));
#92096=CARTESIAN_POINT('Ctrl Pts',(-11.4005235009538,21.4141470489058,3.9247214841989));
#92097=CARTESIAN_POINT('Ctrl Pts',(-11.3991499195689,21.4144026044021,3.92922478860827));
#92098=CARTESIAN_POINT('Ctrl Pts',(-11.3962524959583,21.4149318192255,3.93856231961155));
#92099=CARTESIAN_POINT('Ctrl Pts',(-11.3947252210479,21.4152053629606,3.94339542094852));
#92100=CARTESIAN_POINT('Ctrl Pts',(-11.3910732724636,21.4158469655779,3.95474651993349));
#92101=CARTESIAN_POINT('Ctrl Pts',(-11.3889278380108,21.4162143426062,3.96125774760939));
#92102=CARTESIAN_POINT('Ctrl Pts',(-11.3817252394348,21.417417140065,3.98261109456256));
#92103=CARTESIAN_POINT('Ctrl Pts',(-11.3764752066174,21.4182462506883,3.99738731033037));
#92104=CARTESIAN_POINT('Ctrl Pts',(-11.3292636805123,21.4253175255697,4.12378725111242));
#92105=CARTESIAN_POINT('Ctrl Pts',(-11.2740437030693,21.4310658466671,4.22997794860489));
#92106=CARTESIAN_POINT('Ctrl Pts',(-11.1623467181847,21.4406756934843,4.39268199255192));
#92107=CARTESIAN_POINT('Ctrl Pts',(-11.1130695486394,21.4445030057006,4.45341727426985));
#92108=CARTESIAN_POINT('Ctrl Pts',(-11.0513696799749,21.4492189029787,4.51812694890517));
#92109=CARTESIAN_POINT('Ctrl Pts',(-11.0434542517006,21.4498227039456,4.52623773902712));
#92110=CARTESIAN_POINT('Ctrl Pts',(-11.0323535385172,21.4506692231751,4.53735122601047));
#92111=CARTESIAN_POINT('Ctrl Pts',(-11.0292475780893,21.4509060501968,4.54043299476479));
#92112=CARTESIAN_POINT('Ctrl Pts',(-11.0242488139958,21.4512872500056,4.54534853625745));
#92113=CARTESIAN_POINT('Ctrl Pts',(-11.0223647703632,21.4514309357564,4.54719122958526));
#92114=CARTESIAN_POINT('Ctrl Pts',(-11.0184194178687,21.4517318750698,4.55102919534127));
#92115=CARTESIAN_POINT('Ctrl Pts',(-11.0163572151585,21.4518892035245,4.55302349967875));
#92116=CARTESIAN_POINT('Ctrl Pts',(-11.011339869751,21.4522720279664,4.55784718001797));
#92117=CARTESIAN_POINT('Ctrl Pts',(-11.0083787098952,21.4524980011133,4.56067024329916));
#92118=CARTESIAN_POINT('Ctrl Pts',(-10.9978878319446,21.4532985824309,4.57058823076288));
#92119=CARTESIAN_POINT('Ctrl Pts',(-10.990294936522,21.4538780069786,4.57761552107226));
#92120=CARTESIAN_POINT('Ctrl Pts',(-10.9106348595005,21.4599508610021,4.64978870188361));
#92121=CARTESIAN_POINT('Ctrl Pts',(-10.8323310993438,21.4658523484903,4.70768048372725));
#92122=CARTESIAN_POINT('Ctrl Pts',(-10.6636701055125,21.4776595746329,4.80813222026336));
#92123=CARTESIAN_POINT('Ctrl Pts',(-10.5735132042922,21.4835265031393,4.85009488892858));
#92124=CARTESIAN_POINT('Ctrl Pts',(-10.4635806071914,21.4900367973308,4.88824339932996));
#92125=CARTESIAN_POINT('Ctrl Pts',(-10.4472708446001,21.4909876635815,4.89358370467582));
#92126=CARTESIAN_POINT('Ctrl Pts',(-10.4238786922607,21.4923306146242,4.90079000135828));
#92127=CARTESIAN_POINT('Ctrl Pts',(-10.4168708189894,21.4927303040876,4.90289147714915));
#92128=CARTESIAN_POINT('Ctrl Pts',(-10.4049500007657,21.4934058084196,4.90636900292444));
#92129=CARTESIAN_POINT('Ctrl Pts',(-10.4000451310839,21.4936824923587,4.90777205879353));
#92130=CARTESIAN_POINT('Ctrl Pts',(-10.3901188711676,21.4942399346962,4.91055543473153));
#92131=CARTESIAN_POINT('Ctrl Pts',(-10.3850972484291,21.4945206543603,4.91193465794634));
#92132=CARTESIAN_POINT('Ctrl Pts',(-10.3727400762796,21.4952083409809,4.9152578113658));
#92133=CARTESIAN_POINT('Ctrl Pts',(-10.3653965184493,21.4956143349415,4.91717155783715));
#92134=CARTESIAN_POINT('Ctrl Pts',(-10.3383769547443,21.4970985724304,4.92398892728958));
#92135=CARTESIAN_POINT('Ctrl Pts',(-10.318614034365,21.4981655994218,4.9285407165118));
#92136=CARTESIAN_POINT('Ctrl Pts',(-10.2109951546144,21.5038854037379,4.95098288513548));
#92137=CARTESIAN_POINT('Ctrl Pts',(-10.121729655085,21.5082887873556,4.96118249698326));
#92138=CARTESIAN_POINT('Ctrl Pts',(-9.92992853709821,21.5176239561816,4.96538836637921));
#92139=CARTESIAN_POINT('Ctrl Pts',(-9.82783213578223,21.5225206155021,4.95692344151619));
#92140=CARTESIAN_POINT('Ctrl Pts',(-9.71697043832576,21.5284816183374,4.9359110733186));
#92141=CARTESIAN_POINT('Ctrl Pts',(-9.706498229179,21.529051339805,4.93380718389019));
#92142=CARTESIAN_POINT('Ctrl Pts',(-9.69187516239833,21.5298573509298,4.93070246801058));
#92143=CARTESIAN_POINT('Ctrl Pts',(-9.68770398137463,21.5300884602971,4.92979777008576));
#92144=CARTESIAN_POINT('Ctrl Pts',(-9.68098368093543,21.5304628254161,4.928309377099));
#92145=CARTESIAN_POINT('Ctrl Pts',(-9.67843203204906,21.5306054394769,4.92773706623591));
#92146=CARTESIAN_POINT('Ctrl Pts',(-9.67306558853104,21.5309063912656,4.92651830749124));
#92147=CARTESIAN_POINT('Ctrl Pts',(-9.67025116274484,21.5310648161495,4.92587036399165));
#92148=CARTESIAN_POINT('Ctrl Pts',(-9.66335892770833,21.5314542005217,4.92426212100243));
#92149=CARTESIAN_POINT('Ctrl Pts',(-9.65928330527601,21.5316856757874,4.92329263818901));
#92150=CARTESIAN_POINT('Ctrl Pts',(-9.64453861928741,21.5325273759645,4.91971830705854));
#92151=CARTESIAN_POINT('Ctrl Pts',(-9.63389507014034,21.5331430820803,4.91701094919041));
#92152=CARTESIAN_POINT('Ctrl Pts',(-9.56569500565599,21.537136145647,4.89884351244477));
#92153=CARTESIAN_POINT('Ctrl Pts',(-9.50910243901627,21.5406674438585,4.88000083132761));
#92154=CARTESIAN_POINT('Ctrl Pts',(-9.39369499913671,21.5481262414772,4.83357666379679));
#92155=CARTESIAN_POINT('Ctrl Pts',(-9.33523932841442,21.5520520350159,4.80542181671792));
#92156=CARTESIAN_POINT('Ctrl Pts',(-9.20969095279338,21.5606384150614,4.73432540275917));
#92157=CARTESIAN_POINT('Ctrl Pts',(-9.14383671507622,21.5652461191646,4.68959455534421));
#92158=CARTESIAN_POINT('Ctrl Pts',(-9.07362143403438,21.5702425261918,4.63303526267893));
#92159=CARTESIAN_POINT('Ctrl Pts',(-9.06538328134277,21.5708303520168,4.6262494180452));
#92160=CARTESIAN_POINT('Ctrl Pts',(-9.05227971458969,21.5717681162534,4.61521308685246));
#92161=CARTESIAN_POINT('Ctrl Pts',(-9.0473670359062,21.5721203338421,4.61101953450838));
#92162=CARTESIAN_POINT('Ctrl Pts',(-9.03868272230908,21.5727441568008,4.60350649411708));
#92163=CARTESIAN_POINT('Ctrl Pts',(-9.03490013913785,21.5730162815768,4.60019986838014));
#92164=CARTESIAN_POINT('Ctrl Pts',(-9.0270405597478,21.5735826044486,4.59325752521818));
#92165=CARTESIAN_POINT('Ctrl Pts',(-9.02296673562821,21.5738766521926,4.58961832319621));
#92166=CARTESIAN_POINT('Ctrl Pts',(-9.012402450437,21.5746405733763,4.58007422033769));
#92167=CARTESIAN_POINT('Ctrl Pts',(-9.00594449612028,21.5751089442167,4.57413355830013));
#92168=CARTESIAN_POINT('Ctrl Pts',(-8.97759692328527,21.577171583483,4.54758204285154));
#92169=CARTESIAN_POINT('Ctrl Pts',(-8.95629125461885,21.5787395449588,4.52635686198655));
#92170=CARTESIAN_POINT('Ctrl Pts',(-8.90027272691854,21.5829291137524,4.46700021312388));
#92171=CARTESIAN_POINT('Ctrl Pts',(-8.86689569467471,21.5854990417828,4.42766624861666));
#92172=CARTESIAN_POINT('Ctrl Pts',(-8.77414649587277,21.5930211415696,4.30586928039764));
#92173=CARTESIAN_POINT('Ctrl Pts',(-8.72120955576969,21.5978324447365,4.21891187167456));
#92174=CARTESIAN_POINT('Ctrl Pts',(-8.66355289207488,21.6046531457452,4.09735365213714));
#92175=CARTESIAN_POINT('Ctrl Pts',(-8.65041864478409,21.6063621962531,4.06705564722612));
#92176=CARTESIAN_POINT('Ctrl Pts',(-8.63620402408808,21.6084368345276,4.03096718776663));
#92177=CARTESIAN_POINT('Ctrl Pts',(-8.63411891939832,21.6087475260663,4.02558014597852));
#92178=CARTESIAN_POINT('Ctrl Pts',(-8.63079238850586,21.6092538856038,4.01683227654651));
#92179=CARTESIAN_POINT('Ctrl Pts',(-8.629531295767,21.6094484246239,4.01347893395347));
#92180=CARTESIAN_POINT('Ctrl Pts',(-8.62730939922858,21.6097958659071,4.00750424542958));
#92181=CARTESIAN_POINT('Ctrl Pts',(-8.62634376999786,21.6099484803674,4.00488474547713));
#92182=CARTESIAN_POINT('Ctrl Pts',(-8.62427682545913,21.6102786854143,3.9992278391402));
#92183=CARTESIAN_POINT('Ctrl Pts',(-8.62317808708969,21.6104564187353,3.99618958882145));
#92184=CARTESIAN_POINT('Ctrl Pts',(-8.62015035700992,21.6109523238718,3.98772976874868));
#92185=CARTESIAN_POINT('Ctrl Pts',(-8.61824328994696,21.6112717419276,3.98230048367763));
#92186=CARTESIAN_POINT('Ctrl Pts',(-8.60749992970006,21.6131117352009,3.95112813176044));
#92187=CARTESIAN_POINT('Ctrl Pts',(-8.59935165171072,21.6146683185928,3.92515532070323));
#92188=CARTESIAN_POINT('Ctrl Pts',(-8.57510736430442,21.6198387214066,3.83959151156066));
#92189=CARTESIAN_POINT('Ctrl Pts',(-8.56205598451551,21.62355128336,3.77920893705136));
#92190=CARTESIAN_POINT('Ctrl Pts',(-8.53569718837198,21.6341987549722,3.60438159422973));
#92191=CARTESIAN_POINT('Ctrl Pts',(-8.53202029854842,21.6410713840203,3.48892978470404));
#92192=CARTESIAN_POINT('Ctrl Pts',(-8.54334599968473,21.6484386677781,3.35763137325285));
#92193=CARTESIAN_POINT('Ctrl Pts',(-8.54506075021879,21.6493611657897,3.34106128796563));
#92194=CARTESIAN_POINT('Ctrl Pts',(-8.54783797473983,21.6506316787789,3.31806591235982));
#92195=CARTESIAN_POINT('Ctrl Pts',(-8.54866094100329,21.6509871206973,3.31161343572553));
#92196=CARTESIAN_POINT('Ctrl Pts',(-8.55015559525731,21.6515982908575,3.30048620793536));
#92197=CARTESIAN_POINT('Ctrl Pts',(-8.55080693787177,21.6518546514241,3.29580886259368));
#92198=CARTESIAN_POINT('Ctrl Pts',(-8.55220296095287,21.6523841904108,3.2861271863853));
#92199=CARTESIAN_POINT('Ctrl Pts',(-8.5529509755268,21.6526572605281,3.2811233947266));
#92200=CARTESIAN_POINT('Ctrl Pts',(-8.55476508418211,21.6532954264855,3.26940398435029));
#92201=CARTESIAN_POINT('Ctrl Pts',(-8.55585206773396,21.6536598617201,3.2626916853773));
#92202=CARTESIAN_POINT('Ctrl Pts',(-8.5595474060199,21.654843001421,3.24083863497887));
#92203=CARTESIAN_POINT('Ctrl Pts',(-8.56234744738258,21.6556556829691,3.2257310623716));
#92204=CARTESIAN_POINT('Ctrl Pts',(-8.57820690049982,21.6598620696137,3.14709348702723));
#92205=CARTESIAN_POINT('Ctrl Pts',(-8.59524139441734,21.6631279102112,3.08443638661618));
#92206=CARTESIAN_POINT('Ctrl Pts',(-8.64832388837808,21.6711603447862,2.93042560695165));
#92207=CARTESIAN_POINT('Ctrl Pts',(-8.6894993367167,21.67581103413,2.84119087886284));
#92208=CARTESIAN_POINT('Ctrl Pts',(-8.74716094007279,21.6815026878103,2.74338440508356));
#92209=CARTESIAN_POINT('Ctrl Pts',(-8.75525056029391,21.6822869272086,2.730148276203));
#92210=CARTESIAN_POINT('Ctrl Pts',(-8.77821095889576,21.6844811522371,2.69388902718335));
#92211=CARTESIAN_POINT('Ctrl Pts',(-8.79351969635526,21.6859093181553,2.67115233702656));
#92212=CARTESIAN_POINT('Ctrl Pts',(-8.81263598908858,21.6876694369555,2.6444131599741));
#92213=CARTESIAN_POINT('Ctrl Pts',(-8.81584016799393,21.6879637192051,2.63998393874469));
#92214=CARTESIAN_POINT('Ctrl Pts',(-8.82112963502436,21.6884485014838,2.63275777127744));
#92215=CARTESIAN_POINT('Ctrl Pts',(-8.82320027096488,21.6886380247415,2.62995010607206));
#92216=CARTESIAN_POINT('Ctrl Pts',(-8.82694193964282,21.6889800981769,2.62491440790014));
#92217=CARTESIAN_POINT('Ctrl Pts',(-8.82860931044412,21.689132396177,2.62268371798023));
#92218=CARTESIAN_POINT('Ctrl Pts',(-8.83226681894093,21.6894661841141,2.61781954033371));
#92219=CARTESIAN_POINT('Ctrl Pts',(-8.83425947728678,21.6896478454222,2.61518805454251));
#92220=CARTESIAN_POINT('Ctrl Pts',(-8.83994636165077,21.690165697717,2.6077305653912));
#92221=CARTESIAN_POINT('Ctrl Pts',(-8.84366172616329,21.690503315778,2.6029208610141));
#92222=CARTESIAN_POINT('Ctrl Pts',(-8.86783893013152,21.6926950256579,2.57202215175352));
#92223=CARTESIAN_POINT('Ctrl Pts',(-8.88915098163295,21.6946026487201,2.546613562257));
#92224=CARTESIAN_POINT('Ctrl Pts',(-8.94321995279271,21.6993405190733,2.48642774225776));
#92225=CARTESIAN_POINT('Ctrl Pts',(-8.97685263418257,21.702203688261,2.45248777621627));
#92226=CARTESIAN_POINT('Ctrl Pts',(-9.10321776134156,21.7125115776972,2.33686951608614));
#92227=CARTESIAN_POINT('Ctrl Pts',(-9.20456201505614,21.7199226053434,2.26534213100808));
#92228=CARTESIAN_POINT('Ctrl Pts',(-9.32783209949298,21.7277166016019,2.19989288638051));
#92229=CARTESIAN_POINT('Ctrl Pts',(-9.34208462899249,21.7286019830116,2.19262263041452));
#92230=CARTESIAN_POINT('Ctrl Pts',(-9.36219656264053,21.7298298692306,2.18277568021352));
#92231=CARTESIAN_POINT('Ctrl Pts',(-9.36795763769513,21.7301791683883,2.18000167143456));
#92232=CARTESIAN_POINT('Ctrl Pts',(-9.3779793532746,21.7307826421209,2.17525677982484));
#92233=CARTESIAN_POINT('Ctrl Pts',(-9.3822316073647,21.7310374122636,2.17326849056468));
#92234=CARTESIAN_POINT('Ctrl Pts',(-9.39110404444629,21.7315663518774,2.16917177830147));
#92235=CARTESIAN_POINT('Ctrl Pts',(-9.3957257892238,21.7318403984058,2.16706687360271));
#92236=CARTESIAN_POINT('Ctrl Pts',(-9.40666453160325,21.7324855602976,2.16215357320406));
#92237=CARTESIAN_POINT('Ctrl Pts',(-9.41299068757409,21.7328559717701,2.15936578101823));
#92238=CARTESIAN_POINT('Ctrl Pts',(-9.43403285327849,21.734079284786,2.15027048020333));
#92239=CARTESIAN_POINT('Ctrl Pts',(-9.44883288276655,21.7349255695233,2.14415951407857));
#92240=CARTESIAN_POINT('Ctrl Pts',(-9.52906867994482,21.7394423698928,2.11256095026807));
#92241=CARTESIAN_POINT('Ctrl Pts',(-9.59617710057964,21.7429615978522,2.09156400279486));
#92242=CARTESIAN_POINT('Ctrl Pts',(-9.76691284034193,21.7515778549495,2.05135787362345));
#92243=CARTESIAN_POINT('Ctrl Pts',(-9.87157660648177,21.7565534298126,2.03835791657455));
#92244=CARTESIAN_POINT('Ctrl Pts',(-10.0060080229752,21.7634070930866,2.03621922122293));
#92245=CARTESIAN_POINT('Ctrl Pts',(-10.035301683776,21.764930057192,2.03663270926404));
#92246=CARTESIAN_POINT('Ctrl Pts',(-10.0701346239639,21.7667963509163,2.03817083469018));
#92247=CARTESIAN_POINT('Ctrl Pts',(-10.0757065422489,21.7670965755635,2.03844880640597));
#92248=CARTESIAN_POINT('Ctrl Pts',(-10.0847940716645,21.767589179462,2.03895426971784));
#92249=CARTESIAN_POINT('Ctrl Pts',(-10.0883107425056,21.7677805279407,2.03916261247456));
#92250=CARTESIAN_POINT('Ctrl Pts',(-10.0946082120583,21.7681245314717,2.0395585242061));
#92251=CARTESIAN_POINT('Ctrl Pts',(-10.0973892590605,21.7682769213467,2.03974134138634));
#92252=CARTESIAN_POINT('Ctrl Pts',(-10.1034360315283,21.768609300604,2.04015618786846));
#92253=CARTESIAN_POINT('Ctrl Pts',(-10.1067014622168,21.7687894504287,2.04039122845712));
#92254=CARTESIAN_POINT('Ctrl Pts',(-10.1159018366542,21.7692988184276,2.04108449595121));
#92255=CARTESIAN_POINT('Ctrl Pts',(-10.1218347422387,21.7696293924527,2.04156797320136));
#92256=CARTESIAN_POINT('Ctrl Pts',(-10.1583232370984,21.7716747568578,2.04476564937557));
#92257=CARTESIAN_POINT('Ctrl Pts',(-10.1887881843106,21.7734353545049,2.04840363262481));
#92258=CARTESIAN_POINT('Ctrl Pts',(-10.3697689285931,21.7841235796752,2.07580881393421));
#92259=CARTESIAN_POINT('Ctrl Pts',(-10.5159487183711,21.7935825196164,2.12200826181782));
#92260=CARTESIAN_POINT('Ctrl Pts',(-10.6817707313447,21.8041691130149,2.20458562574347));
#92261=CARTESIAN_POINT('Ctrl Pts',(-10.7106547921966,21.80601341701,2.22020324260207));
#92262=CARTESIAN_POINT('Ctrl Pts',(-10.7469615037909,21.808333028399,2.24144287583651));
#92263=CARTESIAN_POINT('Ctrl Pts',(-10.7548879323417,21.8088395520228,2.24618113827204));
#92264=CARTESIAN_POINT('Ctrl Pts',(-10.7675935307528,21.8096517765627,2.25394046005246));
#92265=CARTESIAN_POINT('Ctrl Pts',(-10.7724008833816,21.8099591637388,2.2569146923277));
#92266=CARTESIAN_POINT('Ctrl Pts',(-10.7813297440851,21.8105302554633,2.26251063071585));
#92267=CARTESIAN_POINT('Ctrl Pts',(-10.7854555803099,21.8107942135645,2.26512525321639));
#92268=CARTESIAN_POINT('Ctrl Pts',(-10.7936026256696,21.8113156044262,2.2703455441182));
#92269=CARTESIAN_POINT('Ctrl Pts',(-10.797624279808,21.8115730624537,2.27295040143109));
#92270=CARTESIAN_POINT('Ctrl Pts',(-10.8101128630608,21.8123728649195,2.28112669773267));
#92271=CARTESIAN_POINT('Ctrl Pts',(-10.8185348602932,21.8129126752935,2.28676644157736));
#92272=CARTESIAN_POINT('Ctrl Pts',(-10.8661469664403,21.815967985095,2.31937109987882));
#92273=CARTESIAN_POINT('Ctrl Pts',(-10.9040644797114,21.8184138817216,2.34814793507277));
#92274=CARTESIAN_POINT('Ctrl Pts',(-11.0289642439808,21.8266163543261,2.45291256216595));
#92275=CARTESIAN_POINT('Ctrl Pts',(-11.1083182141848,21.8320574296612,2.53730139872324));
#92276=CARTESIAN_POINT('Ctrl Pts',(-11.1863610599694,21.8385838297982,2.64289357858589));
#92277=CARTESIAN_POINT('Ctrl Pts',(-11.1955831183539,21.8393782718541,2.65580513673452));
#92278=CARTESIAN_POINT('Ctrl Pts',(-11.2242499692351,21.8419316305723,2.69735295202304));
#92279=CARTESIAN_POINT('Ctrl Pts',(-11.242888416667,21.8437200462267,2.72652841387841));
#92280=CARTESIAN_POINT('Ctrl Pts',(-11.2634485713923,21.845883648014,2.7613768014552));
#92281=CARTESIAN_POINT('Ctrl Pts',(-11.2663930179554,21.8461984518695,2.76643661230873));
#92282=CARTESIAN_POINT('Ctrl Pts',(-11.2711019299935,21.8467102080988,2.77464137372456));
#92283=CARTESIAN_POINT('Ctrl Pts',(-11.2728852969587,21.8469059918271,2.77777546887162));
#92284=CARTESIAN_POINT('Ctrl Pts',(-11.2760299051731,21.8472547940099,2.78334964032118));
#92285=CARTESIAN_POINT('Ctrl Pts',(-11.2773957614572,21.847407515856,2.78578705877666));
#92286=CARTESIAN_POINT('Ctrl Pts',(-11.2803184063214,21.8477369619707,2.79103782431816));
#92287=CARTESIAN_POINT('Ctrl Pts',(-11.2818728826596,21.8479138224963,2.79385235226335));
#92288=CARTESIAN_POINT('Ctrl Pts',(-11.2861494166674,21.848404893105,2.80165608051859));
#92289=CARTESIAN_POINT('Ctrl Pts',(-11.2888516748809,21.8487203110767,2.80665599457686));
#92290=CARTESIAN_POINT('Ctrl Pts',(-11.3037983379101,21.8504933316307,2.83470071834496));
#92291=CARTESIAN_POINT('Ctrl Pts',(-11.3154530729182,21.8519840091943,2.85805274384681));
#92292=CARTESIAN_POINT('Ctrl Pts',(-11.3507307212526,21.856831431449,2.93373630265889));
#92293=CARTESIAN_POINT('Ctrl Pts',(-11.371900796309,21.8602748106418,2.98714960778562));
#92294=CARTESIAN_POINT('Ctrl Pts',(-11.4216525001829,21.8698378809376,3.13801905024715));
#92295=CARTESIAN_POINT('Ctrl Pts',(-11.4433252705287,21.8759378400675,3.2374295162171));
#92296=CARTESIAN_POINT('Ctrl Pts',(-11.4563522824748,21.8826644899865,3.35460500502699));
#92297=CARTESIAN_POINT('Ctrl Pts',(-11.457891424295,21.8835931616838,3.37094845953377));
#92298=CARTESIAN_POINT('Ctrl Pts',(-11.4605892125318,21.8855578127953,3.40588199734631));
#92299=CARTESIAN_POINT('Ctrl Pts',(-11.4616686110426,21.8865912394602,3.42447541686786));
#92300=CARTESIAN_POINT('Ctrl Pts',(-11.4626808709883,21.8880202694117,3.45048475970381));
#92301=CARTESIAN_POINT('Ctrl Pts',(-11.4629126978096,21.8884250843579,3.45788669104469));
#92302=CARTESIAN_POINT('Ctrl Pts',(-11.4631998693633,21.8890841179268,3.46999153948444));
#92303=CARTESIAN_POINT('Ctrl Pts',(-11.4632887430357,21.8893393724585,3.4746934666286));
#92304=CARTESIAN_POINT('Ctrl Pts',(-11.4634130901352,21.8898174460827,3.48352485824998));
#92305=CARTESIAN_POINT('Ctrl Pts',(-11.4634537519943,21.8900404237556,3.48765419376562));
#92306=CARTESIAN_POINT('Ctrl Pts',(-11.4634923619222,21.8904108660782,3.49453132473303));
#92307=CARTESIAN_POINT('Ctrl Pts',(-11.4635000499487,21.8905586306153,3.49727902167419));
#92308=CARTESIAN_POINT('Ctrl Pts',(-11.4634999997558,21.890706156692,3.5000267339998));
#92309=CARTESIAN_POINT('Origin',(-10.,13.2,3.5));
#92310=CARTESIAN_POINT('',(-11.4635,22.4609791425484,3.50000000009405));
#92311=CARTESIAN_POINT('',(-11.4635,22.3887666433152,3.49999999992021));
#92312=CARTESIAN_POINT('',(-11.4635,13.2,3.5));
#92313=CARTESIAN_POINT('Ctrl Pts',(-11.4635,22.4609791425484,3.50000000009405));
#92314=CARTESIAN_POINT('Ctrl Pts',(-11.4635000000081,22.453441659244,3.3747282078163));
#92315=CARTESIAN_POINT('Ctrl Pts',(-11.4474152347156,22.4459190550057,3.24994710482719));
#92316=CARTESIAN_POINT('Ctrl Pts',(-11.4116157797429,22.438041381404,3.11344773460056));
#92317=CARTESIAN_POINT('Ctrl Pts',(-11.4073613069359,22.4371674081074,3.09823397015972));
#92318=CARTESIAN_POINT('Ctrl Pts',(-11.4010518680726,22.4359531013682,3.07700324437868));
#92319=CARTESIAN_POINT('Ctrl Pts',(-11.3992028591701,22.4356061589841,3.07092663451453));
#92320=CARTESIAN_POINT('Ctrl Pts',(-11.3959221543699,22.4350056870989,3.06039163690732));
#92321=CARTESIAN_POINT('Ctrl Pts',(-11.3945085224811,22.4347515756788,3.05592775880627));
#92322=CARTESIAN_POINT('Ctrl Pts',(-11.3915152500106,22.4342229910092,3.0466310449727));
#92323=CARTESIAN_POINT('Ctrl Pts',(-11.3899317967644,22.4339486461168,3.04179949624827));
#92324=CARTESIAN_POINT('Ctrl Pts',(-11.3861228901722,22.433300981241,3.03037893006756));
#92325=CARTESIAN_POINT('Ctrl Pts',(-11.3838755739913,22.4329283815508,3.02379729739795));
#92326=CARTESIAN_POINT('Ctrl Pts',(-11.3762175534057,22.4316896761417,3.00188164506415));
#92327=CARTESIAN_POINT('Ctrl Pts',(-11.370598120755,22.4308304244476,2.98662151481658));
#92328=CARTESIAN_POINT('Ctrl Pts',(-11.3385840571663,22.4261892278569,2.90395942239943));
#92329=CARTESIAN_POINT('Ctrl Pts',(-11.3074700823218,22.4225686245297,2.83849021529213));
#92330=CARTESIAN_POINT('Ctrl Pts',(-11.2233089145379,22.4142279840878,2.69075364256234));
#92331=CARTESIAN_POINT('Ctrl Pts',(-11.1666182671082,22.4095911108816,2.61097599619532));
#92332=CARTESIAN_POINT('Ctrl Pts',(-11.080156780591,22.4029344120636,2.5119521077098));
#92333=CARTESIAN_POINT('Ctrl Pts',(-11.0570249789257,22.4011844450203,2.48724377881045));
#92334=CARTESIAN_POINT('Ctrl Pts',(-11.028934403681,22.3990636016404,2.45925019332943));
#92335=CARTESIAN_POINT('Ctrl Pts',(-11.0247847753268,22.3987504059162,2.45516397020435));
#92336=CARTESIAN_POINT('Ctrl Pts',(-11.0180334921898,22.3982407936784,2.44859475378917));
#92337=CARTESIAN_POINT('Ctrl Pts',(-11.0154468391288,22.3980455304747,2.4460963519755));
#92338=CARTESIAN_POINT('Ctrl Pts',(-11.0108354820087,22.3976973453942,2.44167506161189));
#92339=CARTESIAN_POINT('Ctrl Pts',(-11.0088144552741,22.3975447167183,2.43974840646015));
#92340=CARTESIAN_POINT('Ctrl Pts',(-11.0044511092749,22.3972151172888,2.43561257730597));
#92341=CARTESIAN_POINT('Ctrl Pts',(-11.0021070449818,22.3970380080602,2.43340537855366));
#92342=CARTESIAN_POINT('Ctrl Pts',(-10.9955881333902,22.396545393596,2.42730755333567));
#92343=CARTESIAN_POINT('Ctrl Pts',(-10.9913978306028,22.3962286677509,2.42343362686863));
#92344=CARTESIAN_POINT('Ctrl Pts',(-10.9676386541808,22.3944329445069,2.40172466305618));
#92345=CARTESIAN_POINT('Ctrl Pts',(-10.9476124065932,22.3929198870113,2.38439979060911));
#92346=CARTESIAN_POINT('Ctrl Pts',(-10.8815916695705,22.3879639938376,2.33034532778859));
#92347=CARTESIAN_POINT('Ctrl Pts',(-10.8338495660784,22.3844305116281,2.29584466678645));
#92348=CARTESIAN_POINT('Ctrl Pts',(-10.683513713846,22.3737101406872,2.2004419133008));
#92349=CARTESIAN_POINT('Ctrl Pts',(-10.5754183893993,22.36657532429,2.14909454356247));
#92350=CARTESIAN_POINT('Ctrl Pts',(-10.4467432856713,22.3589972716214,2.10625657211431));
#92351=CARTESIAN_POINT('Ctrl Pts',(-10.4311229950802,22.358090810679,2.10134589702028));
#92352=CARTESIAN_POINT('Ctrl Pts',(-10.4092327263416,22.3568387600062,2.09486566298727));
#92353=CARTESIAN_POINT('Ctrl Pts',(-10.4030301979122,22.3564860194169,2.09307406349707));
#92354=CARTESIAN_POINT('Ctrl Pts',(-10.3922835171911,22.3558782943612,2.0900467861769));
#92355=CARTESIAN_POINT('Ctrl Pts',(-10.3877449159423,22.3556226934884,2.08879189914717));
#92356=CARTESIAN_POINT('Ctrl Pts',(-10.3783117710276,22.3550936105217,2.08623265329043));
#92357=CARTESIAN_POINT('Ctrl Pts',(-10.3734163480532,22.3548202427096,2.08493175478436));
#92358=CARTESIAN_POINT('Ctrl Pts',(-10.3618912112809,22.3541794477191,2.08193306398127));
#92359=CARTESIAN_POINT('Ctrl Pts',(-10.3552561155014,22.3538126982899,2.08025629834244));
#92360=CARTESIAN_POINT('Ctrl Pts',(-10.3334390649444,22.3526136883446,2.07490539839853));
#92361=CARTESIAN_POINT('Ctrl Pts',(-10.3182097489619,22.3517876834809,2.07142770083017));
#92362=CARTESIAN_POINT('Ctrl Pts',(-10.2374083315898,22.3474589229615,2.05433253577324));
#92363=CARTESIAN_POINT('Ctrl Pts',(-10.171011952334,22.3440930014806,2.04498337836854));
#92364=CARTESIAN_POINT('Ctrl Pts',(-10.0042365798917,22.3358614751077,2.0330785757467));
#92365=CARTESIAN_POINT('Ctrl Pts',(-9.90380919840749,22.3311116340162,2.03623041411179));
#92366=CARTESIAN_POINT('Ctrl Pts',(-9.80171056261637,22.3259191779904,2.04999259914285));
#92367=CARTESIAN_POINT('Ctrl Pts',(-9.79892377927207,22.325777154047,2.05037642236464));
#92368=CARTESIAN_POINT('Ctrl Pts',(-9.76176353436641,22.323879199411,2.05560371404392));
#92369=CARTESIAN_POINT('Ctrl Pts',(-9.72757437776214,22.3220857885533,2.06166027588769));
#92370=CARTESIAN_POINT('Ctrl Pts',(-9.68790742336772,22.319916638834,2.07015217974135));
#92371=CARTESIAN_POINT('Ctrl Pts',(-9.68218678228741,22.3196016383399,2.07141282315864));
#92372=CARTESIAN_POINT('Ctrl Pts',(-9.6729567178659,22.3190896583551,2.07350501289964));
#92373=CARTESIAN_POINT('Ctrl Pts',(-9.66944247320062,22.3188938496718,2.07431526012259));
#92374=CARTESIAN_POINT('Ctrl Pts',(-9.66321175375146,22.3185450665787,2.07577609567074));
#92375=CARTESIAN_POINT('Ctrl Pts',(-9.66049410744754,22.3183923892261,2.07642148046793));
#92376=CARTESIAN_POINT('Ctrl Pts',(-9.65465436318324,22.3180631150732,2.07782597250852));
#92377=CARTESIAN_POINT('Ctrl Pts',(-9.65153295967162,22.3178863826004,2.0785875705009));
#92378=CARTESIAN_POINT('Ctrl Pts',(-9.64290427639287,22.3173958528702,2.08072303197534));
#92379=CARTESIAN_POINT('Ctrl Pts',(-9.63740250363302,22.3170808514538,2.08211865050367));
#92380=CARTESIAN_POINT('Ctrl Pts',(-9.60674267061579,22.3153135029586,2.09008615795025));
#92381=CARTESIAN_POINT('Ctrl Pts',(-9.58175656738352,22.3138283183034,2.09729524541833));
#92382=CARTESIAN_POINT('Ctrl Pts',(-9.50258687594062,22.3090067414711,2.12244085344623));
#92383=CARTESIAN_POINT('Ctrl Pts',(-9.44925630694772,22.3055846408473,2.14288185052232));
#92384=CARTESIAN_POINT('Ctrl Pts',(-9.28622390353112,22.2948152270453,2.21656592506491));
#92385=CARTESIAN_POINT('Ctrl Pts',(-9.18186934398083,22.2875115529114,2.28042963453321));
#92386=CARTESIAN_POINT('Ctrl Pts',(-9.07401023684823,22.2798007898842,2.36658211836855));
#92387=CARTESIAN_POINT('Ctrl Pts',(-9.06155739252458,22.2789067510308,2.37687105026899));
#92388=CARTESIAN_POINT('Ctrl Pts',(-9.04439725640887,22.2776689847781,2.39153401257806));
#92389=CARTESIAN_POINT('Ctrl Pts',(-9.03954487961192,22.2773183172445,2.39573580498567));
#92390=CARTESIAN_POINT('Ctrl Pts',(-9.03118806519789,22.2767131887378,2.40306893188401));
#92391=CARTESIAN_POINT('Ctrl Pts',(-9.02767080347391,22.2764581237428,2.40618545104144));
#92392=CARTESIAN_POINT('Ctrl Pts',(-9.02038881961954,22.2759292380194,2.41270063545079));
#92393=CARTESIAN_POINT('Ctrl Pts',(-9.01662662693801,22.2756555365314,2.41610204220034));
#92394=CARTESIAN_POINT('Ctrl Pts',(-9.00780122110452,22.2750123606508,2.42416488415785));
#92395=CARTESIAN_POINT('Ctrl Pts',(-9.00275303176898,22.2746435787352,2.42884263533469));
#92396=CARTESIAN_POINT('Ctrl Pts',(-8.98619510306899,22.2734308818861,2.44440405381404));
#92397=CARTESIAN_POINT('Ctrl Pts',(-8.97482884685701,22.2725934256301,2.45543918166863));
#92398=CARTESIAN_POINT('Ctrl Pts',(-8.91506276222844,22.2681585679347,2.51537954698643));
#92399=CARTESIAN_POINT('Ctrl Pts',(-8.86997573435278,22.2647060572061,2.56746967331064));
#92400=CARTESIAN_POINT('Ctrl Pts',(-8.7881677395128,22.2579971754959,2.67667201586876));
#92401=CARTESIAN_POINT('Ctrl Pts',(-8.75141949705516,22.2547457390184,2.73354517203979));
#92402=CARTESIAN_POINT('Ctrl Pts',(-8.68650933204098,22.2481577662853,2.85113818227098));
#92403=CARTESIAN_POINT('Ctrl Pts',(-8.65831416395289,22.2448292432934,2.91164934895216));
#92404=CARTESIAN_POINT('Ctrl Pts',(-8.63173297742916,22.2408849473277,2.98064423941501));
#92405=CARTESIAN_POINT('Ctrl Pts',(-8.62917124271432,22.2404946401123,2.98744408602256));
#92406=CARTESIAN_POINT('Ctrl Pts',(-8.62543503637043,22.2399095542948,2.99758982636545));
#92407=CARTESIAN_POINT('Ctrl Pts',(-8.62422187668698,22.2397169894226,3.00092147242979));
#92408=CARTESIAN_POINT('Ctrl Pts',(-8.62207648328155,22.2393717323787,3.00688053734894));
#92409=CARTESIAN_POINT('Ctrl Pts',(-8.6211396383289,22.2392193143046,3.00950624343724));
#92410=CARTESIAN_POINT('Ctrl Pts',(-8.61912527683928,22.2388879693458,3.01520329747373));
#92411=CARTESIAN_POINT('Ctrl Pts',(-8.61805051695262,22.2387088894656,3.01827552509349));
#92412=CARTESIAN_POINT('Ctrl Pts',(-8.6150669486696,22.2382053270773,3.02689628697774));
#92413=CARTESIAN_POINT('Ctrl Pts',(-8.61318127026585,22.2378795359493,3.03245268857771));
#92414=CARTESIAN_POINT('Ctrl Pts',(-8.60212631219366,22.2359244690102,3.06568292527354));
#92415=CARTESIAN_POINT('Ctrl Pts',(-8.59375278051438,22.2342538378012,3.09361263443529));
#92416=CARTESIAN_POINT('Ctrl Pts',(-8.55251670032763,22.2249544152286,3.24774908013765));
#92417=CARTESIAN_POINT('Ctrl Pts',(-8.53580094404877,22.216891924607,3.37766880170769));
#92418=CARTESIAN_POINT('Ctrl Pts',(-8.53660320429906,22.2084222407454,3.5227053797132));
#92419=CARTESIAN_POINT('Ctrl Pts',(-8.53690280324924,22.2075742235998,3.53731390287786));
#92420=CARTESIAN_POINT('Ctrl Pts',(-8.53885701667855,22.204398525715,3.5923682498504));
#92421=CARTESIAN_POINT('Ctrl Pts',(-8.54197063521228,22.2021111663004,3.63274612247325));
#92422=CARTESIAN_POINT('Ctrl Pts',(-8.54793540193512,22.1993236021993,3.68286739055649));
#92423=CARTESIAN_POINT('Ctrl Pts',(-8.54921771331841,22.1987749797223,3.69277666635852));
#92424=CARTESIAN_POINT('Ctrl Pts',(-8.55140304503727,22.1979135307653,3.7084049396166));
#92425=CARTESIAN_POINT('Ctrl Pts',(-8.55223867610499,22.1975986064184,3.71413291937994));
#92426=CARTESIAN_POINT('Ctrl Pts',(-8.55385492399381,22.1970152637434,3.72476959656631));
#92427=CARTESIAN_POINT('Ctrl Pts',(-8.5546266027463,22.1967465695821,3.72967955014046));
#92428=CARTESIAN_POINT('Ctrl Pts',(-8.55639139683723,22.1961530966896,3.7405471452594));
#92429=CARTESIAN_POINT('Ctrl Pts',(-8.55739641309606,22.1958286967279,3.74650278044281));
#92430=CARTESIAN_POINT('Ctrl Pts',(-8.56041170243848,22.1948931580168,3.76372080297073));
#92431=CARTESIAN_POINT('Ctrl Pts',(-8.56251722499109,22.1942850197878,3.7749661976395));
#92432=CARTESIAN_POINT('Ctrl Pts',(-8.58084439463448,22.189335888439,3.86687842309058));
#92433=CARTESIAN_POINT('Ctrl Pts',(-8.60371115984457,22.1852185581605,3.94607416589016));
#92434=CARTESIAN_POINT('Ctrl Pts',(-8.66190954830837,22.1772388119776,4.09819678910241));
#92435=CARTESIAN_POINT('Ctrl Pts',(-8.69686769078022,22.1733841527389,4.17094762434115));
#92436=CARTESIAN_POINT('Ctrl Pts',(-8.74347906824812,22.1687953875763,4.25041379766014));
#92437=CARTESIAN_POINT('Ctrl Pts',(-8.74944188972407,22.1682167027023,4.260309229143));
#92438=CARTESIAN_POINT('Ctrl Pts',(-8.77477775253492,22.1657877883902,4.30125014612093));
#92439=CARTESIAN_POINT('Ctrl Pts',(-8.7951932255784,22.1639013047104,4.33163187179823));
#92440=CARTESIAN_POINT('Ctrl Pts',(-8.82022333003114,22.1616275792496,4.36602229928506));
#92441=CARTESIAN_POINT('Ctrl Pts',(-8.82375198188072,22.1613078790986,4.37080894077497));
#92442=CARTESIAN_POINT('Ctrl Pts',(-8.82946001563113,22.160791831555,4.3784539338452));
#92443=CARTESIAN_POINT('Ctrl Pts',(-8.83162096265796,22.1605967163792,4.38132604263797));
#92444=CARTESIAN_POINT('Ctrl Pts',(-8.83548318118876,22.1602483767575,4.38642013753526));
#92445=CARTESIAN_POINT('Ctrl Pts',(-8.83718027028188,22.1600954426378,4.38864523720031));
#92446=CARTESIAN_POINT('Ctrl Pts',(-8.84082115155021,22.1597675990558,4.39339060717344));
#92447=CARTESIAN_POINT('Ctrl Pts',(-8.84276675543991,22.159592566684,4.39590936872275));
#92448=CARTESIAN_POINT('Ctrl Pts',(-8.84812046434553,22.1591114142786,4.40279369671992));
#92449=CARTESIAN_POINT('Ctrl Pts',(-8.85154512261252,22.1588041628705,4.40714624845664));
#92450=CARTESIAN_POINT('Ctrl Pts',(-8.86993469438994,22.1571575962457,4.43024733951644));
#92451=CARTESIAN_POINT('Ctrl Pts',(-8.88533337436298,22.15579038881,4.44864423474454));
#92452=CARTESIAN_POINT('Ctrl Pts',(-8.93416628567594,22.151511040341,4.50415407153844));
#92453=CARTESIAN_POINT('Ctrl Pts',(-8.96905260893748,22.1485319418415,4.53993931794324));
#92454=CARTESIAN_POINT('Ctrl Pts',(-9.09811103967232,22.1379645422718,4.65943540509156));
#92455=CARTESIAN_POINT('Ctrl Pts',(-9.20120310006712,22.1303614756987,4.73273211345151));
#92456=CARTESIAN_POINT('Ctrl Pts',(-9.33003685209406,22.1221616190645,4.80129931551687));
#92457=CARTESIAN_POINT('Ctrl Pts',(-9.34784457455688,22.1210526730699,4.81031442199412));
#92458=CARTESIAN_POINT('Ctrl Pts',(-9.3728375928425,22.1195292855669,4.82233127214512));
#92459=CARTESIAN_POINT('Ctrl Pts',(-9.37987024524739,22.119104189983,4.82564390723366));
#92460=CARTESIAN_POINT('Ctrl Pts',(-9.39121516927925,22.1184240610725,4.83087774064756));
#92461=CARTESIAN_POINT('Ctrl Pts',(-9.39551085965176,22.1181678197877,4.83283435227153));
#92462=CARTESIAN_POINT('Ctrl Pts',(-9.40442898698283,22.1176384768501,4.83684441909221));
#92463=CARTESIAN_POINT('Ctrl Pts',(-9.40905275875837,22.1173654836952,4.83889476485651));
#92464=CARTESIAN_POINT('Ctrl Pts',(-9.4199168894195,22.1167274118548,4.84364506656454));
#92465=CARTESIAN_POINT('Ctrl Pts',(-9.42616564823459,22.116362994089,4.84632559915584));
#92466=CARTESIAN_POINT('Ctrl Pts',(-9.44659962658261,22.1151795524961,4.85492306052979));
#92467=CARTESIAN_POINT('Ctrl Pts',(-9.46085966915013,22.1143665575774,4.86066020758447));
#92468=CARTESIAN_POINT('Ctrl Pts',(-9.5358121100377,22.1101564696417,4.88945194186944));
#92469=CARTESIAN_POINT('Ctrl Pts',(-9.59790134507879,22.1068875170248,4.90867491018563));
#92470=CARTESIAN_POINT('Ctrl Pts',(-9.75557643684844,22.0988959128173,4.94621144036176));
#92471=CARTESIAN_POINT('Ctrl Pts',(-9.8520848686336,22.0942851976122,4.95924287508606));
#92472=CARTESIAN_POINT('Ctrl Pts',(-9.95996801387705,22.0888786143383,4.9629923048275));
#92473=CARTESIAN_POINT('Ctrl Pts',(-9.97077226603069,22.0883341632263,4.96324802263293));
#92474=CARTESIAN_POINT('Ctrl Pts',(-10.0139753732146,22.0861417915224,4.96379188538768));
#92475=CARTESIAN_POINT('Ctrl Pts',(-10.0463749145489,22.0844633937425,4.96312373410443));
#92476=CARTESIAN_POINT('Ctrl Pts',(-10.0844592918168,22.0824231496989,4.96107216693288));
#92477=CARTESIAN_POINT('Ctrl Pts',(-10.0901934839031,22.0821141558287,4.96072940076222));
#92478=CARTESIAN_POINT('Ctrl Pts',(-10.0994901061791,22.0816100594823,4.96011873853654));
#92479=CARTESIAN_POINT('Ctrl Pts',(-10.1030538898299,22.0814160700342,4.95987153787275));
#92480=CARTESIAN_POINT('Ctrl Pts',(-10.1093993832349,22.0810692735898,4.95940803397205));
#92481=CARTESIAN_POINT('Ctrl Pts',(-10.112181416177,22.0809167507836,4.95919682167899));
#92482=CARTESIAN_POINT('Ctrl Pts',(-10.1181887464026,22.0805863565253,4.95872346286045));
#92483=CARTESIAN_POINT('Ctrl Pts',(-10.121413736495,22.0804083398846,4.95845857844769));
#92484=CARTESIAN_POINT('Ctrl Pts',(-10.1303974613309,22.0799106936558,4.95769069705039));
#92485=CARTESIAN_POINT('Ctrl Pts',(-10.1361540684313,22.0795898033474,4.95716427816398));
#92486=CARTESIAN_POINT('Ctrl Pts',(-10.1694440945456,22.0777230917166,4.95392105031625));
#92487=CARTESIAN_POINT('Ctrl Pts',(-10.1968975041733,22.0761400504187,4.95045816582561));
#92488=CARTESIAN_POINT('Ctrl Pts',(-10.3376128891108,22.0678564580878,4.92864044099296));
#92489=CARTESIAN_POINT('Ctrl Pts',(-10.4485305027671,22.0607953565512,4.89779036562906));
#92490=CARTESIAN_POINT('Ctrl Pts',(-10.6192529357573,22.0498829116838,4.82786401519054));
#92491=CARTESIAN_POINT('Ctrl Pts',(-10.6818304502024,22.0458635700918,4.79684481337659));
#92492=CARTESIAN_POINT('Ctrl Pts',(-10.7517847537885,22.0413680693651,4.75569970496187));
#92493=CARTESIAN_POINT('Ctrl Pts',(-10.7615379957926,22.0407410631841,4.7498087679152));
#92494=CARTESIAN_POINT('Ctrl Pts',(-10.7763472171529,22.0397884781689,4.74062630162041));
#92495=CARTESIAN_POINT('Ctrl Pts',(-10.7814531447003,22.0394599440512,4.73741650466368));
#92496=CARTESIAN_POINT('Ctrl Pts',(-10.7906256409295,22.0388695228771,4.73157087815094));
#92497=CARTESIAN_POINT('Ctrl Pts',(-10.7946992159788,22.0386072299439,4.72894625143294));
#92498=CARTESIAN_POINT('Ctrl Pts',(-10.8026742588822,22.0380935338403,4.72375165335497));
#92499=CARTESIAN_POINT('Ctrl Pts',(-10.8065766027964,22.0378420811543,4.72118313920472));
#92500=CARTESIAN_POINT('Ctrl Pts',(-10.8175261332349,22.0371362335968,4.71390080025658));
#92501=CARTESIAN_POINT('Ctrl Pts',(-10.8245448181947,22.0366834317571,4.70914431655468));
#92502=CARTESIAN_POINT('Ctrl Pts',(-10.8539819317172,22.0347824029638,4.68881960158661));
#92503=CARTESIAN_POINT('Ctrl Pts',(-10.8760046323874,22.0333555619906,4.67268631540138));
#92504=CARTESIAN_POINT('Ctrl Pts',(-10.9329757461267,22.0296395929748,4.62844961090898));
#92505=CARTESIAN_POINT('Ctrl Pts',(-10.9671066525063,22.0273881298577,4.59933952514363));
#92506=CARTESIAN_POINT('Ctrl Pts',(-11.0598057092244,22.0211109455964,4.51261316555036));
#92507=CARTESIAN_POINT('Ctrl Pts',(-11.1149341768736,22.0171837786732,4.4515750286615));
#92508=CARTESIAN_POINT('Ctrl Pts',(-11.2016955977774,22.0101313039045,4.33755706769133));
#92509=CARTESIAN_POINT('Ctrl Pts',(-11.2356460165396,22.0070605143647,4.28660755910382));
#92510=CARTESIAN_POINT('Ctrl Pts',(-11.269930599622,22.003411907177,4.22743439232937));
#92511=CARTESIAN_POINT('Ctrl Pts',(-11.2735087064465,22.0030235261731,4.22115192110603));
#92512=CARTESIAN_POINT('Ctrl Pts',(-11.2787683912248,22.0024407777463,4.21175569702305));
#92513=CARTESIAN_POINT('Ctrl Pts',(-11.2804855179427,22.0022485982691,4.20866184350611));
#92514=CARTESIAN_POINT('Ctrl Pts',(-11.2835351856019,22.0019037550703,4.20311979535971));
#92515=CARTESIAN_POINT('Ctrl Pts',(-11.2848719687843,22.0017513627127,4.2006739919366));
#92516=CARTESIAN_POINT('Ctrl Pts',(-11.2877571490049,22.001419748754,4.19535919027451));
#92517=CARTESIAN_POINT('Ctrl Pts',(-11.2893029278831,22.0012403719883,4.19248887213935));
#92518=CARTESIAN_POINT('Ctrl Pts',(-11.2936154835886,22.0007351535464,4.18441650125373));
#92519=CARTESIAN_POINT('Ctrl Pts',(-11.2963604217629,22.0004079896983,4.17920293067916));
#92520=CARTESIAN_POINT('Ctrl Pts',(-11.3126994443173,21.9984271683819,4.14770968867428));
#92521=CARTESIAN_POINT('Ctrl Pts',(-11.3255246337247,21.9967309077959,4.12104095865997));
#92522=CARTESIAN_POINT('Ctrl Pts',(-11.3926644296615,21.987084682709,3.96986077497243));
#92523=CARTESIAN_POINT('Ctrl Pts',(-11.4302488217402,21.9786761397781,3.83864269421216));
#92524=CARTESIAN_POINT('Ctrl Pts',(-11.4559229522552,21.9679796483223,3.65635356779133));
#92525=CARTESIAN_POINT('Ctrl Pts',(-11.4602848338256,21.9652394749179,3.6082914467565));
#92526=CARTESIAN_POINT('Ctrl Pts',(-11.4626948800845,21.9619945793909,3.54965124027359));
#92527=CARTESIAN_POINT('Ctrl Pts',(-11.4630122637918,21.9614200016354,3.53920053386947));
#92528=CARTESIAN_POINT('Ctrl Pts',(-11.4633246277521,21.9605513674528,3.52330133005845));
#92529=CARTESIAN_POINT('Ctrl Pts',(-11.4634012166515,21.960254790277,3.51785492628046));
#92530=CARTESIAN_POINT('Ctrl Pts',(-11.4634713637882,21.9598057384796,3.50958161548477));
#92531=CARTESIAN_POINT('Ctrl Pts',(-11.4634871404727,21.9596525759417,3.50675498409382));
#92532=CARTESIAN_POINT('Ctrl Pts',(-11.4634981925777,21.9594298416703,3.50263751532071));
#92533=CARTESIAN_POINT('Ctrl Pts',(-11.4634999496205,21.9593600692025,3.50134671354812));
#92534=CARTESIAN_POINT('Ctrl Pts',(-11.4634999989321,21.9592903496774,3.50005590890961));
#92535=CARTESIAN_POINT('Ctrl Pts',(-11.4634999997572,21.8907061526447,3.50002665861792));
#92536=CARTESIAN_POINT('Ctrl Pts',(-11.4634998748308,21.8910743722622,3.50688484649636));
#92537=CARTESIAN_POINT('Ctrl Pts',(-11.463451542126,21.8914411004734,3.51374303113273));
#92538=CARTESIAN_POINT('Ctrl Pts',(-11.463197530598,21.892402160295,3.53178653891741));
#92539=CARTESIAN_POINT('Ctrl Pts',(-11.4629118060168,21.8929940237266,3.54297039138399));
#92540=CARTESIAN_POINT('Ctrl Pts',(-11.4602288213616,21.8968058150075,3.61543306443494));
#92541=CARTESIAN_POINT('Ctrl Pts',(-11.4541101003046,21.8999085988066,3.67651606038468));
#92542=CARTESIAN_POINT('Ctrl Pts',(-11.4274677810593,21.9080509034445,3.83883538003897));
#92543=CARTESIAN_POINT('Ctrl Pts',(-11.4000451466615,21.9129317401083,3.93857182873777));
#92544=CARTESIAN_POINT('Ctrl Pts',(-11.3517927132806,21.9195492143766,4.06153960555146));
#92545=CARTESIAN_POINT('Ctrl Pts',(-11.3404216078735,21.9210220395044,4.08816664706924));
#92546=CARTESIAN_POINT('Ctrl Pts',(-11.3235812573302,21.9231139835003,4.12457151651568));
#92547=CARTESIAN_POINT('Ctrl Pts',(-11.3187777212497,21.9237017266148,4.13465126820184));
#92548=CARTESIAN_POINT('Ctrl Pts',(-11.3102421852116,21.924732572778,4.1520468526634));
#92549=CARTESIAN_POINT('Ctrl Pts',(-11.3065630155415,21.9251727914233,4.15938817261978));
#92550=CARTESIAN_POINT('Ctrl Pts',(-11.301124435131,21.9258181911071,4.1700159296998));
#92551=CARTESIAN_POINT('Ctrl Pts',(-11.2994138747964,21.9260204407393,4.17332735211605));
#92552=CARTESIAN_POINT('Ctrl Pts',(-11.2963923507264,21.9263764614262,4.17912223430904));
#92553=CARTESIAN_POINT('Ctrl Pts',(-11.2950868638673,21.9265298901638,4.18160850281825));
#92554=CARTESIAN_POINT('Ctrl Pts',(-11.292304578325,21.9268560711533,4.18687044756367));
#92555=CARTESIAN_POINT('Ctrl Pts',(-11.2908260125752,21.9270289292762,4.18964508246653));
#92556=CARTESIAN_POINT('Ctrl Pts',(-11.2868024026863,21.9274979874139,4.19713740424601));
#92557=CARTESIAN_POINT('Ctrl Pts',(-11.2842403866769,21.9277952273199,4.20184586011237));
#92558=CARTESIAN_POINT('Ctrl Pts',(-11.2724562859347,21.9291555719528,4.223222034322));
#92559=CARTESIAN_POINT('Ctrl Pts',(-11.2629355871003,21.9302358839294,4.23972207080109));
#92560=CARTESIAN_POINT('Ctrl Pts',(-11.2003879433655,21.9371953382564,4.34339273009055));
#92561=CARTESIAN_POINT('Ctrl Pts',(-11.1386909554315,21.9434363486893,4.42499959528285));
#92562=CARTESIAN_POINT('Ctrl Pts',(-11.0085140950354,21.9548446394095,4.5642264468861));
#92563=CARTESIAN_POINT('Ctrl Pts',(-10.9422604566426,21.9600235828667,4.62331123269489));
#92564=CARTESIAN_POINT('Ctrl Pts',(-10.8600809710249,21.965709236107,4.68417888342102));
#92565=CARTESIAN_POINT('Ctrl Pts',(-10.8489886807373,21.9664629160807,4.69215650920394));
#92566=CARTESIAN_POINT('Ctrl Pts',(-10.8326263598107,21.9675550849795,4.70358015682235));
#92567=CARTESIAN_POINT('Ctrl Pts',(-10.8274434497495,21.9678982236067,4.70714919879279));
#92568=CARTESIAN_POINT('Ctrl Pts',(-10.8221661803877,21.968244795917,4.71073326099728));
#92569=CARTESIAN_POINT('Ctrl Pts',(-10.8220947328629,21.9682494875455,4.71078177540692));
#92570=CARTESIAN_POINT('Ctrl Pts',(-10.821951768276,21.968258874328,4.71087883295523));
#92571=CARTESIAN_POINT('Ctrl Pts',(-10.8218802512169,21.9682635694809,4.71092737607618));
#92572=CARTESIAN_POINT('Ctrl Pts',(-10.8217369152581,21.9682729785585,4.71102464864867));
#92573=CARTESIAN_POINT('Ctrl Pts',(-10.8216650963192,21.9682776924817,4.71107337805077));
#92574=CARTESIAN_POINT('Ctrl Pts',(-10.8215209097618,21.968287155287,4.71117119040635));
#92575=CARTESIAN_POINT('Ctrl Pts',(-10.8214485420768,21.9682919041657,4.71122027326418));
#92576=CARTESIAN_POINT('Ctrl Pts',(-10.8213029921463,21.968301454304,4.71131897240524));
#92577=CARTESIAN_POINT('Ctrl Pts',(-10.8212298098202,21.9683062555571,4.71136858853121));
#92578=CARTESIAN_POINT('Ctrl Pts',(-10.8210823402887,21.9683159294532,4.71146855036329));
#92579=CARTESIAN_POINT('Ctrl Pts',(-10.8210080529223,21.9683208020904,4.71151889588647));
#92580=CARTESIAN_POINT('Ctrl Pts',(-10.8208580517571,21.9683306397945,4.71162053351247));
#92581=CARTESIAN_POINT('Ctrl Pts',(-10.8207823377936,21.9683356048505,4.7116718253428));
#92582=CARTESIAN_POINT('Ctrl Pts',(-10.8206291222447,21.9683456510101,4.71177559906311));
#92583=CARTESIAN_POINT('Ctrl Pts',(-10.820551620425,21.9683507321014,4.71182808061982));
#92584=CARTESIAN_POINT('Ctrl Pts',(-10.8203944175345,21.9683610372319,4.71193451099511));
#92585=CARTESIAN_POINT('Ctrl Pts',(-10.8203147161731,21.9683662612553,4.71198845938921));
#92586=CARTESIAN_POINT('Ctrl Pts',(-10.8201526380789,21.9683768833484,4.71209814377574));
#92587=CARTESIAN_POINT('Ctrl Pts',(-10.8200702609818,21.9683822813983,4.7121538792355));
#92588=CARTESIAN_POINT('Ctrl Pts',(-10.8199022722045,21.968393288052,4.71226751367654));
#92589=CARTESIAN_POINT('Ctrl Pts',(-10.8198166600698,21.9683988966308,4.71232541198875));
#92590=CARTESIAN_POINT('Ctrl Pts',(-10.8196415337722,21.9684103678967,4.7124438204675));
#92591=CARTESIAN_POINT('Ctrl Pts',(-10.8195520190268,21.9684162305528,4.71250432979987));
#92592=CARTESIAN_POINT('Ctrl Pts',(-10.8193682770411,21.9684282628382,4.71262850432881));
#92593=CARTESIAN_POINT('Ctrl Pts',(-10.8192740491149,21.9684344324249,4.71269216843304));
#92594=CARTESIAN_POINT('Ctrl Pts',(-10.8190798781763,21.9684471439426,4.71282332501919));
#92595=CARTESIAN_POINT('Ctrl Pts',(-10.8189799342142,21.9684536858237,4.71289081614891));
#92596=CARTESIAN_POINT('Ctrl Pts',(-10.8187730647724,21.9684672244734,4.71303047572784));
#92597=CARTESIAN_POINT('Ctrl Pts',(-10.8186661381075,21.9684742211739,4.71310264238333));
#92598=CARTESIAN_POINT('Ctrl Pts',(-10.8184436652786,21.9684887761839,4.7132527503332));
#92599=CARTESIAN_POINT('Ctrl Pts',(-10.8183281174961,21.9684963344059,4.71333068927688));
#92600=CARTESIAN_POINT('Ctrl Pts',(-10.818086224307,21.9685121543227,4.7134938000734));
#92601=CARTESIAN_POINT('Ctrl Pts',(-10.8179598767135,21.9685204158973,4.7135789687137));
#92602=CARTESIAN_POINT('Ctrl Pts',(-10.8176933891285,21.9685378375021,4.71375854267936));
#92603=CARTESIAN_POINT('Ctrl Pts',(-10.8175532460828,21.968546997362,4.71385294347014));
#92604=CARTESIAN_POINT('Ctrl Pts',(-10.8136038127563,21.9688050796486,4.71651229979693));
#92605=CARTESIAN_POINT('Ctrl Pts',(-10.8097824573528,21.9690533301211,4.71905935545328));
#92606=CARTESIAN_POINT('Ctrl Pts',(-10.8010925827219,21.9696145841972,4.72479254432749));
#92607=CARTESIAN_POINT('Ctrl Pts',(-10.7962169081917,21.9699271783823,4.72796772725514));
#92608=CARTESIAN_POINT('Ctrl Pts',(-10.7825403764259,21.9707976723271,4.73675858462343));
#92609=CARTESIAN_POINT('Ctrl Pts',(-10.7736980794,21.9713531835782,4.74230935231646));
#92610=CARTESIAN_POINT('Ctrl Pts',(-10.7240156703094,21.9744351813889,4.77276136284784));
#92611=CARTESIAN_POINT('Ctrl Pts',(-10.6820313126561,21.9768916026595,4.79574459928614));
#92612=CARTESIAN_POINT('Ctrl Pts',(-10.5164223427695,21.9861438710776,4.876118669063));
#92613=CARTESIAN_POINT('Ctrl Pts',(-10.3861620492173,21.9924623938844,4.91819135349303));
#92614=CARTESIAN_POINT('Ctrl Pts',(-10.2228014318503,22.0009183102586,4.94674428002749));
#92615=CARTESIAN_POINT('Ctrl Pts',(-10.1934793515914,22.0024590523433,4.95095657868612));
#92616=CARTESIAN_POINT('Ctrl Pts',(-10.1581937435553,22.0043616300477,4.95493702358752));
#92617=CARTESIAN_POINT('Ctrl Pts',(-10.1523318822887,22.0046792957759,4.95556243369102));
#92618=CARTESIAN_POINT('Ctrl Pts',(-10.1432214159017,22.0051757079196,4.95647880628542));
#92619=CARTESIAN_POINT('Ctrl Pts',(-10.1399752791049,22.005353115199,4.95679436021216));
#92620=CARTESIAN_POINT('Ctrl Pts',(-10.1339520315398,22.0056833261085,4.95735955684384));
#92621=CARTESIAN_POINT('Ctrl Pts',(-10.1311752473293,22.0058359663863,4.95761211533821));
#92622=CARTESIAN_POINT('Ctrl Pts',(-10.1248719459341,22.0061833826945,4.9581672657449));
#92623=CARTESIAN_POINT('Ctrl Pts',(-10.121345058097,22.0063784237152,4.95846499927265));
#92624=CARTESIAN_POINT('Ctrl Pts',(-10.1106091762258,22.0069740388085,4.95933209178829));
#92625=CARTESIAN_POINT('Ctrl Pts',(-10.1033971230959,22.0073767724275,4.95986080656225));
#92626=CARTESIAN_POINT('Ctrl Pts',(-10.0351607744107,22.0112100412938,4.96435503330603));
#92627=CARTESIAN_POINT('Ctrl Pts',(-9.97395390869413,22.014818850994,4.96454498525115));
#92628=CARTESIAN_POINT('Ctrl Pts',(-9.85267291100218,22.0220921318146,4.95731595535349));
#92629=CARTESIAN_POINT('Ctrl Pts',(-9.79270372475452,22.0257479281469,4.95000120308259));
#92630=CARTESIAN_POINT('Ctrl Pts',(-9.67477066658229,22.032915489132,4.92814856277899));
#92631=CARTESIAN_POINT('Ctrl Pts',(-9.61689785912112,22.0364217347995,4.91372428260201));
#92632=CARTESIAN_POINT('Ctrl Pts',(-9.52848053384113,22.0417176537997,4.88585642973307));
#92633=CARTESIAN_POINT('Ctrl Pts',(-9.49724538710658,22.043576981709,4.87483333514987));
#92634=CARTESIAN_POINT('Ctrl Pts',(-9.45796564231367,22.0459014153428,4.85945328319706));
#92635=CARTESIAN_POINT('Ctrl Pts',(-9.44955285351882,22.0463984569333,4.85606873654565));
#92636=CARTESIAN_POINT('Ctrl Pts',(-9.43606349337157,22.0471942588067,4.85049561902494));
#92637=CARTESIAN_POINT('Ctrl Pts',(-9.43096700766257,22.0474946537564,4.84835613074385));
#92638=CARTESIAN_POINT('Ctrl Pts',(-9.42127744166367,22.0480652931244,4.84422375982401));
#92639=CARTESIAN_POINT('Ctrl Pts',(-9.41668223765199,22.0483357078916,4.84223608392613));
#92640=CARTESIAN_POINT('Ctrl Pts',(-9.40620211852893,22.0489519996026,4.83763887734628));
#92641=CARTESIAN_POINT('Ctrl Pts',(-9.40032401655242,22.0492973514997,4.83501401000542));
#92642=CARTESIAN_POINT('Ctrl Pts',(-9.38502669995551,22.0501953902724,4.82806157047441));
#92643=CARTESIAN_POINT('Ctrl Pts',(-9.37563571615882,22.050745981241,4.82367252111219));
#92644=CARTESIAN_POINT('Ctrl Pts',(-9.30670012967024,22.0547839013786,4.79055732755841));
#92645=CARTESIAN_POINT('Ctrl Pts',(-9.24911316879043,22.0581313113593,4.75792419203766));
#92646=CARTESIAN_POINT('Ctrl Pts',(-9.09528193418636,22.067248115937,4.65641051571358));
#92647=CARTESIAN_POINT('Ctrl Pts',(-9.0048977651671,22.0727919791811,4.57961413658884));
#92648=CARTESIAN_POINT('Ctrl Pts',(-8.90572674350895,22.0802644833843,4.4722055869489));
#92649=CARTESIAN_POINT('Ctrl Pts',(-8.88731182132546,22.0817251183974,4.45107438017727));
#92650=CARTESIAN_POINT('Ctrl Pts',(-8.86583040885561,22.0835380228467,4.42494609002167));
#92651=CARTESIAN_POINT('Ctrl Pts',(-8.86217150719607,22.0838508233243,4.42044133415475));
#92652=CARTESIAN_POINT('Ctrl Pts',(-8.85651087972144,22.0843412568194,4.41338676876146));
#92653=CARTESIAN_POINT('Ctrl Pts',(-8.8544906275482,22.0845176021297,4.4108518182182));
#92654=CARTESIAN_POINT('Ctrl Pts',(-8.85074691273074,22.0848468810217,4.40612216530549));
#92655=CARTESIAN_POINT('Ctrl Pts',(-8.84902129642667,22.0849996594038,4.40392923427325));
#92656=CARTESIAN_POINT('Ctrl Pts',(-8.84510405772229,22.0853487568711,4.39892176370605));
#92657=CARTESIAN_POINT('Ctrl Pts',(-8.84291645515684,22.0855453516001,4.39610414821671));
#92658=CARTESIAN_POINT('Ctrl Pts',(-8.83724472560966,22.0860592837821,4.38874360719605));
#92659=CARTESIAN_POINT('Ctrl Pts',(-8.8337769508376,22.0863777089599,4.38418822931801));
#92660=CARTESIAN_POINT('Ctrl Pts',(-8.81110553810187,22.0884867157653,4.35404094500185));
#92661=CARTESIAN_POINT('Ctrl Pts',(-8.7927201450553,22.0903269564238,4.32784722532375));
#92662=CARTESIAN_POINT('Ctrl Pts',(-8.76401506284007,22.0933957444598,4.28395900695168));
#92663=CARTESIAN_POINT('Ctrl Pts',(-8.75318117746453,22.094605200493,4.26661154681494));
#92664=CARTESIAN_POINT('Ctrl Pts',(-8.69632430617389,22.1012188882643,4.17117606652502));
#92665=CARTESIAN_POINT('Ctrl Pts',(-8.65726497784818,22.1067439338684,4.08916181754542));
#92666=CARTESIAN_POINT('Ctrl Pts',(-8.60447708175757,22.1157990278512,3.94527425252378));
#92667=CARTESIAN_POINT('Ctrl Pts',(-8.58670308899088,22.1194124833181,3.88515812811265));
#92668=CARTESIAN_POINT('Ctrl Pts',(-8.56949346164546,22.1237436465362,3.80937167794232));
#92669=CARTESIAN_POINT('Ctrl Pts',(-8.56638065445041,22.1245771586564,3.79461056906044));
#92670=CARTESIAN_POINT('Ctrl Pts',(-8.56220607494877,22.1257731844546,3.77317839827974));
#92671=CARTESIAN_POINT('Ctrl Pts',(-8.56096145088509,22.1261414485365,3.76654430119513));
#92672=CARTESIAN_POINT('Ctrl Pts',(-8.55886570598945,22.1267827726359,3.75493079787183));
#92673=CARTESIAN_POINT('Ctrl Pts',(-8.55799439364573,22.1270564651864,3.74995519040138));
#92674=CARTESIAN_POINT('Ctrl Pts',(-8.55635610290043,22.1275851939063,3.74030600803198));
#92675=CARTESIAN_POINT('Ctrl Pts',(-8.5555860168554,22.1278403247682,3.73563303068786));
#92676=CARTESIAN_POINT('Ctrl Pts',(-8.55380391283131,22.1284469758645,3.72448188544319));
#92677=CARTESIAN_POINT('Ctrl Pts',(-8.55281271422711,22.1287978399415,3.71800046153499));
#92678=CARTESIAN_POINT('Ctrl Pts',(-8.54941132236074,22.1300524204314,3.69471260025974));
#92679=CARTESIAN_POINT('Ctrl Pts',(-8.54725001769878,22.130948367659,3.67787082067707));
#92680=CARTESIAN_POINT('Ctrl Pts',(-8.53346270707527,22.1374989625693,3.55329989332224));
#92681=CARTESIAN_POINT('Ctrl Pts',(-8.53353908582426,22.1427605146645,3.44461420875881));
#92682=CARTESIAN_POINT('Ctrl Pts',(-8.55567232005459,22.1524191486553,3.24721974889649));
#92683=CARTESIAN_POINT('Ctrl Pts',(-8.57400707557569,22.1568058832743,3.15864926168474));
#92684=CARTESIAN_POINT('Ctrl Pts',(-8.60298181120139,22.1620708250013,3.06382129929687));
#92685=CARTESIAN_POINT('Ctrl Pts',(-8.60566384414128,22.1625479531297,3.05532218923868));
#92686=CARTESIAN_POINT('Ctrl Pts',(-8.60961632516433,22.1632375750851,3.04318457430629));
#92687=CARTESIAN_POINT('Ctrl Pts',(-8.61082383328572,22.1634465445029,3.0395255994677));
#92688=CARTESIAN_POINT('Ctrl Pts',(-8.61294220659321,22.1638102782918,3.03319070499079));
#92689=CARTESIAN_POINT('Ctrl Pts',(-8.61384640921342,22.1639646547203,3.0305125530506));
#92690=CARTESIAN_POINT('Ctrl Pts',(-8.61562919322852,22.1642673535614,3.02528218388922));
#92691=CARTESIAN_POINT('Ctrl Pts',(-8.61650707765149,22.1644156294216,3.02272977346037));
#92692=CARTESIAN_POINT('Ctrl Pts',(-8.61893326590075,22.164823265413,3.01573868085732));
#92693=CARTESIAN_POINT('Ctrl Pts',(-8.62049588907889,22.1650834491609,3.01130504815456));
#92694=CARTESIAN_POINT('Ctrl Pts',(-8.62664020650202,22.1660972600922,2.99413607666613));
#92695=CARTESIAN_POINT('Ctrl Pts',(-8.63137697641954,22.1668593317833,2.98145740412045));
#92696=CARTESIAN_POINT('Ctrl Pts',(-8.67507478130511,22.1737111459457,2.86926532623544));
#92697=CARTESIAN_POINT('Ctrl Pts',(-8.72464921269192,22.180252375855,2.7742372276203));
#92698=CARTESIAN_POINT('Ctrl Pts',(-8.83632298131635,22.1922710396534,2.60754051578375));
#92699=CARTESIAN_POINT('Ctrl Pts',(-8.89589738625106,22.197754551217,2.5348105436654));
#92700=CARTESIAN_POINT('Ctrl Pts',(-8.97024122864046,22.2035962071607,2.46001698198819));
#92701=CARTESIAN_POINT('Ctrl Pts',(-8.97854747885132,22.2042368512649,2.45185756550034));
#92702=CARTESIAN_POINT('Ctrl Pts',(-8.99134059085267,22.2052056625035,2.43958713164148));
#92703=CARTESIAN_POINT('Ctrl Pts',(-8.99575705178449,22.2055369466724,2.43540366449849));
#92704=CARTESIAN_POINT('Ctrl Pts',(-9.00348167530305,22.2061109446072,2.42817740343023));
#92705=CARTESIAN_POINT('Ctrl Pts',(-9.00677798641658,22.2063541891962,2.42512210817563));
#92706=CARTESIAN_POINT('Ctrl Pts',(-9.01420496614086,22.2068984856945,2.41830150221231));
#92707=CARTESIAN_POINT('Ctrl Pts',(-9.01834324826844,22.207199183005,2.41454456016516));
#92708=CARTESIAN_POINT('Ctrl Pts',(-9.02946012790565,22.2080001657881,2.40456766873976));
#92709=CARTESIAN_POINT('Ctrl Pts',(-9.0364770316985,22.2084986633406,2.39839066330193));
#92710=CARTESIAN_POINT('Ctrl Pts',(-9.06786861568483,22.2106982945188,2.37128595532881));
#92711=CARTESIAN_POINT('Ctrl Pts',(-9.09287021598116,22.2123693907942,2.35109614574636));
#92712=CARTESIAN_POINT('Ctrl Pts',(-9.13567363722489,22.2151126605051,2.31879972305439));
#92713=CARTESIAN_POINT('Ctrl Pts',(-9.15311334903888,22.2161996834704,2.30623402429931));
#92714=CARTESIAN_POINT('Ctrl Pts',(-9.28048285998501,22.2239450539178,2.21865798166779));
#92715=CARTESIAN_POINT('Ctrl Pts',(-9.39989846183862,22.2301283419472,2.15857761733415));
#92716=CARTESIAN_POINT('Ctrl Pts',(-9.55356135362848,22.2384134733811,2.1059456678371));
#92717=CARTESIAN_POINT('Ctrl Pts',(-9.58162668197631,22.2399418352708,2.09726749483232));
#92718=CARTESIAN_POINT('Ctrl Pts',(-9.61560074068774,22.2418305572055,2.08787250916541));
#92719=CARTESIAN_POINT('Ctrl Pts',(-9.62127869605408,22.2421474919794,2.086339145158));
#92720=CARTESIAN_POINT('Ctrl Pts',(-9.63011648693593,22.2426430061294,2.0840095147169));
#92721=CARTESIAN_POINT('Ctrl Pts',(-9.63327006507881,22.2428202541525,2.08318948971373));
#92722=CARTESIAN_POINT('Ctrl Pts',(-9.63912751994568,22.2431503238564,2.08168724199177));
#92723=CARTESIAN_POINT('Ctrl Pts',(-9.641830622287,22.2433029834021,2.08100221181624));
#92724=CARTESIAN_POINT('Ctrl Pts',(-9.64797307959817,22.243650645303,2.07946423702906));
#92725=CARTESIAN_POINT('Ctrl Pts',(-9.65141356980905,22.2438459142127,2.07861605936026));
#92726=CARTESIAN_POINT('Ctrl Pts',(-9.66190446529486,22.2444429011342,2.07607013860111));
#92727=CARTESIAN_POINT('Ctrl Pts',(-9.66896432947109,22.2448467929309,2.07441232427301));
#92728=CARTESIAN_POINT('Ctrl Pts',(-9.73795198291566,22.2488124938283,2.05875255543484));
#92729=CARTESIAN_POINT('Ctrl Pts',(-9.8007108636651,22.2525662347383,2.04874346243632));
#92730=CARTESIAN_POINT('Ctrl Pts',(-9.97833562145495,22.2632567738457,2.03215482531083));
#92731=CARTESIAN_POINT('Ctrl Pts',(-10.0936368131551,22.2702377785958,2.03498204341848));
#92732=CARTESIAN_POINT('Ctrl Pts',(-10.2425185400727,22.2788530377613,2.05629857679318));
#92733=CARTESIAN_POINT('Ctrl Pts',(-10.2774196446066,22.2808472449842,2.06259689452283));
#92734=CARTESIAN_POINT('Ctrl Pts',(-10.3211205628221,22.2833131071254,2.07213451551405));
#92735=CARTESIAN_POINT('Ctrl Pts',(-10.3301624534263,22.2838216298429,2.07419811419579));
#92736=CARTESIAN_POINT('Ctrl Pts',(-10.3446053664413,22.2846313462907,2.07763912880652));
#92737=CARTESIAN_POINT('Ctrl Pts',(-10.3500190957812,22.2849342784268,2.0789616682617));
#92738=CARTESIAN_POINT('Ctrl Pts',(-10.3602724792542,22.2855069592888,2.08152865394662));
#92739=CARTESIAN_POINT('Ctrl Pts',(-10.3651135606679,22.2857768975296,2.08276702424921));
#92740=CARTESIAN_POINT('Ctrl Pts',(-10.3760965938596,22.2863883258784,2.08563654434856));
#92741=CARTESIAN_POINT('Ctrl Pts',(-10.3822344778311,22.2867293214878,2.08728295887278));
#92742=CARTESIAN_POINT('Ctrl Pts',(-10.3980910677557,22.2876085329456,2.09164720785049));
#92743=CARTESIAN_POINT('Ctrl Pts',(-10.4077928232807,22.2881447967354,2.0944257026218));
#92744=CARTESIAN_POINT('Ctrl Pts',(-10.4725317784981,22.2917132561691,2.11369307768479));
#92745=CARTESIAN_POINT('Ctrl Pts',(-10.5265885218191,22.2946415962917,2.13331105761356));
#92746=CARTESIAN_POINT('Ctrl Pts',(-10.695529752119,22.3038047992147,2.20613950238704));
#92747=CARTESIAN_POINT('Ctrl Pts',(-10.8047054756562,22.3097066588664,2.27106549942956));
#92748=CARTESIAN_POINT('Ctrl Pts',(-10.9268237923954,22.3176351491507,2.367012671397));
#92749=CARTESIAN_POINT('Ctrl Pts',(-10.948950613736,22.3191355986231,2.38547986030676));
#92750=CARTESIAN_POINT('Ctrl Pts',(-10.9748949681556,22.3209930779516,2.40846609229575));
#92751=CARTESIAN_POINT('Ctrl Pts',(-10.9792501329606,22.3213083370287,2.41237154993949));
#92752=CARTESIAN_POINT('Ctrl Pts',(-10.9859894587572,22.3218017922268,2.41848827550402));
#92753=CARTESIAN_POINT('Ctrl Pts',(-10.9883899113329,22.3219786747619,2.42068160130729));
#92754=CARTESIAN_POINT('Ctrl Pts',(-10.9928359407773,22.3223084222953,2.42477126842293));
#92755=CARTESIAN_POINT('Ctrl Pts',(-10.9948834164606,22.3224611279589,2.42666546791513));
#92756=CARTESIAN_POINT('Ctrl Pts',(-10.9995266119369,22.3228093620652,2.4309857691967));
#92757=CARTESIAN_POINT('Ctrl Pts',(-11.0021189092997,22.3230051606963,2.43341546762361));
#92758=CARTESIAN_POINT('Ctrl Pts',(-11.0088310265022,22.3235156666897,2.43975264611415));
#92759=CARTESIAN_POINT('Ctrl Pts',(-11.0129369589023,22.3238314387093,2.44367466819873));
#92760=CARTESIAN_POINT('Ctrl Pts',(-11.0393808730648,22.3258872102307,2.4692300735727));
#92761=CARTESIAN_POINT('Ctrl Pts',(-11.0610458807732,22.3276741242561,2.49154543925271));
#92762=CARTESIAN_POINT('Ctrl Pts',(-11.0900548349518,22.330192460721,2.52339545628815));
#92763=CARTESIAN_POINT('Ctrl Pts',(-11.0980181964138,22.3308977523125,2.53235750035761));
#92764=CARTESIAN_POINT('Ctrl Pts',(-11.1696780201647,22.3373663805239,2.61502786914373));
#92765=CARTESIAN_POINT('Ctrl Pts',(-11.2259770888658,22.3433222520924,2.69482685579464));
#92766=CARTESIAN_POINT('Ctrl Pts',(-11.3058725866744,22.3529291419746,2.83611748346024));
#92767=CARTESIAN_POINT('Ctrl Pts',(-11.3340244891197,22.3566801773988,2.89467066488936));
#92768=CARTESIAN_POINT('Ctrl Pts',(-11.3639230564336,22.3611559624163,2.96916826968876));
#92769=CARTESIAN_POINT('Ctrl Pts',(-11.3694222003879,22.3620054171893,2.98352028870059));
#92770=CARTESIAN_POINT('Ctrl Pts',(-11.3770272454513,22.3632199489929,3.00434441316852));
#92771=CARTESIAN_POINT('Ctrl Pts',(-11.379315551355,22.3635910271429,3.0107484211073));
#92772=CARTESIAN_POINT('Ctrl Pts',(-11.3832283571807,22.3642356159443,3.02194439661502));
#92773=CARTESIAN_POINT('Ctrl Pts',(-11.3848727853526,22.3645097782961,3.02672923466602));
#92774=CARTESIAN_POINT('Ctrl Pts',(-11.388210587683,22.3650731223719,3.0366076983308));
#92775=CARTESIAN_POINT('Ctrl Pts',(-11.3899008200342,22.3653621978181,3.04170231014588));
#92776=CARTESIAN_POINT('Ctrl Pts',(-11.3941462061364,22.3660982067782,3.05473806132351));
#92777=CARTESIAN_POINT('Ctrl Pts',(-11.3966615808529,22.366543840011,3.06269201861919));
#92778=CARTESIAN_POINT('Ctrl Pts',(-11.4060733515762,22.3682493685352,3.09336307494882));
#92779=CARTESIAN_POINT('Ctrl Pts',(-11.4124848137888,22.369493601722,3.11622585638976));
#92780=CARTESIAN_POINT('Ctrl Pts',(-11.4483292668002,22.3770163013476,3.25714747176875));
#92781=CARTESIAN_POINT('Ctrl Pts',(-11.4634999999934,22.3828111295509,3.3783324018081));
#92782=CARTESIAN_POINT('Ctrl Pts',(-11.4635,22.3887666433152,3.49999999992021));
#92783=CARTESIAN_POINT('Origin',(-10.,13.2,3.5));
#92784=CARTESIAN_POINT('',(-11.4635,22.9615280277103,3.50000000002193));
#92785=CARTESIAN_POINT('',(-11.4635,22.8886966621701,3.49999999996283));
#92786=CARTESIAN_POINT('',(-11.4635,13.2,3.5));
#92787=CARTESIAN_POINT('',(-11.4634996241254,22.9614759749743,3.49895110311648));
#92788=CARTESIAN_POINT('Ctrl Pts',(-11.4635,22.9615280277103,3.50000000002193));
#92789=CARTESIAN_POINT('Ctrl Pts',(-11.4635,22.9615106796706,3.49965037019642));
#92790=CARTESIAN_POINT('Ctrl Pts',(-11.4634998747103,22.9614933287665,3.49930073787219));
#92791=CARTESIAN_POINT('Ctrl Pts',(-11.4634996241254,22.9614759749743,3.49895110311631));
#92792=CARTESIAN_POINT('Ctrl Pts',(-11.4634996227294,22.9614758783865,3.49894915711806));
#92793=CARTESIAN_POINT('Ctrl Pts',(-11.4634732452863,22.9596525387403,3.46221352449691));
#92794=CARTESIAN_POINT('Ctrl Pts',(-11.4620637099453,22.9577996109202,3.42549345045632));
#92795=CARTESIAN_POINT('Ctrl Pts',(-11.4581077419284,22.9550890724053,3.37354803891934));
#92796=CARTESIAN_POINT('Ctrl Pts',(-11.4566999901143,22.9542796794849,3.35824885081634));
#92797=CARTESIAN_POINT('Ctrl Pts',(-11.4545582938092,22.9532121376693,3.3384030684732));
#92798=CARTESIAN_POINT('Ctrl Pts',(-11.4540433356523,22.9529651037365,3.33383329060898));
#92799=CARTESIAN_POINT('Ctrl Pts',(-11.453141352384,22.9525478402738,3.32615444841089));
#92800=CARTESIAN_POINT('Ctrl Pts',(-11.4527658623536,22.9523782257767,3.32304403194678));
#92801=CARTESIAN_POINT('Ctrl Pts',(-11.4520582732807,22.9520658655692,3.31733671638442));
#92802=CARTESIAN_POINT('Ctrl Pts',(-11.4517291868762,22.95192328611,3.31473944852019));
#92803=CARTESIAN_POINT('Ctrl Pts',(-11.4510334839562,22.9516272991256,3.30936440807431));
#92804=CARTESIAN_POINT('Ctrl Pts',(-11.4506658617093,22.9514738333081,3.3065868213375));
#92805=CARTESIAN_POINT('Ctrl Pts',(-11.4498047599134,22.9511209672799,3.30022131027363));
#92806=CARTESIAN_POINT('Ctrl Pts',(-11.4493059364927,22.9509212721497,3.29663415084392));
#92807=CARTESIAN_POINT('Ctrl Pts',(-11.447939669845,22.9503866213018,3.28706938481767));
#92808=CARTESIAN_POINT('Ctrl Pts',(-11.447048535404,22.9500504020038,3.28109529924195));
#92809=CARTESIAN_POINT('Ctrl Pts',(-11.4401422078661,22.9475347194591,3.23668186635204));
#92810=CARTESIAN_POINT('Ctrl Pts',(-11.4326337019908,22.9452820229483,3.1984934683087));
#92811=CARTESIAN_POINT('Ctrl Pts',(-11.4178662325746,22.9415278490329,3.13654162919375));
#92812=CARTESIAN_POINT('Ctrl Pts',(-11.4115073323534,22.9400508489001,3.11258081753115));
#92813=CARTESIAN_POINT('Ctrl Pts',(-11.3850662966905,22.9344131355215,3.02226706459585));
#92814=CARTESIAN_POINT('Ctrl Pts',(-11.3608865634778,22.9302103812058,2.95720567509524));
#92815=CARTESIAN_POINT('Ctrl Pts',(-11.3105661700983,22.9229866428742,2.84656620096894));
#92816=CARTESIAN_POINT('Ctrl Pts',(-11.2864155588632,22.9199336403855,2.80021771283935));
#92817=CARTESIAN_POINT('Ctrl Pts',(-11.2444023432422,22.9152330577863,2.72914658989345));
#92818=CARTESIAN_POINT('Ctrl Pts',(-11.2281593016871,22.9135336143108,2.70352206951157));
#92819=CARTESIAN_POINT('Ctrl Pts',(-11.2061909941863,22.9113786000927,2.67113754909324));
#92820=CARTESIAN_POINT('Ctrl Pts',(-11.2011856138087,22.9108964959853,2.66390024344747));
#92821=CARTESIAN_POINT('Ctrl Pts',(-11.1929651611424,22.9101188686488,2.65224044703891));
#92822=CARTESIAN_POINT('Ctrl Pts',(-11.1897900964486,22.9098218415531,2.64779012980379));
#92823=CARTESIAN_POINT('Ctrl Pts',(-11.1836514842201,22.9092538621523,2.63928714501705));
#92824=CARTESIAN_POINT('Ctrl Pts',(-11.1806918777961,22.9089827650489,2.6352317389013));
#92825=CARTESIAN_POINT('Ctrl Pts',(-11.173885989987,22.9083655306467,2.62600603163217));
#92826=CARTESIAN_POINT('Ctrl Pts',(-11.1700262960853,22.9080199165649,2.62084572314555));
#92827=CARTESIAN_POINT('Ctrl Pts',(-11.1597125685023,22.9071078886038,2.6072447688895));
#92828=CARTESIAN_POINT('Ctrl Pts',(-11.1532004181785,22.9065437398669,2.5988485434561));
#92829=CARTESIAN_POINT('Ctrl Pts',(-11.0987936786368,22.9019237642244,2.53025672947721));
#92830=CARTESIAN_POINT('Ctrl Pts',(-11.0463106533937,22.8980613861498,2.47384916700088));
#92831=CARTESIAN_POINT('Ctrl Pts',(-10.939578223559,22.8909457544782,2.37588217397486));
#92832=CARTESIAN_POINT('Ctrl Pts',(-10.8863884780223,22.8876805205979,2.33348235656279));
#92833=CARTESIAN_POINT('Ctrl Pts',(-10.7933382059773,22.8821303986175,2.26935882031832));
#92834=CARTESIAN_POINT('Ctrl Pts',(-10.7550707615303,22.8798873171283,2.24551570384066));
#92835=CARTESIAN_POINT('Ctrl Pts',(-10.7027153707901,22.8767907665733,2.21615917451802));
#92836=CARTESIAN_POINT('Ctrl Pts',(-10.6895525526661,22.8760099747101,2.20904167230537));
#92837=CARTESIAN_POINT('Ctrl Pts',(-10.6700477227002,22.8748463254496,2.19887827618754));
#92838=CARTESIAN_POINT('Ctrl Pts',(-10.6637888450575,22.8744719303134,2.1956740988806));
#92839=CARTESIAN_POINT('Ctrl Pts',(-10.6524777643006,22.8737931111861,2.18998598875085));
#92840=CARTESIAN_POINT('Ctrl Pts',(-10.6474338192235,22.8734896216981,2.18748585141701));
#92841=CARTESIAN_POINT('Ctrl Pts',(-10.6395090463834,22.8730113792248,2.18361456706637));
#92842=CARTESIAN_POINT('Ctrl Pts',(-10.6366378915162,22.8728378218714,2.18222360655009));
#92843=CARTESIAN_POINT('Ctrl Pts',(-10.6337541194724,22.8726631896323,2.18083815771796));
#92844=CARTESIAN_POINT('Ctrl Pts',(-10.6337459992963,22.8726626978972,2.18083425663901));
#92845=CARTESIAN_POINT('Ctrl Pts',(-10.6337297220678,22.8726617121891,2.18082643695011));
#92846=CARTESIAN_POINT('Ctrl Pts',(-10.6337215651112,22.8726612182218,2.18082251838698));
#92847=CARTESIAN_POINT('Ctrl Pts',(-10.633705214225,22.8726602280431,2.18081466368569));
#92848=CARTESIAN_POINT('Ctrl Pts',(-10.6336970201241,22.8726597318214,2.18081072746609));
#92849=CARTESIAN_POINT('Ctrl Pts',(-10.633680594533,22.8726587371086,2.18080283725454));
#92850=CARTESIAN_POINT('Ctrl Pts',(-10.6336723632717,22.8726582386314,2.18079888337332));
#92851=CARTESIAN_POINT('Ctrl Pts',(-10.6336558631569,22.8726572393953,2.18079095774359));
#92852=CARTESIAN_POINT('Ctrl Pts',(-10.6336475942764,22.8726567386348,2.18078698598296));
#92853=CARTESIAN_POINT('Ctrl Pts',(-10.6336310188618,22.8726557348283,2.1807790245675));
#92854=CARTESIAN_POINT('Ctrl Pts',(-10.633622712158,22.8726552317721,2.18077503483202));
#92855=CARTESIAN_POINT('Ctrl Pts',(-10.6336060607994,22.872654223356,2.18076703732665));
#92856=CARTESIAN_POINT('Ctrl Pts',(-10.6335977161272,22.8726537179952,2.18076302954923));
#92857=CARTESIAN_POINT('Ctrl Pts',(-10.6335809884122,22.8726527049444,2.18075499576115));
#92858=CARTESIAN_POINT('Ctrl Pts',(-10.6335726055373,22.8726521972647,2.180750969832));
#92859=CARTESIAN_POINT('Ctrl Pts',(-10.6310480371142,22.8724993047404,2.17953855935238));
#92860=CARTESIAN_POINT('Ctrl Pts',(-10.6285284620908,22.8723464723902,2.17833740564742));
#92861=CARTESIAN_POINT('Ctrl Pts',(-10.6227644868692,22.8719962972652,2.17560976289968));
#92862=CARTESIAN_POINT('Ctrl Pts',(-10.6195179130081,22.8717986715108,2.1740879889186));
#92863=CARTESIAN_POINT('Ctrl Pts',(-10.6110157468355,22.8712801770037,2.17014079272056));
#92864=CARTESIAN_POINT('Ctrl Pts',(-10.6057513522915,22.8709581889716,2.16773461690217));
#92865=CARTESIAN_POINT('Ctrl Pts',(-10.5701233442704,22.8687733939266,2.15170508824438));
#92866=CARTESIAN_POINT('Ctrl Pts',(-10.539319037039,22.866856876712,2.13909058391791));
#92867=CARTESIAN_POINT('Ctrl Pts',(-10.490951763895,22.8638343877516,2.12118401036187));
#92868=CARTESIAN_POINT('Ctrl Pts',(-10.4736721816777,22.8627519898839,2.11515278938161));
#92869=CARTESIAN_POINT('Ctrl Pts',(-10.3712266359488,22.8563360105673,2.08153714905513));
#92870=CARTESIAN_POINT('Ctrl Pts',(-10.2837862196306,22.8508796704172,2.06148943069912));
#92871=CARTESIAN_POINT('Ctrl Pts',(-10.1249924508596,22.8414016889792,2.0401345461916));
#92872=CARTESIAN_POINT('Ctrl Pts',(-10.0543292150462,22.8373288740529,2.03580025987142));
#92873=CARTESIAN_POINT('Ctrl Pts',(-9.97248175545239,22.8327991070005,2.03671633227608));
#92874=CARTESIAN_POINT('Ctrl Pts',(-9.96134419308052,22.8321865598913,2.03696818754709));
#92875=CARTESIAN_POINT('Ctrl Pts',(-9.94423725542512,22.8312514399127,2.03755051856193));
#92876=CARTESIAN_POINT('Ctrl Pts',(-9.93826538179682,22.8309260714968,2.03779043641578));
#92877=CARTESIAN_POINT('Ctrl Pts',(-9.92737938139554,22.8303348767917,2.03829458792155));
#92878=CARTESIAN_POINT('Ctrl Pts',(-9.92246481877847,22.8300686888562,2.03854703721307));
#92879=CARTESIAN_POINT('Ctrl Pts',(-9.91173580259414,22.8294890904623,2.03915243354299));
#92880=CARTESIAN_POINT('Ctrl Pts',(-9.90592197901186,22.8291759931195,2.03951531734213));
#92881=CARTESIAN_POINT('Ctrl Pts',(-9.88998290910093,22.8283202026221,2.04060576395182));
#92882=CARTESIAN_POINT('Ctrl Pts',(-9.87986271825187,22.8277797080709,2.04140398431158));
#92883=CARTESIAN_POINT('Ctrl Pts',(-9.82731287488445,22.8249871155621,2.04609944596996));
#92884=CARTESIAN_POINT('Ctrl Pts',(-9.78505800028072,22.8227898373998,2.05174310309314));
#92885=CARTESIAN_POINT('Ctrl Pts',(-9.60357328982192,22.8134731653276,2.08410216307224));
#92886=CARTESIAN_POINT('Ctrl Pts',(-9.46841375493798,22.8069204477127,2.12911363783852));
#92887=CARTESIAN_POINT('Ctrl Pts',(-9.31503733309478,22.7981697349257,2.20633884689591));
#92888=CARTESIAN_POINT('Ctrl Pts',(-9.28865381232147,22.7966091742222,2.22065665692394));
#92889=CARTESIAN_POINT('Ctrl Pts',(-9.25762089799422,22.79468449035,2.23875438063674));
#92890=CARTESIAN_POINT('Ctrl Pts',(-9.2525290487486,22.794365744567,2.24176535650229));
#92891=CARTESIAN_POINT('Ctrl Pts',(-9.24465523892611,22.7938680426169,2.24648605775432));
#92892=CARTESIAN_POINT('Ctrl Pts',(-9.24186045141881,22.7936904373678,2.24817439875327));
#92893=CARTESIAN_POINT('Ctrl Pts',(-9.23669081958393,22.7933601102193,2.25132105340545));
#92894=CARTESIAN_POINT('Ctrl Pts',(-9.23431447778206,22.7932075535382,2.25277680535463));
#92895=CARTESIAN_POINT('Ctrl Pts',(-9.22893613498647,22.7928606577584,2.25609275334152));
#92896=CARTESIAN_POINT('Ctrl Pts',(-9.22593671453192,22.7926660564008,2.25795702499085));
#92897=CARTESIAN_POINT('Ctrl Pts',(-9.21819044690254,22.7921605777362,2.26281062828502));
#92898=CARTESIAN_POINT('Ctrl Pts',(-9.21345403206892,22.7918486687422,2.26581640058524));
#92899=CARTESIAN_POINT('Ctrl Pts',(-9.18361006114819,22.789865931455,2.2849972258552));
#92900=CARTESIAN_POINT('Ctrl Pts',(-9.1589869212381,22.788151817656,2.3019094252259));
#92901=CARTESIAN_POINT('Ctrl Pts',(-9.05050753570982,22.7803015469432,2.38140997779612));
#92902=CARTESIAN_POINT('Ctrl Pts',(-8.97299146723634,22.7738853242976,2.45212898819746));
#92903=CARTESIAN_POINT('Ctrl Pts',(-8.86936332633942,22.7645914861725,2.56931411253569));
#92904=CARTESIAN_POINT('Ctrl Pts',(-8.83713057946245,22.761564342947,2.60991515808132));
#92905=CARTESIAN_POINT('Ctrl Pts',(-8.78964159187339,22.7568982410933,2.67672931779638));
#92906=CARTESIAN_POINT('Ctrl Pts',(-8.77293022254313,22.7552083562166,2.70185086433013));
#92907=CARTESIAN_POINT('Ctrl Pts',(-8.75237036170699,22.7530635250058,2.7349315926207));
#92908=CARTESIAN_POINT('Ctrl Pts',(-8.74780157353129,22.7525823531225,2.7424325193172));
#92909=CARTESIAN_POINT('Ctrl Pts',(-8.74050076516666,22.7518058559297,2.75466532860033));
#92910=CARTESIAN_POINT('Ctrl Pts',(-8.73772728104875,22.7515090348037,2.75937210486224));
#92911=CARTESIAN_POINT('Ctrl Pts',(-8.73245515423332,22.7509412038779,2.76843487645601));
#92912=CARTESIAN_POINT('Ctrl Pts',(-8.72995245301274,22.7506700509194,2.77278841093122));
#92913=CARTESIAN_POINT('Ctrl Pts',(-8.72428563435984,22.7500523529439,2.78276452218088));
#92914=CARTESIAN_POINT('Ctrl Pts',(-8.72113617735537,22.7497063339397,2.78839533567326));
#92915=CARTESIAN_POINT('Ctrl Pts',(-8.71288610292295,22.7487925203549,2.80337706255747));
#92916=CARTESIAN_POINT('Ctrl Pts',(-8.7078501070075,22.7482270053733,2.81276324092941));
#92917=CARTESIAN_POINT('Ctrl Pts',(-8.66665355199016,22.7435332994342,2.89160013638136));
#92918=CARTESIAN_POINT('Ctrl Pts',(-8.63601583884849,22.7396060759652,2.96379818617022));
#92919=CARTESIAN_POINT('Ctrl Pts',(-8.59039816304495,22.7325125468467,3.10095008341315));
#92920=CARTESIAN_POINT('Ctrl Pts',(-8.57378661896455,22.7293279832478,3.16513674912525));
#92921=CARTESIAN_POINT('Ctrl Pts',(-8.55323254667196,22.7238525722675,3.27473036813422));
#92922=CARTESIAN_POINT('Ctrl Pts',(-8.54695636824686,22.7215994634492,3.31959447999967));
#92923=CARTESIAN_POINT('Ctrl Pts',(-8.54068423888189,22.7181005954297,3.38713465360805));
#92924=CARTESIAN_POINT('Ctrl Pts',(-8.53911811063888,22.7169170246536,3.4096392169471));
#92925=CARTESIAN_POINT('Ctrl Pts',(-8.53782097584902,22.715415061166,3.43759599882887));
#92926=CARTESIAN_POINT('Ctrl Pts',(-8.53759942493791,22.7151219897871,3.44302356436409));
#92927=CARTESIAN_POINT('Ctrl Pts',(-8.5372968229345,22.7146558688001,3.4516094364999));
#92928=CARTESIAN_POINT('Ctrl Pts',(-8.5371957717898,22.7144839075952,3.45476704325511));
#92929=CARTESIAN_POINT('Ctrl Pts',(-8.53702435003934,22.7141582699073,3.46072715173168));
#92930=CARTESIAN_POINT('Ctrl Pts',(-8.53695180727693,22.7140047142547,3.46352954220039));
#92931=CARTESIAN_POINT('Ctrl Pts',(-8.5368037273368,22.7136510993821,3.46996468298871));
#92932=CARTESIAN_POINT('Ctrl Pts',(-8.53673366710158,22.7134507408156,3.47359751861213));
#92933=CARTESIAN_POINT('Ctrl Pts',(-8.53658253141766,22.7129131589034,3.48331054085524));
#92934=CARTESIAN_POINT('Ctrl Pts',(-8.53652582146499,22.7125746505804,3.48939096868958));
#92935=CARTESIAN_POINT('Ctrl Pts',(-8.53638325076678,22.7099955052644,3.53546573631324));
#92936=CARTESIAN_POINT('Ctrl Pts',(-8.53789900869216,22.7076775240428,3.57544504617879));
#92937=CARTESIAN_POINT('Ctrl Pts',(-8.54849305359739,22.6997433998366,3.70948718960912));
#92938=CARTESIAN_POINT('Ctrl Pts',(-8.56503787126248,22.6939704175269,3.80272389431009));
#92939=CARTESIAN_POINT('Ctrl Pts',(-8.60423299226438,22.6853189730104,3.94304614335));
#92940=CARTESIAN_POINT('Ctrl Pts',(-8.62059246009301,22.682327538178,3.99162083570523));
#92941=CARTESIAN_POINT('Ctrl Pts',(-8.65049543517712,22.6777091455558,4.06706754963956));
#92942=CARTESIAN_POINT('Ctrl Pts',(-8.66237576933256,22.6760325416527,4.09455006417245));
#92943=CARTESIAN_POINT('Ctrl Pts',(-8.67881187770535,22.6739018708786,4.12957995242003));
#92944=CARTESIAN_POINT('Ctrl Pts',(-8.68260362463712,22.6734220032802,4.13747609041152));
#92945=CARTESIAN_POINT('Ctrl Pts',(-8.68887277207805,22.6726470872648,4.15023644212917));
#92946=CARTESIAN_POINT('Ctrl Pts',(-8.69130685921244,22.6723505542669,4.15512159394418));
#92947=CARTESIAN_POINT('Ctrl Pts',(-8.69603352162394,22.6717829295593,4.16447641434488));
#92948=CARTESIAN_POINT('Ctrl Pts',(-8.69832188873457,22.6715116969924,4.16894811268964));
#92949=CARTESIAN_POINT('Ctrl Pts',(-8.7036068643279,22.6708933435004,4.1791456775413));
#92950=CARTESIAN_POINT('Ctrl Pts',(-8.70661847914049,22.6705467525397,4.18486367757874));
#92951=CARTESIAN_POINT('Ctrl Pts',(-8.71471126413086,22.66963041481,4.19998525419879));
#92952=CARTESIAN_POINT('Ctrl Pts',(-8.71985779380491,22.6690629681527,4.20935353005815));
#92953=CARTESIAN_POINT('Ctrl Pts',(-8.77191907131174,22.6634691476678,4.30170894273364));
#92954=CARTESIAN_POINT('Ctrl Pts',(-8.82673462887108,22.658751251724,4.37998369660948));
#92955=CARTESIAN_POINT('Ctrl Pts',(-8.94276960040558,22.6500618603562,4.51537139454248));
#92956=CARTESIAN_POINT('Ctrl Pts',(-9.0020133400753,22.6460821487852,4.57365544564109));
#92957=CARTESIAN_POINT('Ctrl Pts',(-9.09121922817761,22.6402021306045,4.64762105758992));
#92958=CARTESIAN_POINT('Ctrl Pts',(-9.11726849491881,22.6384957524693,4.66777624396315));
#92959=CARTESIAN_POINT('Ctrl Pts',(-9.14889274793297,22.6364079045773,4.69058199347438));
#92960=CARTESIAN_POINT('Ctrl Pts',(-9.15383417936643,22.636081211939,4.69409900725277));
#92961=CARTESIAN_POINT('Ctrl Pts',(-9.16149559774753,22.6355737545293,4.69948050877862));
#92962=CARTESIAN_POINT('Ctrl Pts',(-9.16420032366015,22.6353944269104,4.70136673173851));
#92963=CARTESIAN_POINT('Ctrl Pts',(-9.16920047831088,22.6350625341961,4.70482868354144));
#92964=CARTESIAN_POINT('Ctrl Pts',(-9.17149404215828,22.6349101473326,4.7064070123273));
#92965=CARTESIAN_POINT('Ctrl Pts',(-9.17667281855228,22.6345657336821,4.70994908275563));
#92966=CARTESIAN_POINT('Ctrl Pts',(-9.17956054240587,22.6343734606614,4.71190904216155));
#92967=CARTESIAN_POINT('Ctrl Pts',(-9.18699497091596,22.6338779358729,4.71691619709011));
#92968=CARTESIAN_POINT('Ctrl Pts',(-9.19155176818449,22.6335737172127,4.71994822128145));
#92969=CARTESIAN_POINT('Ctrl Pts',(-9.21913457863256,22.6317297943003,4.73807900192011));
#92970=CARTESIAN_POINT('Ctrl Pts',(-9.24256455991984,22.6301533034055,4.75255010906952));
#92971=CARTESIAN_POINT('Ctrl Pts',(-9.35847478967007,22.6223572920333,4.81969836048252));
#92972=CARTESIAN_POINT('Ctrl Pts',(-9.45610518015055,22.6158270129194,4.86284161023424));
#92973=CARTESIAN_POINT('Ctrl Pts',(-9.62506051372539,22.6052915413896,4.91642809731541));
#92974=CARTESIAN_POINT('Ctrl Pts',(-9.694041148166,22.6011795437054,4.93291296673286));
#92975=CARTESIAN_POINT('Ctrl Pts',(-9.77982123375063,22.5963276866793,4.94693196239669));
#92976=CARTESIAN_POINT('Ctrl Pts',(-9.79573206100958,22.5954382363144,4.94926375481091));
#92977=CARTESIAN_POINT('Ctrl Pts',(-9.81854446093554,22.5941775312039,4.95222383668252));
#92978=CARTESIAN_POINT('Ctrl Pts',(-9.82541669103518,22.5937996235824,4.95306601881147));
#92979=CARTESIAN_POINT('Ctrl Pts',(-9.83734016167326,22.593147138594,4.95444141242383));
#92980=CARTESIAN_POINT('Ctrl Pts',(-9.84238863938118,22.5928718622089,4.95499714951122));
#92981=CARTESIAN_POINT('Ctrl Pts',(-9.85210384147005,22.5923439960224,4.95601544192326));
#92982=CARTESIAN_POINT('Ctrl Pts',(-9.85677008976282,22.592091288654,4.9564818688694));
#92983=CARTESIAN_POINT('Ctrl Pts',(-9.86778974556372,22.591496423386,4.95752989723281));
#92984=CARTESIAN_POINT('Ctrl Pts',(-9.8741449025253,22.5911548630033,4.95809240067142));
#92985=CARTESIAN_POINT('Ctrl Pts',(-9.8963724763953,22.5899653425686,4.95991338701998));
#92986=CARTESIAN_POINT('Ctrl Pts',(-9.9122618919183,22.5891241248389,4.96095441809888));
#92987=CARTESIAN_POINT('Ctrl Pts',(-10.0523400549234,22.5817811305488,4.96783831305953));
#92988=CARTESIAN_POINT('Ctrl Pts',(-10.1767821266354,22.5758204370791,4.95809436211311));
#92989=CARTESIAN_POINT('Ctrl Pts',(-10.352786077654,22.5670507395725,4.92142495588696));
#92990=CARTESIAN_POINT('Ctrl Pts',(-10.4063800518975,22.5643228853359,4.90703992533168));
#92991=CARTESIAN_POINT('Ctrl Pts',(-10.4832964210507,22.5601658805956,4.88163316941541));
#92992=CARTESIAN_POINT('Ctrl Pts',(-10.5073525058914,22.5588296684193,4.87298176333184));
#92993=CARTESIAN_POINT('Ctrl Pts',(-10.5364301773216,22.5571562520763,4.86165590506921));
#92994=CARTESIAN_POINT('Ctrl Pts',(-10.5416801496039,22.5568517623694,4.85957594579463));
#92995=CARTESIAN_POINT('Ctrl Pts',(-10.5498921626083,22.5563715861309,4.85626735636548));
#92996=CARTESIAN_POINT('Ctrl Pts',(-10.5528624832187,22.5561971017345,4.85505926316343));
#92997=CARTESIAN_POINT('Ctrl Pts',(-10.5584137120274,22.5558694618426,4.85278016852993));
#92998=CARTESIAN_POINT('Ctrl Pts',(-10.5609955360152,22.5557164474096,4.85171153220216));
#92999=CARTESIAN_POINT('Ctrl Pts',(-10.566911733211,22.555364376178,4.84924290427161));
#93000=CARTESIAN_POINT('Ctrl Pts',(-10.5702439808846,22.5551650246104,4.8478379463667));
#93001=CARTESIAN_POINT('Ctrl Pts',(-10.5789906386521,22.55463905706,4.84411189779674));
#93002=CARTESIAN_POINT('Ctrl Pts',(-10.5843962454322,22.5543112700257,4.84177046449532));
#93003=CARTESIAN_POINT('Ctrl Pts',(-10.6221557598251,22.5520031963805,4.82514350701536));
#93004=CARTESIAN_POINT('Ctrl Pts',(-10.6539943130848,22.549962301649,4.80972292829475));
#93005=CARTESIAN_POINT('Ctrl Pts',(-10.7254993130253,22.5452091159894,4.77183287634479));
#93006=CARTESIAN_POINT('Ctrl Pts',(-10.7647384705003,22.5424758684529,4.74863239749089));
#93007=CARTESIAN_POINT('Ctrl Pts',(-10.9060906270905,22.5323002412033,4.65589133514381));
#93008=CARTESIAN_POINT('Ctrl Pts',(-11.0003808480297,22.5248957318843,4.57532969754823));
#93009=CARTESIAN_POINT('Ctrl Pts',(-11.0940584743266,22.5171208528616,4.47217175681321));
#93010=CARTESIAN_POINT('Ctrl Pts',(-11.1044901012918,22.5162471505228,4.46030386526878));
#93011=CARTESIAN_POINT('Ctrl Pts',(-11.1191823929969,22.5150046261628,4.44303249467248));
#93012=CARTESIAN_POINT('Ctrl Pts',(-11.1236000810993,22.5146294114197,4.43776456257167));
#93013=CARTESIAN_POINT('Ctrl Pts',(-11.1312112287079,22.5139800759859,4.42855754616877));
#93014=CARTESIAN_POINT('Ctrl Pts',(-11.1344216149669,22.5137052748293,4.42463266268131));
#93015=CARTESIAN_POINT('Ctrl Pts',(-11.140568990456,22.5131772752128,4.41703692816707));
#93016=CARTESIAN_POINT('Ctrl Pts',(-11.1435088134412,22.5129239653447,4.41336846009926));
#93017=CARTESIAN_POINT('Ctrl Pts',(-11.1504248939997,22.512326082151,4.40465247469064));
#93018=CARTESIAN_POINT('Ctrl Pts',(-11.1543857051605,22.5119821214191,4.39959278688027));
#93019=CARTESIAN_POINT('Ctrl Pts',(-11.1682100304846,22.5107759287708,4.38169142327106));
#93020=CARTESIAN_POINT('Ctrl Pts',(-11.1778938225474,22.5099206952712,4.36871204172841));
#93021=CARTESIAN_POINT('Ctrl Pts',(-11.2583371411775,22.5027194438443,4.2570733205469));
#93022=CARTESIAN_POINT('Ctrl Pts',(-11.3167803750904,22.496885062275,4.15012633511043));
#93023=CARTESIAN_POINT('Ctrl Pts',(-11.3824075122001,22.4881708618385,3.98381162221937));
#93024=CARTESIAN_POINT('Ctrl Pts',(-11.400309287888,22.4853539038468,3.92925193913991));
#93025=CARTESIAN_POINT('Ctrl Pts',(-11.4216235868321,22.4810749154837,3.84856712176743));
#93026=CARTESIAN_POINT('Ctrl Pts',(-11.427609928413,22.4797122288226,3.82317547311844));
#93027=CARTESIAN_POINT('Ctrl Pts',(-11.4340697085064,22.4780091281776,3.79207635968033));
#93028=CARTESIAN_POINT('Ctrl Pts',(-11.4351927488141,22.4777028109347,3.78650706860523));
#93029=CARTESIAN_POINT('Ctrl Pts',(-11.4369003020955,22.4772203864281,3.77777707382073));
#93030=CARTESIAN_POINT('Ctrl Pts',(-11.4375068908089,22.47704549995,3.77462068270932));
#93031=CARTESIAN_POINT('Ctrl Pts',(-11.4386211642336,22.4767175259073,3.76871769088514));
#93032=CARTESIAN_POINT('Ctrl Pts',(-11.4391313865424,22.4765645825659,3.7659716214551));
#93033=CARTESIAN_POINT('Ctrl Pts',(-11.4402820754215,22.4762132330069,3.75967823707123));
#93034=CARTESIAN_POINT('Ctrl Pts',(-11.4409172976905,22.4760145364928,3.75613001431306));
#93035=CARTESIAN_POINT('Ctrl Pts',(-11.4425493561025,22.4754914094448,3.74681541708485));
#93036=CARTESIAN_POINT('Ctrl Pts',(-11.4435247157383,22.4751658276659,3.74104540572246));
#93037=CARTESIAN_POINT('Ctrl Pts',(-11.4500263477957,22.4729036216027,3.70112790356265));
#93038=CARTESIAN_POINT('Ctrl Pts',(-11.4543746179919,22.4709089950979,3.66680210651175));
#93039=CARTESIAN_POINT('Ctrl Pts',(-11.4614622886472,22.4663096565819,3.58875359134485));
#93040=CARTESIAN_POINT('Ctrl Pts',(-11.4634631165743,22.4636863066559,3.5449957527342));
#93041=CARTESIAN_POINT('Ctrl Pts',(-11.4634998316009,22.4610279215406,3.50081071340477));
#93042=CARTESIAN_POINT('Ctrl Pts',(-11.4635,22.4610035323129,3.50040535415972));
#93043=CARTESIAN_POINT('Ctrl Pts',(-11.4635,22.4609791425484,3.50000000009405));
#93044=CARTESIAN_POINT('',(-11.463499731436,22.8886344895975,3.49895700858923));
#93045=CARTESIAN_POINT('Ctrl Pts',(-11.4635,22.3887666433152,3.49999999992021));
#93046=CARTESIAN_POINT('Ctrl Pts',(-11.4635,22.3887864753112,3.50040515578243));
#93047=CARTESIAN_POINT('Ctrl Pts',(-11.4634998317572,22.3888063096356,3.50081031697022));
#93048=CARTESIAN_POINT('Ctrl Pts',(-11.4634414153931,22.3922499147876,3.5711463205363));
#93049=CARTESIAN_POINT('Ctrl Pts',(-11.4583710933305,22.3957287202161,3.64097534271047));
#93050=CARTESIAN_POINT('Ctrl Pts',(-11.4472875942407,22.3998459927665,3.71735608274318));
#93051=CARTESIAN_POINT('Ctrl Pts',(-11.4461906229825,22.4002362853658,3.72453891598871));
#93052=CARTESIAN_POINT('Ctrl Pts',(-11.444478747129,22.4008213923889,3.73521474365312));
#93053=CARTESIAN_POINT('Ctrl Pts',(-11.4439045419782,22.4010139935623,3.73871426361317));
#93054=CARTESIAN_POINT('Ctrl Pts',(-11.4428560750092,22.401359337681,3.74496198547646));
#93055=CARTESIAN_POINT('Ctrl Pts',(-11.4423866719365,22.4015118065534,3.7477109524882));
#93056=CARTESIAN_POINT('Ctrl Pts',(-11.441352114708,22.4018432907535,3.75366697789371));
#93057=CARTESIAN_POINT('Ctrl Pts',(-11.4407841210342,22.4020224593706,3.75687345210515));
#93058=CARTESIAN_POINT('Ctrl Pts',(-11.4391619377477,22.4025263464491,3.76585643968429));
#93059=CARTESIAN_POINT('Ctrl Pts',(-11.4380836895846,22.4028523756356,3.77162847594833));
#93060=CARTESIAN_POINT('Ctrl Pts',(-11.4314354600568,22.4048105108482,3.80606800764421));
#93061=CARTESIAN_POINT('Ctrl Pts',(-11.4250434955166,22.4064841137481,3.83456823090937));
#93062=CARTESIAN_POINT('Ctrl Pts',(-11.3853258268499,22.4158211782022,3.98975885778564));
#93063=CARTESIAN_POINT('Ctrl Pts',(-11.3359576300993,22.4239209942555,4.11173045469656));
#93064=CARTESIAN_POINT('Ctrl Pts',(-11.2643770012013,22.4323484510507,4.23713093768342));
#93065=CARTESIAN_POINT('Ctrl Pts',(-11.2575859048152,22.4331248972202,4.24865808397973));
#93066=CARTESIAN_POINT('Ctrl Pts',(-11.2293459393181,22.4362611205455,4.29512353940633));
#93067=CARTESIAN_POINT('Ctrl Pts',(-11.2065904314168,22.4385785969067,4.32924838239373));
#93068=CARTESIAN_POINT('Ctrl Pts',(-11.176518551953,22.4413972610217,4.37048090032699));
#93069=CARTESIAN_POINT('Ctrl Pts',(-11.1705235596547,22.4419481707111,4.37852575617457));
#93070=CARTESIAN_POINT('Ctrl Pts',(-11.1609334320775,22.4428124716891,4.39112257620886));
#93071=CARTESIAN_POINT('Ctrl Pts',(-11.1573932259788,22.4431279829346,4.39571580389915));
#93072=CARTESIAN_POINT('Ctrl Pts',(-11.1507968221072,22.4437094049003,4.40416987808131));
#93073=CARTESIAN_POINT('Ctrl Pts',(-11.1477482716439,22.4439756099944,4.40803656311885));
#93074=CARTESIAN_POINT('Ctrl Pts',(-11.1409351656734,22.4445650605231,4.41658896131871));
#93075=CARTESIAN_POINT('Ctrl Pts',(-11.1371611295861,22.4448879238874,4.42126703138382));
#93076=CARTESIAN_POINT('Ctrl Pts',(-11.1262122810549,22.4458142340023,4.43466877790436));
#93077=CARTESIAN_POINT('Ctrl Pts',(-11.1189650705888,22.44641477371,4.44333292464552));
#93078=CARTESIAN_POINT('Ctrl Pts',(-11.0621510974471,22.4510286227644,4.50967877619092));
#93079=CARTESIAN_POINT('Ctrl Pts',(-11.0082541199108,22.4548531801478,4.56350446287798));
#93080=CARTESIAN_POINT('Ctrl Pts',(-10.883461342075,22.4629211200718,4.67007675353308));
#93081=CARTESIAN_POINT('Ctrl Pts',(-10.8114919256778,22.4671179684292,4.7210910054779));
#93082=CARTESIAN_POINT('Ctrl Pts',(-10.72629793268,22.4720307904386,4.77060373689243));
#93083=CARTESIAN_POINT('Ctrl Pts',(-10.7171615562358,22.4725571427608,4.77578283379038));
#93084=CARTESIAN_POINT('Ctrl Pts',(-10.6758909548467,22.4749358702569,4.79859429861302));
#93085=CARTESIAN_POINT('Ctrl Pts',(-10.6431591778464,22.476825302443,4.81511276584703));
#93086=CARTESIAN_POINT('Ctrl Pts',(-10.6044353346551,22.4791024017168,4.83286367880385));
#93087=CARTESIAN_POINT('Ctrl Pts',(-10.5990109719022,22.4794223072308,4.8353102685113));
#93088=CARTESIAN_POINT('Ctrl Pts',(-10.5902849268182,22.4799386571361,4.83918217088102));
#93089=CARTESIAN_POINT('Ctrl Pts',(-10.5869925928706,22.480133867515,4.84062853803226));
#93090=CARTESIAN_POINT('Ctrl Pts',(-10.5811277770254,22.4804823587555,4.84317928589764));
#93091=CARTESIAN_POINT('Ctrl Pts',(-10.5785574194492,22.4806353488974,4.84428843616002));
#93092=CARTESIAN_POINT('Ctrl Pts',(-10.5730572266018,22.4809632942659,4.84664315986661));
#93093=CARTESIAN_POINT('Ctrl Pts',(-10.5701265510248,22.4811383723668,4.84788653097856));
#93094=CARTESIAN_POINT('Ctrl Pts',(-10.5620856910867,22.4816196107549,4.85126703776691));
#93095=CARTESIAN_POINT('Ctrl Pts',(-10.556967448217,22.4819269025589,4.85338471658757));
#93096=CARTESIAN_POINT('Ctrl Pts',(-10.5296264381595,22.4835730885363,4.86451573052521));
#93097=CARTESIAN_POINT('Ctrl Pts',(-10.5071978644269,22.4849398555446,4.87301039038172));
#93098=CARTESIAN_POINT('Ctrl Pts',(-10.4374726871198,22.4892169015712,4.89747679838489));
#93099=CARTESIAN_POINT('Ctrl Pts',(-10.389561225325,22.4921940506583,4.91158251923256));
#93100=CARTESIAN_POINT('Ctrl Pts',(-10.2187042126284,22.5027498596996,4.95252279674843));
#93101=CARTESIAN_POINT('Ctrl Pts',(-10.0930883918712,22.5103436952666,4.96594655266575));
#93102=CARTESIAN_POINT('Ctrl Pts',(-9.94719455106615,22.5185445538024,4.96268519073684));
#93103=CARTESIAN_POINT('Ctrl Pts',(-9.92710725936704,22.5196617784042,4.96182183850248));
#93104=CARTESIAN_POINT('Ctrl Pts',(-9.89926200125617,22.5211945809215,4.96004962279458));
#93105=CARTESIAN_POINT('Ctrl Pts',(-9.89148458351597,22.5216209854787,4.9594921901468));
#93106=CARTESIAN_POINT('Ctrl Pts',(-9.87900101644436,22.5223027231859,4.95849711321739));
#93107=CARTESIAN_POINT('Ctrl Pts',(-9.87429195693191,22.5225592742618,4.95809878675033));
#93108=CARTESIAN_POINT('Ctrl Pts',(-9.86454776042906,22.5230888957556,4.95722699548386));
#93109=CARTESIAN_POINT('Ctrl Pts',(-9.85951297723979,22.5233618595618,4.956750226667));
#93110=CARTESIAN_POINT('Ctrl Pts',(-9.84772754396771,22.5239992414438,4.95557253682056));
#93111=CARTESIAN_POINT('Ctrl Pts',(-9.84097906594481,22.5243630037593,4.95485073305045));
#93112=CARTESIAN_POINT('Ctrl Pts',(-9.81904237227039,22.525541678257,4.95234996691129));
#93113=CARTESIAN_POINT('Ctrl Pts',(-9.80387669397077,22.5263506316995,4.95037986800109));
#93114=CARTESIAN_POINT('Ctrl Pts',(-9.72514010678688,22.530523389766,4.93889397453724));
#93115=CARTESIAN_POINT('Ctrl Pts',(-9.66221303996137,22.5337617301061,4.92543502397663));
#93116=CARTESIAN_POINT('Ctrl Pts',(-9.50314940943004,22.5419183568554,4.88028440052389));
#93117=CARTESIAN_POINT('Ctrl Pts',(-9.40905612180236,22.5467051003403,4.84269456087022));
#93118=CARTESIAN_POINT('Ctrl Pts',(-9.28463538804256,22.5537686416941,4.77735843630602));
#93119=CARTESIAN_POINT('Ctrl Pts',(-9.25043951768621,22.5557974036299,4.75759678468063));
#93120=CARTESIAN_POINT('Ctrl Pts',(-9.21196450136535,22.5582307368725,4.73323520340183));
#93121=CARTESIAN_POINT('Ctrl Pts',(-9.20686201993588,22.5585566041021,4.72995981888036));
#93122=CARTESIAN_POINT('Ctrl Pts',(-9.19873835479184,22.5590807381084,4.72467350596726));
#93123=CARTESIAN_POINT('Ctrl Pts',(-9.19570398826674,22.5592777108738,4.72268284736137));
#93124=CARTESIAN_POINT('Ctrl Pts',(-9.19033865550719,22.5596281812374,4.71913437216778));
#93125=CARTESIAN_POINT('Ctrl Pts',(-9.18800472399327,22.559781375924,4.71758111919497));
#93126=CARTESIAN_POINT('Ctrl Pts',(-9.18304650777291,22.5601084199452,4.71426078359355));
#93127=CARTESIAN_POINT('Ctrl Pts',(-9.1804235274089,22.5602823836695,4.71249192336214));
#93128=CARTESIAN_POINT('Ctrl Pts',(-9.17329830821541,22.5607574997561,4.70765320234867));
#93129=CARTESIAN_POINT('Ctrl Pts',(-9.16880749336588,22.5610597371712,4.70456671020674));
#93130=CARTESIAN_POINT('Ctrl Pts',(-9.14564520508725,22.5626326197223,4.68845630205375));
#93131=CARTESIAN_POINT('Ctrl Pts',(-9.12726320025808,22.5639283412568,4.67502376884263));
#93132=CARTESIAN_POINT('Ctrl Pts',(-9.07275907440296,22.567897499983,4.63321063302459));
#93133=CARTESIAN_POINT('Ctrl Pts',(-9.03765364698384,22.5706280636724,4.60355383027538));
#93134=CARTESIAN_POINT('Ctrl Pts',(-8.96104735560925,22.576898838187,4.53239855890177));
#93135=CARTESIAN_POINT('Ctrl Pts',(-8.92052698077911,22.5804473722342,4.48995333718377));
#93136=CARTESIAN_POINT('Ctrl Pts',(-8.82784427719296,22.5890119061862,4.38039047884784));
#93137=CARTESIAN_POINT('Ctrl Pts',(-8.77876148970576,22.5939496597367,4.31093574509366));
#93138=CARTESIAN_POINT('Ctrl Pts',(-8.73056857989218,22.5992490905748,4.22834816152548));
#93139=CARTESIAN_POINT('Ctrl Pts',(-8.72526732849789,22.5998395876382,4.21902976263872));
#93140=CARTESIAN_POINT('Ctrl Pts',(-8.7169300870781,22.6007807728254,4.20399271866026));
#93141=CARTESIAN_POINT('Ctrl Pts',(-8.71382888898637,22.6011337666144,4.19831083655522));
#93142=CARTESIAN_POINT('Ctrl Pts',(-8.70838683153946,22.6017584798298,4.18818088804253));
#93143=CARTESIAN_POINT('Ctrl Pts',(-8.70603101286213,22.602030723746,4.18374101296351));
#93144=CARTESIAN_POINT('Ctrl Pts',(-8.70116572675879,22.6025968158955,4.17445648284007));
#93145=CARTESIAN_POINT('Ctrl Pts',(-8.69866038114204,22.6028905167333,4.16960974760642));
#93146=CARTESIAN_POINT('Ctrl Pts',(-8.69221027626545,22.6036524994976,4.156958715662));
#93147=CARTESIAN_POINT('Ctrl Pts',(-8.688308223726,22.6041192932145,4.14913280930692));
#93148=CARTESIAN_POINT('Ctrl Pts',(-8.67143169860479,22.6061648174623,4.11451184381907));
#93149=CARTESIAN_POINT('Ctrl Pts',(-8.65920596021384,22.6077177893871,4.08735852891814));
#93150=CARTESIAN_POINT('Ctrl Pts',(-8.62838014972795,22.6118557861262,4.01290614814757));
#93151=CARTESIAN_POINT('Ctrl Pts',(-8.61140075924212,22.6143907918847,3.96498001105964));
#93152=CARTESIAN_POINT('Ctrl Pts',(-8.5824091863414,22.6194021548061,3.86726182230662));
#93153=CARTESIAN_POINT('Ctrl Pts',(-8.57044768130865,22.621874729861,3.81752984479307));
#93154=CARTESIAN_POINT('Ctrl Pts',(-8.5470523962627,22.6281143211862,3.69157981223646));
#93155=CARTESIAN_POINT('Ctrl Pts',(-8.53898854594407,22.6318914986452,3.61490202496454));
#93156=CARTESIAN_POINT('Ctrl Pts',(-8.53669852566943,22.6365488222445,3.52663329570811));
#93157=CARTESIAN_POINT('Ctrl Pts',(-8.53653623689309,22.6371522753425,3.51530802586005));
#93158=CARTESIAN_POINT('Ctrl Pts',(-8.53649351503026,22.6379983820729,3.4996079979015));
#93159=CARTESIAN_POINT('Ctrl Pts',(-8.53650122439319,22.6382351519513,3.49523365804045));
#93160=CARTESIAN_POINT('Ctrl Pts',(-8.53654500298769,22.6386162832846,3.48822435302707));
#93161=CARTESIAN_POINT('Ctrl Pts',(-8.53656857841696,22.6387599581613,3.485589301262));
#93162=CARTESIAN_POINT('Ctrl Pts',(-8.53663268604307,22.6390608965735,3.48008554270168));
#93163=CARTESIAN_POINT('Ctrl Pts',(-8.53667453709305,22.63921823512,3.47721688554606));
#93164=CARTESIAN_POINT('Ctrl Pts',(-8.53679654829945,22.6396011210742,3.47025685106362));
#93165=CARTESIAN_POINT('Ctrl Pts',(-8.5368854341287,22.639827146003,3.46616566415688));
#93166=CARTESIAN_POINT('Ctrl Pts',(-8.53725972763587,22.6406281068654,3.45172679953076));
#93167=CARTESIAN_POINT('Ctrl Pts',(-8.53763775586047,22.6412078651074,3.44138207833712));
#93168=CARTESIAN_POINT('Ctrl Pts',(-8.54062012861015,22.6447838264441,3.37815679354885));
#93169=CARTESIAN_POINT('Ctrl Pts',(-8.54598259541785,22.6479030951848,3.32544983487339));
#93170=CARTESIAN_POINT('Ctrl Pts',(-8.5696521625787,22.657028497248,3.1745905257829));
#93171=CARTESIAN_POINT('Ctrl Pts',(-8.59515715009997,22.6631050551889,3.07785567250033));
#93172=CARTESIAN_POINT('Ctrl Pts',(-8.63541009758138,22.6697776582425,2.97090976213766));
#93173=CARTESIAN_POINT('Ctrl Pts',(-8.64071389204297,22.67061842507,2.95742892043499));
#93174=CARTESIAN_POINT('Ctrl Pts',(-8.66161464579819,22.6737902041093,2.90653585103432));
#93175=CARTESIAN_POINT('Ctrl Pts',(-8.6785640213756,22.6760806892185,2.8696965342615));
#93176=CARTESIAN_POINT('Ctrl Pts',(-8.7015746585457,22.6788715919741,2.82470463045362));
#93177=CARTESIAN_POINT('Ctrl Pts',(-8.70621819402671,22.6794205601664,2.8158502729913));
#93178=CARTESIAN_POINT('Ctrl Pts',(-8.71369423279636,22.6802824957722,2.80194322553294));
#93179=CARTESIAN_POINT('Ctrl Pts',(-8.71646656441212,22.680597564009,2.79685868547283));
#93180=CARTESIAN_POINT('Ctrl Pts',(-8.72167497630141,22.681181141717,2.78743975487316));
#93181=CARTESIAN_POINT('Ctrl Pts',(-8.72410309731634,22.6814499274489,2.78310107845231));
#93182=CARTESIAN_POINT('Ctrl Pts',(-8.72953039706457,22.6820435649402,2.77351825028911));
#93183=CARTESIAN_POINT('Ctrl Pts',(-8.73254004097025,22.682368037936,2.76828010933189));
#93184=CARTESIAN_POINT('Ctrl Pts',(-8.741343005884,22.6833036776209,2.75317625109079));
#93185=CARTESIAN_POINT('Ctrl Pts',(-8.74721975983142,22.683911843915,2.74335951700131));
#93186=CARTESIAN_POINT('Ctrl Pts',(-8.79624458086464,22.6888555074478,2.66360403823154));
#93187=CARTESIAN_POINT('Ctrl Pts',(-8.8450998973512,22.6929679573975,2.59734096251965));
#93188=CARTESIAN_POINT('Ctrl Pts',(-8.95081886252593,22.7008277252456,2.47668640122467));
#93189=CARTESIAN_POINT('Ctrl Pts',(-9.00700469158878,22.7045730324335,2.42208009176569));
#93190=CARTESIAN_POINT('Ctrl Pts',(-9.08007448707135,22.7092848832404,2.36164818997359));
#93191=CARTESIAN_POINT('Ctrl Pts',(-9.0930448151381,22.7101160606059,2.35128765136581));
#93192=CARTESIAN_POINT('Ctrl Pts',(-9.13327206936112,22.7126873021239,2.32026068537524));
#93193=CARTESIAN_POINT('Ctrl Pts',(-9.16107792589567,22.7144554446702,2.30032856113271));
#93194=CARTESIAN_POINT('Ctrl Pts',(-9.19441224937206,22.7165962941725,2.2781593124847));
#93195=CARTESIAN_POINT('Ctrl Pts',(-9.19928952173482,22.7169100458983,2.27495754467257));
#93196=CARTESIAN_POINT('Ctrl Pts',(-9.20720698261587,22.7174204218165,2.26982747478636));
#93197=CARTESIAN_POINT('Ctrl Pts',(-9.21023541875867,22.7176158875706,2.26788104638606));
#93198=CARTESIAN_POINT('Ctrl Pts',(-9.21562651509707,22.7179643411153,2.26444413730028));
#93199=CARTESIAN_POINT('Ctrl Pts',(-9.21798629426919,22.7181170345464,2.262949225944));
#93200=CARTESIAN_POINT('Ctrl Pts',(-9.22307474343982,22.7184466700936,2.2597460909196));
#93201=CARTESIAN_POINT('Ctrl Pts',(-9.22580473291283,22.7186237501001,2.25804013701011));
#93202=CARTESIAN_POINT('Ctrl Pts',(-9.23338518222181,22.7191160351367,2.25333786606279));
#93203=CARTESIAN_POINT('Ctrl Pts',(-9.23824750241473,22.7194324576396,2.25036089799427));
#93204=CARTESIAN_POINT('Ctrl Pts',(-9.26569853111618,22.721221998116,2.23377368023433));
#93205=CARTESIAN_POINT('Ctrl Pts',(-9.28863318567846,22.7227289026172,2.22074833709387));
#93206=CARTESIAN_POINT('Ctrl Pts',(-9.36349016166762,22.7276544911791,2.18087013012933));
#93207=CARTESIAN_POINT('Ctrl Pts',(-9.41667185743574,22.7311626819627,2.15650607990044));
#93208=CARTESIAN_POINT('Ctrl Pts',(-9.58286126871001,22.7418934069023,2.09210175433712));
#93209=CARTESIAN_POINT('Ctrl Pts',(-9.69947160524684,22.7490656316642,2.06268490817348));
#93210=CARTESIAN_POINT('Ctrl Pts',(-9.83457843120436,22.7566733659988,2.04578731457639));
#93211=CARTESIAN_POINT('Ctrl Pts',(-9.85081269514866,22.7575772843953,2.04403227773033));
#93212=CARTESIAN_POINT('Ctrl Pts',(-9.87349634966723,22.758826482709,2.04196341822132));
#93213=CARTESIAN_POINT('Ctrl Pts',(-9.87992316449001,22.7591788695553,2.0414200732242));
#93214=CARTESIAN_POINT('Ctrl Pts',(-9.89104746321068,22.7597862081531,2.04055361101967));
#93215=CARTESIAN_POINT('Ctrl Pts',(-9.89574326661374,22.7600417738813,2.04021064812564));
#93216=CARTESIAN_POINT('Ctrl Pts',(-9.90549741223821,22.7605709925661,2.03954555007214));
#93217=CARTESIAN_POINT('Ctrl Pts',(-9.91055594269594,22.7608445300248,2.03922701937872));
#93218=CARTESIAN_POINT('Ctrl Pts',(-9.92245935497029,22.7614860876628,2.03853953692759));
#93219=CARTESIAN_POINT('Ctrl Pts',(-9.9293054091789,22.7618534262664,2.03819238141261));
#93220=CARTESIAN_POINT('Ctrl Pts',(-9.95181444004333,22.7630559655072,2.03720947251223));
#93221=CARTESIAN_POINT('Ctrl Pts',(-9.9674855009764,22.7638848601518,2.0367772528237));
#93222=CARTESIAN_POINT('Ctrl Pts',(-10.1002298403708,22.7708421441393,2.03524978859578));
#93223=CARTESIAN_POINT('Ctrl Pts',(-10.217036074077,22.7764968213933,2.04795409076538));
#93224=CARTESIAN_POINT('Ctrl Pts',(-10.4092654661118,22.7861016063849,2.09259982242306));
#93225=CARTESIAN_POINT('Ctrl Pts',(-10.4858075344022,22.7900266848575,2.11715452202747));
#93226=CARTESIAN_POINT('Ctrl Pts',(-10.5704196880202,22.7948569382465,2.15219354125984));
#93227=CARTESIAN_POINT('Ctrl Pts',(-10.5808467652359,22.7954611601564,2.1566542178859));
#93228=CARTESIAN_POINT('Ctrl Pts',(-10.595224340333,22.7963081784401,2.1630035936448));
#93229=CARTESIAN_POINT('Ctrl Pts',(-10.5992200510468,22.7965450745061,2.1647896288009));
#93230=CARTESIAN_POINT('Ctrl Pts',(-10.6056089803002,22.7969263570545,2.16767985847276));
#93231=CARTESIAN_POINT('Ctrl Pts',(-10.6080073640733,22.7970700559468,2.16877265595065));
#93232=CARTESIAN_POINT('Ctrl Pts',(-10.6130099511688,22.7973709963732,2.17106836944284));
#93233=CARTESIAN_POINT('Ctrl Pts',(-10.6156135749375,22.7975283126558,2.17227246589962));
#93234=CARTESIAN_POINT('Ctrl Pts',(-10.6218463179888,22.7979065360459,2.17517719311851));
#93235=CARTESIAN_POINT('Ctrl Pts',(-10.6254720142168,22.7981278824866,2.17688508757524));
#93236=CARTESIAN_POINT('Ctrl Pts',(-10.6380206811357,22.7988984623876,2.1828592780222));
#93237=CARTESIAN_POINT('Ctrl Pts',(-10.6469071845318,22.799452061825,2.18720102271969));
#93238=CARTESIAN_POINT('Ctrl Pts',(-10.6685520949324,22.8008186578342,2.19804936736561));
#93239=CARTESIAN_POINT('Ctrl Pts',(-10.6812601242232,22.8016366628312,2.2046537265875));
#93240=CARTESIAN_POINT('Ctrl Pts',(-10.7309158696414,22.80488916689,2.23139261074237));
#93241=CARTESIAN_POINT('Ctrl Pts',(-10.767083292063,22.8073818547067,2.25292922879085));
#93242=CARTESIAN_POINT('Ctrl Pts',(-10.822896835068,22.8113754987719,2.28951196558835));
#93243=CARTESIAN_POINT('Ctrl Pts',(-10.8431781172665,22.8128595271252,2.30355061979335));
#93244=CARTESIAN_POINT('Ctrl Pts',(-10.9572840015759,22.8213679653181,2.38687726366919));
#93245=CARTESIAN_POINT('Ctrl Pts',(-11.0429303386377,22.8283385923076,2.4666848248111));
#93246=CARTESIAN_POINT('Ctrl Pts',(-11.1288827374588,22.8357853937335,2.56847960483394));
#93247=CARTESIAN_POINT('Ctrl Pts',(-11.1393511040777,22.836702425393,2.58131312470328));
#93248=CARTESIAN_POINT('Ctrl Pts',(-11.1536151227035,22.8379666762122,2.59941879867794));
#93249=CARTESIAN_POINT('Ctrl Pts',(-11.1575966367605,22.8383212274291,2.60454236282957));
#93250=CARTESIAN_POINT('Ctrl Pts',(-11.1644143085091,22.8389312797684,2.61343706924072));
#93251=CARTESIAN_POINT('Ctrl Pts',(-11.1672665234708,22.8391874078525,2.61719573179112));
#93252=CARTESIAN_POINT('Ctrl Pts',(-11.1731409083994,22.8397168490923,2.62501526753549));
#93253=CARTESIAN_POINT('Ctrl Pts',(-11.1761602901202,22.8399900518644,2.62907816318595));
#93254=CARTESIAN_POINT('Ctrl Pts',(-11.1831953719825,22.8406291894151,2.63864791676857));
#93255=CARTESIAN_POINT('Ctrl Pts',(-11.1871938235436,22.8409944575832,2.64416734869062));
#93256=CARTESIAN_POINT('Ctrl Pts',(-11.2001315268154,22.842183140367,2.66229160630215));
#93257=CARTESIAN_POINT('Ctrl Pts',(-11.2089098875799,22.843000451886,2.67501033811641));
#93258=CARTESIAN_POINT('Ctrl Pts',(-11.2538775766745,22.8472488226323,2.74242225251815));
#93259=CARTESIAN_POINT('Ctrl Pts',(-11.2865635122918,22.8505489835348,2.79936556394677));
#93260=CARTESIAN_POINT('Ctrl Pts',(-11.3338967311457,22.8558691003758,2.89638884000875));
#93261=CARTESIAN_POINT('Ctrl Pts',(-11.3508097537221,22.8579272232439,2.93525224182512));
#93262=CARTESIAN_POINT('Ctrl Pts',(-11.3822882437941,22.8621917575018,3.01712509042033));
#93263=CARTESIAN_POINT('Ctrl Pts',(-11.3965864969178,22.8643960686362,3.06018766095683));
#93264=CARTESIAN_POINT('Ctrl Pts',(-11.413960769318,22.8675830727605,3.12197619298645));
#93265=CARTESIAN_POINT('Ctrl Pts',(-11.4187089063772,22.8685263357334,3.14020553463525));
#93266=CARTESIAN_POINT('Ctrl Pts',(-11.4307820501429,22.8711499322043,3.19051999796195));
#93267=CARTESIAN_POINT('Ctrl Pts',(-11.4373783487565,22.8728536122414,3.2227666769586));
#93268=CARTESIAN_POINT('Ctrl Pts',(-11.4438471757254,22.8749222356935,3.26089565077517));
#93269=CARTESIAN_POINT('Ctrl Pts',(-11.4447788210633,22.875232644233,3.26659110412079));
#93270=CARTESIAN_POINT('Ctrl Pts',(-11.4462339212287,22.8757386322208,3.27582926369374));
#93271=CARTESIAN_POINT('Ctrl Pts',(-11.4467781107998,22.8759330853976,3.27936869786372));
#93272=CARTESIAN_POINT('Ctrl Pts',(-11.4477234132299,22.8762804332114,3.28567090130255));
#93273=CARTESIAN_POINT('Ctrl Pts',(-11.4481296171573,22.8764330406532,3.28843285808626));
#93274=CARTESIAN_POINT('Ctrl Pts',(-11.4489032929726,22.8767303498689,3.2938000495479));
#93275=CARTESIAN_POINT('Ctrl Pts',(-11.4492716379632,22.8768749935162,3.2964050808023));
#93276=CARTESIAN_POINT('Ctrl Pts',(-11.4500718859662,22.8771962038907,3.30217687069662));
#93277=CARTESIAN_POINT('Ctrl Pts',(-11.4505004425063,22.8773729526437,3.30534407059447));
#93278=CARTESIAN_POINT('Ctrl Pts',(-11.4515403440335,22.8778138430751,3.31322350615535));
#93279=CARTESIAN_POINT('Ctrl Pts',(-11.4521391158866,22.8780786431754,3.31793732979647));
#93280=CARTESIAN_POINT('Ctrl Pts',(-11.4546836389871,22.8792538586846,3.33878056841656));
#93281=CARTESIAN_POINT('Ctrl Pts',(-11.4563836145155,22.8801763564431,3.35493822620845));
#93282=CARTESIAN_POINT('Ctrl Pts',(-11.4615725124831,22.8835608832481,3.41363202851132));
#93283=CARTESIAN_POINT('Ctrl Pts',(-11.4634692177633,22.8860835649692,3.45628519631487));
#93284=CARTESIAN_POINT('Ctrl Pts',(-11.4634996283537,22.8886343115925,3.49895701930366));
#93285=CARTESIAN_POINT('Ctrl Pts',(-11.4634996286686,22.8886343380185,3.49895746138947));
#93286=CARTESIAN_POINT('Ctrl Pts',(-11.4634998762247,22.8886551110645,3.49930497676595));
#93287=CARTESIAN_POINT('Ctrl Pts',(-11.4635,22.8886758857888,3.49965248964563));
#93288=CARTESIAN_POINT('Ctrl Pts',(-11.4635,22.8886966621701,3.49999999996283));
#93289=CARTESIAN_POINT('Origin',(-10.,13.2,3.5));
#93290=CARTESIAN_POINT('',(-11.4635,23.4593691294935,3.50000000000014));
#93291=CARTESIAN_POINT('',(-11.4635,23.3906983315425,3.49999999997929));
#93292=CARTESIAN_POINT('',(-11.4635,13.2,3.5));
#93293=CARTESIAN_POINT('Ctrl Pts',(-11.4635,23.4593691294935,3.50000000000014));
#93294=CARTESIAN_POINT('Ctrl Pts',(-11.4635,23.4593632578606,3.49988815824253));
#93295=CARTESIAN_POINT('Ctrl Pts',(-11.4634999872435,23.4593573865652,3.49977631641766));
#93296=CARTESIAN_POINT('Ctrl Pts',(-11.4634862607233,23.4562145842122,3.43990509731606));
#93297=CARTESIAN_POINT('Ctrl Pts',(-11.4598124220148,23.4531917336194,3.38019956334097));
#93298=CARTESIAN_POINT('Ctrl Pts',(-11.4448085976956,23.4471221355299,3.25853176031568));
#93299=CARTESIAN_POINT('Ctrl Pts',(-11.4331130811415,23.4440884055884,3.19674123955496));
#93300=CARTESIAN_POINT('Ctrl Pts',(-11.3969745636183,23.4370116351706,3.05605230727827));
#93301=CARTESIAN_POINT('Ctrl Pts',(-11.3697592702726,23.4329623945494,2.97809621824932));
#93302=CARTESIAN_POINT('Ctrl Pts',(-11.3332284796358,23.4281841636351,2.89635710278226));
#93303=CARTESIAN_POINT('Ctrl Pts',(-11.3302765428507,23.4278016676637,2.88987932200807));
#93304=CARTESIAN_POINT('Ctrl Pts',(-11.3257961099855,23.4272260655346,2.88023448876226));
#93305=CARTESIAN_POINT('Ctrl Pts',(-11.324303222454,23.4270350694218,2.8770508940192));
#93306=CARTESIAN_POINT('Ctrl Pts',(-11.3216070504611,23.4266914894448,2.87135477826376));
#93307=CARTESIAN_POINT('Ctrl Pts',(-11.3204080520168,23.4265391685386,2.86884028436942));
#93308=CARTESIAN_POINT('Ctrl Pts',(-11.3177830551722,23.4262066950051,2.8633754583176));
#93309=CARTESIAN_POINT('Ctrl Pts',(-11.3163543439752,23.4260263803924,2.86042652632021));
#93310=CARTESIAN_POINT('Ctrl Pts',(-11.3122950715138,23.4255159183703,2.85211920258404));
#93311=CARTESIAN_POINT('Ctrl Pts',(-11.3096416444315,23.4251844054637,2.84677213543443));
#93312=CARTESIAN_POINT('Ctrl Pts',(-11.292997408534,23.4231188401392,2.81374047722888));
#93313=CARTESIAN_POINT('Ctrl Pts',(-11.2781629935707,23.4213379441754,2.78649210635572));
#93314=CARTESIAN_POINT('Ctrl Pts',(-11.182015491558,23.410234127612,2.62251800540867));
#93315=CARTESIAN_POINT('Ctrl Pts',(-11.079718451366,23.4003521842531,2.49931923367241));
#93316=CARTESIAN_POINT('Ctrl Pts',(-10.9391425458784,23.3897884236964,2.37724651157466));
#93317=CARTESIAN_POINT('Ctrl Pts',(-10.9182273781797,23.3882755129909,2.36007774999035));
#93318=CARTESIAN_POINT('Ctrl Pts',(-10.8899155711151,23.3863026481125,2.33812243797221));
#93319=CARTESIAN_POINT('Ctrl Pts',(-10.8829356113594,23.3858220765509,2.33280939699018));
#93320=CARTESIAN_POINT('Ctrl Pts',(-10.8715335385063,23.3850463071887,2.32429112439137));
#93321=CARTESIAN_POINT('Ctrl Pts',(-10.8671405821222,23.3847496187462,2.32104737970939));
#93322=CARTESIAN_POINT('Ctrl Pts',(-10.858672683635,23.3841818831132,2.31486764634948));
#93323=CARTESIAN_POINT('Ctrl Pts',(-10.854600588547,23.3839106938222,2.31192790277092));
#93324=CARTESIAN_POINT('Ctrl Pts',(-10.8451695547439,23.3832867745188,2.30519298897646));
#93325=CARTESIAN_POINT('Ctrl Pts',(-10.8398000221075,23.3829346179594,2.30141279222511));
#93326=CARTESIAN_POINT('Ctrl Pts',(-10.8228252374415,23.3818308130526,2.28963247055054));
#93327=CARTESIAN_POINT('Ctrl Pts',(-10.811129558823,23.3810841027067,2.28176365806137));
#93328=CARTESIAN_POINT('Ctrl Pts',(-10.7531947883521,23.3774497194202,2.24398961914468));
#93329=CARTESIAN_POINT('Ctrl Pts',(-10.7054048273343,23.3746526114417,2.21654009464506));
#93330=CARTESIAN_POINT('Ctrl Pts',(-10.5624940011442,23.3667031977485,2.14485512230858));
#93331=CARTESIAN_POINT('Ctrl Pts',(-10.4640395967639,23.3617458600027,2.10806511993116));
#93332=CARTESIAN_POINT('Ctrl Pts',(-10.3524648877767,23.3560027984606,2.07953946264981));
#93333=CARTESIAN_POINT('Ctrl Pts',(-10.342398292027,23.3554833392569,2.07707939833107));
#93334=CARTESIAN_POINT('Ctrl Pts',(-10.2966815823984,23.3531150951225,2.06642041754621));
#93335=CARTESIAN_POINT('Ctrl Pts',(-10.2607604035848,23.3512292676502,2.05945358476841));
#93336=CARTESIAN_POINT('Ctrl Pts',(-10.2187432672426,23.3489562776205,2.05292744128819));
#93337=CARTESIAN_POINT('Ctrl Pts',(-10.2128621248004,23.3486366073718,2.05205064986091));
#93338=CARTESIAN_POINT('Ctrl Pts',(-10.2034179087093,23.3481205989619,2.05070143789938));
#93339=CARTESIAN_POINT('Ctrl Pts',(-10.1998580928725,23.3479254927213,2.05020625265458));
#93340=CARTESIAN_POINT('Ctrl Pts',(-10.1935233503482,23.3475771631589,2.04934883784084));
#93341=CARTESIAN_POINT('Ctrl Pts',(-10.1907491682092,23.347424230102,2.04898144873012));
#93342=CARTESIAN_POINT('Ctrl Pts',(-10.1848174475355,23.347096381962,2.0482132073175));
#93343=CARTESIAN_POINT('Ctrl Pts',(-10.1816596997272,23.3469213439259,2.0478147041727));
#93344=CARTESIAN_POINT('Ctrl Pts',(-10.1730032350141,23.3464401601862,2.04675094726629));
#93345=CARTESIAN_POINT('Ctrl Pts',(-10.1675020604446,23.3461328828674,2.04610661108514));
#93346=CARTESIAN_POINT('Ctrl Pts',(-10.1381497675732,23.344485928735,2.042837463267));
#93347=CARTESIAN_POINT('Ctrl Pts',(-10.1142417447085,23.343118344492,2.04076845456114));
#93348=CARTESIAN_POINT('Ctrl Pts',(-10.0404221280921,23.3388373269634,2.03620523060962));
#93349=CARTESIAN_POINT('Ctrl Pts',(-9.99042675817685,23.3358568814999,2.03567871350067));
#93350=CARTESIAN_POINT('Ctrl Pts',(-9.81456210462102,23.325281853267,2.04283387757246));
#93351=CARTESIAN_POINT('Ctrl Pts',(-9.68978186000774,23.3176728032944,2.06420897701625));
#93352=CARTESIAN_POINT('Ctrl Pts',(-9.55029787953807,23.3094738924047,2.10716312457877));
#93353=CARTESIAN_POINT('Ctrl Pts',(-9.53144045429824,23.3083705902725,2.1133931468163));
#93354=CARTESIAN_POINT('Ctrl Pts',(-9.50539886178193,23.3068535474493,2.12258860052247));
#93355=CARTESIAN_POINT('Ctrl Pts',(-9.49810330949461,23.3064292703481,2.12523014120577));
#93356=CARTESIAN_POINT('Ctrl Pts',(-9.48640626101758,23.3057501092564,2.12957087898147));
#93357=CARTESIAN_POINT('Ctrl Pts',(-9.48199143939019,23.3054940237328,2.13123353477724));
#93358=CARTESIAN_POINT('Ctrl Pts',(-9.47285838992828,23.3049647464603,2.1347236276359));
#93359=CARTESIAN_POINT('Ctrl Pts',(-9.46814143973695,23.3046916646018,2.13655424648889));
#93360=CARTESIAN_POINT('Ctrl Pts',(-9.45709838241703,23.304052942589,2.14090601587066));
#93361=CARTESIAN_POINT('Ctrl Pts',(-9.45078016070777,23.303687967372,2.14344694378261));
#93362=CARTESIAN_POINT('Ctrl Pts',(-9.4302054019061,23.302500816227,2.15188857070964));
#93363=CARTESIAN_POINT('Ctrl Pts',(-9.41602414599485,23.3016847228339,2.15797073966035));
#93364=CARTESIAN_POINT('Ctrl Pts',(-9.34224590152656,23.2974465479455,2.1910043028034));
#93365=CARTESIAN_POINT('Ctrl Pts',(-9.28440630869461,23.2941546344506,2.22170538834727));
#93366=CARTESIAN_POINT('Ctrl Pts',(-9.15689389870421,23.286759799131,2.30076506349985));
#93367=CARTESIAN_POINT('Ctrl Pts',(-9.08898316446741,23.2827197268619,2.35150534435276));
#93368=CARTESIAN_POINT('Ctrl Pts',(-9.02143385367742,23.2782386133338,2.41175582593712));
#93369=CARTESIAN_POINT('Ctrl Pts',(-9.0170530810563,23.277945689634,2.41571109074918));
#93370=CARTESIAN_POINT('Ctrl Pts',(-9.00331008218715,23.2770190158152,2.42827095472169));
#93371=CARTESIAN_POINT('Ctrl Pts',(-8.99403614000006,23.2763822387354,2.43697100709232));
#93372=CARTESIAN_POINT('Ctrl Pts',(-8.95881370713339,23.2739140938223,2.47088751948754));
#93373=CARTESIAN_POINT('Ctrl Pts',(-8.93369213583686,23.2720479596064,2.49694041704338));
#93374=CARTESIAN_POINT('Ctrl Pts',(-8.90560883913313,23.2697970169586,2.52831311806146));
#93375=CARTESIAN_POINT('Ctrl Pts',(-8.90168098651855,23.2694782272225,2.53275507147281));
#93376=CARTESIAN_POINT('Ctrl Pts',(-8.89541909311083,23.268963369262,2.53992388184037));
#93377=CARTESIAN_POINT('Ctrl Pts',(-8.89306786164096,23.2687685242123,2.54263571560635));
#93378=CARTESIAN_POINT('Ctrl Pts',(-8.88890158620925,23.2684204862605,2.54747682807188));
#93379=CARTESIAN_POINT('Ctrl Pts',(-8.88708264600147,23.2682675818162,2.54960269294711));
#93380=CARTESIAN_POINT('Ctrl Pts',(-8.88320551986509,23.267939592452,2.55416043174865));
#93381=CARTESIAN_POINT('Ctrl Pts',(-8.8811492075398,23.2677643832859,2.55659377596874));
#93382=CARTESIAN_POINT('Ctrl Pts',(-8.87553076939329,23.2672822579619,2.56328657994895));
#93383=CARTESIAN_POINT('Ctrl Pts',(-8.87198495194373,23.26697420297,2.56755958302119));
#93384=CARTESIAN_POINT('Ctrl Pts',(-8.8531230885981,23.2653155977007,2.59055472882892));
#93385=CARTESIAN_POINT('Ctrl Pts',(-8.8382494979434,23.2639366810581,2.60963323191021));
#93386=CARTESIAN_POINT('Ctrl Pts',(-8.79373001966236,23.259605297363,2.66975438663009));
#93387=CARTESIAN_POINT('Ctrl Pts',(-8.76573659039813,23.2565841590063,2.71197191164284));
#93388=CARTESIAN_POINT('Ctrl Pts',(-8.67284352356797,23.245609574786,2.86919756308391));
#93389=CARTESIAN_POINT('Ctrl Pts',(-8.6213676387662,23.237654381996,2.99143144450295));
#93390=CARTESIAN_POINT('Ctrl Pts',(-8.58298529249327,23.2294356849403,3.13375227232262));
#93391=CARTESIAN_POINT('Ctrl Pts',(-8.57922013462518,23.2285868725809,3.14864166619938));
#93392=CARTESIAN_POINT('Ctrl Pts',(-8.57428361476905,23.2274103659465,3.16954203385923));
#93393=CARTESIAN_POINT('Ctrl Pts',(-8.57291464210262,23.227076399603,3.17550491318166));
#93394=CARTESIAN_POINT('Ctrl Pts',(-8.57047572243623,23.2264668752726,3.18644222720206));
#93395=CARTESIAN_POINT('Ctrl Pts',(-8.56939425365882,23.2261909546299,3.19141397233299));
#93396=CARTESIAN_POINT('Ctrl Pts',(-8.56725580517542,23.2256336173116,3.20149778708062));
#93397=CARTESIAN_POINT('Ctrl Pts',(-8.56620020494644,23.2253522479343,3.20661007584037));
#93398=CARTESIAN_POINT('Ctrl Pts',(-8.56366398540935,23.2246603502547,3.21923370296954));
#93399=CARTESIAN_POINT('Ctrl Pts',(-8.56221490003068,23.2242508232875,3.2267512677378));
#93400=CARTESIAN_POINT('Ctrl Pts',(-8.55705625614476,23.2227377885463,3.25469117004693));
#93401=CARTESIAN_POINT('Ctrl Pts',(-8.55372219686599,23.221646088447,3.27518086611885));
#93402=CARTESIAN_POINT('Ctrl Pts',(-8.53663135843362,23.2152795472986,3.39643339167672));
#93403=CARTESIAN_POINT('Ctrl Pts',(-8.53297124394648,23.2103349814459,3.49833741550094));
#93404=CARTESIAN_POINT('Ctrl Pts',(-8.54596128297862,23.2010739510337,3.68837360792246));
#93405=CARTESIAN_POINT('Ctrl Pts',(-8.56006087037098,23.196767056641,3.77619696614342));
#93406=CARTESIAN_POINT('Ctrl Pts',(-8.58480149378482,23.191492710328,3.87305660669383));
#93407=CARTESIAN_POINT('Ctrl Pts',(-8.58770194194969,23.1908950371236,3.88389090093137));
#93408=CARTESIAN_POINT('Ctrl Pts',(-8.59190119147437,23.1900558360469,3.89888465315383));
#93409=CARTESIAN_POINT('Ctrl Pts',(-8.59309454848456,23.1898200686923,3.90307353002356));
#93410=CARTESIAN_POINT('Ctrl Pts',(-8.59503870182253,23.1894401720479,3.90978399496553));
#93411=CARTESIAN_POINT('Ctrl Pts',(-8.59577763958166,23.1892967214946,3.91230902752832));
#93412=CARTESIAN_POINT('Ctrl Pts',(-8.59733713228558,23.188995900171,3.91758516673725));
#93413=CARTESIAN_POINT('Ctrl Pts',(-8.59815897544982,23.1888384525243,3.92033585781708));
#93414=CARTESIAN_POINT('Ctrl Pts',(-8.60017580564527,23.1884547064939,3.92701443933313));
#93415=CARTESIAN_POINT('Ctrl Pts',(-8.60137923454308,23.1882279250823,3.93093974067632));
#93416=CARTESIAN_POINT('Ctrl Pts',(-8.60570210166082,23.1874211077206,3.94483106178019));
#93417=CARTESIAN_POINT('Ctrl Pts',(-8.60891159981861,23.1868361562742,3.95476846080497));
#93418=CARTESIAN_POINT('Ctrl Pts',(-8.62933717053681,23.1832009346289,4.01577096110999));
#93419=CARTESIAN_POINT('Ctrl Pts',(-8.6492552212961,23.1800233902133,4.06588318245053));
#93420=CARTESIAN_POINT('Ctrl Pts',(-8.71106002443181,23.1712264548011,4.19940072776324));
#93421=CARTESIAN_POINT('Ctrl Pts',(-8.75823340650999,23.1655523979265,4.28009329937455));
#93422=CARTESIAN_POINT('Ctrl Pts',(-8.84697252406236,23.1566519456506,4.40320662572449));
#93423=CARTESIAN_POINT('Ctrl Pts',(-8.8839969289981,23.1533049202004,4.44857421088516));
#93424=CARTESIAN_POINT('Ctrl Pts',(-8.9305013832462,23.1495058338649,4.49905327290175));
#93425=CARTESIAN_POINT('Ctrl Pts',(-8.93743777428377,23.1489487338904,4.50642747232824));
#93426=CARTESIAN_POINT('Ctrl Pts',(-8.94885794735696,23.1480467616796,4.51831877465833));
#93427=CARTESIAN_POINT('Ctrl Pts',(-8.95329558090572,23.1476999322257,4.52287956402217));
#93428=CARTESIAN_POINT('Ctrl Pts',(-8.96127043618129,23.1470830801619,4.530969498547));
#93429=CARTESIAN_POINT('Ctrl Pts',(-8.96479623111008,23.1468125682619,4.53450972514551));
#93430=CARTESIAN_POINT('Ctrl Pts',(-8.97228706870468,23.1462424501754,4.54195458011746));
#93431=CARTESIAN_POINT('Ctrl Pts',(-8.97625639784298,23.1459430390391,4.54585479603831));
#93432=CARTESIAN_POINT('Ctrl Pts',(-8.98687755017851,23.1451489209597,4.55617260953813));
#93433=CARTESIAN_POINT('Ctrl Pts',(-8.99356814729659,23.1446559485351,4.56255005087068));
#93434=CARTESIAN_POINT('Ctrl Pts',(-9.02596106013155,23.1423030911922,4.59284632058364));
#93435=CARTESIAN_POINT('Ctrl Pts',(-9.05245915722957,23.1404798058875,4.61589943327915));
#93436=CARTESIAN_POINT('Ctrl Pts',(-9.13053700935324,23.1353574659586,4.67903787322278));
#93437=CARTESIAN_POINT('Ctrl Pts',(-9.1840050877526,23.1321462581884,4.7166549800129));
#93438=CARTESIAN_POINT('Ctrl Pts',(-9.33310267538688,23.1236444654527,4.8072872519166));
#93439=CARTESIAN_POINT('Ctrl Pts',(-9.43243620930461,23.1184442891638,4.85337240871525));
#93440=CARTESIAN_POINT('Ctrl Pts',(-9.54545439915662,23.1121382749076,4.89115812745899));
#93441=CARTESIAN_POINT('Ctrl Pts',(-9.5549889202999,23.1116032436673,4.89423734234839));
#93442=CARTESIAN_POINT('Ctrl Pts',(-9.56812852638618,23.1108608072702,4.89833232752536));
#93443=CARTESIAN_POINT('Ctrl Pts',(-9.57170723254709,23.1106580797545,4.89943258953251));
#93444=CARTESIAN_POINT('Ctrl Pts',(-9.57783360307508,23.1103100863705,4.90129042234548));
#93445=CARTESIAN_POINT('Ctrl Pts',(-9.58037920051778,23.110165211746,4.90205481307217));
#93446=CARTESIAN_POINT('Ctrl Pts',(-9.58565830928646,23.109864165248,4.90362435634884));
#93447=CARTESIAN_POINT('Ctrl Pts',(-9.58839209096988,23.1097079314967,4.9044284599533));
#93448=CARTESIAN_POINT('Ctrl Pts',(-9.59496125611254,23.1093317256189,4.90633986020267));
#93449=CARTESIAN_POINT('Ctrl Pts',(-9.59879884463419,23.1091113147192,4.90743945468558));
#93450=CARTESIAN_POINT('Ctrl Pts',(-9.6120102780117,23.1083504448057,4.91116653824107));
#93451=CARTESIAN_POINT('Ctrl Pts',(-9.62140560496999,23.1078057679646,4.91371613015089));
#93452=CARTESIAN_POINT('Ctrl Pts',(-9.67623851796131,23.1046089660205,4.92801024295915));
#93453=CARTESIAN_POINT('Ctrl Pts',(-9.72219109816754,23.1018590684047,4.93765649757183));
#93454=CARTESIAN_POINT('Ctrl Pts',(-9.83231283422067,23.0952210562306,4.95529611892682));
#93455=CARTESIAN_POINT('Ctrl Pts',(-9.8967085531115,23.0913037976168,4.96127911044436));
#93456=CARTESIAN_POINT('Ctrl Pts',(-9.9867199916218,23.0859089540211,4.96366085426181));
#93457=CARTESIAN_POINT('Ctrl Pts',(-10.0121651137151,23.0843923057755,4.96367056651665));
#93458=CARTESIAN_POINT('Ctrl Pts',(-10.1065936189521,23.078807917991,4.96124384243889));
#93459=CARTESIAN_POINT('Ctrl Pts',(-10.1753837173784,23.0748325462652,4.95459219188854));
#93460=CARTESIAN_POINT('Ctrl Pts',(-10.2537500861445,23.0704305712913,4.94137161724813));
#93461=CARTESIAN_POINT('Ctrl Pts',(-10.2640259993883,23.0698557578925,4.93952475658371));
#93462=CARTESIAN_POINT('Ctrl Pts',(-10.2805576373101,23.0689347397767,4.93637059509323));
#93463=CARTESIAN_POINT('Ctrl Pts',(-10.2868259714919,23.0685863825012,4.9351320281393));
#93464=CARTESIAN_POINT('Ctrl Pts',(-10.2979972780856,23.067967043965,4.93284856144747));
#93465=CARTESIAN_POINT('Ctrl Pts',(-10.3029033436998,23.0676955680726,4.93181945196736));
#93466=CARTESIAN_POINT('Ctrl Pts',(-10.3131750518944,23.0671282358291,4.92960967381251));
#93467=CARTESIAN_POINT('Ctrl Pts',(-10.3185395362618,23.0668325443672,4.92842395581855));
#93468=CARTESIAN_POINT('Ctrl Pts',(-10.3325981443541,23.0660591492435,4.92523342956317));
#93469=CARTESIAN_POINT('Ctrl Pts',(-10.3412809074715,23.0655830201735,4.92317925832111));
#93470=CARTESIAN_POINT('Ctrl Pts',(-10.380609474594,23.0634327922,4.9134942679144));
#93471=CARTESIAN_POINT('Ctrl Pts',(-10.411023289227,23.0617879117006,4.90495183681221));
#93472=CARTESIAN_POINT('Ctrl Pts',(-10.4940180318713,23.057328341729,4.87871466943892));
#93473=CARTESIAN_POINT('Ctrl Pts',(-10.5459071062503,23.054574588893,4.85900479136008));
#93474=CARTESIAN_POINT('Ctrl Pts',(-10.6684754957301,23.0479992730299,4.80429140150898));
#93475=CARTESIAN_POINT('Ctrl Pts',(-10.73768422059,23.0442290290857,4.76643464969769));
#93476=CARTESIAN_POINT('Ctrl Pts',(-10.8155808967734,23.0395938933898,4.71526486194281));
#93477=CARTESIAN_POINT('Ctrl Pts',(-10.827535045466,23.0388706446855,4.70715641724224));
#93478=CARTESIAN_POINT('Ctrl Pts',(-10.8683403438949,23.0363535603659,4.67858739199002));
#93479=CARTESIAN_POINT('Ctrl Pts',(-10.8965666937535,23.0345276683949,4.65726011568945));
#93480=CARTESIAN_POINT('Ctrl Pts',(-10.928559106889,23.0323219576975,4.63121392287582));
#93481=CARTESIAN_POINT('Ctrl Pts',(-10.9331049844457,23.0320052058447,4.62746709041018));
#93482=CARTESIAN_POINT('Ctrl Pts',(-10.9404047329227,23.0314909290128,4.62137605932743));
#93483=CARTESIAN_POINT('Ctrl Pts',(-10.9431727981696,23.0312945919339,4.6190488820226));
#93484=CARTESIAN_POINT('Ctrl Pts',(-10.9480643389099,23.0309452277237,4.61490540735256));
#93485=CARTESIAN_POINT('Ctrl Pts',(-10.9501912697296,23.0307925013838,4.61309326153195));
#93486=CARTESIAN_POINT('Ctrl Pts',(-10.9523249508494,23.0306384595706,4.6112647921337));
#93487=CARTESIAN_POINT('Ctrl Pts',(-10.9523368681591,23.0306375991705,4.61125457919919));
#93488=CARTESIAN_POINT('Ctrl Pts',(-10.9523605487933,23.030635889436,4.61123428463221));
#93489=CARTESIAN_POINT('Ctrl Pts',(-10.952372312197,23.0306350400965,4.6112242029404));
#93490=CARTESIAN_POINT('Ctrl Pts',(-10.9523956883441,23.0306333522451,4.61120416803462));
#93491=CARTESIAN_POINT('Ctrl Pts',(-10.9524073009021,23.0306325137473,4.61119421498775));
#93492=CARTESIAN_POINT('Ctrl Pts',(-10.9524303776033,23.030630847419,4.61117443547197));
#93493=CARTESIAN_POINT('Ctrl Pts',(-10.952441841901,23.030630019578,4.6111646088786));
#93494=CARTESIAN_POINT('Ctrl Pts',(-10.9524646252504,23.0306283743365,4.61114507957735));
#93495=CARTESIAN_POINT('Ctrl Pts',(-10.9524759441808,23.0306275569454,4.61113537698118));
#93496=CARTESIAN_POINT('Ctrl Pts',(-10.9524984390757,23.0306259324406,4.61111609374318));
#93497=CARTESIAN_POINT('Ctrl Pts',(-10.9525096151478,23.0306251253199,4.61110651301652));
#93498=CARTESIAN_POINT('Ctrl Pts',(-10.9525318272815,23.0306235211443,4.61108747100626));
#93499=CARTESIAN_POINT('Ctrl Pts',(-10.9525428632257,23.0306227240985,4.61107800983062));
#93500=CARTESIAN_POINT('Ctrl Pts',(-10.9525647974261,23.0306211399068,4.61105920495296));
#93501=CARTESIAN_POINT('Ctrl Pts',(-10.9525756957366,23.0306203527576,4.61104986121145));
#93502=CARTESIAN_POINT('Ctrl Pts',(-10.9525973570583,23.0306187881881,4.6110312891753));
#93503=CARTESIAN_POINT('Ctrl Pts',(-10.9526081201667,23.0306180107613,4.61102206080415));
#93504=CARTESIAN_POINT('Ctrl Pts',(-10.9526295136086,23.0306164654561,4.61100371736456));
#93505=CARTESIAN_POINT('Ctrl Pts',(-10.9526401439421,23.0306156975781,4.61099460230281));
#93506=CARTESIAN_POINT('Ctrl Pts',(-10.9526612742903,23.0306141711946,4.610976483396));
#93507=CARTESIAN_POINT('Ctrl Pts',(-10.952671774227,23.0306134126952,4.61096747962417));
#93508=CARTESIAN_POINT('Ctrl Pts',(-10.9526926462581,23.0306119048913,4.61094958119281));
#93509=CARTESIAN_POINT('Ctrl Pts',(-10.9527030182358,23.0306111555959,4.61094068663956));
#93510=CARTESIAN_POINT('Ctrl Pts',(-10.9527236360655,23.0306096660773,4.61092300519182));
#93511=CARTESIAN_POINT('Ctrl Pts',(-10.9527338821429,23.0306089258385,4.61091421811006));
#93512=CARTESIAN_POINT('Ctrl Pts',(-10.952754250693,23.0306074542526,4.6108967494616));
#93513=CARTESIAN_POINT('Ctrl Pts',(-10.9527643731362,23.030606722908,4.6108880679259));
#93514=CARTESIAN_POINT('Ctrl Pts',(-10.9527844967566,23.0306052689432,4.61087080838141));
#93515=CARTESIAN_POINT('Ctrl Pts',(-10.9527944978278,23.0306045463309,4.61086223046907));
#93516=CARTESIAN_POINT('Ctrl Pts',(-10.9528143804219,23.0306031097078,4.61084517671488));
#93517=CARTESIAN_POINT('Ctrl Pts',(-10.952824262079,23.0306023956877,4.61083670076346));
#93518=CARTESIAN_POINT('Ctrl Pts',(-10.9552872847535,23.0304244202936,4.60872399598248));
#93519=CARTESIAN_POINT('Ctrl Pts',(-10.9577334242768,23.0302465630711,4.6066116677886));
#93520=CARTESIAN_POINT('Ctrl Pts',(-10.9644624545162,23.0297543014739,4.60076188872639));
#93521=CARTESIAN_POINT('Ctrl Pts',(-10.9687305510463,23.0294386978024,4.59700760213731));
#93522=CARTESIAN_POINT('Ctrl Pts',(-10.9783589302154,23.0287192670967,4.58843831708486));
#93523=CARTESIAN_POINT('Ctrl Pts',(-10.9837057091619,23.0283144419386,4.58360843484943));
#93524=CARTESIAN_POINT('Ctrl Pts',(-11.0004316116084,23.0270318297848,4.56827368950422));
#93525=CARTESIAN_POINT('Ctrl Pts',(-11.0116794744991,23.0261453330871,4.55762786019576));
#93526=CARTESIAN_POINT('Ctrl Pts',(-11.0567928968582,23.0224983913433,4.51355090731788));
#93527=CARTESIAN_POINT('Ctrl Pts',(-11.0891857827384,23.019665579348,4.47865747361497));
#93528=CARTESIAN_POINT('Ctrl Pts',(-11.1264843322814,23.0161883078593,4.43432995192514));
#93529=CARTESIAN_POINT('Ctrl Pts',(-11.1330649195315,23.0155659108045,4.42633865088414));
#93530=CARTESIAN_POINT('Ctrl Pts',(-11.2176150503767,23.0074571491648,4.32141407137539));
#93531=CARTESIAN_POINT('Ctrl Pts',(-11.2830167386506,22.9999901814597,4.21497307682452));
#93532=CARTESIAN_POINT('Ctrl Pts',(-11.3407058238333,22.9921532613856,4.08702074242542));
#93533=CARTESIAN_POINT('Ctrl Pts',(-11.3470093254799,22.9912727084644,4.07240838853835));
#93534=CARTESIAN_POINT('Ctrl Pts',(-11.3555040026487,22.9900504448996,4.05179872324019));
#93535=CARTESIAN_POINT('Ctrl Pts',(-11.3578960139323,22.9897020197334,4.04588583908946));
#93536=CARTESIAN_POINT('Ctrl Pts',(-11.3619793355063,22.9890996957697,4.03559922205542));
#93537=CARTESIAN_POINT('Ctrl Pts',(-11.3636884089891,22.988845206278,4.03123268057793));
#93538=CARTESIAN_POINT('Ctrl Pts',(-11.3672049856253,22.9883165102487,4.02211931159909));
#93539=CARTESIAN_POINT('Ctrl Pts',(-11.3690088246199,22.9880424284064,4.017371131079));
#93540=CARTESIAN_POINT('Ctrl Pts',(-11.3732135905657,22.9873965838185,4.00612710200566));
#93541=CARTESIAN_POINT('Ctrl Pts',(-11.375593213383,22.987025530078,3.99962338039434));
#93542=CARTESIAN_POINT('Ctrl Pts',(-11.3833476881162,22.9857974041388,3.97795427986121));
#93543=CARTESIAN_POINT('Ctrl Pts',(-11.3885187179659,22.9849470236355,3.96271688612295));
#93544=CARTESIAN_POINT('Ctrl Pts',(-11.4151157823096,22.9803905222009,3.87987914613787));
#93545=CARTESIAN_POINT('Ctrl Pts',(-11.4318592815955,22.9768388640165,3.81087190089729));
#93546=CARTESIAN_POINT('Ctrl Pts',(-11.4568229829728,22.9693929687705,3.66129315498171));
#93547=CARTESIAN_POINT('Ctrl Pts',(-11.4634999999988,22.9655328877089,3.58071335569824));
#93548=CARTESIAN_POINT('Ctrl Pts',(-11.4635,22.9615280277103,3.50000000002193));
#93549=CARTESIAN_POINT('Ctrl Pts',(-11.4635,22.8886966621701,3.49999999996283));
#93550=CARTESIAN_POINT('Ctrl Pts',(-11.4635000000021,22.8937025595212,3.58372973847256));
#93551=CARTESIAN_POINT('Ctrl Pts',(-11.4563143010388,22.898792645016,3.66731143336459));
#93552=CARTESIAN_POINT('Ctrl Pts',(-11.4314010571588,22.9074124895052,3.81111579450248));
#93553=CARTESIAN_POINT('Ctrl Pts',(-11.416884068329,22.9110010896834,3.87167606728241));
#93554=CARTESIAN_POINT('Ctrl Pts',(-11.3941261690681,22.9153060509761,3.94550022529331));
#93555=CARTESIAN_POINT('Ctrl Pts',(-11.3894765407924,22.9161366426632,3.95979690332411));
#93556=CARTESIAN_POINT('Ctrl Pts',(-11.3824241860813,22.9173292740733,3.98039676483398));
#93557=CARTESIAN_POINT('Ctrl Pts',(-11.3801969786291,22.9176970188189,3.98675865091151));
#93558=CARTESIAN_POINT('Ctrl Pts',(-11.3762244309044,22.9183377417142,3.99785948400651));
#93559=CARTESIAN_POINT('Ctrl Pts',(-11.3744983783646,22.9186113488688,4.00260517187402));
#93560=CARTESIAN_POINT('Ctrl Pts',(-11.3711050989067,22.9191401297543,4.01178658799793));
#93561=CARTESIAN_POINT('Ctrl Pts',(-11.3694408252204,22.9193953969098,4.01622333427418));
#93562=CARTESIAN_POINT('Ctrl Pts',(-11.3654188835486,22.9200027142629,4.02678899305744));
#93563=CARTESIAN_POINT('Ctrl Pts',(-11.3630414448596,22.9203541049237,4.03291030414066));
#93564=CARTESIAN_POINT('Ctrl Pts',(-11.3543464020176,22.9216125518846,4.05485897650305));
#93565=CARTESIAN_POINT('Ctrl Pts',(-11.3477935325393,22.9225117750562,4.07059204865107));
#93566=CARTESIAN_POINT('Ctrl Pts',(-11.2983203266025,22.928966640721,4.18376348041435));
#93567=CARTESIAN_POINT('Ctrl Pts',(-11.2451555538814,22.9341445989993,4.27637522888001));
#93568=CARTESIAN_POINT('Ctrl Pts',(-11.1498840933806,22.9420052592637,4.4069978113952));
#93569=CARTESIAN_POINT('Ctrl Pts',(-11.1148654046305,22.9446886973284,4.44971208895779));
#93570=CARTESIAN_POINT('Ctrl Pts',(-11.0589617407059,22.9488378641672,4.51053669669999));
#93571=CARTESIAN_POINT('Ctrl Pts',(-11.0398403248026,22.9502365251758,4.53020208144455));
#93572=CARTESIAN_POINT('Ctrl Pts',(-11.0124641018614,22.9522303927913,4.55681808551152));
#93573=CARTESIAN_POINT('Ctrl Pts',(-11.0046671313447,22.9527973437842,4.56423304133091));
#93574=CARTESIAN_POINT('Ctrl Pts',(-10.9910419749323,22.9537879835973,4.57690745605331));
#93575=CARTESIAN_POINT('Ctrl Pts',(-10.9852518351393,22.9542089340998,4.58220731881851));
#93576=CARTESIAN_POINT('Ctrl Pts',(-10.9766817943306,22.9548324280526,4.58992591357902));
#93577=CARTESIAN_POINT('Ctrl Pts',(-10.9739348474169,22.9550323416452,4.59238122322338));
#93578=CARTESIAN_POINT('Ctrl Pts',(-10.9690745550257,22.9553862333389,4.59669260414874));
#93579=CARTESIAN_POINT('Ctrl Pts',(-10.9669650640809,22.9555398906743,4.59855301463682));
#93580=CARTESIAN_POINT('Ctrl Pts',(-10.9624988818325,22.9558653591276,4.60246901622453));
#93581=CARTESIAN_POINT('Ctrl Pts',(-10.960140971205,22.956037270746,4.60452312981589));
#93582=CARTESIAN_POINT('Ctrl Pts',(-10.9537808184027,22.9565011535274,4.61002807476317));
#93583=CARTESIAN_POINT('Ctrl Pts',(-10.9497664783668,22.9567941266349,4.6134647776789));
#93584=CARTESIAN_POINT('Ctrl Pts',(-10.9317473009013,22.9581096626698,4.62872277220361));
#93585=CARTESIAN_POINT('Ctrl Pts',(-10.9175403451224,22.9591481170951,4.64030161814578));
#93586=CARTESIAN_POINT('Ctrl Pts',(-10.8081182811567,22.9671313530352,4.72611304263082));
#93587=CARTESIAN_POINT('Ctrl Pts',(-10.7042644820556,22.9745793570156,4.7885730893246));
#93588=CARTESIAN_POINT('Ctrl Pts',(-10.5256988943206,22.9861673048739,4.86786127589499));
#93589=CARTESIAN_POINT('Ctrl Pts',(-10.4552545788374,22.9904783766083,4.8928925797401));
#93590=CARTESIAN_POINT('Ctrl Pts',(-10.3723341030013,22.9952342074735,4.91538909561249));
#93591=CARTESIAN_POINT('Ctrl Pts',(-10.3614357189462,22.9958533128884,4.91821127031986));
#93592=CARTESIAN_POINT('Ctrl Pts',(-10.3446777466164,22.9967963603612,4.92234508190429));
#93593=CARTESIAN_POINT('Ctrl Pts',(-10.3388410070031,22.9971231712414,4.92374683652096));
#93594=CARTESIAN_POINT('Ctrl Pts',(-10.32862703471,22.997692238648,4.92613346140754));
#93595=CARTESIAN_POINT('Ctrl Pts',(-10.3242536186214,22.9979349973668,4.92713418048937));
#93596=CARTESIAN_POINT('Ctrl Pts',(-10.3143656882362,22.9984818413064,4.9293489240532));
#93597=CARTESIAN_POINT('Ctrl Pts',(-10.3088485925227,22.9987855491592,4.93055118075345));
#93598=CARTESIAN_POINT('Ctrl Pts',(-10.2939253890208,22.99960331623,4.93371281177883));
#93599=CARTESIAN_POINT('Ctrl Pts',(-10.2845066281513,23.0001154517433,4.93561155798408));
#93600=CARTESIAN_POINT('Ctrl Pts',(-10.2409877083828,23.0024640725947,4.94393950485668));
#93601=CARTESIAN_POINT('Ctrl Pts',(-10.2066830320024,23.0042651577015,4.94924764659064));
#93602=CARTESIAN_POINT('Ctrl Pts',(-10.04503497652,23.0125666405154,4.96840298399521));
#93603=CARTESIAN_POINT('Ctrl Pts',(-9.91643235842142,23.0185796574468,4.96671403208011));
#93604=CARTESIAN_POINT('Ctrl Pts',(-9.74332276811312,23.0272642201687,4.94157714298139));
#93605=CARTESIAN_POINT('Ctrl Pts',(-9.69730572637098,23.0296385340975,4.93262112164391));
#93606=CARTESIAN_POINT('Ctrl Pts',(-9.64235249806421,23.0326362372217,4.91916001955848));
#93607=CARTESIAN_POINT('Ctrl Pts',(-9.63292677333581,23.0331562884835,4.91675126006371));
#93608=CARTESIAN_POINT('Ctrl Pts',(-9.61966856185606,23.0338969890205,4.9132219151892));
#93609=CARTESIAN_POINT('Ctrl Pts',(-9.61581536835474,23.0341133575106,4.91217929189465));
#93610=CARTESIAN_POINT('Ctrl Pts',(-9.60921826350841,23.034485768747,4.91036520396044));
#93611=CARTESIAN_POINT('Ctrl Pts',(-9.60647221986265,23.0346413701986,4.90960145441706));
#93612=CARTESIAN_POINT('Ctrl Pts',(-9.60116848789708,23.0349430600413,4.90810963589697));
#93613=CARTESIAN_POINT('Ctrl Pts',(-9.59861053932601,23.0350890828149,4.9073826140669));
#93614=CARTESIAN_POINT('Ctrl Pts',(-9.59245311847913,23.0354418142173,4.90561439581743));
#93615=CARTESIAN_POINT('Ctrl Pts',(-9.58885565505423,23.0356489111278,4.90456634494435));
#93616=CARTESIAN_POINT('Ctrl Pts',(-9.57563869390418,23.0364134089598,4.90066071293694));
#93617=CARTESIAN_POINT('Ctrl Pts',(-9.56604486210916,23.0369754242256,4.89771809669462));
#93618=CARTESIAN_POINT('Ctrl Pts',(-9.45263613124677,23.0436969931857,4.86165327913227));
#93619=CARTESIAN_POINT('Ctrl Pts',(-9.35280981319758,23.0503644264584,4.81713677057715));
#93620=CARTESIAN_POINT('Ctrl Pts',(-9.17835442233576,23.0624946045419,4.71467955693113));
#93621=CARTESIAN_POINT('Ctrl Pts',(-9.10255141115444,23.0679677192448,4.65980123022178));
#93622=CARTESIAN_POINT('Ctrl Pts',(-9.02233695720921,23.0739101339972,4.58912357607396));
#93623=CARTESIAN_POINT('Ctrl Pts',(-9.01231297860954,23.0746561527892,4.58004145950308));
#93624=CARTESIAN_POINT('Ctrl Pts',(-8.99768966560636,23.0757498810816,4.56641829068668));
#93625=CARTESIAN_POINT('Ctrl Pts',(-8.99299238323127,23.0761020547853,4.56198382228049));
#93626=CARTESIAN_POINT('Ctrl Pts',(-8.98470480512746,23.0767249750428,4.55405550668758));
#93627=CARTESIAN_POINT('Ctrl Pts',(-8.9811028212063,23.0769962459546,4.55057407345802));
#93628=CARTESIAN_POINT('Ctrl Pts',(-8.97357251969335,23.0775645278476,4.54322063832996));
#93629=CARTESIAN_POINT('Ctrl Pts',(-8.96964806754071,23.0778613652198,4.53934477868884));
#93630=CARTESIAN_POINT('Ctrl Pts',(-8.95936711718237,23.0786408478511,4.5290756673897));
#93631=CARTESIAN_POINT('Ctrl Pts',(-8.9530475644933,23.0791218730946,4.52264565158095));
#93632=CARTESIAN_POINT('Ctrl Pts',(-8.92658804141508,23.0811444863814,4.49522126822913));
#93633=CARTESIAN_POINT('Ctrl Pts',(-8.90701631609068,23.0826617805098,4.4736865113541));
#93634=CARTESIAN_POINT('Ctrl Pts',(-8.78620872849108,23.0922042776851,4.3325256048145));
#93635=CARTESIAN_POINT('Ctrl Pts',(-8.70411667639938,23.0993937177774,4.19790032297425));
#93636=CARTESIAN_POINT('Ctrl Pts',(-8.63326035128343,23.1089395912479,4.02422319550739));
#93637=CARTESIAN_POINT('Ctrl Pts',(-8.6224968793901,23.1105447258081,3.99524954553582));
#93638=CARTESIAN_POINT('Ctrl Pts',(-8.61076019305092,23.1125193610057,3.96030488296422));
#93639=CARTESIAN_POINT('Ctrl Pts',(-8.60889575873792,23.1128407114197,3.95463921298278));
#93640=CARTESIAN_POINT('Ctrl Pts',(-8.60606090231911,23.1133416489456,3.94584389348931));
#93641=CARTESIAN_POINT('Ctrl Pts',(-8.60506624805134,23.113519857383,3.94272204897525));
#93642=CARTESIAN_POINT('Ctrl Pts',(-8.60324498437891,23.1138507859955,3.93693871783368));
#93643=CARTESIAN_POINT('Ctrl Pts',(-8.60241548904494,23.1140033367239,3.93427819559775));
#93644=CARTESIAN_POINT('Ctrl Pts',(-8.60055563392569,23.1143495508551,3.92825238231057));
#93645=CARTESIAN_POINT('Ctrl Pts',(-8.59952981660688,23.1145434715495,3.92488575121337));
#93646=CARTESIAN_POINT('Ctrl Pts',(-8.59646225404224,23.115132367723,3.91468650715257));
#93647=CARTESIAN_POINT('Ctrl Pts',(-8.59445832679202,23.1155294336795,3.90784274445678));
#93648=CARTESIAN_POINT('Ctrl Pts',(-8.5780749033127,23.1188803246379,3.85033533551735));
#93649=CARTESIAN_POINT('Ctrl Pts',(-8.56639109989419,23.1219668345176,3.79894860190357));
#93650=CARTESIAN_POINT('Ctrl Pts',(-8.54476688026983,23.1296003436141,3.67268707318201));
#93651=CARTESIAN_POINT('Ctrl Pts',(-8.53780028193211,23.1341854447125,3.5974506706282));
#93652=CARTESIAN_POINT('Ctrl Pts',(-8.53543170949651,23.1435669509989,3.43998488473847));
#93653=CARTESIAN_POINT('Ctrl Pts',(-8.54109664249258,23.1483274520173,3.3579908879184));
#93654=CARTESIAN_POINT('Ctrl Pts',(-8.5553496851577,23.153504476523,3.26558894905294));
#93655=CARTESIAN_POINT('Ctrl Pts',(-8.55722583930858,23.1541336650272,3.25430546472472));
#93656=CARTESIAN_POINT('Ctrl Pts',(-8.56029467594815,23.155088782984,3.23709827487902));
#93657=CARTESIAN_POINT('Ctrl Pts',(-8.56139205137798,23.1554176963114,3.23115820848394));
#93658=CARTESIAN_POINT('Ctrl Pts',(-8.56345965032266,23.15601521438,3.2203416501542));
#93659=CARTESIAN_POINT('Ctrl Pts',(-8.564418003776,23.1562841890715,3.21546300442164));
#93660=CARTESIAN_POINT('Ctrl Pts',(-8.56654651970561,23.1568647908666,3.20491202504406));
#93661=CARTESIAN_POINT('Ctrl Pts',(-8.56772553304102,23.1571761331146,3.1992415491617));
#93662=CARTESIAN_POINT('Ctrl Pts',(-8.57103193634381,23.1580221573305,3.18379987053516));
#93663=CARTESIAN_POINT('Ctrl Pts',(-8.57322588391218,23.1585547249872,3.17404313608866));
#93664=CARTESIAN_POINT('Ctrl Pts',(-8.58482358974776,23.1612318870614,3.12482904463172));
#93665=CARTESIAN_POINT('Ctrl Pts',(-8.59576523049385,23.1633270905225,3.08575054272287));
#93666=CARTESIAN_POINT('Ctrl Pts',(-8.61254634397472,23.1660742408351,3.03417660266031));
#93667=CARTESIAN_POINT('Ctrl Pts',(-8.61695758629698,23.1667619419361,3.0212382859478));
#93668=CARTESIAN_POINT('Ctrl Pts',(-8.66562409351874,23.1740083561033,2.88478713744418));
#93669=CARTESIAN_POINT('Ctrl Pts',(-8.72610938857207,23.1801112962626,2.76771424503984));
#93670=CARTESIAN_POINT('Ctrl Pts',(-8.81814092906498,23.1882947743067,2.63634779226111));
#93671=CARTESIAN_POINT('Ctrl Pts',(-8.83561790402756,23.1898154654618,2.61292609910041));
#93672=CARTESIAN_POINT('Ctrl Pts',(-8.85743437493096,23.1916956019755,2.58544517265444));
#93673=CARTESIAN_POINT('Ctrl Pts',(-8.86111347779629,23.1920120800991,2.58086767709557));
#93674=CARTESIAN_POINT('Ctrl Pts',(-8.86687537430508,23.1925070332029,2.57378650510597));
#93675=CARTESIAN_POINT('Ctrl Pts',(-8.86893918489258,23.1926841816826,2.5712673756213));
#93676=CARTESIAN_POINT('Ctrl Pts',(-8.87278592585717,23.1930141633791,2.56660380409002));
#93677=CARTESIAN_POINT('Ctrl Pts',(-8.87456658697335,23.1931668352226,2.56445755845141));
#93678=CARTESIAN_POINT('Ctrl Pts',(-8.87862539302519,23.1935146517819,2.55959380290808));
#93679=CARTESIAN_POINT('Ctrl Pts',(-8.8809072773608,23.1937100640358,2.5568794868701));
#93680=CARTESIAN_POINT('Ctrl Pts',(-8.88789408781464,23.1943079147478,2.54862968924078));
#93681=CARTESIAN_POINT('Ctrl Pts',(-8.89263031313694,23.1947125359804,2.54312101063837));
#93682=CARTESIAN_POINT('Ctrl Pts',(-8.94549683050246,23.1992195995307,2.48255041388535));
#93683=CARTESIAN_POINT('Ctrl Pts',(-8.99764396342708,23.2035754572301,2.43114044228027));
#93684=CARTESIAN_POINT('Ctrl Pts',(-9.07353880045009,23.2095576035611,2.36677510817375));
#93685=CARTESIAN_POINT('Ctrl Pts',(-9.09412830144786,23.2111490737651,2.35024982149241));
#93686=CARTESIAN_POINT('Ctrl Pts',(-9.19263068806143,23.2185898359108,2.2754803390266));
#93687=CARTESIAN_POINT('Ctrl Pts',(-9.2757883655974,23.2243576161389,2.22453289374682));
#93688=CARTESIAN_POINT('Ctrl Pts',(-9.3818036026017,23.2309735749948,2.17331868716748));
#93689=CARTESIAN_POINT('Ctrl Pts',(-9.40039446825325,23.2321092748022,2.16481336237043));
#93690=CARTESIAN_POINT('Ctrl Pts',(-9.42614515125295,23.2336497577142,2.15367878683996));
#93691=CARTESIAN_POINT('Ctrl Pts',(-9.43315575341989,23.2340658949496,2.15071211388196));
#93692=CARTESIAN_POINT('Ctrl Pts',(-9.4450052236418,23.2347638656202,2.14580643304056));
#93693=CARTESIAN_POINT('Ctrl Pts',(-9.44983182920665,23.2350466719247,2.14383835646204));
#93694=CARTESIAN_POINT('Ctrl Pts',(-9.45939922417467,23.2356043393218,2.13999667831226));
#93695=CARTESIAN_POINT('Ctrl Pts',(-9.46413949001787,23.2358792341282,2.13812197735152));
#93696=CARTESIAN_POINT('Ctrl Pts',(-9.47462018360812,23.2364839675119,2.13404022004967));
#93697=CARTESIAN_POINT('Ctrl Pts',(-9.48036494081066,23.2368134259113,2.13184449760066));
#93698=CARTESIAN_POINT('Ctrl Pts',(-9.50068342966843,23.2379717275707,2.12422493887533));
#93699=CARTESIAN_POINT('Ctrl Pts',(-9.51532987442783,23.23879410264,2.11899712164681));
#93700=CARTESIAN_POINT('Ctrl Pts',(-9.65370638310688,23.2464532233741,2.07207850194481));
#93701=CARTESIAN_POINT('Ctrl Pts',(-9.78240355481591,23.2526822643321,2.04688860198743));
#93702=CARTESIAN_POINT('Ctrl Pts',(-9.96415333620947,23.2615825051734,2.03603284564221));
#93703=CARTESIAN_POINT('Ctrl Pts',(-10.0156877715751,23.2641269927053,2.03567831213103));
#93704=CARTESIAN_POINT('Ctrl Pts',(-10.0915514969956,23.2680315690132,2.03916179875368));
#93705=CARTESIAN_POINT('Ctrl Pts',(-10.1159398593617,23.2693112864002,2.04089488504383));
#93706=CARTESIAN_POINT('Ctrl Pts',(-10.145818416135,23.270921379738,2.04377189677918));
#93707=CARTESIAN_POINT('Ctrl Pts',(-10.1513617485163,23.2712218929209,2.04433763593095));
#93708=CARTESIAN_POINT('Ctrl Pts',(-10.1600740725861,23.2716972123874,2.04527709761038));
#93709=CARTESIAN_POINT('Ctrl Pts',(-10.1632453621957,23.2718708569266,2.04562955792767));
#93710=CARTESIAN_POINT('Ctrl Pts',(-10.1691954680698,23.272197877064,2.04631056502229));
#93711=CARTESIAN_POINT('Ctrl Pts',(-10.1719745083046,23.272351118643,2.04663671168225));
#93712=CARTESIAN_POINT('Ctrl Pts',(-10.1783113306848,23.27270168243,2.04739882720235));
#93713=CARTESIAN_POINT('Ctrl Pts',(-10.1818684540578,23.2728992853135,2.04783989769752));
#93714=CARTESIAN_POINT('Ctrl Pts',(-10.1912872534378,23.2734246112179,2.04904294457913));
#93715=CARTESIAN_POINT('Ctrl Pts',(-10.1971459335241,23.273753530381,2.04982736596946));
#93716=CARTESIAN_POINT('Ctrl Pts',(-10.2383244312395,23.2760797878145,2.05559491874596));
#93717=CARTESIAN_POINT('Ctrl Pts',(-10.2734539078621,23.2781387538969,2.06183202253101));
#93718=CARTESIAN_POINT('Ctrl Pts',(-10.4085024221498,23.2862558521334,2.09093605699013));
#93719=CARTESIAN_POINT('Ctrl Pts',(-10.5061423467224,23.2925346786565,2.12299002641057));
#93720=CARTESIAN_POINT('Ctrl Pts',(-10.660326143257,23.3025508771655,2.19224308173794));
#93721=CARTESIAN_POINT('Ctrl Pts',(-10.7190932462435,23.3064014513024,2.22361230993027));
#93722=CARTESIAN_POINT('Ctrl Pts',(-10.7887312887505,23.3109814397479,2.26712628202359));
#93723=CARTESIAN_POINT('Ctrl Pts',(-10.8018026320707,23.3118421992046,2.27558699130427));
#93724=CARTESIAN_POINT('Ctrl Pts',(-10.8204155682214,23.3130698289545,2.28806053118212));
#93725=CARTESIAN_POINT('Ctrl Pts',(-10.8260676241583,23.3134428811942,2.29190593776933));
#93726=CARTESIAN_POINT('Ctrl Pts',(-10.835860499199,23.3140897669519,2.29866943204233));
#93727=CARTESIAN_POINT('Ctrl Pts',(-10.8400134639367,23.3143642656683,2.30156965620346));
#93728=CARTESIAN_POINT('Ctrl Pts',(-10.8480012681559,23.3148925924222,2.30720986285703));
#93729=CARTESIAN_POINT('Ctrl Pts',(-10.8518380884348,23.3151465266012,2.30994691972722));
#93730=CARTESIAN_POINT('Ctrl Pts',(-10.8609089566859,23.3157472865384,2.31648411365783));
#93731=CARTESIAN_POINT('Ctrl Pts',(-10.8661311905898,23.3160934858749,2.32030052664382));
#93732=CARTESIAN_POINT('Ctrl Pts',(-10.8845340134632,23.3173148126791,2.33393739798975));
#93733=CARTESIAN_POINT('Ctrl Pts',(-10.8975745496082,23.3181827069297,2.34394534326842));
#93734=CARTESIAN_POINT('Ctrl Pts',(-11.0031424200493,23.3252363004946,2.42782666700192));
#93735=CARTESIAN_POINT('Ctrl Pts',(-11.0865593042528,23.3309396058576,2.51245668811158));
#93736=CARTESIAN_POINT('Ctrl Pts',(-11.1951585539255,23.3395999948395,2.65326607584663));
#93737=CARTESIAN_POINT('Ctrl Pts',(-11.2285427195277,23.3425110075756,2.70247624563452));
#93738=CARTESIAN_POINT('Ctrl Pts',(-11.2724213116506,23.346918352538,2.77647724425439));
#93739=CARTESIAN_POINT('Ctrl Pts',(-11.2853727386823,23.3483083789709,2.79974439065669));
#93740=CARTESIAN_POINT('Ctrl Pts',(-11.3003250413342,23.3500421914841,2.82841997754414));
#93741=CARTESIAN_POINT('Ctrl Pts',(-11.3029387490456,23.3503504234604,2.83350502346331));
#93742=CARTESIAN_POINT('Ctrl Pts',(-11.3069789939376,23.3508352397599,2.84148003410413));
#93743=CARTESIAN_POINT('Ctrl Pts',(-11.3084259237483,23.3510105838645,2.84435967350196));
#93744=CARTESIAN_POINT('Ctrl Pts',(-11.3111090656648,23.3513390057636,2.8497438436725));
#93745=CARTESIAN_POINT('Ctrl Pts',(-11.3123476259413,23.3514919361305,2.85224714653069));
#93746=CARTESIAN_POINT('Ctrl Pts',(-11.3151638807789,23.3518427170639,2.85798042204626));
#93747=CARTESIAN_POINT('Ctrl Pts',(-11.3167368412838,23.3520408538252,2.86121266291609));
#93748=CARTESIAN_POINT('Ctrl Pts',(-11.3208237956901,23.3525614423942,2.86969008969881));
#93749=CARTESIAN_POINT('Ctrl Pts',(-11.3233184303534,23.3528850273899,2.87494447296516));
#93750=CARTESIAN_POINT('Ctrl Pts',(-11.340110509812,23.3551026467678,2.91086431059281));
#93751=CARTESIAN_POINT('Ctrl Pts',(-11.3533710994117,23.3570521853978,2.94200057623519));
#93752=CARTESIAN_POINT('Ctrl Pts',(-11.398714046218,23.3644439404849,3.05961754847301));
#93753=CARTESIAN_POINT('Ctrl Pts',(-11.4236795437323,23.370076016115,3.14861095853915));
#93754=CARTESIAN_POINT('Ctrl Pts',(-11.4552606781815,23.3806568484099,3.32310607387804));
#93755=CARTESIAN_POINT('Ctrl Pts',(-11.4630854948338,23.3856051615986,3.40802267691719));
#93756=CARTESIAN_POINT('Ctrl Pts',(-11.463494655631,23.3904459116752,3.49543302098015));
#93757=CARTESIAN_POINT('Ctrl Pts',(-11.4635,23.3905722042834,3.49771651079369));
#93758=CARTESIAN_POINT('Ctrl Pts',(-11.4635,23.3906983315425,3.49999999997929));
#93759=CARTESIAN_POINT('Origin',(-10.,13.2,3.5));
#93760=CARTESIAN_POINT('',(-11.4635,23.9605564584951,3.50000000010085));
#93761=CARTESIAN_POINT('',(-11.4635,23.8891760003868,3.49999987117833));
#93762=CARTESIAN_POINT('',(-11.4635,13.2,3.5));
#93763=CARTESIAN_POINT('Ctrl Pts',(-11.4635,23.9605564584951,3.50000000010084));
#93764=CARTESIAN_POINT('Ctrl Pts',(-11.4635000000071,23.9543681829968,3.39710918915123));
#93765=CARTESIAN_POINT('Ctrl Pts',(-11.4526495736673,23.9482887247367,3.29448451306187));
#93766=CARTESIAN_POINT('Ctrl Pts',(-11.4289758303516,23.9419849953737,3.18382767216033));
#93767=CARTESIAN_POINT('Ctrl Pts',(-11.4267312326161,23.9414185100086,3.17384840647046));
#93768=CARTESIAN_POINT('Ctrl Pts',(-11.4223784615672,23.94037494965,3.15540185477534));
#93769=CARTESIAN_POINT('Ctrl Pts',(-11.4202988392615,23.9398969951479,3.14692836216495));
#93770=CARTESIAN_POINT('Ctrl Pts',(-11.4167970973129,23.9391243851414,3.13319222553145));
#93771=CARTESIAN_POINT('Ctrl Pts',(-11.4154211517208,23.9388282616594,3.12791812359778));
#93772=CARTESIAN_POINT('Ctrl Pts',(-11.4127198823064,23.9382609023692,3.11779580862157));
#93773=CARTESIAN_POINT('Ctrl Pts',(-11.4113989870901,23.9379895291454,3.11294650255681));
#93774=CARTESIAN_POINT('Ctrl Pts',(-11.4083180880955,23.9373701393845,3.10186133744637));
#93775=CARTESIAN_POINT('Ctrl Pts',(-11.4065415932648,23.9370226588313,3.09563014438016));
#93776=CARTESIAN_POINT('Ctrl Pts',(-11.4017091642415,23.9361024318987,3.07909724664258));
#93777=CARTESIAN_POINT('Ctrl Pts',(-11.3985810276646,23.9355320170316,3.06881694592079));
#93778=CARTESIAN_POINT('Ctrl Pts',(-11.3683197729957,23.9302390896538,2.97316211450145));
#93779=CARTESIAN_POINT('Ctrl Pts',(-11.3335141095995,23.9257856365212,2.89041003346788));
#93780=CARTESIAN_POINT('Ctrl Pts',(-11.268148401827,23.9190034737887,2.76783603669243));
#93781=CARTESIAN_POINT('Ctrl Pts',(-11.2427577025094,23.9166204217943,2.72552103708051));
#93782=CARTESIAN_POINT('Ctrl Pts',(-11.1879708728508,23.9118069157457,2.6438693574715));
#93783=CARTESIAN_POINT('Ctrl Pts',(-11.1586365462398,23.9093796434825,2.60456982203685));
#93784=CARTESIAN_POINT('Ctrl Pts',(-11.1120687876538,23.9056223175329,2.54831071531222));
#93785=CARTESIAN_POINT('Ctrl Pts',(-11.0962965693742,23.9043641129525,2.53018394403956));
#93786=CARTESIAN_POINT('Ctrl Pts',(-11.0763297883332,23.9027768838485,2.50834611468825));
#93787=CARTESIAN_POINT('Ctrl Pts',(-11.0725499173417,23.9024766451298,2.50425911286629));
#93788=CARTESIAN_POINT('Ctrl Pts',(-11.0665681319396,23.9020016897821,2.49786485888969));
#93789=CARTESIAN_POINT('Ctrl Pts',(-11.0643817961627,23.9018281321982,2.49554302595069));
#93790=CARTESIAN_POINT('Ctrl Pts',(-11.0602634672969,23.901501236911,2.49119800961621));
#93791=CARTESIAN_POINT('Ctrl Pts',(-11.0583332532581,23.9013480328503,2.48917320945137));
#93792=CARTESIAN_POINT('Ctrl Pts',(-11.0539165423878,23.9009975016114,2.48456658507592));
#93793=CARTESIAN_POINT('Ctrl Pts',(-11.0514263604299,23.9007998935227,2.48198835640601));
#93794=CARTESIAN_POINT('Ctrl Pts',(-11.0448030808621,23.9002744343683,2.47518111874148));
#93795=CARTESIAN_POINT('Ctrl Pts',(-11.0406538238061,23.8999453857695,2.47096801130838));
#93796=CARTESIAN_POINT('Ctrl Pts',(-11.0112631148531,23.8976163207678,2.44148458460281));
#93797=CARTESIAN_POINT('Ctrl Pts',(-10.9851313347235,23.8955545144942,2.41712243448815));
#93798=CARTESIAN_POINT('Ctrl Pts',(-10.9516079953416,23.8929486140665,2.38808764837277));
#93799=CARTESIAN_POINT('Ctrl Pts',(-10.945029156253,23.8924389852871,2.3824908302785));
#93800=CARTESIAN_POINT('Ctrl Pts',(-10.9300655200673,23.8912844629442,2.36998744393083));
#93801=CARTESIAN_POINT('Ctrl Pts',(-10.9216526079498,23.8906385863462,2.36311534771559));
#93802=CARTESIAN_POINT('Ctrl Pts',(-10.8505180829529,23.8852088966488,2.30631755868577));
#93803=CARTESIAN_POINT('Ctrl Pts',(-10.783864896324,23.8803336605694,2.26152701696299));
#93804=CARTESIAN_POINT('Ctrl Pts',(-10.6695503925618,23.8725606869711,2.19765091602785));
#93805=CARTESIAN_POINT('Ctrl Pts',(-10.6239593197965,23.869595982601,2.17520326217796));
#93806=CARTESIAN_POINT('Ctrl Pts',(-10.5591810452508,23.8655852121357,2.14739615300045));
#93807=CARTESIAN_POINT('Ctrl Pts',(-10.540916454845,23.864475482809,2.13998895244032));
#93808=CARTESIAN_POINT('Ctrl Pts',(-10.5089105420873,23.8625670785485,2.12775578471672));
#93809=CARTESIAN_POINT('Ctrl Pts',(-10.4952367888932,23.8617630256511,2.12276194117572));
#93810=CARTESIAN_POINT('Ctrl Pts',(-10.4751219633236,23.8605962847328,2.11575404988019));
#93811=CARTESIAN_POINT('Ctrl Pts',(-10.4687381433734,23.8602283391433,2.11357932591354));
#93812=CARTESIAN_POINT('Ctrl Pts',(-10.4575490668385,23.859587458352,2.10985375112556));
#93813=CARTESIAN_POINT('Ctrl Pts',(-10.4527504275493,23.8593138923398,2.10828350837317));
#93814=CARTESIAN_POINT('Ctrl Pts',(-10.4434357432137,23.8587853290166,2.10528877036745));
#93815=CARTESIAN_POINT('Ctrl Pts',(-10.4389207268927,23.8585302375357,2.103861300353));
#93816=CARTESIAN_POINT('Ctrl Pts',(-10.4281364282006,23.8579235567038,2.10050921564819));
#93817=CARTESIAN_POINT('Ctrl Pts',(-10.4218609509691,23.8575726242696,2.09860476788857));
#93818=CARTESIAN_POINT('Ctrl Pts',(-10.3992776116565,23.8563170970655,2.09191674222341));
#93819=CARTESIAN_POINT('Ctrl Pts',(-10.3828991694546,23.8554202888611,2.08737502158141));
#93820=CARTESIAN_POINT('Ctrl Pts',(-10.2620452711281,23.8488960549862,2.05611882857454));
#93821=CARTESIAN_POINT('Ctrl Pts',(-10.154981120853,23.8436574592109,2.04073850806824));
#93822=CARTESIAN_POINT('Ctrl Pts',(-9.98016220777543,23.8351526879851,2.03509859552735));
#93823=CARTESIAN_POINT('Ctrl Pts',(-9.91306939801964,23.831890922504,2.03754606693212));
#93824=CARTESIAN_POINT('Ctrl Pts',(-9.81802562915411,23.8270095240859,2.04757758899404));
#93825=CARTESIAN_POINT('Ctrl Pts',(-9.78976044708354,23.8255240700692,2.05139907207021));
#93826=CARTESIAN_POINT('Ctrl Pts',(-9.75587362331828,23.823683452169,2.05699322101328));
#93827=CARTESIAN_POINT('Ctrl Pts',(-9.75012619362705,23.8233691866638,2.05797734740935));
#93828=CARTESIAN_POINT('Ctrl Pts',(-9.74118797866969,23.8228769914377,2.05956286860933));
#93829=CARTESIAN_POINT('Ctrl Pts',(-9.73799298892843,23.8227003651004,2.06014059102847));
#93830=CARTESIAN_POINT('Ctrl Pts',(-9.73205741570793,23.8223709064475,2.061234279476));
#93831=CARTESIAN_POINT('Ctrl Pts',(-9.72931637027296,23.8222182318842,2.06174744942576));
#93832=CARTESIAN_POINT('Ctrl Pts',(-9.723082825866,23.8218698261695,2.06293292497623));
#93833=CARTESIAN_POINT('Ctrl Pts',(-9.71959131403065,23.821673823124,2.06361012683548));
#93834=CARTESIAN_POINT('Ctrl Pts',(-9.71051812246244,23.8211623185226,2.06540427456578));
#93835=CARTESIAN_POINT('Ctrl Pts',(-9.70494048355168,23.8208457450908,2.06654106007386));
#93836=CARTESIAN_POINT('Ctrl Pts',(-9.66864891163044,23.8187726569218,2.07415847573261));
#93837=CARTESIAN_POINT('Ctrl Pts',(-9.63814565524022,23.8169683362648,2.08159288504689));
#93838=CARTESIAN_POINT('Ctrl Pts',(-9.50726099412317,23.8090242467858,2.11798931742116));
#93839=CARTESIAN_POINT('Ctrl Pts',(-9.40990128364166,23.8026185679344,2.15667220869621));
#93840=CARTESIAN_POINT('Ctrl Pts',(-9.27257190836735,23.7934035067501,2.22907167012974));
#93841=CARTESIAN_POINT('Ctrl Pts',(-9.22891546086121,23.790439049915,2.25507436120165));
#93842=CARTESIAN_POINT('Ctrl Pts',(-9.16195781472005,23.7858567824691,2.2998321136181));
#93843=CARTESIAN_POINT('Ctrl Pts',(-9.13772875301896,23.784190281127,2.31711955879814));
#93844=CARTESIAN_POINT('Ctrl Pts',(-9.10708496483639,23.7820703967399,2.34042620113659));
#93845=CARTESIAN_POINT('Ctrl Pts',(-9.10017505672099,23.7815915333914,2.34578003346862));
#93846=CARTESIAN_POINT('Ctrl Pts',(-9.08903231448923,23.7808178380375,2.35457437152227));
#93847=CARTESIAN_POINT('Ctrl Pts',(-9.08477008812104,23.7805215300343,2.35797714386127));
#93848=CARTESIAN_POINT('Ctrl Pts',(-9.07661806556957,23.7799540711631,2.36456030689361));
#93849=CARTESIAN_POINT('Ctrl Pts',(-9.07272543721932,23.7796827812032,2.36773705368233));
#93850=CARTESIAN_POINT('Ctrl Pts',(-9.06385714376911,23.7790639320408,2.37505081307066));
#93851=CARTESIAN_POINT('Ctrl Pts',(-9.05889238209177,23.7787169058427,2.37920092175541));
#93852=CARTESIAN_POINT('Ctrl Pts',(-9.04577864055623,23.777798635608,2.3903114421323));
#93853=CARTESIAN_POINT('Ctrl Pts',(-9.03767822866114,23.7772297075361,2.3973287367525));
#93854=CARTESIAN_POINT('Ctrl Pts',(-8.95727051033018,23.7715627107345,2.46854601124162));
#93855=CARTESIAN_POINT('Ctrl Pts',(-8.89141478136627,23.7667828479379,2.53967508974194));
#93856=CARTESIAN_POINT('Ctrl Pts',(-8.78368632444051,23.7580870661973,2.68201208555751));
#93857=CARTESIAN_POINT('Ctrl Pts',(-8.73988020463631,23.7541597935185,2.75125469238017));
#93858=CARTESIAN_POINT('Ctrl Pts',(-8.68698178934722,23.7483486950862,2.85278702992535));
#93859=CARTESIAN_POINT('Ctrl Pts',(-8.67285054304131,23.7466538156276,2.88228205625691));
#93860=CARTESIAN_POINT('Ctrl Pts',(-8.65728845269251,23.7445788374401,2.91776757037786));
#93861=CARTESIAN_POINT('Ctrl Pts',(-8.65489147412222,23.7442527417254,2.92332682356009));
#93862=CARTESIAN_POINT('Ctrl Pts',(-8.65124327387973,23.7437460183106,2.93193450980706));
#93863=CARTESIAN_POINT('Ctrl Pts',(-8.64996771138036,23.743566821238,2.93497263194652));
#93864=CARTESIAN_POINT('Ctrl Pts',(-8.64763322828445,23.743235049758,2.94058591585531));
#93865=CARTESIAN_POINT('Ctrl Pts',(-8.64657139030461,23.7430826526084,2.94315980669144));
#93866=CARTESIAN_POINT('Ctrl Pts',(-8.64419399589271,23.7427380624659,2.94896957375032));
#93867=CARTESIAN_POINT('Ctrl Pts',(-8.64288268335588,23.7425456220755,2.95220711964457));
#93868=CARTESIAN_POINT('Ctrl Pts',(-8.63954278058361,23.742049385323,2.96053872347024));
#93869=CARTESIAN_POINT('Ctrl Pts',(-8.63753122394465,23.7417446175078,2.96563949708205));
#93870=CARTESIAN_POINT('Ctrl Pts',(-8.62553318937835,23.7398911728908,2.99657153249675));
#93871=CARTESIAN_POINT('Ctrl Pts',(-8.61625353682907,23.7383052810604,3.02266913131957));
#93872=CARTESIAN_POINT('Ctrl Pts',(-8.57491228529225,23.7304959575204,3.15029699046659));
#93873=CARTESIAN_POINT('Ctrl Pts',(-8.55325438382536,23.7239630109981,3.25485756940824));
#93874=CARTESIAN_POINT('Ctrl Pts',(-8.53641451493989,23.7134375559269,3.43115858339805));
#93875=CARTESIAN_POINT('Ctrl Pts',(-8.53479684064148,23.7093370306252,3.5018745978602));
#93876=CARTESIAN_POINT('Ctrl Pts',(-8.53908865047082,23.7044970537929,3.58847664664175));
#93877=CARTESIAN_POINT('Ctrl Pts',(-8.54014735344128,23.7036088374729,3.60450056170623));
#93878=CARTESIAN_POINT('Ctrl Pts',(-8.54203935478994,23.702349553272,3.62740050915816));
#93879=CARTESIAN_POINT('Ctrl Pts',(-8.54265803393002,23.7019718531621,3.63429269879728));
#93880=CARTESIAN_POINT('Ctrl Pts',(-8.54381547011056,23.7013196090063,3.64623492708816));
#93881=CARTESIAN_POINT('Ctrl Pts',(-8.54433166994195,23.7010443673951,3.65128698807051));
#93882=CARTESIAN_POINT('Ctrl Pts',(-8.54537520285233,23.7005164866035,3.66099984207542));
#93883=CARTESIAN_POINT('Ctrl Pts',(-8.54589866589839,23.7002637303348,3.66566098060342));
#93884=CARTESIAN_POINT('Ctrl Pts',(-8.54718742724437,23.699668626216,3.6766596357364));
#93885=CARTESIAN_POINT('Ctrl Pts',(-8.5479718029144,23.6993268770486,3.68299484986503));
#93886=CARTESIAN_POINT('Ctrl Pts',(-8.55086006751484,23.6981360610574,3.70513382226229));
#93887=CARTESIAN_POINT('Ctrl Pts',(-8.55318076382091,23.6972937561501,3.7209084720094));
#93888=CARTESIAN_POINT('Ctrl Pts',(-8.57582664036929,23.6899612385402,3.85911742053291));
#93889=CARTESIAN_POINT('Ctrl Pts',(-8.61138990099582,23.6840098804222,3.97853879557646));
#93890=CARTESIAN_POINT('Ctrl Pts',(-8.68408874516995,23.6752444652851,4.14288411813394));
#93891=CARTESIAN_POINT('Ctrl Pts',(-8.70945373911387,23.6725101409102,4.19239579737966));
#93892=CARTESIAN_POINT('Ctrl Pts',(-8.75052123281472,23.6683442640722,4.26242404274384));
#93893=CARTESIAN_POINT('Ctrl Pts',(-8.76404794001469,23.667006106158,4.28416194603441));
#93894=CARTESIAN_POINT('Ctrl Pts',(-8.78124651768241,23.6653305055343,4.31024941699723));
#93895=CARTESIAN_POINT('Ctrl Pts',(-8.78438339982547,23.6650258772773,4.31494812576634));
#93896=CARTESIAN_POINT('Ctrl Pts',(-8.78934355318423,23.664545529096,4.32228553682562));
#93897=CARTESIAN_POINT('Ctrl Pts',(-8.79114846077446,23.664371012689,4.32493665938436));
#93898=CARTESIAN_POINT('Ctrl Pts',(-8.79454213814973,23.6640433449285,4.32988637840088));
#93899=CARTESIAN_POINT('Ctrl Pts',(-8.79612878409373,23.6638903348799,4.3321863690509));
#93900=CARTESIAN_POINT('Ctrl Pts',(-8.79978354159911,23.6635383156789,4.33745195371094));
#93901=CARTESIAN_POINT('Ctrl Pts',(-8.801856057825,23.6633390120951,4.34041443052928));
#93902=CARTESIAN_POINT('Ctrl Pts',(-8.80733262769193,23.6628132534526,4.34818126518695));
#93903=CARTESIAN_POINT('Ctrl Pts',(-8.81075470029879,23.6624856288094,4.35297276295648));
#93904=CARTESIAN_POINT('Ctrl Pts',(-8.83490304813642,23.660180695975,4.38635684649629));
#93905=CARTESIAN_POINT('Ctrl Pts',(-8.85662790605432,23.6581429586635,4.41420962021629));
#93906=CARTESIAN_POINT('Ctrl Pts',(-8.88058870871303,23.655954816684,4.44273771529126));
#93907=CARTESIAN_POINT('Ctrl Pts',(-8.88184356998543,23.6558403833516,4.44422573406034));
#93908=CARTESIAN_POINT('Ctrl Pts',(-8.89662388934563,23.654494484795,4.46168150429698));
#93909=CARTESIAN_POINT('Ctrl Pts',(-8.91048702115756,23.6532512627442,4.4773594938065));
#93910=CARTESIAN_POINT('Ctrl Pts',(-8.97952175168928,23.6471708933847,4.55213714495103));
#93911=CARTESIAN_POINT('Ctrl Pts',(-9.03919348808335,23.6422564068561,4.60689665050153));
#93912=CARTESIAN_POINT('Ctrl Pts',(-9.16035108970536,23.633175437658,4.70086405303821));
#93913=CARTESIAN_POINT('Ctrl Pts',(-9.22084552465803,23.6289954454839,4.74096959099842));
#93914=CARTESIAN_POINT('Ctrl Pts',(-9.2938331427261,23.6243638265268,4.78190713672895));
#93915=CARTESIAN_POINT('Ctrl Pts',(-9.30365826919754,23.6237483001826,4.78727065578239));
#93916=CARTESIAN_POINT('Ctrl Pts',(-9.31883244167052,23.622809609249,4.79532963435776));
#93917=CARTESIAN_POINT('Ctrl Pts',(-9.32413796563381,23.622483615709,4.798105780034));
#93918=CARTESIAN_POINT('Ctrl Pts',(-9.33383482729666,23.6218917718208,4.80310415250842));
#93919=CARTESIAN_POINT('Ctrl Pts',(-9.3382206025941,23.6216255556642,4.80533692953072));
#93920=CARTESIAN_POINT('Ctrl Pts',(-9.34781294306131,23.6210464605069,4.81015957311223));
#93921=CARTESIAN_POINT('Ctrl Pts',(-9.3530238633584,23.6207338907921,4.81274062335622));
#93922=CARTESIAN_POINT('Ctrl Pts',(-9.36733380977932,23.6198809521415,4.81972265998443));
#93923=CARTESIAN_POINT('Ctrl Pts',(-9.37646335519453,23.6193427573395,4.82406059792162));
#93924=CARTESIAN_POINT('Ctrl Pts',(-9.4237508163019,23.6165847779411,4.84593184192215));
#93925=CARTESIAN_POINT('Ctrl Pts',(-9.46260729887426,23.6144181499851,4.86191231395234));
#93926=CARTESIAN_POINT('Ctrl Pts',(-9.63599083623422,23.6050934835798,4.92464131622404));
#93927=CARTESIAN_POINT('Ctrl Pts',(-9.77621417859209,23.5985130682301,4.95327833017854));
#93928=CARTESIAN_POINT('Ctrl Pts',(-9.94836092545851,23.5897275599948,4.96289750402448));
#93929=CARTESIAN_POINT('Ctrl Pts',(-9.97841410790338,23.5881647724552,4.96364937866056));
#93930=CARTESIAN_POINT('Ctrl Pts',(-10.0143847984895,23.5862375972276,4.96344126957989));
#93931=CARTESIAN_POINT('Ctrl Pts',(-10.0203022696429,23.5859187237099,4.9633711379504));
#93932=CARTESIAN_POINT('Ctrl Pts',(-10.0294842333617,23.5854208652798,4.96320661385304));
#93933=CARTESIAN_POINT('Ctrl Pts',(-10.0327491783033,23.5852432326608,4.96313717939708));
#93934=CARTESIAN_POINT('Ctrl Pts',(-10.038799784885,23.5849128816183,4.96298824087418));
#93935=CARTESIAN_POINT('Ctrl Pts',(-10.041585466855,23.5847603286252,4.96291170779709));
#93936=CARTESIAN_POINT('Ctrl Pts',(-10.0479001802112,23.5844134763294,4.96272016801026));
#93937=CARTESIAN_POINT('Ctrl Pts',(-10.0514290077657,23.5842189150392,4.96260034657077));
#93938=CARTESIAN_POINT('Ctrl Pts',(-10.0605607399908,23.5837136073046,4.9622571898706));
#93939=CARTESIAN_POINT('Ctrl Pts',(-10.06616280344,23.5834018302963,4.9620144232989));
#93940=CARTESIAN_POINT('Ctrl Pts',(-10.1015524847365,23.5814215666116,4.96027698769106));
#93941=CARTESIAN_POINT('Ctrl Pts',(-10.1312880617372,23.5797099148056,4.95790431246343));
#93942=CARTESIAN_POINT('Ctrl Pts',(-10.3059844534842,23.5694512341025,4.93857729052175));
#93943=CARTESIAN_POINT('Ctrl Pts',(-10.4478332918166,23.5604000257373,4.9009239418998));
#93944=CARTESIAN_POINT('Ctrl Pts',(-10.6178548370982,23.5497402358234,4.82726523545954));
#93945=CARTESIAN_POINT('Ctrl Pts',(-10.6532840365219,23.5475226475161,4.81019005742227));
#93946=CARTESIAN_POINT('Ctrl Pts',(-10.6964413787712,23.5448252378798,4.7872037323046));
#93947=CARTESIAN_POINT('Ctrl Pts',(-10.7048532820597,23.5442996313555,4.78261681706844));
#93948=CARTESIAN_POINT('Ctrl Pts',(-10.7181439941829,23.5434692910718,4.77519930025588));
#93949=CARTESIAN_POINT('Ctrl Pts',(-10.7230524305683,23.5431626594194,4.77242258532526));
#93950=CARTESIAN_POINT('Ctrl Pts',(-10.7322683720483,23.5425869415287,4.76713855612959));
#93951=CARTESIAN_POINT('Ctrl Pts',(-10.7365793458197,23.5423176379663,4.76463748058266));
#93952=CARTESIAN_POINT('Ctrl Pts',(-10.7462598382276,23.541712870559,4.75895490622871));
#93953=CARTESIAN_POINT('Ctrl Pts',(-10.7516219696941,23.541377859835,4.75576097183759));
#93954=CARTESIAN_POINT('Ctrl Pts',(-10.7652840618685,23.5405241338797,4.74750433698011));
#93955=CARTESIAN_POINT('Ctrl Pts',(-10.7735543771945,23.5400071845511,4.74239301259026));
#93956=CARTESIAN_POINT('Ctrl Pts',(-10.8242641229988,23.5368355315662,4.71035006230517));
#93957=CARTESIAN_POINT('Ctrl Pts',(-10.8653458494322,23.5342591811885,4.68132800874782));
#93958=CARTESIAN_POINT('Ctrl Pts',(-11.0099878620285,23.5250315900361,4.56754362834255));
#93959=CARTESIAN_POINT('Ctrl Pts',(-11.1032720823039,23.5188190513534,4.47082907660747));
#93960=CARTESIAN_POINT('Ctrl Pts',(-11.1994648900954,23.5104969730295,4.33903637219664));
#93961=CARTESIAN_POINT('Ctrl Pts',(-11.2160902273755,23.5089659483734,4.31475295792951));
#93962=CARTESIAN_POINT('Ctrl Pts',(-11.235146861266,23.5070743189959,4.28503445181814));
#93963=CARTESIAN_POINT('Ctrl Pts',(-11.2382925069395,23.506757300823,4.28006315406942));
#93964=CARTESIAN_POINT('Ctrl Pts',(-11.2431335549875,23.5062617212544,4.2723094133114));
#93965=CARTESIAN_POINT('Ctrl Pts',(-11.2448498184939,23.5060844923462,4.26953998882264));
#93966=CARTESIAN_POINT('Ctrl Pts',(-11.2480172776146,23.5057545000391,4.26439053845503));
#93967=CARTESIAN_POINT('Ctrl Pts',(-11.2494709290368,23.5056018989879,4.26201208494968));
#93968=CARTESIAN_POINT('Ctrl Pts',(-11.2527558029482,23.5052544281633,4.25660272787043));
#93969=CARTESIAN_POINT('Ctrl Pts',(-11.2545828175223,23.5050592924624,4.25356933528042));
#93970=CARTESIAN_POINT('Ctrl Pts',(-11.2601134945302,23.504462909639,4.2443108890349));
#93971=CARTESIAN_POINT('Ctrl Pts',(-11.2637819081826,23.5040594943091,4.23806503966421));
#93972=CARTESIAN_POINT('Ctrl Pts',(-11.2987298205431,23.5001415870304,4.17753815050211));
#93973=CARTESIAN_POINT('Ctrl Pts',(-11.3265368152965,23.4964401316593,4.12133369070578));
#93974=CARTESIAN_POINT('Ctrl Pts',(-11.3818491481376,23.487835051943,3.9887618787863));
#93975=CARTESIAN_POINT('Ctrl Pts',(-11.4067833023341,23.4829173331846,3.91153031144746));
#93976=CARTESIAN_POINT('Ctrl Pts',(-11.4353262932692,23.4755080236475,3.78923438261099));
#93977=CARTESIAN_POINT('Ctrl Pts',(-11.4434679743336,23.472921971183,3.74539527512577));
#93978=CARTESIAN_POINT('Ctrl Pts',(-11.4533340272061,23.4688532343965,3.67433037236646));
#93979=CARTESIAN_POINT('Ctrl Pts',(-11.4563208811755,23.4673343047547,3.6473109068342));
#93980=CARTESIAN_POINT('Ctrl Pts',(-11.459249067983,23.4653728503826,3.61178582297373));
#93981=CARTESIAN_POINT('Ctrl Pts',(-11.4598712712659,23.4649093132918,3.60334306066155));
#93982=CARTESIAN_POINT('Ctrl Pts',(-11.4607699047658,23.4641541887159,3.58951325845839));
#93983=CARTESIAN_POINT('Ctrl Pts',(-11.4610898656212,23.4638612546469,3.58412932766789));
#93984=CARTESIAN_POINT('Ctrl Pts',(-11.4616515599508,23.4632960447493,3.57370501575531));
#93985=CARTESIAN_POINT('Ctrl Pts',(-11.4618970011509,23.4630236576435,3.56866491798058));
#93986=CARTESIAN_POINT('Ctrl Pts',(-11.4624037093391,23.4623963519076,3.55702039848241));
#93987=CARTESIAN_POINT('Ctrl Pts',(-11.4626463139728,23.4620420170152,3.55041524676307));
#93988=CARTESIAN_POINT('Ctrl Pts',(-11.4632813540841,23.4609091098581,3.52921017164921));
#93989=CARTESIAN_POINT('Ctrl Pts',(-11.4635,23.4601359197492,3.51460567629416));
#93990=CARTESIAN_POINT('Ctrl Pts',(-11.4635,23.4593691294935,3.50000000000014));
#93991=CARTESIAN_POINT('Ctrl Pts',(-11.4635,23.3906983315425,3.49999999997929));
#93992=CARTESIAN_POINT('Ctrl Pts',(-11.4635000000001,23.3912074294038,3.50921703575764));
#93993=CARTESIAN_POINT('Ctrl Pts',(-11.4634129275492,23.3917138314248,3.51843406141093));
#93994=CARTESIAN_POINT('Ctrl Pts',(-11.4631244128564,23.3925483519854,3.53370234837801));
#93995=CARTESIAN_POINT('Ctrl Pts',(-11.4629724897685,23.3928779932348,3.53975413817928));
#93996=CARTESIAN_POINT('Ctrl Pts',(-11.4626273931823,23.3934762749692,3.55077483019609));
#93997=CARTESIAN_POINT('Ctrl Pts',(-11.4624464372592,23.3937452902563,3.55574400113536));
#93998=CARTESIAN_POINT('Ctrl Pts',(-11.4620003484589,23.3943253544777,3.5664879537063));
#93999=CARTESIAN_POINT('Ctrl Pts',(-11.461726318057,23.394636122758,3.5722622951167));
#94000=CARTESIAN_POINT('Ctrl Pts',(-11.4608874126257,23.3954790516295,3.58797310230369));
#94001=CARTESIAN_POINT('Ctrl Pts',(-11.4602553767715,23.3960091240089,3.59790577235364));
#94002=CARTESIAN_POINT('Ctrl Pts',(-11.4565795420355,23.3986509037902,3.64765902006547));
#94003=CARTESIAN_POINT('Ctrl Pts',(-11.4520079048078,23.4007148223623,3.68735143334495));
#94004=CARTESIAN_POINT('Ctrl Pts',(-11.4433918987835,23.4035328160469,3.74227492096282));
#94005=CARTESIAN_POINT('Ctrl Pts',(-11.440717792496,23.4043201497397,3.75770054492073));
#94006=CARTESIAN_POINT('Ctrl Pts',(-11.4192878089853,23.4100586458689,3.87053155916608));
#94007=CARTESIAN_POINT('Ctrl Pts',(-11.3909205558537,23.414773281846,3.96584434415665));
#94008=CARTESIAN_POINT('Ctrl Pts',(-11.3329290384623,23.4222857546511,4.10658431205819));
#94009=CARTESIAN_POINT('Ctrl Pts',(-11.3100781448902,23.424953532139,4.15447579479587));
#94010=CARTESIAN_POINT('Ctrl Pts',(-11.2797193890136,23.4283062234842,4.21011116313542));
#94011=CARTESIAN_POINT('Ctrl Pts',(-11.2746606830645,23.428859404488,4.21915207677826));
#94012=CARTESIAN_POINT('Ctrl Pts',(-11.2674699191754,23.4296392926779,4.23168914895539));
#94013=CARTESIAN_POINT('Ctrl Pts',(-11.2654184090124,23.4298610859948,4.2352314302484));
#94014=CARTESIAN_POINT('Ctrl Pts',(-11.2619037256965,23.4302399521439,4.24124184279518));
#94015=CARTESIAN_POINT('Ctrl Pts',(-11.2604480879947,23.4303965437505,4.24371439396251));
#94016=CARTESIAN_POINT('Ctrl Pts',(-11.2576417667,23.4306978565715,4.24844931642227));
#94017=CARTESIAN_POINT('Ctrl Pts',(-11.2562922334766,23.430842499369,4.250712339368));
#94018=CARTESIAN_POINT('Ctrl Pts',(-11.2526867675871,23.43122822969,4.25672137159404));
#94019=CARTESIAN_POINT('Ctrl Pts',(-11.2504201627304,23.4314699972862,4.2604609046783));
#94020=CARTESIAN_POINT('Ctrl Pts',(-11.2422275209524,23.4323411244157,4.27384178624076));
#94021=CARTESIAN_POINT('Ctrl Pts',(-11.236206609363,23.4329762483821,4.28342423171753));
#94022=CARTESIAN_POINT('Ctrl Pts',(-11.1849399700597,23.4383361116751,4.36295380733965));
#94023=CARTESIAN_POINT('Ctrl Pts',(-11.1339123406492,23.4433564274495,4.42898467047999));
#94024=CARTESIAN_POINT('Ctrl Pts',(-11.0003776861745,23.4552409214194,4.57428293112232));
#94025=CARTESIAN_POINT('Ctrl Pts',(-10.9136394915394,23.4620351592899,4.6489607599487));
#94026=CARTESIAN_POINT('Ctrl Pts',(-10.8061105600909,23.4692734297799,4.72158238463592));
#94027=CARTESIAN_POINT('Ctrl Pts',(-10.7929854823801,23.470139782948,4.73014300352123));
#94028=CARTESIAN_POINT('Ctrl Pts',(-10.7739253172125,23.4713738862977,4.74214283536102));
#94029=CARTESIAN_POINT('Ctrl Pts',(-10.7680999015707,23.4717479088373,4.74575349227136));
#94030=CARTESIAN_POINT('Ctrl Pts',(-10.7579227196591,23.4723959254996,4.75196289415709));
#94031=CARTESIAN_POINT('Ctrl Pts',(-10.7535824516535,23.4726705914718,4.75458017949424));
#94032=CARTESIAN_POINT('Ctrl Pts',(-10.7451839016029,23.4731988532377,4.7595853973536));
#94033=CARTESIAN_POINT('Ctrl Pts',(-10.741127525107,23.4734525574434,4.7619763914895));
#94034=CARTESIAN_POINT('Ctrl Pts',(-10.7314866795827,23.4740521761558,4.76759658418733));
#94035=CARTESIAN_POINT('Ctrl Pts',(-10.7258922338726,23.4743974699716,4.77080853367548));
#94036=CARTESIAN_POINT('Ctrl Pts',(-10.7060575681069,23.475612490521,4.78202253127321));
#94037=CARTESIAN_POINT('Ctrl Pts',(-10.6917045203374,23.4764750830559,4.78982322233451));
#94038=CARTESIAN_POINT('Ctrl Pts',(-10.5710905347894,23.4835938031456,4.85278279158265));
#94039=CARTESIAN_POINT('Ctrl Pts',(-10.4585633439973,23.4893548244639,4.8949508375397));
#94040=CARTESIAN_POINT('Ctrl Pts',(-10.2852621820657,23.4980382713809,4.93662135274832));
#94041=CARTESIAN_POINT('Ctrl Pts',(-10.2276102801366,23.5009074934132,4.94687527445646));
#94042=CARTESIAN_POINT('Ctrl Pts',(-10.1432937750199,23.5052579058688,4.95670706039194));
#94043=CARTESIAN_POINT('Ctrl Pts',(-10.1170072954747,23.5066359145043,4.95905369546237));
#94044=CARTESIAN_POINT('Ctrl Pts',(-10.084982086561,23.5083562586701,4.96104168710037));
#94045=CARTESIAN_POINT('Ctrl Pts',(-10.0792887970383,23.5086636851918,4.96136171121067));
#94046=CARTESIAN_POINT('Ctrl Pts',(-10.0703785277654,23.5091475108078,4.96181034252474));
#94047=CARTESIAN_POINT('Ctrl Pts',(-10.0671626844056,23.5093226779747,4.96196162333239));
#94048=CARTESIAN_POINT('Ctrl Pts',(-10.0611555791827,23.509650950606,4.96222434965143));
#94049=CARTESIAN_POINT('Ctrl Pts',(-10.0583644835089,23.5098039100244,4.96233841508109));
#94050=CARTESIAN_POINT('Ctrl Pts',(-10.0519759898551,23.5101549985461,4.96258117868936));
#94051=CARTESIAN_POINT('Ctrl Pts',(-10.0483784420901,23.5103534157619,4.96270459544909));
#94052=CARTESIAN_POINT('Ctrl Pts',(-10.0389500161523,23.5108752181624,4.96299322377851));
#94053=CARTESIAN_POINT('Ctrl Pts',(-10.0331186003284,23.5111997449206,4.96313684683909));
#94054=CARTESIAN_POINT('Ctrl Pts',(-9.99311175813237,23.5134377751768,4.96388289383226));
#94055=CARTESIAN_POINT('Ctrl Pts',(-9.95892760717565,23.5154079173911,4.96332268288292));
#94056=CARTESIAN_POINT('Ctrl Pts',(-9.82457592999175,23.5232996323083,4.95640981504714));
#94057=CARTESIAN_POINT('Ctrl Pts',(-9.7251514606692,23.5294445074818,4.94095875797759));
#94058=CARTESIAN_POINT('Ctrl Pts',(-9.57829745194627,23.5384629635976,4.90237282047192));
#94059=CARTESIAN_POINT('Ctrl Pts',(-9.52922797043155,23.5414705900432,4.8866712140115));
#94060=CARTESIAN_POINT('Ctrl Pts',(-9.45299685464826,23.5461107510936,4.85776366144886));
#94061=CARTESIAN_POINT('Ctrl Pts',(-9.42524264703663,23.5477935047904,4.84624989266624));
#94062=CARTESIAN_POINT('Ctrl Pts',(-9.38986601936233,23.5499308395707,4.83028031644137));
#94063=CARTESIAN_POINT('Ctrl Pts',(-9.38190355055782,23.5504114163702,4.8265994039391));
#94064=CARTESIAN_POINT('Ctrl Pts',(-9.36903755682835,23.551187257947,4.82051068822291));
#94065=CARTESIAN_POINT('Ctrl Pts',(-9.36411365287844,23.5514840129918,4.81814666751325));
#94066=CARTESIAN_POINT('Ctrl Pts',(-9.35468604669761,23.5520519190293,4.81355524985056));
#94067=CARTESIAN_POINT('Ctrl Pts',(-9.35018036182279,23.5523232119286,4.8113321209541));
#94068=CARTESIAN_POINT('Ctrl Pts',(-9.33990758163315,23.5529415065507,4.80619752853585));
#94069=CARTESIAN_POINT('Ctrl Pts',(-9.33414811394634,23.5532879795763,4.80327098180013));
#94070=CARTESIAN_POINT('Ctrl Pts',(-9.31892193142294,23.5542035884413,4.79540685039448));
#94071=CARTESIAN_POINT('Ctrl Pts',(-9.30948945320616,23.5547704310484,4.79040359435589));
#94072=CARTESIAN_POINT('Ctrl Pts',(-9.21408026041001,23.5605025744142,4.73845008775281));
#94073=CARTESIAN_POINT('Ctrl Pts',(-9.13296612948781,23.5653403437218,4.68308232362608));
#94074=CARTESIAN_POINT('Ctrl Pts',(-9.00446566970936,23.5735173533358,4.57500428320357));
#94075=CARTESIAN_POINT('Ctrl Pts',(-8.95424396841218,23.5768855711764,4.52621453271419));
#94076=CARTESIAN_POINT('Ctrl Pts',(-8.88852742325798,23.5818331800146,4.4525183704844));
#94077=CARTESIAN_POINT('Ctrl Pts',(-8.86999028792273,23.583299498442,4.43045172412937));
#94078=CARTESIAN_POINT('Ctrl Pts',(-8.84521299814401,23.5853828488466,4.39912352722885));
#94079=CARTESIAN_POINT('Ctrl Pts',(-8.83840844824702,23.5859687850385,4.39031521956254));
#94080=CARTESIAN_POINT('Ctrl Pts',(-8.82677171945817,23.5869967335051,4.37489127967897));
#94081=CARTESIAN_POINT('Ctrl Pts',(-8.82189332148713,23.5874358833291,4.36831100269691));
#94082=CARTESIAN_POINT('Ctrl Pts',(-8.81487822977822,23.5880799981029,4.35868067615856));
#94083=CARTESIAN_POINT('Ctrl Pts',(-8.81269744491141,23.5882820480314,4.35566275828639));
#94084=CARTESIAN_POINT('Ctrl Pts',(-8.80889243524333,23.5886378425583,4.35035457461003));
#94085=CARTESIAN_POINT('Ctrl Pts',(-8.80726325325438,23.588791246254,4.3480679137093));
#94086=CARTESIAN_POINT('Ctrl Pts',(-8.8038225045393,23.5891175134407,4.34320907656469));
#94087=CARTESIAN_POINT('Ctrl Pts',(-8.80201267740766,23.5892904836699,4.34063578437401));
#94088=CARTESIAN_POINT('Ctrl Pts',(-8.79713646055003,23.5897601544766,4.33365483611582));
#94089=CARTESIAN_POINT('Ctrl Pts',(-8.79408603865047,23.5900578994709,4.3292361523121));
#94090=CARTESIAN_POINT('Ctrl Pts',(-8.78027535397555,23.5914236422683,4.3089933405341));
#94091=CARTESIAN_POINT('Ctrl Pts',(-8.76980225136383,23.5925090094735,4.2929765848516));
#94092=CARTESIAN_POINT('Ctrl Pts',(-8.74942540632657,23.5947160802679,4.26043823450301));
#94093=CARTESIAN_POINT('Ctrl Pts',(-8.73952762730232,23.595837770075,4.24391697436218));
#94094=CARTESIAN_POINT('Ctrl Pts',(-8.72494000965346,23.5975637848104,4.21844018529922));
#94095=CARTESIAN_POINT('Ctrl Pts',(-8.72001186434161,23.5981604876917,4.20962288951818));
#94096=CARTESIAN_POINT('Ctrl Pts',(-8.67045171980135,23.6042983895561,4.11875510921249));
#94097=CARTESIAN_POINT('Ctrl Pts',(-8.63368012113684,23.6100006217181,4.03266095603095));
#94098=CARTESIAN_POINT('Ctrl Pts',(-8.58563102793481,23.6193833890263,3.88161488111155));
#94099=CARTESIAN_POINT('Ctrl Pts',(-8.57005707368791,23.6231466901718,3.81833077532525));
#94100=CARTESIAN_POINT('Ctrl Pts',(-8.55607393135115,23.6276353357323,3.73905377258055));
#94101=CARTESIAN_POINT('Ctrl Pts',(-8.55363938058424,23.6284861942424,3.72385303651734));
#94102=CARTESIAN_POINT('Ctrl Pts',(-8.55047502946003,23.6297023538986,3.70188094432194));
#94103=CARTESIAN_POINT('Ctrl Pts',(-8.54955200184913,23.6300736784682,3.69513882942634));
#94104=CARTESIAN_POINT('Ctrl Pts',(-8.54802464389022,23.6307185540238,3.68337235539854));
#94105=CARTESIAN_POINT('Ctrl Pts',(-8.54739929122677,23.6309927583898,3.67835088236336));
#94106=CARTESIAN_POINT('Ctrl Pts',(-8.54624086449818,23.6315212150679,3.66863841238113));
#94107=CARTESIAN_POINT('Ctrl Pts',(-8.5457044216321,23.6317755694375,3.66394788697628));
#94108=CARTESIAN_POINT('Ctrl Pts',(-8.544483445273,23.6323784057571,3.65279414041362));
#94109=CARTESIAN_POINT('Ctrl Pts',(-8.54381924697325,23.6327262508379,3.64632876269826));
#94110=CARTESIAN_POINT('Ctrl Pts',(-8.54160941330306,23.6339591422253,3.62331066987504));
#94111=CARTESIAN_POINT('Ctrl Pts',(-8.54030273999111,23.6348367716442,3.60673595195195));
#94112=CARTESIAN_POINT('Ctrl Pts',(-8.53215590185929,23.6417538883302,3.4747192922915));
#94113=CARTESIAN_POINT('Ctrl Pts',(-8.5387376484625,23.6473367116108,3.35886047152888));
#94114=CARTESIAN_POINT('Ctrl Pts',(-8.57386758289224,23.6571493904704,3.16034538405839));
#94115=CARTESIAN_POINT('Ctrl Pts',(-8.59626830586342,23.661354714722,3.07720876805326));
#94116=CARTESIAN_POINT('Ctrl Pts',(-8.6283330912345,23.6663266552157,2.98969108657156));
#94117=CARTESIAN_POINT('Ctrl Pts',(-8.63088962320762,23.6667178511021,2.98287132403634));
#94118=CARTESIAN_POINT('Ctrl Pts',(-8.6347676903831,23.6673040540762,2.97275661092185));
#94119=CARTESIAN_POINT('Ctrl Pts',(-8.63605052306429,23.6674968357774,2.96944682229547));
#94120=CARTESIAN_POINT('Ctrl Pts',(-8.63836277762046,23.6678423740748,2.96354487268786));
#94121=CARTESIAN_POINT('Ctrl Pts',(-8.6393875804885,23.6679948553176,2.96095095519485));
#94122=CARTESIAN_POINT('Ctrl Pts',(-8.64162409435158,23.6683262148944,2.95533704257536));
#94123=CARTESIAN_POINT('Ctrl Pts',(-8.64283844730232,23.6685052455081,2.95231819667746));
#94124=CARTESIAN_POINT('Ctrl Pts',(-8.64620931932002,23.6689997375778,2.94401836138178));
#94125=CARTESIAN_POINT('Ctrl Pts',(-8.64838663869101,23.6693164042342,2.93874594975514));
#94126=CARTESIAN_POINT('Ctrl Pts',(-8.65968336054095,23.6709450795215,2.91183775385509));
#94127=CARTESIAN_POINT('Ctrl Pts',(-8.66929117634481,23.6722835094616,2.89041208997631));
#94128=CARTESIAN_POINT('Ctrl Pts',(-8.6821257881266,23.6740069534355,2.86354141700963));
#94129=CARTESIAN_POINT('Ctrl Pts',(-8.68487866764491,23.6743731359694,2.85787240726105));
#94130=CARTESIAN_POINT('Ctrl Pts',(-8.73430206442872,23.6808843924724,2.75774574992416));
#94131=CARTESIAN_POINT('Ctrl Pts',(-8.79100076328839,23.6873469492549,2.66858310208491));
#94132=CARTESIAN_POINT('Ctrl Pts',(-8.88918141947249,23.6966904549748,2.54574251604854));
#94133=CARTESIAN_POINT('Ctrl Pts',(-8.92371634816917,23.6997233753054,2.50695439417005));
#94134=CARTESIAN_POINT('Ctrl Pts',(-8.98149663479204,23.704397306475,2.44862216364288));
#94135=CARTESIAN_POINT('Ctrl Pts',(-9.00341163434028,23.7060894467004,2.42782637641828));
#94136=CARTESIAN_POINT('Ctrl Pts',(-9.03251486834469,23.7082367861879,2.40187341127457));
#94137=CARTESIAN_POINT('Ctrl Pts',(-9.03912665820261,23.7087182821949,2.39608337697353));
#94138=CARTESIAN_POINT('Ctrl Pts',(-9.04993435879627,23.7094952377843,2.38678959780096));
#94139=CARTESIAN_POINT('Ctrl Pts',(-9.05409838086998,23.7097921955656,2.38324924436234));
#94140=CARTESIAN_POINT('Ctrl Pts',(-9.06212721379505,23.7103602464071,2.37650005858213));
#94141=CARTESIAN_POINT('Ctrl Pts',(-9.0659888971158,23.7106314829962,2.37328764006588));
#94142=CARTESIAN_POINT('Ctrl Pts',(-9.07484882257735,23.7112493156504,2.36599418673633));
#94143=CARTESIAN_POINT('Ctrl Pts',(-9.07985768874789,23.7115953857987,2.36192618233066));
#94144=CARTESIAN_POINT('Ctrl Pts',(-9.09320513927605,23.7125092181573,2.35123162959849));
#94145=CARTESIAN_POINT('Ctrl Pts',(-9.1015895202636,23.7130747015515,2.34466268729551));
#94146=CARTESIAN_POINT('Ctrl Pts',(-9.17207181688326,23.7177595741196,2.29067292883538));
#94147=CARTESIAN_POINT('Ctrl Pts',(-9.23780684439185,23.7216789204664,2.24820103123834));
#94148=CARTESIAN_POINT('Ctrl Pts',(-9.36512936956547,23.7287750257926,2.17970274562462));
#94149=CARTESIAN_POINT('Ctrl Pts',(-9.42570712249699,23.7319693083531,2.15224888152499));
#94150=CARTESIAN_POINT('Ctrl Pts',(-9.53032754788325,23.7374534491439,2.113173614276));
#94151=CARTESIAN_POINT('Ctrl Pts',(-9.57342439056545,23.7397050746534,2.09931717969435));
#94152=CARTESIAN_POINT('Ctrl Pts',(-9.63885413113765,23.7432019411162,2.08158032820589));
#94153=CARTESIAN_POINT('Ctrl Pts',(-9.66074984669421,23.744385086094,2.07618472889172));
#94154=CARTESIAN_POINT('Ctrl Pts',(-9.68806376261951,23.7458866348142,2.07011974340862));
#94155=CARTESIAN_POINT('Ctrl Pts',(-9.69337373615627,23.7461797374485,2.06897166456006));
#94156=CARTESIAN_POINT('Ctrl Pts',(-9.70178223699026,23.7466459331697,2.06720259572797));
#94157=CARTESIAN_POINT('Ctrl Pts',(-9.70487664872617,23.7468179377778,2.06656201982508));
#94158=CARTESIAN_POINT('Ctrl Pts',(-9.71072110873403,23.7471436760102,2.06537188168046));
#94159=CARTESIAN_POINT('Ctrl Pts',(-9.71347067547705,23.7472972888507,2.06482019923414));
#94160=CARTESIAN_POINT('Ctrl Pts',(-9.71978817208197,23.7476510628716,2.06357151328188));
#94161=CARTESIAN_POINT('Ctrl Pts',(-9.72335712560096,23.7478515238229,2.06287989874965));
#94162=CARTESIAN_POINT('Ctrl Pts',(-9.73290660553494,23.7483894406915,2.06106622998448));
#94163=CARTESIAN_POINT('Ctrl Pts',(-9.73889154979099,23.748728183542,2.05996817727254));
#94164=CARTESIAN_POINT('Ctrl Pts',(-9.78434068015442,23.7513118893759,2.05192230718739));
#94165=CARTESIAN_POINT('Ctrl Pts',(-9.8240653539505,23.7536344875168,2.04656118086459));
#94166=CARTESIAN_POINT('Ctrl Pts',(-9.95141974968251,23.7611825599238,2.03467110851035));
#94167=CARTESIAN_POINT('Ctrl Pts',(-10.0394401651108,23.7665406072006,2.03439652104904));
#94168=CARTESIAN_POINT('Ctrl Pts',(-10.2094693422858,23.7767121510989,2.04920188757023));
#94169=CARTESIAN_POINT('Ctrl Pts',(-10.2912345862112,23.7815210109707,2.06337945700882));
#94170=CARTESIAN_POINT('Ctrl Pts',(-10.3824512719545,23.7867429806841,2.08730948789723));
#94171=CARTESIAN_POINT('Ctrl Pts',(-10.3934966717795,23.7873731098237,2.09034619917073));
#94172=CARTESIAN_POINT('Ctrl Pts',(-10.4103140338702,23.7883293527013,2.09518286839099));
#94173=CARTESIAN_POINT('Ctrl Pts',(-10.4161122157039,23.7886584611566,2.09688938243383));
#94174=CARTESIAN_POINT('Ctrl Pts',(-10.4266605943626,23.7892561833274,2.10006510596323));
#94175=CARTESIAN_POINT('Ctrl Pts',(-10.4314141724557,23.7895251682968,2.10152269129109));
#94176=CARTESIAN_POINT('Ctrl Pts',(-10.4416859068248,23.7901056236096,2.10472966110867));
#94177=CARTESIAN_POINT('Ctrl Pts',(-10.447201311261,23.7904168102328,2.10648762208454));
#94178=CARTESIAN_POINT('Ctrl Pts',(-10.4622034260914,23.7912619961072,2.11136758495307));
#94179=CARTESIAN_POINT('Ctrl Pts',(-10.4716689373083,23.7917938881245,2.11455407488816));
#94180=CARTESIAN_POINT('Ctrl Pts',(-10.5192478743587,23.7944614171595,2.13111528395226));
#94181=CARTESIAN_POINT('Ctrl Pts',(-10.5568303053279,23.7965481022977,2.14596746333614));
#94182=CARTESIAN_POINT('Ctrl Pts',(-10.6071965002018,23.7993398329171,2.16832398383076));
#94183=CARTESIAN_POINT('Ctrl Pts',(-10.6205499732611,23.8000796116419,2.17449392787499));
#94184=CARTESIAN_POINT('Ctrl Pts',(-10.7236865949669,23.8057989703966,2.22404823334212));
#94185=CARTESIAN_POINT('Ctrl Pts',(-10.8089124218148,23.8105374522379,2.27630260807894));
#94186=CARTESIAN_POINT('Ctrl Pts',(-10.9302446611886,23.8180721266269,2.36894717852285));
#94187=CARTESIAN_POINT('Ctrl Pts',(-10.97054817513,23.8207360104829,2.40333650516365));
#94188=CARTESIAN_POINT('Ctrl Pts',(-11.0163951107256,23.824083981939,2.446966102421));
#94189=CARTESIAN_POINT('Ctrl Pts',(-11.0238179203126,23.8246367374346,2.45418153368306));
#94190=CARTESIAN_POINT('Ctrl Pts',(-11.0340672627171,23.825416123773,2.46435822193894));
#94191=CARTESIAN_POINT('Ctrl Pts',(-11.0369590336273,23.8256378491634,2.46725368165889));
#94192=CARTESIAN_POINT('Ctrl Pts',(-11.0418574412937,23.8260166344921,2.47219965309399));
#94193=CARTESIAN_POINT('Ctrl Pts',(-11.0438702867074,23.8261732137143,2.47424403219436));
#94194=CARTESIAN_POINT('Ctrl Pts',(-11.0477204068644,23.8264745322719,2.47817753824375));
#94195=CARTESIAN_POINT('Ctrl Pts',(-11.0495586057889,23.8266191933508,2.48006572412928));
#94196=CARTESIAN_POINT('Ctrl Pts',(-11.0544346147417,23.8270050284649,2.48510146874311));
#94197=CARTESIAN_POINT('Ctrl Pts',(-11.0574634044309,23.8272468832122,2.48825767470511));
#94198=CARTESIAN_POINT('Ctrl Pts',(-11.0682835557755,23.8281186250283,2.49963467589067));
#94199=CARTESIAN_POINT('Ctrl Pts',(-11.0759933709856,23.8287542867525,2.5079320654771));
#94200=CARTESIAN_POINT('Ctrl Pts',(-11.1353419302449,23.8337560246244,2.57330932742279));
#94201=CARTESIAN_POINT('Ctrl Pts',(-11.1824968697725,23.8383752703551,2.63428873496673));
#94202=CARTESIAN_POINT('Ctrl Pts',(-11.2599362719332,23.8468910854631,2.7526380550076));
#94203=CARTESIAN_POINT('Ctrl Pts',(-11.2916364442379,23.8507749371621,2.80886657267899));
#94204=CARTESIAN_POINT('Ctrl Pts',(-11.3444467221146,23.8579583824061,2.91895354179092));
#94205=CARTESIAN_POINT('Ctrl Pts',(-11.3662798428304,23.8612705589165,2.9723328669278));
#94206=CARTESIAN_POINT('Ctrl Pts',(-11.3895782093693,23.8652825537784,3.04052951177835));
#94207=CARTESIAN_POINT('Ctrl Pts',(-11.3940437773868,23.8660798044702,3.05426162692007));
#94208=CARTESIAN_POINT('Ctrl Pts',(-11.4002628856262,23.8672335885791,3.0743944503738));
#94209=CARTESIAN_POINT('Ctrl Pts',(-11.4021771878489,23.8675953208337,3.08074426821107));
#94210=CARTESIAN_POINT('Ctrl Pts',(-11.4054682768792,23.868229117632,3.09193566012703));
#94211=CARTESIAN_POINT('Ctrl Pts',(-11.4068633631765,23.8685017705102,3.09677170111645));
#94212=CARTESIAN_POINT('Ctrl Pts',(-11.4097128521104,23.8690671452016,3.10684423040019));
#94213=CARTESIAN_POINT('Ctrl Pts',(-11.4111630924045,23.8693597292699,3.11208182266669));
#94214=CARTESIAN_POINT('Ctrl Pts',(-11.4148452621738,23.870115452321,3.12567405501381));
#94215=CARTESIAN_POINT('Ctrl Pts',(-11.4170324021359,23.8705771505744,3.13404070525964));
#94216=CARTESIAN_POINT('Ctrl Pts',(-11.4261910350154,23.8725684127715,3.17038966971276));
#94217=CARTESIAN_POINT('Ctrl Pts',(-11.4324090284434,23.8740739152525,3.19855620594468));
#94218=CARTESIAN_POINT('Ctrl Pts',(-11.4468430287676,23.8780505865583,3.27454401483362));
#94219=CARTESIAN_POINT('Ctrl Pts',(-11.4535207052353,23.880476716683,3.32262133396581));
#94220=CARTESIAN_POINT('Ctrl Pts',(-11.461599903769,23.8849905269656,3.41388284459606));
#94221=CARTESIAN_POINT('Ctrl Pts',(-11.46349999621,23.8870825918401,3.45694326727398));
#94222=CARTESIAN_POINT('Ctrl Pts',(-11.4635,23.8891760003868,3.49999987117833));
#94223=CARTESIAN_POINT('Origin',(-10.,13.2,3.5));
#94224=CARTESIAN_POINT('',(-11.4635,24.4618423224409,3.5000000024766));
#94225=CARTESIAN_POINT('',(-11.4635,24.3883362350912,3.49999997785042));
#94226=CARTESIAN_POINT('',(-11.4635,13.2,3.5));
#94227=CARTESIAN_POINT('',(-11.4634993894688,23.9606357550012,3.50131794111532));
#94228=CARTESIAN_POINT('Ctrl Pts',(-11.4635,24.4618423224409,3.5000000024766));
#94229=CARTESIAN_POINT('Ctrl Pts',(-11.4635000000413,24.4605992464299,3.47560470021283));
#94230=CARTESIAN_POINT('Ctrl Pts',(-11.4628900255798,24.4593350241618,3.45121150056634));
#94231=CARTESIAN_POINT('Ctrl Pts',(-11.4612084486067,24.4575508424555,3.41761358387352));
#94232=CARTESIAN_POINT('Ctrl Pts',(-11.4606590987307,24.4570564898491,3.40838864519993));
#94233=CARTESIAN_POINT('Ctrl Pts',(-11.4597544135585,24.456347357988,3.3952887978131));
#94234=CARTESIAN_POINT('Ctrl Pts',(-11.4594709207471,24.4561364416346,3.39140895733704));
#94235=CARTESIAN_POINT('Ctrl Pts',(-11.4589552409549,24.4557711333003,3.38471857087606));
#94236=CARTESIAN_POINT('Ctrl Pts',(-11.4587303949448,24.4556171524389,3.38190750334044));
#94237=CARTESIAN_POINT('Ctrl Pts',(-11.4582451514157,24.4552954668714,3.3760538293116));
#94238=CARTESIAN_POINT('Ctrl Pts',(-11.4579833598935,24.4551276921148,3.3730114305314));
#94239=CARTESIAN_POINT('Ctrl Pts',(-11.457271900044,24.4546863734907,3.36503555713485));
#94240=CARTESIAN_POINT('Ctrl Pts',(-11.4568067042835,24.4544119866951,3.36010355115903));
#94241=CARTESIAN_POINT('Ctrl Pts',(-11.454786693268,24.453276046025,3.33979105976632));
#94242=CARTESIAN_POINT('Ctrl Pts',(-11.45301332472,24.4524033307197,3.32443386932067));
#94243=CARTESIAN_POINT('Ctrl Pts',(-11.4372726914926,24.4455104654705,3.20478689737983));
#94244=CARTESIAN_POINT('Ctrl Pts',(-11.4123388201589,24.4390713827039,3.1022550533107));
#94245=CARTESIAN_POINT('Ctrl Pts',(-11.3449846918308,24.4271872177322,2.91558433975732));
#94246=CARTESIAN_POINT('Ctrl Pts',(-11.3050272236307,24.4217382590728,2.83109457089067));
#94247=CARTESIAN_POINT('Ctrl Pts',(-11.2513280475935,24.4159263074224,2.74095702639467));
#94248=CARTESIAN_POINT('Ctrl Pts',(-11.2452427554995,24.4152849220257,2.73101455840975));
#94249=CARTESIAN_POINT('Ctrl Pts',(-11.2357958904314,24.4143147562223,2.71598602823573));
#94250=CARTESIAN_POINT('Ctrl Pts',(-11.2325203480046,24.413982861006,2.71084666632516));
#94251=CARTESIAN_POINT('Ctrl Pts',(-11.2265071958815,24.4133816182688,2.70154073330227));
#94252=CARTESIAN_POINT('Ctrl Pts',(-11.2237802291797,24.4131118853662,2.69736742301124));
#94253=CARTESIAN_POINT('Ctrl Pts',(-11.2178497437404,24.4125315215079,2.6883919830812));
#94254=CARTESIAN_POINT('Ctrl Pts',(-11.2146390225884,24.4122211633616,2.68359469773532));
#94255=CARTESIAN_POINT('Ctrl Pts',(-11.2058552591927,24.4113823573186,2.67063699638782));
#94256=CARTESIAN_POINT('Ctrl Pts',(-11.2002277600222,24.4108559499104,2.66251374438105));
#94257=CARTESIAN_POINT('Ctrl Pts',(-11.1720840478895,24.4082758650757,2.62275488993514));
#94258=CARTESIAN_POINT('Ctrl Pts',(-11.1483962910001,24.4062670416568,2.59196569733561));
#94259=CARTESIAN_POINT('Ctrl Pts',(-11.0276800369282,24.3967041380207,2.44735147800674));
#94260=CARTESIAN_POINT('Ctrl Pts',(-10.914837715372,24.389823106038,2.34793342793114));
#94261=CARTESIAN_POINT('Ctrl Pts',(-10.7673264346335,24.3808406815148,2.2535253424028));
#94262=CARTESIAN_POINT('Ctrl Pts',(-10.7453848254409,24.3795022017801,2.24028168447792));
#94263=CARTESIAN_POINT('Ctrl Pts',(-10.7179926271854,24.3778143135933,2.2247143617253));
#94264=CARTESIAN_POINT('Ctrl Pts',(-10.7128595999059,24.377497304607,2.22183801481982));
#94265=CARTESIAN_POINT('Ctrl Pts',(-10.7048183975702,24.3769993595737,2.21739554588596));
#94266=CARTESIAN_POINT('Ctrl Pts',(-10.7019219710476,24.3768197329366,2.21580815086366));
#94267=CARTESIAN_POINT('Ctrl Pts',(-10.6965901436601,24.3764885345314,2.21290945444745));
#94268=CARTESIAN_POINT('Ctrl Pts',(-10.6941563844152,24.3763371483724,2.21159524435182));
#94269=CARTESIAN_POINT('Ctrl Pts',(-10.6886396813893,24.3759935244096,2.20863643840028));
#94270=CARTESIAN_POINT('Ctrl Pts',(-10.6855545926824,24.3758010341536,2.20699599422859));
#94271=CARTESIAN_POINT('Ctrl Pts',(-10.6762763603838,24.3752212208592,2.20210499046995));
#94272=CARTESIAN_POINT('Ctrl Pts',(-10.6700658506369,24.3748319032563,2.1988878129801));
#94273=CARTESIAN_POINT('Ctrl Pts',(-10.6027711116291,24.3706023302133,2.16463727998377));
#94274=CARTESIAN_POINT('Ctrl Pts',(-10.5396085436835,24.3665378906929,2.13788867564553));
#94275=CARTESIAN_POINT('Ctrl Pts',(-10.3797877727207,24.3563971630509,2.08307178870065));
#94276=CARTESIAN_POINT('Ctrl Pts',(-10.2816476108466,24.3503097343258,2.06034625668137));
#94277=CARTESIAN_POINT('Ctrl Pts',(-10.13907714812,24.3420031489043,2.04248273590023));
#94278=CARTESIAN_POINT('Ctrl Pts',(-10.0959865747642,24.3395568576619,2.03901192661985));
#94279=CARTESIAN_POINT('Ctrl Pts',(-10.0426126114907,24.336605972174,2.03708497243275));
#94280=CARTESIAN_POINT('Ctrl Pts',(-10.0324193070899,24.3360459231807,2.03682358942609));
#94281=CARTESIAN_POINT('Ctrl Pts',(-10.0163877176333,24.3351704674137,2.0365801143203));
#94282=CARTESIAN_POINT('Ctrl Pts',(-10.0105509813942,24.3348528510723,2.03652639338397));
#94283=CARTESIAN_POINT('Ctrl Pts',(-10.0002405443076,24.3342937225662,2.03649318268341));
#94284=CARTESIAN_POINT('Ctrl Pts',(-9.99576699208508,24.3340517670489,2.03649928443706));
#94285=CARTESIAN_POINT('Ctrl Pts',(-9.98550691261684,24.3334982885705,2.03656032367706));
#94286=CARTESIAN_POINT('Ctrl Pts',(-9.97972052119056,24.3331871974598,2.03662906962207));
#94287=CARTESIAN_POINT('Ctrl Pts',(-9.96368942687116,24.3323281668534,2.0369146334498));
#94288=CARTESIAN_POINT('Ctrl Pts',(-9.95344625330707,24.3317825018007,2.037204729516));
#94289=CARTESIAN_POINT('Ctrl Pts',(-9.89376184005028,24.3286206928419,2.03952261434719));
#94290=CARTESIAN_POINT('Ctrl Pts',(-9.84444344419266,24.3260801876343,2.04394932739963));
#94291=CARTESIAN_POINT('Ctrl Pts',(-9.67874424122476,24.3176762772866,2.06733942607496));
#94292=CARTESIAN_POINT('Ctrl Pts',(-9.5644742715828,24.3121353977366,2.097845719034));
#94293=CARTESIAN_POINT('Ctrl Pts',(-9.44582016518994,24.3057541781828,2.14544582514436));
#94294=CARTESIAN_POINT('Ctrl Pts',(-9.43657528336014,24.3052523614222,2.14926505749606));
#94295=CARTESIAN_POINT('Ctrl Pts',(-9.39416734121248,24.3029260398728,2.16729569182307));
#94296=CARTESIAN_POINT('Ctrl Pts',(-9.36150016062898,24.3010649588785,2.18263462332949));
#94297=CARTESIAN_POINT('Ctrl Pts',(-9.32416998150307,24.298819703213,2.2018778439513));
#94298=CARTESIAN_POINT('Ctrl Pts',(-9.31892087339443,24.2985011914166,2.20462416000015));
#94299=CARTESIAN_POINT('Ctrl Pts',(-9.31052036262235,24.2979867175908,2.20908445367893));
#94300=CARTESIAN_POINT('Ctrl Pts',(-9.30735828213727,24.29779197635,2.2107783091303));
#94301=CARTESIAN_POINT('Ctrl Pts',(-9.30174228573925,24.2974441155898,2.21381329707106));
#94302=CARTESIAN_POINT('Ctrl Pts',(-9.2992859500533,24.297291284266,2.21514985682126));
#94303=CARTESIAN_POINT('Ctrl Pts',(-9.29404143577756,24.2969634923553,2.21802305388046));
#94304=CARTESIAN_POINT('Ctrl Pts',(-9.291254480004,24.2967884078324,2.21956172649082));
#94305=CARTESIAN_POINT('Ctrl Pts',(-9.28362273490776,24.2963065488991,2.22380774727159));
#94306=CARTESIAN_POINT('Ctrl Pts',(-9.27878834276833,24.2959986355492,2.22653355155644));
#94307=CARTESIAN_POINT('Ctrl Pts',(-9.25295986205717,24.2943396628485,2.24129082328629));
#94308=CARTESIAN_POINT('Ctrl Pts',(-9.23225223680887,24.2929601906867,2.2538134205982));
#94309=CARTESIAN_POINT('Ctrl Pts',(-9.16917210382241,24.2886254431122,2.29412912856841));
#94310=CARTESIAN_POINT('Ctrl Pts',(-9.1279266467284,24.285601309655,2.32361273170463));
#94311=CARTESIAN_POINT('Ctrl Pts',(-8.98507538527094,24.2746257515227,2.43737503485389));
#94312=CARTESIAN_POINT('Ctrl Pts',(-8.89342298214994,24.2666729412143,2.53317828308894));
#94313=CARTESIAN_POINT('Ctrl Pts',(-8.80682578562209,24.2584564928517,2.65241312861247));
#94314=CARTESIAN_POINT('Ctrl Pts',(-8.79799500966825,24.2576074437074,2.66498368942001));
#94315=CARTESIAN_POINT('Ctrl Pts',(-8.78592761066472,24.2564308694675,2.68274980726382));
#94316=CARTESIAN_POINT('Ctrl Pts',(-8.78252338927163,24.2560970608161,2.687829852805));
#94317=CARTESIAN_POINT('Ctrl Pts',(-8.77634754064163,24.2554879234222,2.69717202738611));
#94318=CARTESIAN_POINT('Ctrl Pts',(-8.77356610215866,24.2552122314031,2.7014275298766));
#94319=CARTESIAN_POINT('Ctrl Pts',(-8.76797705494692,24.2546554577014,2.7100766506332));
#94320=CARTESIAN_POINT('Ctrl Pts',(-8.76517063793304,24.2543744226549,2.71447095371354));
#94321=CARTESIAN_POINT('Ctrl Pts',(-8.758308304691,24.2536835381748,2.72534368765688));
#94322=CARTESIAN_POINT('Ctrl Pts',(-8.75427951576073,24.2532746870019,2.73183911411364));
#94323=CARTESIAN_POINT('Ctrl Pts',(-8.73952950569231,24.2517653731785,2.75604110506058));
#94324=CARTESIAN_POINT('Ctrl Pts',(-8.72913313845304,24.2506766612723,2.77394340370713));
#94325=CARTESIAN_POINT('Ctrl Pts',(-8.66933680169356,24.244249431691,2.88213342220499));
#94326=CARTESIAN_POINT('Ctrl Pts',(-8.62919274718192,24.2392508083272,2.9772061041372));
#94327=CARTESIAN_POINT('Ctrl Pts',(-8.57393229098751,24.2299845664,3.15963009151653));
#94328=CARTESIAN_POINT('Ctrl Pts',(-8.55610762734898,24.2257268958965,3.24565384453934));
#94329=CARTESIAN_POINT('Ctrl Pts',(-8.54480362005008,24.2205090372751,3.34391594620524));
#94330=CARTESIAN_POINT('Ctrl Pts',(-8.54364716817559,24.2199097696098,3.35510296770986));
#94331=CARTESIAN_POINT('Ctrl Pts',(-8.54222167444811,24.2190688099773,3.37064160102376));
#94332=CARTESIAN_POINT('Ctrl Pts',(-8.54184294377679,24.2188329207025,3.37498304021043));
#94333=CARTESIAN_POINT('Ctrl Pts',(-8.54126679376097,24.2184529799122,3.38194663290108));
#94334=CARTESIAN_POINT('Ctrl Pts',(-8.54105703829013,24.2183096094216,3.38456777434806));
#94335=CARTESIAN_POINT('Ctrl Pts',(-8.54063314508165,24.2180089354005,3.39005061177839));
#94336=CARTESIAN_POINT('Ctrl Pts',(-8.54042035956009,24.2178515550498,3.39291238178762));
#94337=CARTESIAN_POINT('Ctrl Pts',(-8.53992402273555,24.2174682050402,3.39986409808154));
#94338=CARTESIAN_POINT('Ctrl Pts',(-8.53964923918421,24.2172417546554,3.40395463161733));
#94339=CARTESIAN_POINT('Ctrl Pts',(-8.53873799852227,24.2164374843061,3.41842892120816));
#94340=CARTESIAN_POINT('Ctrl Pts',(-8.53819509216671,24.2158547898865,3.42881800327112));
#94341=CARTESIAN_POINT('Ctrl Pts',(-8.53554173370634,24.2122453841602,3.49264340472883));
#94342=CARTESIAN_POINT('Ctrl Pts',(-8.53625101826255,24.2090932502014,3.54615220639344));
#94343=CARTESIAN_POINT('Ctrl Pts',(-8.54639665401212,24.2001726816885,3.69503926894906));
#94344=CARTESIAN_POINT('Ctrl Pts',(-8.5622701647745,24.1943433812652,3.78972124706008));
#94345=CARTESIAN_POINT('Ctrl Pts',(-8.59350079636938,24.1873406105241,3.90516603482704));
#94346=CARTESIAN_POINT('Ctrl Pts',(-8.6002809811674,24.185959421648,3.92800265788734));
#94347=CARTESIAN_POINT('Ctrl Pts',(-8.61852655509086,24.1825629590765,3.98437463994475));
#94348=CARTESIAN_POINT('Ctrl Pts',(-8.63065850041411,24.1805682148269,4.01767927569416));
#94349=CARTESIAN_POINT('Ctrl Pts',(-8.64762824433548,24.1780790606336,4.0594787953523));
#94350=CARTESIAN_POINT('Ctrl Pts',(-8.65135713281831,24.1775481172202,4.06840857759662));
#94351=CARTESIAN_POINT('Ctrl Pts',(-8.65740781018749,24.1767112338042,4.08250366445936));
#94352=CARTESIAN_POINT('Ctrl Pts',(-8.65967143679712,24.1764033464329,4.08769350104765));
#94353=CARTESIAN_POINT('Ctrl Pts',(-8.66396471900413,24.1758289588639,4.09738291026805));
#94354=CARTESIAN_POINT('Ctrl Pts',(-8.66598712543226,24.1755622181436,4.10188559117097));
#94355=CARTESIAN_POINT('Ctrl Pts',(-8.67059721555972,24.174962684309,4.11201209850057));
#94356=CARTESIAN_POINT('Ctrl Pts',(-8.67319788899172,24.1746303391109,4.11762993112479));
#94357=CARTESIAN_POINT('Ctrl Pts',(-8.68101397159529,24.1736485552074,4.13423659392936));
#94358=CARTESIAN_POINT('Ctrl Pts',(-8.68633088673907,24.1730025977637,4.14517724147775));
#94359=CARTESIAN_POINT('Ctrl Pts',(-8.7387012037998,24.1668418201424,4.24960776469685));
#94360=CARTESIAN_POINT('Ctrl Pts',(-8.79551960920961,24.1617043001886,4.33786437117493));
#94361=CARTESIAN_POINT('Ctrl Pts',(-8.92319594397368,24.1518175200531,4.49601335112564));
#94362=CARTESIAN_POINT('Ctrl Pts',(-8.99270107425714,24.147077589766,4.566252102984));
#94363=CARTESIAN_POINT('Ctrl Pts',(-9.0771029604954,24.1412999155452,4.63587466367133));
#94364=CARTESIAN_POINT('Ctrl Pts',(-9.08555719991905,24.1407208259081,4.64269179949379));
#94365=CARTESIAN_POINT('Ctrl Pts',(-9.09746296763309,24.1399035955974,4.65207536213955));
#94366=CARTESIAN_POINT('Ctrl Pts',(-9.1008513290916,24.1396708215779,4.65472178532317));
#94367=CARTESIAN_POINT('Ctrl Pts',(-9.10632434798996,24.1392944404083,4.658957700309));
#94368=CARTESIAN_POINT('Ctrl Pts',(-9.10840172747276,24.1391514874416,4.66055660883204));
#94369=CARTESIAN_POINT('Ctrl Pts',(-9.11277197244891,24.1388505365662,4.66390162096455));
#94370=CARTESIAN_POINT('Ctrl Pts',(-9.11506570633544,24.1386924553217,4.66564653802022));
#94371=CARTESIAN_POINT('Ctrl Pts',(-9.12068308571926,24.1383050344389,4.66989372269628));
#94372=CARTESIAN_POINT('Ctrl Pts',(-9.12401226370448,24.1380751905223,4.67238860585257));
#94373=CARTESIAN_POINT('Ctrl Pts',(-9.13601693227755,24.1372456891179,4.68130521534761));
#94374=CARTESIAN_POINT('Ctrl Pts',(-9.14475255003708,24.136640752458,4.68764495468732));
#94375=CARTESIAN_POINT('Ctrl Pts',(-9.20051276717484,24.1327752834402,4.72717785975241));
#94376=CARTESIAN_POINT('Ctrl Pts',(-9.24938739575732,24.1293705979757,4.75766643117006));
#94377=CARTESIAN_POINT('Ctrl Pts',(-9.33601776407901,24.1234610978858,4.80485595855693));
#94378=CARTESIAN_POINT('Ctrl Pts',(-9.37292259939883,24.1209793509464,4.82298729827759));
#94379=CARTESIAN_POINT('Ctrl Pts',(-9.49925217401818,24.1126819079522,4.87857801169276));
#94380=CARTESIAN_POINT('Ctrl Pts',(-9.59163321917607,24.1069560473513,4.90871133357948));
#94381=CARTESIAN_POINT('Ctrl Pts',(-9.70312365076309,24.1005696421488,4.93317562455307));
#94382=CARTESIAN_POINT('Ctrl Pts',(-9.71998373812841,24.0996167690119,4.93656495365636));
#94383=CARTESIAN_POINT('Ctrl Pts',(-9.74410159331199,24.0982715838354,4.94097253549342));
#94384=CARTESIAN_POINT('Ctrl Pts',(-9.7513128824114,24.0978716311227,4.94223457276102));
#94385=CARTESIAN_POINT('Ctrl Pts',(-9.76356474583563,24.0971958781554,4.94428412825072));
#94386=CARTESIAN_POINT('Ctrl Pts',(-9.76860047041574,24.0969192065697,4.94509948832378));
#94387=CARTESIAN_POINT('Ctrl Pts',(-9.77878198775772,24.0963619507379,4.9466934453799));
#94388=CARTESIAN_POINT('Ctrl Pts',(-9.78392787724483,24.096081404227,4.94747095742117));
#94389=CARTESIAN_POINT('Ctrl Pts',(-9.79657705425232,24.0953944361364,4.9493132118683));
#94390=CARTESIAN_POINT('Ctrl Pts',(-9.80408472081647,24.0949889836757,4.95034716094596));
#94391=CARTESIAN_POINT('Ctrl Pts',(-9.83164858846582,24.0935084963069,4.95392529526432));
#94392=CARTESIAN_POINT('Ctrl Pts',(-9.85174936899462,24.0924446048277,4.9561122089326));
#94393=CARTESIAN_POINT('Ctrl Pts',(-9.95793437632452,24.0868980389183,4.96544313863447));
#94394=CARTESIAN_POINT('Ctrl Pts',(-10.044482138714,24.082644767287,4.96537246235983));
#94395=CARTESIAN_POINT('Ctrl Pts',(-10.1498797483258,24.0774922705189,4.95593471421279));
#94396=CARTESIAN_POINT('Ctrl Pts',(-10.1691973472546,24.0765483659117,4.95381638818162));
#94397=CARTESIAN_POINT('Ctrl Pts',(-10.2730308924274,24.0714564070366,4.94033260691188));
#94398=CARTESIAN_POINT('Ctrl Pts',(-10.3564637043396,24.0673058268442,4.92198246495188));
#94399=CARTESIAN_POINT('Ctrl Pts',(-10.4485863038485,24.0622131318139,4.8931008714851));
#94400=CARTESIAN_POINT('Ctrl Pts',(-10.459319336881,24.0616115879296,4.88959902180716));
#94401=CARTESIAN_POINT('Ctrl Pts',(-10.4741464832155,24.0607678031505,4.88457084922579));
#94402=CARTESIAN_POINT('Ctrl Pts',(-10.4782761622519,24.0605314060915,4.88314975172676));
#94403=CARTESIAN_POINT('Ctrl Pts',(-10.4848852624666,24.0601507638355,4.88084230279655));
#94404=CARTESIAN_POINT('Ctrl Pts',(-10.4873687931607,24.0600072025104,4.87996769606254));
#94405=CARTESIAN_POINT('Ctrl Pts',(-10.4925529236495,24.059706406538,4.87812629877421));
#94406=CARTESIAN_POINT('Ctrl Pts',(-10.4952530469698,24.0595490964187,4.87715826867005));
#94407=CARTESIAN_POINT('Ctrl Pts',(-10.5018003738325,24.0591661149236,4.87478921978362));
#94408=CARTESIAN_POINT('Ctrl Pts',(-10.5056445650871,24.0589399647994,4.87337998637585));
#94409=CARTESIAN_POINT('Ctrl Pts',(-10.5187831568519,24.0581627485124,4.86850089963037));
#94410=CARTESIAN_POINT('Ctrl Pts',(-10.5280479532947,24.0576073261653,4.86495275528486));
#94411=CARTESIAN_POINT('Ctrl Pts',(-10.5507572792709,24.0562289917525,4.85598994606123));
#94412=CARTESIAN_POINT('Ctrl Pts',(-10.5641586127851,24.0554008757033,4.85046930531036));
#94413=CARTESIAN_POINT('Ctrl Pts',(-10.6168693683716,24.0520912107425,4.82783376687953));
#94414=CARTESIAN_POINT('Ctrl Pts',(-10.655498804781,24.0495494790711,4.80919486663624));
#94415=CARTESIAN_POINT('Ctrl Pts',(-10.7688477599786,24.0418433300742,4.74822810396001));
#94416=CARTESIAN_POINT('Ctrl Pts',(-10.8407253467814,24.036628656488,4.70099239909976));
#94417=CARTESIAN_POINT('Ctrl Pts',(-10.9572354004524,24.0278862082785,4.60881301122854));
#94418=CARTESIAN_POINT('Ctrl Pts',(-11.003873602144,24.0242881469058,4.56677331728973));
#94419=CARTESIAN_POINT('Ctrl Pts',(-11.0548360313142,24.0202470080194,4.51452372073893));
#94420=CARTESIAN_POINT('Ctrl Pts',(-11.0619197808835,24.0196825001892,4.50710665741033));
#94421=CARTESIAN_POINT('Ctrl Pts',(-11.0732984658576,24.0187709948098,4.49493901820026));
#94422=CARTESIAN_POINT('Ctrl Pts',(-11.0776411337006,24.0184219705346,4.49023372772759));
#94423=CARTESIAN_POINT('Ctrl Pts',(-11.0853200322576,24.0178026971717,4.48180328051215));
#94424=CARTESIAN_POINT('Ctrl Pts',(-11.0886682933413,24.0175319439779,4.47808926074207));
#94425=CARTESIAN_POINT('Ctrl Pts',(-11.0956868590616,24.0169628157268,4.47022330680425));
#94426=CARTESIAN_POINT('Ctrl Pts',(-11.0993527553319,24.0166646262469,4.46606753319355));
#94427=CARTESIAN_POINT('Ctrl Pts',(-11.106753876334,24.0160606630876,4.45758070939539));
#94428=CARTESIAN_POINT('Ctrl Pts',(-11.1104874958876,24.015754957724,4.45324838343436));
#94429=CARTESIAN_POINT('Ctrl Pts',(-11.1265352423983,24.0144363760583,4.43440505110665));
#94430=CARTESIAN_POINT('Ctrl Pts',(-11.138591369394,24.0134339348372,4.41967613295051));
#94431=CARTESIAN_POINT('Ctrl Pts',(-11.1878677699537,24.0092799168571,4.35702058804743));
#94432=CARTESIAN_POINT('Ctrl Pts',(-11.2223776735103,24.0062326820263,4.30703651282465));
#94433=CARTESIAN_POINT('Ctrl Pts',(-11.2797235512721,24.000756266381,4.21181928121408));
#94434=CARTESIAN_POINT('Ctrl Pts',(-11.3035067690404,23.9983122670245,4.16727001302749));
#94435=CARTESIAN_POINT('Ctrl Pts',(-11.3594137157013,23.991907013445,4.04810064909302));
#94436=CARTESIAN_POINT('Ctrl Pts',(-11.3877099373611,23.9879410339104,3.97188781795715));
#94437=CARTESIAN_POINT('Ctrl Pts',(-11.4125899330435,23.9830633151568,3.88281895045071));
#94438=CARTESIAN_POINT('Ctrl Pts',(-11.4155117208977,23.9824595620678,3.87186989673844));
#94439=CARTESIAN_POINT('Ctrl Pts',(-11.4193846037964,23.9816131622765,3.85664930879598));
#94440=CARTESIAN_POINT('Ctrl Pts',(-11.4204442065977,23.9813764072504,3.8524055020941));
#94441=CARTESIAN_POINT('Ctrl Pts',(-11.4221114316054,23.98099534016,3.84559841651867));
#94442=CARTESIAN_POINT('Ctrl Pts',(-11.4227311937402,23.9808517148989,3.84303810216134));
#94443=CARTESIAN_POINT('Ctrl Pts',(-11.4240111943254,23.9805508974935,3.83768712177561));
#94444=CARTESIAN_POINT('Ctrl Pts',(-11.4246701443856,23.9803936305015,3.8348961824285));
#94445=CARTESIAN_POINT('Ctrl Pts',(-11.426248803378,23.9800109855722,3.82812089530692));
#94446=CARTESIAN_POINT('Ctrl Pts',(-11.4271600213203,23.979785131083,3.82413460751766));
#94447=CARTESIAN_POINT('Ctrl Pts',(-11.4290684616233,23.9793013466763,3.81562171441978));
#94448=CARTESIAN_POINT('Ctrl Pts',(-11.4300609069921,23.9790431640214,3.81109409470195));
#94449=CARTESIAN_POINT('Ctrl Pts',(-11.4348169732641,23.9777731107869,3.78889276379791));
#94450=CARTESIAN_POINT('Ctrl Pts',(-11.4382743937767,23.9767459190681,3.77115583004349));
#94451=CARTESIAN_POINT('Ctrl Pts',(-11.45603124916,23.970841939527,3.67013457373519));
#94452=CARTESIAN_POINT('Ctrl Pts',(-11.4634233187998,23.9657175935564,3.585805604991));
#94453=CARTESIAN_POINT('Ctrl Pts',(-11.4634994065207,23.9606357315493,3.50131799604382));
#94454=CARTESIAN_POINT('Ctrl Pts',(-11.4634994065687,23.9606357283428,3.50131794273411));
#94455=CARTESIAN_POINT('Ctrl Pts',(-11.4634998021939,23.9606093036564,3.50087862372563));
#94456=CARTESIAN_POINT('Ctrl Pts',(-11.4635,23.9605828803629,3.50043930947062));
#94457=CARTESIAN_POINT('Ctrl Pts',(-11.4635,23.9605564584951,3.50000000010085));
#94458=CARTESIAN_POINT('Ctrl Pts',(-11.4635,23.8891760003868,3.49999987117833));
#94459=CARTESIAN_POINT('Ctrl Pts',(-11.4635000043558,23.8915819689193,3.54948511583872));
#94460=CARTESIAN_POINT('Ctrl Pts',(-11.4609901519458,23.8939896094975,3.59896532125907));
#94461=CARTESIAN_POINT('Ctrl Pts',(-11.454965132913,23.8969582981221,3.65813760143904));
#94462=CARTESIAN_POINT('Ctrl Pts',(-11.4538576145332,23.8974569041636,3.66801508877796));
#94463=CARTESIAN_POINT('Ctrl Pts',(-11.4482522193293,23.8997847642009,3.7137912154954));
#94464=CARTESIAN_POINT('Ctrl Pts',(-11.442525069736,23.9016507411869,3.74952393081664));
#94465=CARTESIAN_POINT('Ctrl Pts',(-11.4343256065951,23.9039015782604,3.79082207375434));
#94466=CARTESIAN_POINT('Ctrl Pts',(-11.4331353011141,23.9042204339671,3.79663214700676));
#94467=CARTESIAN_POINT('Ctrl Pts',(-11.4311678069335,23.9047354126907,3.80594745979007));
#94468=CARTESIAN_POINT('Ctrl Pts',(-11.4304129643129,23.9049303121381,3.8094574134188));
#94469=CARTESIAN_POINT('Ctrl Pts',(-11.4290467030395,23.9052784558143,3.81569859669613));
#94470=CARTESIAN_POINT('Ctrl Pts',(-11.4284403564398,23.9054314114728,3.81843088954174));
#94471=CARTESIAN_POINT('Ctrl Pts',(-11.4271267564389,23.9057595222497,3.82427091895385));
#94472=CARTESIAN_POINT('Ctrl Pts',(-11.4264171990844,23.9059348017707,3.82737804077043));
#94473=CARTESIAN_POINT('Ctrl Pts',(-11.4244429828954,23.9064171559432,3.83589477806128));
#94474=CARTESIAN_POINT('Ctrl Pts',(-11.4231576752806,23.9067253707084,3.84129949122094));
#94475=CARTESIAN_POINT('Ctrl Pts',(-11.4161059862807,23.908385427406,3.8702192533847));
#94476=CARTESIAN_POINT('Ctrl Pts',(-11.4097878121441,23.9097656892219,3.89359451711435));
#94477=CARTESIAN_POINT('Ctrl Pts',(-11.3884550623496,23.9141027294769,3.96539756220762));
#94478=CARTESIAN_POINT('Ctrl Pts',(-11.3715023840858,23.917128355793,4.0132084843924));
#94479=CARTESIAN_POINT('Ctrl Pts',(-11.3016412266426,23.9280998971019,4.1818742059472));
#94480=CARTESIAN_POINT('Ctrl Pts',(-11.2349300001728,23.9360468914732,4.29635626870393));
#94481=CARTESIAN_POINT('Ctrl Pts',(-11.1443122588589,23.944259725814,4.41247909054203));
#94482=CARTESIAN_POINT('Ctrl Pts',(-11.1346628484518,23.9451095583647,4.42445058394195));
#94483=CARTESIAN_POINT('Ctrl Pts',(-11.1209098110972,23.9462872948732,4.44097339168951));
#94484=CARTESIAN_POINT('Ctrl Pts',(-11.1169637816443,23.9466214869798,4.44565408082026));
#94485=CARTESIAN_POINT('Ctrl Pts',(-11.1096832255637,23.9472313570204,4.45418095681914));
#94486=CARTESIAN_POINT('Ctrl Pts',(-11.1063577942191,23.9475073984856,4.45803475486801));
#94487=CARTESIAN_POINT('Ctrl Pts',(-11.0995807757439,23.9480649138154,4.46580620599107));
#94488=CARTESIAN_POINT('Ctrl Pts',(-11.0961281933649,23.9483463407409,4.46972289578022));
#94489=CARTESIAN_POINT('Ctrl Pts',(-11.0875620169128,23.9490382602046,4.47933636172204));
#94490=CARTESIAN_POINT('Ctrl Pts',(-11.0824245125678,23.9494477520653,4.48501168908409));
#94491=CARTESIAN_POINT('Ctrl Pts',(-11.0632030982987,23.9509599390239,4.50591331926932));
#94492=CARTESIAN_POINT('Ctrl Pts',(-11.048840166506,23.952050846162,4.5208804023639));
#94493=CARTESIAN_POINT('Ctrl Pts',(-10.9618375290716,23.9584439026487,4.6077675841196));
#94494=CARTESIAN_POINT('Ctrl Pts',(-10.8821434031152,23.9634118528417,4.6722225832342));
#94495=CARTESIAN_POINT('Ctrl Pts',(-10.7223357933823,23.9726730174311,4.77587277489688));
#94496=CARTESIAN_POINT('Ctrl Pts',(-10.644112044499,23.9769565313717,4.81709389213275));
#94497=CARTESIAN_POINT('Ctrl Pts',(-10.5522968611014,23.9822037846373,4.8553326346104));
#94498=CARTESIAN_POINT('Ctrl Pts',(-10.5418805347667,23.9828022238575,4.85953074404555));
#94499=CARTESIAN_POINT('Ctrl Pts',(-10.5273559775163,23.9836423778154,4.86519116680553));
#94500=CARTESIAN_POINT('Ctrl Pts',(-10.5232877110615,23.9838783160043,4.86675572777747));
#94501=CARTESIAN_POINT('Ctrl Pts',(-10.5167516378089,23.9842584492258,4.86923589020384));
#94502=CARTESIAN_POINT('Ctrl Pts',(-10.5142882119134,23.984401964313,4.87016306075622));
#94503=CARTESIAN_POINT('Ctrl Pts',(-10.5091321143925,23.984702885859,4.87208782000409));
#94504=CARTESIAN_POINT('Ctrl Pts',(-10.5064390018102,23.9848603690552,4.87308413168626));
#94505=CARTESIAN_POINT('Ctrl Pts',(-10.4998883050112,23.9852441455079,4.87548565542237));
#94506=CARTESIAN_POINT('Ctrl Pts',(-10.4960277188141,23.9854709215557,4.87688256837301));
#94507=CARTESIAN_POINT('Ctrl Pts',(-10.4823320277322,23.9862774204521,4.88177313634685));
#94508=CARTESIAN_POINT('Ctrl Pts',(-10.4724657188922,23.9868620527773,4.88517772037454));
#94509=CARTESIAN_POINT('Ctrl Pts',(-10.4115053612533,23.9904928858565,4.90548636617494));
#94510=CARTESIAN_POINT('Ctrl Pts',(-10.3595514995227,23.9936660389887,4.91966554760186));
#94511=CARTESIAN_POINT('Ctrl Pts',(-10.2157773343699,24.0024576494598,4.95050523950782));
#94512=CARTESIAN_POINT('Ctrl Pts',(-10.1229461244701,24.0081311254835,4.9613048076366));
#94513=CARTESIAN_POINT('Ctrl Pts',(-9.97114050030912,24.0170366965516,4.96438793015942));
#94514=CARTESIAN_POINT('Ctrl Pts',(-9.91254056453779,24.0203889666485,4.96205918234024));
#94515=CARTESIAN_POINT('Ctrl Pts',(-9.84415403662922,24.0241932452024,4.95521368491433));
#94516=CARTESIAN_POINT('Ctrl Pts',(-9.83408664419578,24.0247506209567,4.95410027119156));
#94517=CARTESIAN_POINT('Ctrl Pts',(-9.81771171283066,24.0256530103098,4.95211699087268));
#94518=CARTESIAN_POINT('Ctrl Pts',(-9.81139697945031,24.0259999832322,4.95131033113232));
#94519=CARTESIAN_POINT('Ctrl Pts',(-9.80013404194938,24.0266170737867,4.94979682371275));
#94520=CARTESIAN_POINT('Ctrl Pts',(-9.79518384500367,24.0268876812026,4.94910578452636));
#94521=CARTESIAN_POINT('Ctrl Pts',(-9.78472832007381,24.0274579845106,4.94759156483295));
#94522=CARTESIAN_POINT('Ctrl Pts',(-9.77922394339953,24.0277574853152,4.94676230555027));
#94523=CARTESIAN_POINT('Ctrl Pts',(-9.76459060859419,24.0285518061867,4.94447226949521));
#94524=CARTESIAN_POINT('Ctrl Pts',(-9.75547045132066,24.0290448910683,4.94295634861191));
#94525=CARTESIAN_POINT('Ctrl Pts',(-9.71178536894021,24.0313979281198,4.93526909089378));
#94526=CARTESIAN_POINT('Ctrl Pts',(-9.67743423820888,24.033221279083,4.92794139350722));
#94527=CARTESIAN_POINT('Ctrl Pts',(-9.58004944210803,24.0383435634105,4.90347335450942));
#94528=CARTESIAN_POINT('Ctrl Pts',(-9.51785385010775,24.0415546649996,4.88334083163357));
#94529=CARTESIAN_POINT('Ctrl Pts',(-9.35586305284131,24.0500539680569,4.81864658826274));
#94530=CARTESIAN_POINT('Ctrl Pts',(-9.25937683698116,24.055251907348,4.76696965515162));
#94531=CARTESIAN_POINT('Ctrl Pts',(-9.16126827220221,24.0615564492934,4.69935913982343));
#94532=CARTESIAN_POINT('Ctrl Pts',(-9.15305197798639,24.0620930970591,4.69357123558492));
#94533=CARTESIAN_POINT('Ctrl Pts',(-9.14185345554479,24.0628374597779,4.68550867367234));
#94534=CARTESIAN_POINT('Ctrl Pts',(-9.13881919998386,24.0630404663896,4.6833063576978));
#94535=CARTESIAN_POINT('Ctrl Pts',(-9.13364684044202,24.0633888478916,4.6795217369945));
#94536=CARTESIAN_POINT('Ctrl Pts',(-9.13150451014229,24.0635338299707,4.67794520627324));
#94537=CARTESIAN_POINT('Ctrl Pts',(-9.1270755372757,24.0638350122379,4.67466729581145));
#94538=CARTESIAN_POINT('Ctrl Pts',(-9.12478956608063,24.0639912738644,4.67296507592236));
#94539=CARTESIAN_POINT('Ctrl Pts',(-9.11931538344049,24.0643673918053,4.66886388262));
#94540=CARTESIAN_POINT('Ctrl Pts',(-9.11613199115101,24.0645876857661,4.66645853423958));
#94541=CARTESIAN_POINT('Ctrl Pts',(-9.10523038183066,24.06534738344,4.65815110679264));
#94542=CARTESIAN_POINT('Ctrl Pts',(-9.09756129863414,24.0658909861196,4.65218533043863));
#94543=CARTESIAN_POINT('Ctrl Pts',(-9.05334967454546,24.069075678057,4.61708093750482));
#94544=CARTESIAN_POINT('Ctrl Pts',(-9.01816315329134,24.0718137525028,4.58628371677107));
#94545=CARTESIAN_POINT('Ctrl Pts',(-8.88425962363714,24.0828799742192,4.45725581302095));
#94546=CARTESIAN_POINT('Ctrl Pts',(-8.79827916926299,24.0914052414053,4.3468149000219));
#94547=CARTESIAN_POINT('Ctrl Pts',(-8.71648020514208,24.1007454651063,4.20361005832185));
#94548=CARTESIAN_POINT('Ctrl Pts',(-8.70434521070886,24.1021782090747,4.18100584561681));
#94549=CARTESIAN_POINT('Ctrl Pts',(-8.68894412817977,24.1040634358401,4.15041422529998));
#94550=CARTESIAN_POINT('Ctrl Pts',(-8.68514585918608,24.1045343071191,4.14270114074868));
#94551=CARTESIAN_POINT('Ctrl Pts',(-8.67906257946168,24.1052983974281,4.13006824853465));
#94552=CARTESIAN_POINT('Ctrl Pts',(-8.67673660075418,24.1055930238141,4.12516849257649));
#94553=CARTESIAN_POINT('Ctrl Pts',(-8.67230296855575,24.1061594829812,4.11569328226447));
#94554=CARTESIAN_POINT('Ctrl Pts',(-8.6701915979154,24.1064314402393,4.11111966074841));
#94555=CARTESIAN_POINT('Ctrl Pts',(-8.66534427996868,24.10706101034,4.10047539121013));
#94556=CARTESIAN_POINT('Ctrl Pts',(-8.66262605257737,24.1074180159052,4.09439676413424));
#94557=CARTESIAN_POINT('Ctrl Pts',(-8.65408769492063,24.10855240534,4.07494778093965));
#94558=CARTESIAN_POINT('Ctrl Pts',(-8.64842576462139,24.1093244479378,4.06150867335387));
#94559=CARTESIAN_POINT('Ctrl Pts',(-8.62098454719638,24.1131723669102,3.9935532502429));
#94560=CARTESIAN_POINT('Ctrl Pts',(-8.60229746581209,24.1161446284507,3.93784361434993));
#94561=CARTESIAN_POINT('Ctrl Pts',(-8.57043543326116,24.1222073100312,3.81972742493916));
#94562=CARTESIAN_POINT('Ctrl Pts',(-8.55788797834093,24.1252800684441,3.75728116641249));
#94563=CARTESIAN_POINT('Ctrl Pts',(-8.53844088193275,24.1324185784115,3.61203563974093));
#94564=CARTESIAN_POINT('Ctrl Pts',(-8.53444277571061,24.1364895465003,3.52907818508724));
#94565=CARTESIAN_POINT('Ctrl Pts',(-8.53774861244331,24.141292827249,3.43914295336232));
#94566=CARTESIAN_POINT('Ctrl Pts',(-8.53806118792228,24.1416744833725,3.4320470294758));
#94567=CARTESIAN_POINT('Ctrl Pts',(-8.53860558341159,24.1422491064967,3.42144456474463));
#94568=CARTESIAN_POINT('Ctrl Pts',(-8.53879840540502,24.142439974825,3.41793602087497));
#94569=CARTESIAN_POINT('Ctrl Pts',(-8.53916678214476,24.1427834618995,3.41164659765739));
#94570=CARTESIAN_POINT('Ctrl Pts',(-8.53933764484853,24.1429358188396,3.40886549411152));
#94571=CARTESIAN_POINT('Ctrl Pts',(-8.53972696334491,24.1432685303449,3.40281116426846));
#94572=CARTESIAN_POINT('Ctrl Pts',(-8.53994847960029,24.1434490480574,3.39953822261322));
#94573=CARTESIAN_POINT('Ctrl Pts',(-8.54060515491769,24.1439605411897,3.39029701038639));
#94574=CARTESIAN_POINT('Ctrl Pts',(-8.54106591327014,24.1442928905258,3.38433069622246));
#94575=CARTESIAN_POINT('Ctrl Pts',(-8.54416354205071,24.1463743617964,3.34718852607133));
#94576=CARTESIAN_POINT('Ctrl Pts',(-8.54776282814729,24.1481711479144,3.31610315316027));
#94577=CARTESIAN_POINT('Ctrl Pts',(-8.57659269711208,24.1596470917269,3.12184091109836));
#94578=CARTESIAN_POINT('Ctrl Pts',(-8.62829057149899,24.1699090742136,2.96378307721295));
#94579=CARTESIAN_POINT('Ctrl Pts',(-8.71561776615167,24.1804657712711,2.79808543613992));
#94580=CARTESIAN_POINT('Ctrl Pts',(-8.72637634017,24.1816977525921,2.77874787629847));
#94581=CARTESIAN_POINT('Ctrl Pts',(-8.74167286457121,24.1833602264146,2.75266415780829));
#94582=CARTESIAN_POINT('Ctrl Pts',(-8.7458341961306,24.1838040745777,2.74570153062397));
#94583=CARTESIAN_POINT('Ctrl Pts',(-8.75254242356152,24.1845064618376,2.73468650437593));
#94584=CARTESIAN_POINT('Ctrl Pts',(-8.75505164279409,24.1847663593352,2.73061145040577));
#94585=CARTESIAN_POINT('Ctrl Pts',(-8.76023678109076,24.1852976901061,2.7222823990478));
#94586=CARTESIAN_POINT('Ctrl Pts',(-8.76291471622812,24.1855690449882,2.71802972733174));
#94587=CARTESIAN_POINT('Ctrl Pts',(-8.76915106414651,24.186194007994,2.7082383661729));
#94588=CARTESIAN_POINT('Ctrl Pts',(-8.77272506422185,24.1865470367011,2.70270970052696));
#94589=CARTESIAN_POINT('Ctrl Pts',(-8.78411423913461,24.1876561490568,2.68534969598379));
#94590=CARTESIAN_POINT('Ctrl Pts',(-8.79206424598193,24.1884072258325,2.67360751812575));
#94591=CARTESIAN_POINT('Ctrl Pts',(-8.83206576341668,24.1920776431233,2.61633608360049));
#94592=CARTESIAN_POINT('Ctrl Pts',(-8.86652819296479,24.1949042775574,2.57254390015054));
#94593=CARTESIAN_POINT('Ctrl Pts',(-8.96924678168534,24.2026118408871,2.45632140151088));
#94594=CARTESIAN_POINT('Ctrl Pts',(-9.04250469611667,24.2073288303338,2.38873098545572));
#94595=CARTESIAN_POINT('Ctrl Pts',(-9.13733880729182,24.2132134470591,2.31762389010589));
#94596=CARTESIAN_POINT('Ctrl Pts',(-9.15285428723863,24.2141705663057,2.30645833720846));
#94597=CARTESIAN_POINT('Ctrl Pts',(-9.19557149855446,24.216802894614,2.27696996354199));
#94598=CARTESIAN_POINT('Ctrl Pts',(-9.22317611115832,24.2185009123705,2.25925344294719));
#94599=CARTESIAN_POINT('Ctrl Pts',(-9.25630393470123,24.220563178437,2.23953117916682));
#94600=CARTESIAN_POINT('Ctrl Pts',(-9.26127488604484,24.2208732621228,2.23661142570786));
#94601=CARTESIAN_POINT('Ctrl Pts',(-9.26935953778213,24.2213788110988,2.23192682626655));
#94602=CARTESIAN_POINT('Ctrl Pts',(-9.27246273751292,24.2215731529596,2.23014387031086));
#94603=CARTESIAN_POINT('Ctrl Pts',(-9.27799772085976,24.2219203642975,2.22699067166411));
#94604=CARTESIAN_POINT('Ctrl Pts',(-9.28042691682931,24.2220729472378,2.22561598450397));
#94605=CARTESIAN_POINT('Ctrl Pts',(-9.28567806447831,24.2224032256298,2.22266415033212));
#94606=CARTESIAN_POINT('Ctrl Pts',(-9.28850127220543,24.2225810647352,2.22108942441484));
#94607=CARTESIAN_POINT('Ctrl Pts',(-9.29637271343978,24.2230775994293,2.21673303085421));
#94608=CARTESIAN_POINT('Ctrl Pts',(-9.30143214036592,24.2233975465664,2.21397184489734));
#94609=CARTESIAN_POINT('Ctrl Pts',(-9.33061411064113,24.2252469250134,2.19826877890294));
#94610=CARTESIAN_POINT('Ctrl Pts',(-9.35507824488235,24.2268127916465,2.18597664682072));
#94611=CARTESIAN_POINT('Ctrl Pts',(-9.43634063407504,24.2320298106247,2.14796189524942));
#94612=CARTESIAN_POINT('Ctrl Pts',(-9.4944377235781,24.2357815247438,2.12518186690262));
#94613=CARTESIAN_POINT('Ctrl Pts',(-9.66262407252432,24.2464168834666,2.07134173351853));
#94614=CARTESIAN_POINT('Ctrl Pts',(-9.77516549909753,24.253236527815,2.04936395433782));
#94615=CARTESIAN_POINT('Ctrl Pts',(-9.90579240787828,24.2605606953189,2.03943970870383));
#94616=CARTESIAN_POINT('Ctrl Pts',(-9.92247413307491,24.2614861236123,2.03845930354126));
#94617=CARTESIAN_POINT('Ctrl Pts',(-9.94567707607168,24.2627599950842,2.03749403698348));
#94618=CARTESIAN_POINT('Ctrl Pts',(-9.95218646548796,24.2631159162833,2.03726675714144));
#94619=CARTESIAN_POINT('Ctrl Pts',(-9.96342005339138,24.2637276920648,2.03694959746934));
#94620=CARTESIAN_POINT('Ctrl Pts',(-9.96814353255016,24.2639841818322,2.03683912741972));
#94621=CARTESIAN_POINT('Ctrl Pts',(-9.97792469824924,24.2645137863734,2.03665775873468));
#94622=CARTESIAN_POINT('Ctrl Pts',(-9.98298238882209,24.2647867939368,2.03659020236446));
#94623=CARTESIAN_POINT('Ctrl Pts',(-9.99483158797663,24.2654244666349,2.03649336823946));
#94624=CARTESIAN_POINT('Ctrl Pts',(-10.0016231836129,24.2657884742982,2.03648514148917));
#94625=CARTESIAN_POINT('Ctrl Pts',(-10.0237317577064,24.2669687468812,2.03661226101212));
#94626=CARTESIAN_POINT('Ctrl Pts',(-10.0390468783546,24.26777903056,2.03694079559391));
#94627=CARTESIAN_POINT('Ctrl Pts',(-10.1187939961307,24.2719638076596,2.03990464969452));
#94628=CARTESIAN_POINT('Ctrl Pts',(-10.1830081084489,24.2752119929112,2.04655592005852));
#94629=CARTESIAN_POINT('Ctrl Pts',(-10.3459562420196,24.283365672833,2.07440861991993));
#94630=CARTESIAN_POINT('Ctrl Pts',(-10.4433046342135,24.2881416834927,2.10161688655205));
#94631=CARTESIAN_POINT('Ctrl Pts',(-10.5737851052799,24.2951921807279,2.15309243147087));
#94632=CARTESIAN_POINT('Ctrl Pts',(-10.6098883229884,24.2972198620835,2.16905106551062));
#94633=CARTESIAN_POINT('Ctrl Pts',(-10.6507414859031,24.2996519994487,2.18912070331917));
#94634=CARTESIAN_POINT('Ctrl Pts',(-10.6561666690914,24.2999778574005,2.19182787379549));
#94635=CARTESIAN_POINT('Ctrl Pts',(-10.6648121346717,24.3005019954083,2.19620927761201));
#94636=CARTESIAN_POINT('Ctrl Pts',(-10.6680433400714,24.3006989819193,2.19786194380169));
#94637=CARTESIAN_POINT('Ctrl Pts',(-10.6737603865028,24.301049512546,2.20081292471903));
#94638=CARTESIAN_POINT('Ctrl Pts',(-10.6762486824796,24.3012027540169,2.20210638558195));
#94639=CARTESIAN_POINT('Ctrl Pts',(-10.6815383521137,24.3015299783493,2.20487539243755));
#94640=CARTESIAN_POINT('Ctrl Pts',(-10.6843386154339,24.3017040761191,2.20635285585708));
#94641=CARTESIAN_POINT('Ctrl Pts',(-10.6919498824239,24.3021796113312,2.21040030980002));
#94642=CARTESIAN_POINT('Ctrl Pts',(-10.6967512982756,24.3024821352524,2.21298810138433));
#94643=CARTESIAN_POINT('Ctrl Pts',(-10.7215497981068,24.3040573799705,2.2265330461306));
#94644=CARTESIAN_POINT('Ctrl Pts',(-10.7413022399097,24.3053552391435,2.23792905749997));
#94645=CARTESIAN_POINT('Ctrl Pts',(-10.800114713254,24.3093331385733,2.27371743768528));
#94646=CARTESIAN_POINT('Ctrl Pts',(-10.838296354194,24.3120705094797,2.29949544585657));
#94647=CARTESIAN_POINT('Ctrl Pts',(-10.9203214607578,24.3182083765269,2.36069736831385));
#94648=CARTESIAN_POINT('Ctrl Pts',(-10.963466415326,24.3216147741097,2.39694301047749));
#94649=CARTESIAN_POINT('Ctrl Pts',(-11.0676288404337,24.3301696541822,2.49523392344514));
#94650=CARTESIAN_POINT('Ctrl Pts',(-11.1254101041338,24.3352320369628,2.56040305350164));
#94651=CARTESIAN_POINT('Ctrl Pts',(-11.1834477853916,24.3406449373588,2.63895487391698));
#94652=CARTESIAN_POINT('Ctrl Pts',(-11.1897286762487,24.3412359419211,2.64765438029548));
#94653=CARTESIAN_POINT('Ctrl Pts',(-11.1996468852343,24.3421778555164,2.66171511242194));
#94654=CARTESIAN_POINT('Ctrl Pts',(-11.2033451840857,24.34253107365,2.6670326706173));
#94655=CARTESIAN_POINT('Ctrl Pts',(-11.209851741543,24.3431561397246,2.67652182862578));
#94656=CARTESIAN_POINT('Ctrl Pts',(-11.2126740130567,24.3434285128493,2.6806836543938));
#94657=CARTESIAN_POINT('Ctrl Pts',(-11.2185146019752,24.3439948312592,2.68939269638869));
#94658=CARTESIAN_POINT('Ctrl Pts',(-11.2215290496094,24.3442886293374,2.6939424226746));
#94659=CARTESIAN_POINT('Ctrl Pts',(-11.2293075815342,24.34505077525,2.7058264635067));
#94660=CARTESIAN_POINT('Ctrl Pts',(-11.2340315377667,24.3455176353648,2.71318686821153));
#94661=CARTESIAN_POINT('Ctrl Pts',(-11.2545380122506,24.3475626325797,2.74577706758983));
#94662=CARTESIAN_POINT('Ctrl Pts',(-11.2696154141204,24.3491150417504,2.77144340170441));
#94663=CARTESIAN_POINT('Ctrl Pts',(-11.3082691557988,24.3532506396542,2.84209292728556));
#94664=CARTESIAN_POINT('Ctrl Pts',(-11.330304786355,24.3557839091709,2.88787288368527));
#94665=CARTESIAN_POINT('Ctrl Pts',(-11.3742182370262,24.3613737546387,2.99273820878371));
#94666=CARTESIAN_POINT('Ctrl Pts',(-11.3947516290647,24.3644038546213,3.05227446720345));
#94667=CARTESIAN_POINT('Ctrl Pts',(-11.430270734794,24.3709744280178,3.18179504891252));
#94668=CARTESIAN_POINT('Ctrl Pts',(-11.4440861921214,24.3745205271197,3.25192454721184));
#94669=CARTESIAN_POINT('Ctrl Pts',(-11.4536091432229,24.3787155573626,3.32998385639406));
#94670=CARTESIAN_POINT('Ctrl Pts',(-11.4544351961251,24.3791057884411,3.33720170065257));
#94671=CARTESIAN_POINT('Ctrl Pts',(-11.4555844503232,24.3796908348662,3.34795153787764));
#94672=CARTESIAN_POINT('Ctrl Pts',(-11.4559486198101,24.3798834382273,3.35147915032443));
#94673=CARTESIAN_POINT('Ctrl Pts',(-11.4565761616007,24.3802287331405,3.35778218200639));
#94674=CARTESIAN_POINT('Ctrl Pts',(-11.4568444289099,24.3803811502182,3.36055706502625));
#94675=CARTESIAN_POINT('Ctrl Pts',(-11.4574085595371,24.3807124022988,3.36657165432544));
#94676=CARTESIAN_POINT('Ctrl Pts',(-11.4577015458659,24.380891389665,3.36981153816001));
#94677=CARTESIAN_POINT('Ctrl Pts',(-11.4584925903416,24.3813947887294,3.37889662065334));
#94678=CARTESIAN_POINT('Ctrl Pts',(-11.4589663027267,24.3817205102055,3.38474380843458));
#94679=CARTESIAN_POINT('Ctrl Pts',(-11.4615862143736,24.3836769998825,3.4196915918393));
#94680=CARTESIAN_POINT('Ctrl Pts',(-11.4628967067121,24.3853492480198,3.44884638998033));
#94681=CARTESIAN_POINT('Ctrl Pts',(-11.4634449961681,24.3874770446995,3.48534702905904));
#94682=CARTESIAN_POINT('Ctrl Pts',(-11.4634999998891,24.3879059175572,3.49267432048072));
#94683=CARTESIAN_POINT('Ctrl Pts',(-11.4635,24.3883362350912,3.49999997785042));
#94684=CARTESIAN_POINT('Origin',(-10.,12.3756328852638,3.5));
#94685=CARTESIAN_POINT('',(-9.8111040185181,13.5868901459558,2.33749693734598));
#94686=CARTESIAN_POINT('',(-9.81117889814932,13.4873563446704,2.33776762587097));
#94687=CARTESIAN_POINT('',(-9.81110406371068,12.3756328852638,2.3374969300026));
#94688=CARTESIAN_POINT('',(-10.6730394577908,13.3,4.4664951892051));
#94689=CARTESIAN_POINT('Ctrl Pts',(-9.81110401834328,13.5868901487969,2.33749693737438));
#94690=CARTESIAN_POINT('Ctrl Pts',(-9.75202396300196,13.5831615610686,2.34709689922293));
#94691=CARTESIAN_POINT('Ctrl Pts',(-9.69374318778665,13.5793739864102,2.36118950009534));
#94692=CARTESIAN_POINT('Ctrl Pts',(-9.6273910635311,13.5747909607468,2.38270201310816));
#94693=CARTESIAN_POINT('Ctrl Pts',(-9.61805390999522,13.574139754937,2.38585935099278));
#94694=CARTESIAN_POINT('Ctrl Pts',(-9.6028328166057,13.5730673097639,2.39122015273536));
#94695=CARTESIAN_POINT('Ctrl Pts',(-9.59692481154355,13.5726483364488,2.39335420700961));
#94696=CARTESIAN_POINT('Ctrl Pts',(-9.58634487173694,13.5718930353134,2.39727179106359));
#94697=CARTESIAN_POINT('Ctrl Pts',(-9.58166665712947,13.5715572843994,2.39903802025425));
#94698=CARTESIAN_POINT('Ctrl Pts',(-9.57172488705031,13.5708399155358,2.4028639843681));
#94699=CARTESIAN_POINT('Ctrl Pts',(-9.56646464369583,13.5704580324315,2.40493191897584));
#94700=CARTESIAN_POINT('Ctrl Pts',(-9.55229253621004,13.5694227689886,2.41062145000483));
#94701=CARTESIAN_POINT('Ctrl Pts',(-9.5434099862231,13.5687670234742,2.41431443405679));
#94702=CARTESIAN_POINT('Ctrl Pts',(-9.49659002895795,13.5652730934424,2.43445635749211));
#94703=CARTESIAN_POINT('Ctrl Pts',(-9.45949754686497,13.5623721214329,2.45278405541126));
#94704=CARTESIAN_POINT('Ctrl Pts',(-9.33134228688243,13.5518619026643,2.52473111418173));
#94705=CARTESIAN_POINT('Ctrl Pts',(-9.24662356770226,13.5439427472883,2.58858756243152));
#94706=CARTESIAN_POINT('Ctrl Pts',(-9.15592205131426,13.5348136678083,2.67834839759684));
#94707=CARTESIAN_POINT('Ctrl Pts',(-9.14072211083367,13.5332598207255,2.69425773317486));
#94708=CARTESIAN_POINT('Ctrl Pts',(-9.12226871724548,13.5313524995179,2.71468895094169));
#94709=CARTESIAN_POINT('Ctrl Pts',(-9.11859065541637,13.530971256108,2.71881934304621));
#94710=CARTESIAN_POINT('Ctrl Pts',(-9.11282308212285,13.5303719131736,2.72538881287748));
#94711=CARTESIAN_POINT('Ctrl Pts',(-9.11071427510706,13.5301524488659,2.72781072595031));
#94712=CARTESIAN_POINT('Ctrl Pts',(-9.10697432871951,13.5297626955485,2.73214160341194));
#94713=CARTESIAN_POINT('Ctrl Pts',(-9.10533938231773,13.5295921310226,2.73404716447577));
#94714=CARTESIAN_POINT('Ctrl Pts',(-9.10144108415476,13.529185003522,2.73862021641051));
#94715=CARTESIAN_POINT('Ctrl Pts',(-9.09918351282071,13.5289488631688,2.74129257461589));
#94716=CARTESIAN_POINT('Ctrl Pts',(-9.09235763756514,13.5282336215705,2.74944599491719));
#94717=CARTESIAN_POINT('Ctrl Pts',(-9.08782710005801,13.5277571608841,2.75495867259661));
#94718=CARTESIAN_POINT('Ctrl Pts',(-9.04434725895376,13.5231636827305,2.80885536108641));
#94719=CARTESIAN_POINT('Ctrl Pts',(-9.00922706805586,13.5192860417631,2.86021538210638));
#94720=CARTESIAN_POINT('Ctrl Pts',(-8.92987135235927,13.5094112713398,2.99859748077979));
#94721=CARTESIAN_POINT('Ctrl Pts',(-8.89209475876031,13.5034689921077,3.08875362681169));
#94722=CARTESIAN_POINT('Ctrl Pts',(-8.86205776357743,13.4961920378801,3.19605923742308));
#94723=CARTESIAN_POINT('Ctrl Pts',(-8.85851255205064,13.4952671613288,3.20965727312548));
#94724=CARTESIAN_POINT('Ctrl Pts',(-8.85369713570107,13.4939065842509,3.22958113313364));
#94725=CARTESIAN_POINT('Ctrl Pts',(-8.85223417215518,13.4934770652193,3.23585946565418));
#94726=CARTESIAN_POINT('Ctrl Pts',(-8.8497298533271,13.4927119753081,3.24702060252618));
#94727=CARTESIAN_POINT('Ctrl Pts',(-8.8486678561173,13.4923770737206,3.25189865173501));
#94728=CARTESIAN_POINT('Ctrl Pts',(-8.84651857882453,13.4916768023943,3.26208194592172));
#94729=CARTESIAN_POINT('Ctrl Pts',(-8.84543681485228,13.4913112652322,3.26738822203785));
#94730=CARTESIAN_POINT('Ctrl Pts',(-8.84271362612029,13.4903557495275,3.28123319761674));
#94731=CARTESIAN_POINT('Ctrl Pts',(-8.84113012233277,13.4897639466948,3.28978281584553));
#94732=CARTESIAN_POINT('Ctrl Pts',(-8.83443920364395,13.4870904902932,3.3282843064565));
#94733=CARTESIAN_POINT('Ctrl Pts',(-8.83039775859294,13.4849756468521,3.35840709179579));
#94734=CARTESIAN_POINT('Ctrl Pts',(-8.81836040085209,13.4759735540945,3.48515620388857));
#94735=CARTESIAN_POINT('Ctrl Pts',(-8.82114681937698,13.4687748718923,3.58241640124573));
#94736=CARTESIAN_POINT('Ctrl Pts',(-8.84207610111523,13.4586937655097,3.71913762794658));
#94737=CARTESIAN_POINT('Ctrl Pts',(-8.85049494617204,13.455714288772,3.75970747702375));
#94738=CARTESIAN_POINT('Ctrl Pts',(-8.86254728874883,13.4524227619116,3.80550242029854));
#94739=CARTESIAN_POINT('Ctrl Pts',(-8.86410377844083,13.4520117172482,3.81123974148636));
#94740=CARTESIAN_POINT('Ctrl Pts',(-8.8666666103228,13.4513570397813,3.82041112987392));
#94741=CARTESIAN_POINT('Ctrl Pts',(-8.86764525303397,13.4511119126466,3.82385273225124));
#94742=CARTESIAN_POINT('Ctrl Pts',(-8.86941557803412,13.4506770818707,3.82997230931403));
#94743=CARTESIAN_POINT('Ctrl Pts',(-8.87020111090193,13.4504870356863,3.83265196648745));
#94744=CARTESIAN_POINT('Ctrl Pts',(-8.87191539806998,13.4500784685929,3.8384237229732));
#94745=CARTESIAN_POINT('Ctrl Pts',(-8.87284733718414,13.449860133549,3.84151480307891));
#94746=CARTESIAN_POINT('Ctrl Pts',(-8.87547412178455,13.449254981772,3.85009950472141));
#94747=CARTESIAN_POINT('Ctrl Pts',(-8.87719652703085,13.448869712043,3.85558469935143));
#94748=CARTESIAN_POINT('Ctrl Pts',(-8.88752546273618,13.4466241379359,3.8876548524438));
#94749=CARTESIAN_POINT('Ctrl Pts',(-8.89703653688503,13.4448116294827,3.91394174865034));
#94750=CARTESIAN_POINT('Ctrl Pts',(-8.93467078143929,13.4383851192914,4.00741613913582));
#94751=CARTESIAN_POINT('Ctrl Pts',(-8.96807453249571,13.4339516560813,4.07230136291291));
#94752=CARTESIAN_POINT('Ctrl Pts',(-9.0428736911354,13.4253203500996,4.18948203404957));
#94753=CARTESIAN_POINT('Ctrl Pts',(-9.08312238771654,13.4211528557023,4.2421656847102));
#94754=CARTESIAN_POINT('Ctrl Pts',(-9.13424234251521,13.4161526702062,4.29853436830593));
#94755=CARTESIAN_POINT('Ctrl Pts',(-9.14099843210263,13.4154972282875,4.30579758960577));
#94756=CARTESIAN_POINT('Ctrl Pts',(-9.15220045267458,13.4144186063107,4.31753947740409));
#94757=CARTESIAN_POINT('Ctrl Pts',(-9.15659214938311,13.4139977259003,4.32206937935486));
#94758=CARTESIAN_POINT('Ctrl Pts',(-9.16453907753637,13.4132395327588,4.33013568334671));
#94759=CARTESIAN_POINT('Ctrl Pts',(-9.16808092334,13.4129028042966,4.33368510499508));
#94760=CARTESIAN_POINT('Ctrl Pts',(-9.17566798467224,13.4121839353929,4.34119190124458));
#94761=CARTESIAN_POINT('Ctrl Pts',(-9.17971926061898,13.4118015329181,4.34514294228123));
#94762=CARTESIAN_POINT('Ctrl Pts',(-9.19072684576405,13.4107663029892,4.35572447464828));
#94763=CARTESIAN_POINT('Ctrl Pts',(-9.19773596831187,13.410111128694,4.36229915264965));
#94764=CARTESIAN_POINT('Ctrl Pts',(-9.23507109561241,13.4066413103931,4.39647090009071));
#94765=CARTESIAN_POINT('Ctrl Pts',(-9.26673913051003,13.4037653010211,4.42255303752295));
#94766=CARTESIAN_POINT('Ctrl Pts',(-9.38313166017206,13.3934185291546,4.50863107826452));
#94767=CARTESIAN_POINT('Ctrl Pts',(-9.47434020441842,13.3856539260467,4.55902849766534));
#94768=CARTESIAN_POINT('Ctrl Pts',(-9.5925018559245,13.3765696820416,4.60524893815091));
#94769=CARTESIAN_POINT('Ctrl Pts',(-9.61428567920301,13.3749348647594,4.61303844857112));
#94770=CARTESIAN_POINT('Ctrl Pts',(-9.64166370856107,13.3729407448231,4.62192786222814));
#94771=CARTESIAN_POINT('Ctrl Pts',(-9.64705360877164,13.3725510445259,4.62363511600206));
#94772=CARTESIAN_POINT('Ctrl Pts',(-9.65557029735085,13.3719400260558,4.62626545195662));
#94773=CARTESIAN_POINT('Ctrl Pts',(-9.65868889565908,13.3717172866611,4.62721445122038));
#94774=CARTESIAN_POINT('Ctrl Pts',(-9.66449886008294,13.3713042319055,4.62895611909827));
#94775=CARTESIAN_POINT('Ctrl Pts',(-9.66718916598156,13.3711137292049,4.62975213331571));
#94776=CARTESIAN_POINT('Ctrl Pts',(-9.67340508601241,13.3706752797417,4.63156718435219));
#94777=CARTESIAN_POINT('Ctrl Pts',(-9.67693270485923,13.3704277156604,4.63257938099028));
#94778=CARTESIAN_POINT('Ctrl Pts',(-9.68439944628171,13.3699062593369,4.63468412449678));
#94779=CARTESIAN_POINT('Ctrl Pts',(-9.68833965256466,13.3696325813268,4.63577268891554));
#94780=CARTESIAN_POINT('Ctrl Pts',(-9.69890817809657,13.3689023151001,4.63863332567402));
#94781=CARTESIAN_POINT('Ctrl Pts',(-9.70554655628933,13.3684476060014,4.6403680590295));
#94782=CARTESIAN_POINT('Ctrl Pts',(-9.72623567590027,13.3670417596503,4.64558180482654));
#94783=CARTESIAN_POINT('Ctrl Pts',(-9.7403361380124,13.3660997458703,4.6488599978075));
#94784=CARTESIAN_POINT('Ctrl Pts',(-9.85441722306451,13.3585815513223,4.67317471803309));
#94785=CARTESIAN_POINT('Ctrl Pts',(-9.95669310330162,13.3524411064072,4.68138124185338));
#94786=CARTESIAN_POINT('Ctrl Pts',(-10.0986419529642,13.3434407515419,4.67429126807066));
#94787=CARTESIAN_POINT('Ctrl Pts',(-10.1384007360085,13.3408722499535,4.67027131412355));
#94788=CARTESIAN_POINT('Ctrl Pts',(-10.1876132325974,13.3375932649165,4.6627524971252));
#94789=CARTESIAN_POINT('Ctrl Pts',(-10.1973314329055,13.3369409198207,4.66114270902573));
#94790=CARTESIAN_POINT('Ctrl Pts',(-10.2127467781886,13.33589791752,4.65839009720257));
#94791=CARTESIAN_POINT('Ctrl Pts',(-10.2184577706468,13.3355097082673,4.65732666493088));
#94792=CARTESIAN_POINT('Ctrl Pts',(-10.2291318425239,13.3347806384625,4.65525724564447));
#94793=CARTESIAN_POINT('Ctrl Pts',(-10.2340967724754,13.3344401001199,4.65426141087529));
#94794=CARTESIAN_POINT('Ctrl Pts',(-10.2451888117559,13.3336760540079,4.65196212985747));
#94795=CARTESIAN_POINT('Ctrl Pts',(-10.2513122171472,13.3332520279136,4.65064176395554));
#94796=CARTESIAN_POINT('Ctrl Pts',(-10.2694048325153,13.3319923887743,4.6465892128724));
#94797=CARTESIAN_POINT('Ctrl Pts',(-10.2813418687755,13.3311524828205,4.6437187242201));
#94798=CARTESIAN_POINT('Ctrl Pts',(-10.3706449206016,13.3248000772339,4.62076147674413));
#94799=CARTESIAN_POINT('Ctrl Pts',(-10.445816601514,13.3190407780083,4.59303567102166));
#94800=CARTESIAN_POINT('Ctrl Pts',(-10.5716675881365,13.3087705362018,4.53146290535402));
#94801=CARTESIAN_POINT('Ctrl Pts',(-10.6236309027657,13.3043234952939,4.50090188616107));
#94802=CARTESIAN_POINT('Ctrl Pts',(-10.6730394577914,13.2999999999999,4.4664951892047));
#94803=CARTESIAN_POINT('',(-9.31533557546056,13.3,4.45829519891841));
#94804=CARTESIAN_POINT('Origin',(-10.,13.3,3.5));
#94805=CARTESIAN_POINT('Ctrl Pts',(-9.31533557546056,13.3,4.45829519891842));
#94806=CARTESIAN_POINT('Ctrl Pts',(-9.27955485067773,13.3029712552161,4.4327312710487));
#94807=CARTESIAN_POINT('Ctrl Pts',(-9.24520412249185,13.3058633132367,4.40510172653889));
#94808=CARTESIAN_POINT('Ctrl Pts',(-9.2125067118003,13.3087216394501,4.37560718174327));
#94809=CARTESIAN_POINT('Ctrl Pts',(-9.20890953043532,13.3090360960866,4.37236236129225));
#94810=CARTESIAN_POINT('Ctrl Pts',(-9.20533237168248,13.3093501444625,4.36909501894293));
#94811=CARTESIAN_POINT('Ctrl Pts',(-9.20177554086393,13.3096638451157,4.36580545935624));
#94812=CARTESIAN_POINT('Ctrl Pts',(-9.16642056516623,13.312782036431,4.33310716551634));
#94813=CARTESIAN_POINT('Ctrl Pts',(-9.13307223486999,13.3158666386743,4.29820842073811));
#94814=CARTESIAN_POINT('Ctrl Pts',(-9.10197737074274,13.3189690571681,4.26140275777538));
#94815=CARTESIAN_POINT('Ctrl Pts',(-9.07088946296696,13.322070781608,4.22460532874886));
#94816=CARTESIAN_POINT('Ctrl Pts',(-9.04205365923209,13.3251907834279,4.1859022640497));
#94817=CARTESIAN_POINT('Ctrl Pts',(-9.01567610080399,13.3283631623632,4.14560522160206));
#94818=CARTESIAN_POINT('Ctrl Pts',(-8.98929527243636,13.331535934568,4.10530318366201));
#94819=CARTESIAN_POINT('Ctrl Pts',(-8.96537303797927,13.3347613384183,4.06340697144733));
#94820=CARTESIAN_POINT('Ctrl Pts',(-8.94407975864983,13.3380509499895,4.02024207876584));
#94821=CARTESIAN_POINT('Ctrl Pts',(-8.92222134533198,13.3414278694515,3.9759315688413));
#94822=CARTESIAN_POINT('Ctrl Pts',(-8.90313329659415,13.3448726432002,3.93028412919885));
#94823=CARTESIAN_POINT('Ctrl Pts',(-8.88696388158558,13.3483705621843,3.88366497049273));
#94824=CARTESIAN_POINT('Ctrl Pts',(-8.87117968274283,13.351785147607,3.83815645515627));
#94825=CARTESIAN_POINT('Ctrl Pts',(-8.85817661103945,13.3552501723781,3.7917219170812));
#94826=CARTESIAN_POINT('Ctrl Pts',(-8.84805986849392,13.3587267852057,3.74471375304687));
#94827=CARTESIAN_POINT('Ctrl Pts',(-8.83757277461038,13.3623306690602,3.6959847251703));
#94828=CARTESIAN_POINT('Ctrl Pts',(-8.83018777323948,13.3659467765198,3.6466389664785));
#94829=CARTESIAN_POINT('Ctrl Pts',(-8.82598263306443,13.3695072207974,3.59708597188621));
#94830=CARTESIAN_POINT('Ctrl Pts',(-8.82228640539946,13.3726367746507,3.55352995665964));
#94831=CARTESIAN_POINT('Ctrl Pts',(-8.82104684420149,13.3757226976916,3.50981264481602));
#94832=CARTESIAN_POINT('Ctrl Pts',(-8.8222856938752,13.3787078477362,3.46622919277443));
#94833=CARTESIAN_POINT('Ctrl Pts',(-8.82245626402244,13.3791188560235,3.46022843579012));
#94834=CARTESIAN_POINT('Ctrl Pts',(-8.82267376941736,13.3795279539606,3.45423015119989));
#94835=CARTESIAN_POINT('Ctrl Pts',(-8.82293822277778,13.3799349924019,3.44823504541158));
#94836=CARTESIAN_POINT('Ctrl Pts',(-8.82293899910851,13.3799361873062,3.44821744614621));
#94837=CARTESIAN_POINT('Ctrl Pts',(-8.82293977584426,13.3799373821941,3.44819984688064));
#94838=CARTESIAN_POINT('Ctrl Pts',(-8.82294055298505,13.3799385770658,3.44818224761489));
#94839=CARTESIAN_POINT('Ctrl Pts',(-8.82478706990888,13.3827776388227,3.40636570327091));
#94840=CARTESIAN_POINT('Ctrl Pts',(-8.82892295448533,13.3855245455198,3.36454473495573));
#94841=CARTESIAN_POINT('Ctrl Pts',(-8.83532312249245,13.3882274772244,3.32299108896264));
#94842=CARTESIAN_POINT('Ctrl Pts',(-8.8363298521375,13.3886526412939,3.31645480940954));
#94843=CARTESIAN_POINT('Ctrl Pts',(-8.83739253724907,13.3890767173137,3.30992522352958));
#94844=CARTESIAN_POINT('Ctrl Pts',(-8.83851100094992,13.389499892797,3.30340347508238));
#94845=CARTESIAN_POINT('Ctrl Pts',(-8.8463451349046,13.3924639705939,3.25772273379857));
#94846=CARTESIAN_POINT('Ctrl Pts',(-8.85691924720082,13.3953845903242,3.21242140052275));
#94847=CARTESIAN_POINT('Ctrl Pts',(-8.87014669802613,13.3983178983678,3.16784756043915));
#94848=CARTESIAN_POINT('Ctrl Pts',(-8.88335905457101,13.4012478591169,3.12332458503472));
#94849=CARTESIAN_POINT('Ctrl Pts',(-8.89921819650777,13.4041909205412,3.07952744451848));
#94850=CARTESIAN_POINT('Ctrl Pts',(-8.91759907150029,13.4071860650398,3.03678282607116));
#94851=CARTESIAN_POINT('Ctrl Pts',(-8.93596749485212,13.4101791805563,2.99406716384223));
#94852=CARTESIAN_POINT('Ctrl Pts',(-8.95685393734695,13.4132245375064,2.95240257307865));
#94853=CARTESIAN_POINT('Ctrl Pts',(-8.98010084810828,13.4163391323926,2.91209515177081));
#94854=CARTESIAN_POINT('Ctrl Pts',(-9.00334278896435,13.4194530614165,2.87179634769677));
#94855=CARTESIAN_POINT('Ctrl Pts',(-9.02894404419675,13.4226362773876,2.83285413167521));
#94856=CARTESIAN_POINT('Ctrl Pts',(-9.05671770647299,13.4258815931662,2.79555469395453));
#94857=CARTESIAN_POINT('Ctrl Pts',(-9.08451798305426,13.4291300187913,2.75821951378825));
#94858=CARTESIAN_POINT('Ctrl Pts',(-9.11449484231353,13.4324406099238,2.72253030300228));
#94859=CARTESIAN_POINT('Ctrl Pts',(-9.14643234661305,13.4357817278187,2.68875403987866));
#94860=CARTESIAN_POINT('Ctrl Pts',(-9.17838774451515,13.4391247176393,2.65495885295238));
#94861=CARTESIAN_POINT('Ctrl Pts',(-9.21230617688561,13.4424980354468,2.62307888816323));
#94862=CARTESIAN_POINT('Ctrl Pts',(-9.24794135391478,13.4458476269234,2.59336032458294));
#94863=CARTESIAN_POINT('Ctrl Pts',(-9.28183228109596,13.4490332645514,2.56509640790858));
#94864=CARTESIAN_POINT('Ctrl Pts',(-9.31727655903721,13.452196989286,2.53878737947735));
#94865=CARTESIAN_POINT('Ctrl Pts',(-9.35403222356578,13.4552777283284,2.51462499684154));
#94866=CARTESIAN_POINT('Ctrl Pts',(-9.35599573057558,13.455442303035,2.51333422960097));
#94867=CARTESIAN_POINT('Ctrl Pts',(-9.35796298531366,13.4556066409209,2.51204957719333));
#94868=CARTESIAN_POINT('Ctrl Pts',(-9.35993395280853,13.4557707326757,2.51077106511618));
#94869=CARTESIAN_POINT('Ctrl Pts',(-9.37393448287944,13.4569363386806,2.50168930865456));
#94870=CARTESIAN_POINT('Ctrl Pts',(-9.38812169294092,13.458089405079,2.49291774113444));
#94871=CARTESIAN_POINT('Ctrl Pts',(-9.40248114251727,13.4592262978203,2.48446578966191));
#94872=CARTESIAN_POINT('Ctrl Pts',(-9.40249912531988,13.4592277215878,2.48445520501003));
#94873=CARTESIAN_POINT('Ctrl Pts',(-9.40251710842823,13.4592291453322,2.48444462083696));
#94874=CARTESIAN_POINT('Ctrl Pts',(-9.40253509184229,13.4592305690533,2.48443403714275));
#94875=CARTESIAN_POINT('Ctrl Pts',(-9.43872182154729,13.4620954206655,2.46313723108009));
#94876=CARTESIAN_POINT('Ctrl Pts',(-9.47615075797707,13.4648664476682,2.44377993774979));
#94877=CARTESIAN_POINT('Ctrl Pts',(-9.51457842010804,13.467589944673,2.42648542847173));
#94878=CARTESIAN_POINT('Ctrl Pts',(-9.51897800508859,13.4679017579827,2.42450537922995));
#94879=CARTESIAN_POINT('Ctrl Pts',(-9.52339062599426,13.4682129482707,2.42255235918054));
#94880=CARTESIAN_POINT('Ctrl Pts',(-9.52781587487007,13.4685235850126,2.42062654460647));
#94881=CARTESIAN_POINT('Ctrl Pts',(-9.57294223216398,13.4716912948965,2.40098810189049));
#94882=CARTESIAN_POINT('Ctrl Pts',(-9.61938825430672,13.4748024362306,2.38417988326783));
#94883=CARTESIAN_POINT('Ctrl Pts',(-9.66675063387697,13.4779224731179,2.37033497931386));
#94884=CARTESIAN_POINT('Ctrl Pts',(-9.71411295086191,13.4810425058823,2.35649009365473));
#94885=CARTESIAN_POINT('Ctrl Pts',(-9.76239127307546,13.484172041595,2.34560793136728));
#94886=CARTESIAN_POINT('Ctrl Pts',(-9.81117889814932,13.4873563446704,2.33776762587097));
#94887=CARTESIAN_POINT('Origin',(-10.,12.3756328852638,3.5));
#94888=CARTESIAN_POINT('',(-9.81110406370901,14.0854724903439,2.33749693000287));
#94889=CARTESIAN_POINT('',(-9.81110406371068,13.9872487449619,2.3374969300026));
#94890=CARTESIAN_POINT('',(-9.81110406371068,12.3756328852638,2.3374969300026));
#94891=CARTESIAN_POINT('Ctrl Pts',(-9.81110406370735,14.0854724903439,2.33749693000314));
#94892=CARTESIAN_POINT('Ctrl Pts',(-9.80837956425245,14.08528176319,2.33793963582365));
#94893=CARTESIAN_POINT('Ctrl Pts',(-9.80565658690304,14.0850915193238,2.33839192511108));
#94894=CARTESIAN_POINT('Ctrl Pts',(-9.7993878303637,14.0846544523039,2.33945583192401));
#94895=CARTESIAN_POINT('Ctrl Pts',(-9.79584319597262,14.0844079842951,2.3400741364642));
#94896=CARTESIAN_POINT('Ctrl Pts',(-9.7895438660327,14.0839712321639,2.34120272428794));
#94897=CARTESIAN_POINT('Ctrl Pts',(-9.78678809288852,14.0837805978782,2.34170660288027));
#94898=CARTESIAN_POINT('Ctrl Pts',(-9.78086154463636,14.083371565388,2.3428121090767));
#94899=CARTESIAN_POINT('Ctrl Pts',(-9.77769143347412,14.0831533484427,2.34341693795891));
#94900=CARTESIAN_POINT('Ctrl Pts',(-9.76887736037341,14.0825481236561,2.34513616246796));
#94901=CARTESIAN_POINT('Ctrl Pts',(-9.76323892260838,14.0821626686444,2.34627891006022));
#94902=CARTESIAN_POINT('Ctrl Pts',(-9.73010552204535,14.0799064780369,2.35324722404107));
#94903=CARTESIAN_POINT('Ctrl Pts',(-9.70281532783585,14.0780841629291,2.36001468202912));
#94904=CARTESIAN_POINT('Ctrl Pts',(-9.60459418311645,14.0715707251508,2.38813943943628));
#94905=CARTESIAN_POINT('Ctrl Pts',(-9.53547432530339,14.0670656701688,2.4151971921999));
#94906=CARTESIAN_POINT('Ctrl Pts',(-9.41233600380801,14.0584938892006,2.47734431687218));
#94907=CARTESIAN_POINT('Ctrl Pts',(-9.3577646487029,14.054467079317,2.51070443143162));
#94908=CARTESIAN_POINT('Ctrl Pts',(-9.29821176979242,14.049625114584,2.55412191948246));
#94909=CARTESIAN_POINT('Ctrl Pts',(-9.29032667258213,14.048974447299,2.56002349923409));
#94910=CARTESIAN_POINT('Ctrl Pts',(-9.2775435736164,14.0479032512061,2.56984350681934));
#94911=CARTESIAN_POINT('Ctrl Pts',(-9.2726011146419,14.0474849950673,2.57370347682784));
#94912=CARTESIAN_POINT('Ctrl Pts',(-9.26378310363801,14.0467312509447,2.58070427705748));
#94913=CARTESIAN_POINT('Ctrl Pts',(-9.25989620626059,14.0463963411528,2.58383062816507));
#94914=CARTESIAN_POINT('Ctrl Pts',(-9.25166194902176,14.0456810702316,2.59054029073654));
#94915=CARTESIAN_POINT('Ctrl Pts',(-9.24732021881102,14.0453004464793,2.59413028177683));
#94916=CARTESIAN_POINT('Ctrl Pts',(-9.23566804944887,14.0442693866189,2.60390656560067));
#94917=CARTESIAN_POINT('Ctrl Pts',(-9.22840716625819,14.043616603529,2.61015098848929));
#94918=CARTESIAN_POINT('Ctrl Pts',(-9.19050910362557,14.040153721968,2.64355626196296));
#94919=CARTESIAN_POINT('Ctrl Pts',(-9.16123099808947,14.0372819798163,2.67220941551946));
#94920=CARTESIAN_POINT('Ctrl Pts',(-9.06398839877253,14.0270179475793,2.77784157855102));
#94921=CARTESIAN_POINT('Ctrl Pts',(-9.00464969901487,14.0193354171032,2.8621093127799));
#94922=CARTESIAN_POINT('Ctrl Pts',(-8.94544145929536,14.0101828713199,2.97500555064854));
#94923=CARTESIAN_POINT('Ctrl Pts',(-8.93459575007949,14.0084217750301,2.99737998072639));
#94924=CARTESIAN_POINT('Ctrl Pts',(-8.92212472719435,14.0063000115036,3.02532858008758));
#94925=CARTESIAN_POINT('Ctrl Pts',(-8.91982231292956,14.0059038018646,3.03059161880807));
#94926=CARTESIAN_POINT('Ctrl Pts',(-8.91627391270032,14.0052862605735,3.03886720469023));
#94927=CARTESIAN_POINT('Ctrl Pts',(-8.91500180701086,14.0050634264173,3.04186834963261));
#94928=CARTESIAN_POINT('Ctrl Pts',(-8.91266153927544,14.0046508234429,3.04745392056078));
#94929=CARTESIAN_POINT('Ctrl Pts',(-8.9115901276884,14.0044608695345,3.05003685450816));
#94930=CARTESIAN_POINT('Ctrl Pts',(-8.90915693218752,14.0040270119564,3.05596228783824));
#94931=CARTESIAN_POINT('Ctrl Pts',(-8.90780130535554,14.0037834764147,3.05930724908921));
#94932=CARTESIAN_POINT('Ctrl Pts',(-8.90363242306076,14.0030286707225,3.06973121886648));
#94933=CARTESIAN_POINT('Ctrl Pts',(-8.90087238465933,14.0025204370554,3.07683149867637));
#94934=CARTESIAN_POINT('Ctrl Pts',(-8.89456594422872,14.0013376021882,3.09353307812985));
#94935=CARTESIAN_POINT('Ctrl Pts',(-8.89107537013762,14.0006658735758,3.10315495299672));
#94936=CARTESIAN_POINT('Ctrl Pts',(-8.87911718848562,13.9982977857457,3.13750850885843));
#94937=CARTESIAN_POINT('Ctrl Pts',(-8.87134750287598,13.9966318132238,3.16247653999496));
#94938=CARTESIAN_POINT('Ctrl Pts',(-8.8426226113462,13.9898110202216,3.26692066333203));
#94939=CARTESIAN_POINT('Ctrl Pts',(-8.82918295799498,13.9848359978717,3.3482213230498));
#94940=CARTESIAN_POINT('Ctrl Pts',(-8.8216152638385,13.976799362719,3.47580071364178));
#94941=CARTESIAN_POINT('Ctrl Pts',(-8.82156239420987,13.9738818217062,3.52145363692289));
#94942=CARTESIAN_POINT('Ctrl Pts',(-8.82473330240428,13.9702143704019,3.57711019003066));
#94943=CARTESIAN_POINT('Ctrl Pts',(-8.82544040421432,13.9695437352526,3.58722119742213));
#94944=CARTESIAN_POINT('Ctrl Pts',(-8.82675838488983,13.9684819970452,3.60311636968189));
#94945=CARTESIAN_POINT('Ctrl Pts',(-8.8272817732766,13.9680936149897,3.60890744592317));
#94946=CARTESIAN_POINT('Ctrl Pts',(-8.82832745145944,13.9673739226933,3.61959405825179));
#94947=CARTESIAN_POINT('Ctrl Pts',(-8.82883759863378,13.9670429982251,3.62449067488374));
#94948=CARTESIAN_POINT('Ctrl Pts',(-8.83003797939917,13.966306365672,3.63535131346133));
#94949=CARTESIAN_POINT('Ctrl Pts',(-8.83074314345513,13.9659001997227,3.64131351248222));
#94950=CARTESIAN_POINT('Ctrl Pts',(-8.83290815535112,13.9647247017439,3.65849169076727));
#94951=CARTESIAN_POINT('Ctrl Pts',(-8.83448399259513,13.9639517741263,3.66969210595782));
#94952=CARTESIAN_POINT('Ctrl Pts',(-8.83840359154376,13.9621961434827,3.6949124526799));
#94953=CARTESIAN_POINT('Ctrl Pts',(-8.84084031144782,13.9612106656738,3.70891593162067));
#94954=CARTESIAN_POINT('Ctrl Pts',(-8.84963073527725,13.9579649509341,3.75452907296625));
#94955=CARTESIAN_POINT('Ctrl Pts',(-8.85702853339019,13.9556742860442,3.78592027868278));
#94956=CARTESIAN_POINT('Ctrl Pts',(-8.87970554916105,13.9496086225872,3.86707228580801));
#94957=CARTESIAN_POINT('Ctrl Pts',(-8.89701095039513,13.9457899365153,3.91619251828558));
#94958=CARTESIAN_POINT('Ctrl Pts',(-8.94130221639083,13.937535480823,4.01952141313446));
#94959=CARTESIAN_POINT('Ctrl Pts',(-8.96933737147941,13.9331105791918,4.07313134795413));
#94960=CARTESIAN_POINT('Ctrl Pts',(-9.00654694123221,13.9281918136267,4.13264653299781));
#94961=CARTESIAN_POINT('Ctrl Pts',(-9.01183221356889,13.927512092796,4.14087054632215));
#94962=CARTESIAN_POINT('Ctrl Pts',(-9.01926021911617,13.926583422091,4.15211828557405));
#94963=CARTESIAN_POINT('Ctrl Pts',(-9.02131555656593,13.9263291760415,4.15519885325083));
#94964=CARTESIAN_POINT('Ctrl Pts',(-9.02486407265412,13.9258949198086,4.16046346195009));
#94965=CARTESIAN_POINT('Ctrl Pts',(-9.02635012675529,13.9257144494322,4.1626522361365));
#94966=CARTESIAN_POINT('Ctrl Pts',(-9.02946778142215,13.9253387479846,4.16721102657631));
#94967=CARTESIAN_POINT('Ctrl Pts',(-9.03110070762115,13.9251436149046,4.16958009434967));
#94968=CARTESIAN_POINT('Ctrl Pts',(-9.03510643221353,13.9246688727887,4.17534630798837));
#94969=CARTESIAN_POINT('Ctrl Pts',(-9.03748853902933,13.9243898837448,4.17873700478768));
#94970=CARTESIAN_POINT('Ctrl Pts',(-9.04611528456408,13.9233911285465,4.19087958454551));
#94971=CARTESIAN_POINT('Ctrl Pts',(-9.05246202486794,13.9226778949883,4.19955875850679));
#94972=CARTESIAN_POINT('Ctrl Pts',(-9.06860179853754,13.9209135832482,4.22100718239029));
#94973=CARTESIAN_POINT('Ctrl Pts',(-9.07853956948397,13.9198707761825,4.23366524765841));
#94974=CARTESIAN_POINT('Ctrl Pts',(-9.12316729819788,13.9153538720209,4.28817112729778));
#94975=CARTESIAN_POINT('Ctrl Pts',(-9.16047322840555,13.9119976525774,4.32779529529698));
#94976=CARTESIAN_POINT('Ctrl Pts',(-9.26033177781935,13.9035901425369,4.42013719575697));
#94977=CARTESIAN_POINT('Ctrl Pts',(-9.32587192127041,13.8985432781847,4.46918045473273));
#94978=CARTESIAN_POINT('Ctrl Pts',(-9.40885645597812,13.892238466229,4.51875920346066));
#94979=CARTESIAN_POINT('Ctrl Pts',(-9.42190615942508,13.8912499787935,4.52622048425328));
#94980=CARTESIAN_POINT('Ctrl Pts',(-9.44092897139612,13.8898114390106,4.53661895529123));
#94981=CARTESIAN_POINT('Ctrl Pts',(-9.44679012810352,13.8893685338116,4.53975867780928));
#94982=CARTESIAN_POINT('Ctrl Pts',(-9.45715150761605,13.8885859764846,4.54519668373168));
#94983=CARTESIAN_POINT('Ctrl Pts',(-9.46164056230823,13.8882470695151,4.54751597021385));
#94984=CARTESIAN_POINT('Ctrl Pts',(-9.47094694665004,13.8875446782512,4.55224852523675));
#94985=CARTESIAN_POINT('Ctrl Pts',(-9.47576618230397,13.8871810636836,4.55465776194756));
#94986=CARTESIAN_POINT('Ctrl Pts',(-9.48818861456843,13.8862439775683,4.56076181461754));
#94987=CARTESIAN_POINT('Ctrl Pts',(-9.49581525737343,13.8856688461363,4.56440793891283));
#94988=CARTESIAN_POINT('Ctrl Pts',(-9.52851084610568,13.8832035360072,4.57960872120166));
#94989=CARTESIAN_POINT('Ctrl Pts',(-9.55394076555903,13.8812865073426,4.59036138589155));
#94990=CARTESIAN_POINT('Ctrl Pts',(-9.67268587944295,13.8723299124985,4.63572164850167));
#94991=CARTESIAN_POINT('Ctrl Pts',(-9.76976591482076,13.864946989495,4.65930346886787));
#94992=CARTESIAN_POINT('Ctrl Pts',(-9.89060094924893,13.8560847530131,4.67286645625058));
#94993=CARTESIAN_POINT('Ctrl Pts',(-9.91263830147108,13.8544837874729,4.67471354138045));
#94994=CARTESIAN_POINT('Ctrl Pts',(-9.95646627226951,13.8513443683494,4.67714673175867));
#94995=CARTESIAN_POINT('Ctrl Pts',(-9.97824804066715,13.8498059105185,4.67775065866112));
#94996=CARTESIAN_POINT('Ctrl Pts',(-10.0055474180099,13.8479147422302,4.67774983269789));
#94997=CARTESIAN_POINT('Ctrl Pts',(-10.0110592698183,13.8475348008846,4.67771097379941));
#94998=CARTESIAN_POINT('Ctrl Pts',(-10.0197770360231,13.8469370744195,4.67758830389097));
#94999=CARTESIAN_POINT('Ctrl Pts',(-10.0229831434751,13.8467179359008,4.67753009318425));
#95000=CARTESIAN_POINT('Ctrl Pts',(-10.0287134496716,13.8463275403495,4.67740263979577));
#95001=CARTESIAN_POINT('Ctrl Pts',(-10.0312376496056,13.8461560171673,4.67733837438944));
#95002=CARTESIAN_POINT('Ctrl Pts',(-10.0372984416242,13.8457452268282,4.67716456266365));
#95003=CARTESIAN_POINT('Ctrl Pts',(-10.0408347677477,13.8455063941555,4.67704719697413));
#95004=CARTESIAN_POINT('Ctrl Pts',(-10.0516093611394,13.8447811659782,4.67664098642276));
#95005=CARTESIAN_POINT('Ctrl Pts',(-10.0588457060926,13.8442974712538,4.67630129068867));
#95006=CARTESIAN_POINT('Ctrl Pts',(-10.1245044307226,13.8399356067439,4.67261163949672));
#95007=CARTESIAN_POINT('Ctrl Pts',(-10.18261298426,13.8362668928653,4.66497804775069));
#95008=CARTESIAN_POINT('Ctrl Pts',(-10.3385299155154,13.826384221879,4.63253584678592));
#95009=CARTESIAN_POINT('Ctrl Pts',(-10.4340888607832,13.8202473931297,4.59945656712744));
#95010=CARTESIAN_POINT('Ctrl Pts',(-10.5364514753908,13.8127735873552,4.54857039888152));
#95011=CARTESIAN_POINT('Ctrl Pts',(-10.5485249244142,13.8118775907887,4.54230535313244));
#95012=CARTESIAN_POINT('Ctrl Pts',(-10.566169355979,13.8105452575769,4.53275799160945));
#95013=CARTESIAN_POINT('Ctrl Pts',(-10.5718264447905,13.8101145565875,4.5296365004787));
#95014=CARTESIAN_POINT('Ctrl Pts',(-10.5818245613224,13.8093469057134,4.52401188938961));
#95015=CARTESIAN_POINT('Ctrl Pts',(-10.5861758713091,13.8090106203361,4.52152729593227));
#95016=CARTESIAN_POINT('Ctrl Pts',(-10.5952936625973,13.8083012628786,4.51624360818539));
#95017=CARTESIAN_POINT('Ctrl Pts',(-10.6000565461852,13.8079279838481,4.513438580025));
#95018=CARTESIAN_POINT('Ctrl Pts',(-10.6125956175627,13.8069379148144,4.50593450120273));
#95019=CARTESIAN_POINT('Ctrl Pts',(-10.6203373498948,13.8063190909114,4.5011788929235));
#95020=CARTESIAN_POINT('Ctrl Pts',(-10.6570429591657,13.8033481314669,4.47804210995675));
#95021=CARTESIAN_POINT('Ctrl Pts',(-10.6852469258132,13.8009534835102,4.45849259394078));
#95022=CARTESIAN_POINT('Ctrl Pts',(-10.7646943656913,13.7938685266969,4.39812342878894));
#95023=CARTESIAN_POINT('Ctrl Pts',(-10.8134329889313,13.7890758541339,4.35422956894727));
#95024=CARTESIAN_POINT('Ctrl Pts',(-10.9014867757059,13.7796337438237,4.26052614088151));
#95025=CARTESIAN_POINT('Ctrl Pts',(-10.940944382723,13.7750021153455,4.211128461665));
#95026=CARTESIAN_POINT('Ctrl Pts',(-10.9817324936223,13.7698920932885,4.15068597421095));
#95027=CARTESIAN_POINT('Ctrl Pts',(-10.9871081230018,13.7692112610803,4.14250174726328));
#95028=CARTESIAN_POINT('Ctrl Pts',(-10.9943767810737,13.7682813400099,4.13112883815841));
#95029=CARTESIAN_POINT('Ctrl Pts',(-10.9963575737781,13.7680269375681,4.12799711719326));
#95030=CARTESIAN_POINT('Ctrl Pts',(-10.999727730152,13.7675924551595,4.12261266646345));
#95031=CARTESIAN_POINT('Ctrl Pts',(-11.0011243259431,13.767411914338,4.1203645309294));
#95032=CARTESIAN_POINT('Ctrl Pts',(-11.0040219849772,13.7670363292457,4.11566482703329));
#95033=CARTESIAN_POINT('Ctrl Pts',(-11.0055216641355,13.7668413820931,4.11321244991888));
#95034=CARTESIAN_POINT('Ctrl Pts',(-11.0091581734917,13.7663672209954,4.10721657208559));
#95035=CARTESIAN_POINT('Ctrl Pts',(-11.0112853641807,13.7660886252733,4.1036672080122));
#95036=CARTESIAN_POINT('Ctrl Pts',(-11.0188603161551,13.7650917955673,4.09087546535479));
#95037=CARTESIAN_POINT('Ctrl Pts',(-11.0242006403187,13.7643800722587,4.08156962429296));
#95038=CARTESIAN_POINT('Ctrl Pts',(-11.0372101068087,13.7626200112229,4.05816467537152));
#95039=CARTESIAN_POINT('Ctrl Pts',(-11.0447198199632,13.7615799072526,4.04397900864297));
#95040=CARTESIAN_POINT('Ctrl Pts',(-11.0762713540244,13.7570811504198,3.98131376014176));
#95041=CARTESIAN_POINT('Ctrl Pts',(-11.0972474827516,13.7537395921702,3.93136047198861));
#95042=CARTESIAN_POINT('Ctrl Pts',(-11.1411906507918,13.7453247149666,3.80250179563829));
#95043=CARTESIAN_POINT('Ctrl Pts',(-11.1594801565671,13.7402564862725,3.72232200786644));
#95044=CARTESIAN_POINT('Ctrl Pts',(-11.1710883507654,13.7339280573422,3.62598685320325));
#95045=CARTESIAN_POINT('Ctrl Pts',(-11.1725995971807,13.7329404554373,3.61104397218368));
#95046=CARTESIAN_POINT('Ctrl Pts',(-11.1743665611913,13.7315032277465,3.58945597590824));
#95047=CARTESIAN_POINT('Ctrl Pts',(-11.1748524371892,13.7310607441739,3.58283078809333));
#95048=CARTESIAN_POINT('Ctrl Pts',(-11.1756088354499,13.7302789488712,3.5711646646585));
#95049=CARTESIAN_POINT('Ctrl Pts',(-11.1759030463892,13.7299403817666,3.56612539313044));
#95050=CARTESIAN_POINT('Ctrl Pts',(-11.1764440058136,13.7292387159503,3.5557093636069));
#95051=CARTESIAN_POINT('Ctrl Pts',(-11.1766863088642,13.728875487204,3.55033250315407));
#95052=CARTESIAN_POINT('Ctrl Pts',(-11.1772140401526,13.7279394503562,3.53651662063033));
#95053=CARTESIAN_POINT('Ctrl Pts',(-11.1774455797892,13.7273649845954,3.5280759697063));
#95054=CARTESIAN_POINT('Ctrl Pts',(-11.1780457970171,13.7249032785167,3.49207634041549));
#95055=CARTESIAN_POINT('Ctrl Pts',(-11.1775377579458,13.7229892434101,3.46451348214993));
#95056=CARTESIAN_POINT('Ctrl Pts',(-11.1707442772212,13.7140415613419,3.33770365225719));
#95057=CARTESIAN_POINT('Ctrl Pts',(-11.1528717543418,13.7066645796645,3.2394946298067));
#95058=CARTESIAN_POINT('Ctrl Pts',(-11.1162251753926,13.6978088470079,3.12367050014724));
#95059=CARTESIAN_POINT('Ctrl Pts',(-11.1089739631477,13.6962097257088,3.1028106533509));
#95060=CARTESIAN_POINT('Ctrl Pts',(-11.0933515939303,13.6930594365367,3.06164018187035));
#95061=CARTESIAN_POINT('Ctrl Pts',(-11.084989894004,13.6915086255878,3.04133441429724));
#95062=CARTESIAN_POINT('Ctrl Pts',(-11.0738200224146,13.6896048092734,3.01622720345842));
#95063=CARTESIAN_POINT('Ctrl Pts',(-11.0715397902647,13.689224111752,3.01119734032934));
#95064=CARTESIAN_POINT('Ctrl Pts',(-11.0678795653503,13.6886256001244,3.00327212577477));
#95065=CARTESIAN_POINT('Ctrl Pts',(-11.0665230168985,13.6884064238553,3.00036613187721));
#95066=CARTESIAN_POINT('Ctrl Pts',(-11.0640785260399,13.6880161980655,2.99518487256374));
#95067=CARTESIAN_POINT('Ctrl Pts',(-11.0629951518513,13.6878448808323,2.99290757274255));
#95068=CARTESIAN_POINT('Ctrl Pts',(-11.0603782759185,13.6874349223575,2.98745202497275));
#95069=CARTESIAN_POINT('Ctrl Pts',(-11.0588377962123,13.6871967124288,2.98427717049367));
#95070=CARTESIAN_POINT('Ctrl Pts',(-11.0541083891418,13.6864746479896,2.97464061063705));
#95071=CARTESIAN_POINT('Ctrl Pts',(-11.0508743377206,13.6859934644342,2.96820105604369));
#95072=CARTESIAN_POINT('Ctrl Pts',(-11.0179835920254,13.681219034786,2.90418177205053));
#95073=CARTESIAN_POINT('Ctrl Pts',(-10.9836794412224,13.6771835961947,2.84910276219508));
#95074=CARTESIAN_POINT('Ctrl Pts',(-10.889158746204,13.6673777876629,2.72202108219114));
#95075=CARTESIAN_POINT('Ctrl Pts',(-10.8245585009238,13.661645284195,2.65385844811415));
#95076=CARTESIAN_POINT('Ctrl Pts',(-10.7414997696614,13.6545950961847,2.58486039712428));
#95077=CARTESIAN_POINT('Ctrl Pts',(-10.7302563065948,13.6536474519342,2.5758635932318));
#95078=CARTESIAN_POINT('Ctrl Pts',(-10.7136718498343,13.652257663125,2.56308468655812));
#95079=CARTESIAN_POINT('Ctrl Pts',(-10.7084595318908,13.6518219917088,2.55913714996341));
#95080=CARTESIAN_POINT('Ctrl Pts',(-10.699174229687,13.6510477069659,2.55222585544457));
#95081=CARTESIAN_POINT('Ctrl Pts',(-10.6951145612694,13.6507097873466,2.54924441736699));
#95082=CARTESIAN_POINT('Ctrl Pts',(-10.6866325091008,13.6500049453644,2.54309852633936));
#95083=CARTESIAN_POINT('Ctrl Pts',(-10.682207092241,13.6496378651427,2.53993848403971));
#95084=CARTESIAN_POINT('Ctrl Pts',(-10.6706648083156,13.6486820691636,2.53181662605135));
#95085=CARTESIAN_POINT('Ctrl Pts',(-10.6635148240792,13.6480915663578,2.52690267602969));
#95086=CARTESIAN_POINT('Ctrl Pts',(-10.6315966582526,13.64546188905,2.50548169684432));
#95087=CARTESIAN_POINT('Ctrl Pts',(-10.6062641768747,13.6433912232271,2.48983938567262));
#95088=CARTESIAN_POINT('Ctrl Pts',(-10.4949928936122,13.6343578126546,2.42682541581478));
#95089=CARTESIAN_POINT('Ctrl Pts',(-10.4039172242116,13.6270741246665,2.38933931355589));
#95090=CARTESIAN_POINT('Ctrl Pts',(-10.2698749665405,13.6169581516545,2.35286024369748));
#95091=CARTESIAN_POINT('Ctrl Pts',(-10.2299426472491,13.6140225585947,2.34419324574026));
#95092=CARTESIAN_POINT('Ctrl Pts',(-10.1837658743357,13.6107714209558,2.33665974472558));
#95093=CARTESIAN_POINT('Ctrl Pts',(-10.1778877522899,13.6103602146303,2.33574642050255));
#95094=CARTESIAN_POINT('Ctrl Pts',(-10.1684488893274,13.6097044274908,2.3343529951947));
#95095=CARTESIAN_POINT('Ctrl Pts',(-10.1648925250124,13.6094583656049,2.33384459689718));
#95096=CARTESIAN_POINT('Ctrl Pts',(-10.1585530178436,13.6090216308315,2.33296791653498));
#95097=CARTESIAN_POINT('Ctrl Pts',(-10.1557708316414,13.6088306147442,2.33259330484696));
#95098=CARTESIAN_POINT('Ctrl Pts',(-10.1497653465816,13.6084197101163,2.3318065390477));
#95099=CARTESIAN_POINT('Ctrl Pts',(-10.1465416728934,13.6082000101842,2.33139777511911));
#95100=CARTESIAN_POINT('Ctrl Pts',(-10.1375434478926,13.6075890815874,2.33029461437776));
#95101=CARTESIAN_POINT('Ctrl Pts',(-10.1317652856069,13.6071994382068,2.32962963034546));
#95102=CARTESIAN_POINT('Ctrl Pts',(-10.0971794904755,13.6048818116319,2.32590868639687));
#95103=CARTESIAN_POINT('Ctrl Pts',(-10.0682693609797,13.6030050573454,2.32387335716873));
#95104=CARTESIAN_POINT('Ctrl Pts',(-9.97995507240773,13.597376613144,2.32092395638361));
#95105=CARTESIAN_POINT('Ctrl Pts',(-9.92053037097864,13.5937299755792,2.32343396867559));
#95106=CARTESIAN_POINT('Ctrl Pts',(-9.84467507092052,13.5890005060176,2.33241367566494));
#95107=CARTESIAN_POINT('Ctrl Pts',(-9.82785742148521,13.5879474689535,2.33477466451822));
#95108=CARTESIAN_POINT('Ctrl Pts',(-9.81110401834328,13.5868901487969,2.33749693737438));
#95109=CARTESIAN_POINT('Ctrl Pts',(-9.81114449848021,13.4871956596082,2.33749036045042));
#95110=CARTESIAN_POINT('Ctrl Pts',(-9.83460130906247,13.4887031289619,2.33367968432709));
#95111=CARTESIAN_POINT('Ctrl Pts',(-9.85816692158536,13.4902261927543,2.33058002303858));
#95112=CARTESIAN_POINT('Ctrl Pts',(-9.89603391445815,13.4926982099412,2.32676067340649));
#95113=CARTESIAN_POINT('Ctrl Pts',(-9.91028309603021,13.4936339341941,2.32558511857208));
#95114=CARTESIAN_POINT('Ctrl Pts',(-9.93111828325639,13.4950118606764,2.3242476042958));
#95115=CARTESIAN_POINT('Ctrl Pts',(-9.93769019833253,13.4954478953722,2.32388101254519));
#95116=CARTESIAN_POINT('Ctrl Pts',(-9.94927241800302,13.4962189895655,2.3233322864495));
#95117=CARTESIAN_POINT('Ctrl Pts',(-9.95428150030809,13.4965533397589,2.32312701909735));
#95118=CARTESIAN_POINT('Ctrl Pts',(-9.96412617670132,13.4972122344832,2.3227865394719));
#95119=CARTESIAN_POINT('Ctrl Pts',(-9.96896159899539,13.4975367052893,2.32264912649977));
#95120=CARTESIAN_POINT('Ctrl Pts',(-9.97858607342345,13.4981842655482,2.32243495024421));
#95121=CARTESIAN_POINT('Ctrl Pts',(-9.98337502064357,13.4985073308852,2.32235760454786));
#95122=CARTESIAN_POINT('Ctrl Pts',(-9.99474056699205,13.4992761383291,2.32224338116128));
#95123=CARTESIAN_POINT('Ctrl Pts',(-10.0013172085728,13.4997226601407,2.3222323757135));
#95124=CARTESIAN_POINT('Ctrl Pts',(-10.0247357045077,13.5013187391237,2.32238933406711));
#95125=CARTESIAN_POINT('Ctrl Pts',(-10.041572779569,13.5024774958713,2.32286347872021));
#95126=CARTESIAN_POINT('Ctrl Pts',(-10.092976770881,13.5060511559269,2.32541524174278));
#95127=CARTESIAN_POINT('Ctrl Pts',(-10.1274647444889,13.5084991700587,2.32865616239873));
#95128=CARTESIAN_POINT('Ctrl Pts',(-10.2393197897243,13.5165956866793,2.34416579313634));
#95129=CARTESIAN_POINT('Ctrl Pts',(-10.3156143211647,13.5223803952931,2.36262900902497));
#95130=CARTESIAN_POINT('Ctrl Pts',(-10.4252140636606,13.5307941663748,2.40103689549037));
#95131=CARTESIAN_POINT('Ctrl Pts',(-10.4603045962512,13.5335013880817,2.41526630642648));
#95132=CARTESIAN_POINT('Ctrl Pts',(-10.5003710338081,13.5365637379917,2.43380883537797));
#95133=CARTESIAN_POINT('Ctrl Pts',(-10.5060685962099,13.5369984973955,2.43650136286607));
#95134=CARTESIAN_POINT('Ctrl Pts',(-10.5148093475971,13.5376640638446,2.44071817810893));
#95135=CARTESIAN_POINT('Ctrl Pts',(-10.5178678960987,13.5378966901573,2.44221009388881));
#95136=CARTESIAN_POINT('Ctrl Pts',(-10.5232202327771,13.5383032518542,2.44484966544022));
#95137=CARTESIAN_POINT('Ctrl Pts',(-10.5255167969995,13.5384775259928,2.44599158585664));
#95138=CARTESIAN_POINT('Ctrl Pts',(-10.5308953002472,13.5388852496528,2.44868788814847));
#95139=CARTESIAN_POINT('Ctrl Pts',(-10.533974159385,13.5391183276126,2.45024832735685));
#95140=CARTESIAN_POINT('Ctrl Pts',(-10.5428420864596,13.5397888599252,2.45479191402767));
#95141=CARTESIAN_POINT('Ctrl Pts',(-10.5486134412727,13.540224269579,2.45780962842987));
#95142=CARTESIAN_POINT('Ctrl Pts',(-10.5892555417729,13.5432855761932,2.47949166168329));
#95143=CARTESIAN_POINT('Ctrl Pts',(-10.6231956728638,13.5458168913886,2.49985639433537));
#95144=CARTESIAN_POINT('Ctrl Pts',(-10.7174158135842,13.5529562043275,2.56305307883562));
#95145=CARTESIAN_POINT('Ctrl Pts',(-10.774772921729,13.557452415181,2.60989744004744));
#95146=CARTESIAN_POINT('Ctrl Pts',(-10.8517997600858,13.5642348239417,2.6859292740451));
#95147=CARTESIAN_POINT('Ctrl Pts',(-10.8751677178338,13.5664102919784,2.71110509690412));
#95148=CARTESIAN_POINT('Ctrl Pts',(-10.9070131083949,13.5695854504994,2.748572987383));
#95149=CARTESIAN_POINT('Ctrl Pts',(-10.9164098423391,13.5705511176891,2.76006195871282));
#95150=CARTESIAN_POINT('Ctrl Pts',(-10.9327691432312,13.5722873004723,2.78085348886599));
#95151=CARTESIAN_POINT('Ctrl Pts',(-10.9398159786282,13.5730545146995,2.7900874069955));
#95152=CARTESIAN_POINT('Ctrl Pts',(-10.9503243732758,13.5742294399357,2.80428794430047));
#95153=CARTESIAN_POINT('Ctrl Pts',(-10.9538862569624,13.5746332992808,2.80917970110329));
#95154=CARTESIAN_POINT('Ctrl Pts',(-10.9574404349605,13.5750420709097,2.81414077341459));
#95155=CARTESIAN_POINT('Ctrl Pts',(-10.957470636241,13.5750455448327,2.81418293552434));
#95156=CARTESIAN_POINT('Ctrl Pts',(-10.9575330265506,13.5750527222008,2.8142700468687));
#95157=CARTESIAN_POINT('Ctrl Pts',(-10.9575652151999,13.5750564256604,2.81431499637541));
#95158=CARTESIAN_POINT('Ctrl Pts',(-10.9576317166497,13.5750640779739,2.81440787545273));
#95159=CARTESIAN_POINT('Ctrl Pts',(-10.9576660290411,13.5750680268471,2.81445580536678));
#95160=CARTESIAN_POINT('Ctrl Pts',(-10.9577369244382,13.5750761870469,2.81455485265486));
#95161=CARTESIAN_POINT('Ctrl Pts',(-10.9577735069255,13.5750803983895,2.81460597034783));
#95162=CARTESIAN_POINT('Ctrl Pts',(-10.9578490995345,13.5750891018361,2.81471161580256));
#95163=CARTESIAN_POINT('Ctrl Pts',(-10.9578881091097,13.5750935939635,2.81476614399078));
#95164=CARTESIAN_POINT('Ctrl Pts',(-10.9579687244699,13.5751028786568,2.81487884972569));
#95165=CARTESIAN_POINT('Ctrl Pts',(-10.9580103296226,13.5751076712482,2.81493702774705));
#95166=CARTESIAN_POINT('Ctrl Pts',(-10.9580963171636,13.5751175780247,2.81505729045284));
#95167=CARTESIAN_POINT('Ctrl Pts',(-10.9581406987863,13.5751226922339,2.81511937561826));
#95168=CARTESIAN_POINT('Ctrl Pts',(-10.9582324334248,13.5751332649644,2.8152477289804));
#95169=CARTESIAN_POINT('Ctrl Pts',(-10.9582797856225,13.5751387235199,2.81531399780552));
#95170=CARTESIAN_POINT('Ctrl Pts',(-10.9583776700008,13.5751500093831,2.81545101584856));
#95171=CARTESIAN_POINT('Ctrl Pts',(-10.9584282011931,13.5751558367238,2.81552176571005));
#95172=CARTESIAN_POINT('Ctrl Pts',(-10.9585326673003,13.5751678864106,2.81566806531123));
#95173=CARTESIAN_POINT('Ctrl Pts',(-10.9585866011312,13.5751741087998,2.81574361585117));
#95174=CARTESIAN_POINT('Ctrl Pts',(-10.9586981126653,13.5751869768063,2.81589986032844));
#95175=CARTESIAN_POINT('Ctrl Pts',(-10.9587556891234,13.5751936224723,2.81598055517396));
#95176=CARTESIAN_POINT('Ctrl Pts',(-10.9588747435295,13.5752073673585,2.81614745746432));
#95177=CARTESIAN_POINT('Ctrl Pts',(-10.9589362200376,13.5752144666327,2.81623366592729));
#95178=CARTESIAN_POINT('Ctrl Pts',(-10.9590633507186,13.5752291513047,2.81641199205616));
#95179=CARTESIAN_POINT('Ctrl Pts',(-10.9591290032387,13.5752367367637,2.81650411088112));
#95180=CARTESIAN_POINT('Ctrl Pts',(-10.9592399847994,13.5752495629612,2.81665987958547));
#95181=CARTESIAN_POINT('Ctrl Pts',(-10.9592853207868,13.5752548034373,2.81672352453131));
#95182=CARTESIAN_POINT('Ctrl Pts',(-10.9593926645419,13.5752672138162,2.81687425085038));
#95183=CARTESIAN_POINT('Ctrl Pts',(-10.959454666779,13.5752743839273,2.81696133614253));
#95184=CARTESIAN_POINT('Ctrl Pts',(-10.9596014023371,13.5752913571457,2.81716749309191));
#95185=CARTESIAN_POINT('Ctrl Pts',(-10.9596861253403,13.5753011606419,2.81728657206178));
#95186=CARTESIAN_POINT('Ctrl Pts',(-10.9598864906385,13.5753243534337,2.81756829834988));
#95187=CARTESIAN_POINT('Ctrl Pts',(-10.9600021137355,13.5753377434528,2.81773095926119));
#95188=CARTESIAN_POINT('Ctrl Pts',(-10.9604377907444,13.5753882220686,2.81834420850813));
#95189=CARTESIAN_POINT('Ctrl Pts',(-10.9607575684107,13.5754253210711,2.81879499216153));
#95190=CARTESIAN_POINT('Ctrl Pts',(-10.9640129001659,13.5758034862864,2.82339081468986));
#95191=CARTESIAN_POINT('Ctrl Pts',(-10.9669218883466,13.5761455489663,2.82755452133205));
#95192=CARTESIAN_POINT('Ctrl Pts',(-10.9736020181949,13.5769407942357,2.83724892913097));
#95193=CARTESIAN_POINT('Ctrl Pts',(-10.9773530906429,13.5773947141997,2.84279317960206));
#95194=CARTESIAN_POINT('Ctrl Pts',(-10.9894546955068,13.5788837245337,2.8610126317647));
#95195=CARTESIAN_POINT('Ctrl Pts',(-10.9976071953909,13.5799260369026,2.87381688174727));
#95196=CARTESIAN_POINT('Ctrl Pts',(-11.0476875402531,13.5865879756874,2.95593394741937));
#95197=CARTESIAN_POINT('Ctrl Pts',(-11.0826102054874,13.5924571720685,3.02924774727295));
#95198=CARTESIAN_POINT('Ctrl Pts',(-11.1283000118882,13.6024730078922,3.15778955476222));
#95199=CARTESIAN_POINT('Ctrl Pts',(-11.1431575516141,13.6065608364252,3.21127816082677));
#95200=CARTESIAN_POINT('Ctrl Pts',(-11.1574332193828,13.6117067526323,3.28157691914051));
#95201=CARTESIAN_POINT('Ctrl Pts',(-11.1603430830248,13.6128647311869,3.29760364190141));
#95202=CARTESIAN_POINT('Ctrl Pts',(-11.1646366415851,13.6147705898902,3.32440288491379));
#95203=CARTESIAN_POINT('Ctrl Pts',(-11.1662054179238,13.6155262969437,3.33514309808904));
#95204=CARTESIAN_POINT('Ctrl Pts',(-11.1681700458283,13.6165612030485,3.35002958950527));
#95205=CARTESIAN_POINT('Ctrl Pts',(-11.1686926650549,13.6168468914198,3.35415818169023));
#95206=CARTESIAN_POINT('Ctrl Pts',(-11.1695401059706,13.6173283651981,3.36115006002537));
#95207=CARTESIAN_POINT('Ctrl Pts',(-11.1698763178779,13.6175247716101,3.3640118878564));
#95208=CARTESIAN_POINT('Ctrl Pts',(-11.1704989192158,13.6178990636613,3.36948470765604));
#95209=CARTESIAN_POINT('Ctrl Pts',(-11.1707870830017,13.6180770494245,3.37209547292714));
#95210=CARTESIAN_POINT('Ctrl Pts',(-11.1714566053047,13.6185023549,3.3783532565542));
#95211=CARTESIAN_POINT('Ctrl Pts',(-11.1718296735018,13.6187492158504,3.38200116310408));
#95212=CARTESIAN_POINT('Ctrl Pts',(-11.1731166311541,13.6196383214344,3.39519367817268));
#95213=CARTESIAN_POINT('Ctrl Pts',(-11.1739310261744,13.6202753133151,3.40474793549087));
#95214=CARTESIAN_POINT('Ctrl Pts',(-11.1797107167689,13.6255083152135,3.48397661004278));
#95215=CARTESIAN_POINT('Ctrl Pts',(-11.1785858277258,13.6298210261132,3.55396616523511));
#95216=CARTESIAN_POINT('Ctrl Pts',(-11.1618892000277,13.6396630712478,3.71237768456328));
#95217=CARTESIAN_POINT('Ctrl Pts',(-11.1424217473845,13.6451804339534,3.79993435395114));
#95218=CARTESIAN_POINT('Ctrl Pts',(-11.1095616486035,13.6517881176117,3.89508847418353));
#95219=CARTESIAN_POINT('Ctrl Pts',(-11.1057321892027,13.6525322409155,3.90568246913281));
#95220=CARTESIAN_POINT('Ctrl Pts',(-11.0996424231589,13.6536782737071,3.92180234551705));
#95221=CARTESIAN_POINT('Ctrl Pts',(-11.0974910095438,13.6540765617867,3.92736887957926));
#95222=CARTESIAN_POINT('Ctrl Pts',(-11.0936603686493,13.6547745591338,3.937060516188));
#95223=CARTESIAN_POINT('Ctrl Pts',(-11.0919998612064,13.655073635123,3.94119292712881));
#95224=CARTESIAN_POINT('Ctrl Pts',(-11.0881965115769,13.6557509380498,3.95050508968752));
#95225=CARTESIAN_POINT('Ctrl Pts',(-11.086040060146,13.6561296187427,3.95567912998674));
#95226=CARTESIAN_POINT('Ctrl Pts',(-11.0801029187098,13.6571581023281,3.96964273243618));
#95227=CARTESIAN_POINT('Ctrl Pts',(-11.0762519879975,13.6578102749233,3.97840177673734));
#95228=CARTESIAN_POINT('Ctrl Pts',(-11.0573164384922,13.6609484607955,4.02008513285995));
#95229=CARTESIAN_POINT('Ctrl Pts',(-11.0408267525123,13.6634821863851,4.05234570360193));
#95230=CARTESIAN_POINT('Ctrl Pts',(-10.9836168486827,13.6717012577846,4.15258470600033));
#95231=CARTESIAN_POINT('Ctrl Pts',(-10.937518500822,13.6775515322287,4.21723446593321));
#95232=CARTESIAN_POINT('Ctrl Pts',(-10.8537452691142,13.6868594860221,4.31271255929083));
#95233=CARTESIAN_POINT('Ctrl Pts',(-10.8200361964558,13.6903339281926,4.34671383157753));
#95234=CARTESIAN_POINT('Ctrl Pts',(-10.7772152675003,13.6943536858202,4.38494233873553));
#95235=CARTESIAN_POINT('Ctrl Pts',(-10.7700038414104,13.6950181906,4.39122422205394));
#95236=CARTESIAN_POINT('Ctrl Pts',(-10.7597172660206,13.6959476884215,4.39996679403401));
#95237=CARTESIAN_POINT('Ctrl Pts',(-10.7567053065854,13.6962176684068,4.40250076718877));
#95238=CARTESIAN_POINT('Ctrl Pts',(-10.7515082887924,13.6966796915226,4.40682873042328));
#95239=CARTESIAN_POINT('Ctrl Pts',(-10.7493294022561,13.6968722543313,4.40863001383457));
#95240=CARTESIAN_POINT('Ctrl Pts',(-10.7450649958844,13.6972468851916,4.41212962207686));
#95241=CARTESIAN_POINT('Ctrl Pts',(-10.7429801459825,13.6974290089771,4.41382864838428));
#95242=CARTESIAN_POINT('Ctrl Pts',(-10.737266338376,13.697925389384,4.41845257509309));
#95243=CARTESIAN_POINT('Ctrl Pts',(-10.7336257597137,13.6982386425474,4.42136313845611));
#95244=CARTESIAN_POINT('Ctrl Pts',(-10.7194639059679,13.6994459938885,4.43254807300959));
#95245=CARTESIAN_POINT('Ctrl Pts',(-10.708818675215,13.7003297907966,4.44066484129783));
#95246=CARTESIAN_POINT('Ctrl Pts',(-10.6053827879264,13.7087173600827,4.5167792753322));
#95247=CARTESIAN_POINT('Ctrl Pts',(-10.5032289643628,13.7155346634489,4.57102605133776));
#95248=CARTESIAN_POINT('Ctrl Pts',(-10.3549969182846,13.725463620884,4.62376984473207));
#95249=CARTESIAN_POINT('Ctrl Pts',(-10.3144468292726,13.7281761767541,4.63578345379587));
#95250=CARTESIAN_POINT('Ctrl Pts',(-10.2639297692958,13.7315972382886,4.647836997508));
#95251=CARTESIAN_POINT('Ctrl Pts',(-10.2544904682267,13.732238153732,4.64996664662525));
#95252=CARTESIAN_POINT('Ctrl Pts',(-10.2394867963268,13.7332600160616,4.65315792950868));
#95253=CARTESIAN_POINT('Ctrl Pts',(-10.2339390256806,13.7336385351313,4.65429617792355));
#95254=CARTESIAN_POINT('Ctrl Pts',(-10.2234812036489,13.7343534278153,4.6563633442928));
#95255=CARTESIAN_POINT('Ctrl Pts',(-10.2185730136894,13.7346895136851,4.65730111413302));
#95256=CARTESIAN_POINT('Ctrl Pts',(-10.2075036684653,13.7354488211718,4.65934311936162));
#95257=CARTESIAN_POINT('Ctrl Pts',(-10.2013394190801,13.7358725933673,4.66042952243653));
#95258=CARTESIAN_POINT('Ctrl Pts',(-10.1855160225851,13.7369629227721,4.66308840474104));
#95259=CARTESIAN_POINT('Ctrl Pts',(-10.1758455653866,13.737631681646,4.66458969554645));
#95260=CARTESIAN_POINT('Ctrl Pts',(-10.1065625485152,13.7424411949564,4.67446294186497));
#95261=CARTESIAN_POINT('Ctrl Pts',(-10.0464136340409,13.7467200345899,4.67837280857284));
#95262=CARTESIAN_POINT('Ctrl Pts',(-9.9095344838565,13.7566576515529,4.67677323133549));
#95263=CARTESIAN_POINT('Ctrl Pts',(-9.83310517157141,13.7623545476245,4.66838565075373));
#95264=CARTESIAN_POINT('Ctrl Pts',(-9.73011173089593,13.7699350525143,4.64676478192213));
#95265=CARTESIAN_POINT('Ctrl Pts',(-9.70240777036819,13.7719622646432,4.63988960619347));
#95266=CARTESIAN_POINT('Ctrl Pts',(-9.66941238963437,13.7743417068642,4.6304160429034));
#95267=CARTESIAN_POINT('Ctrl Pts',(-9.66385799175535,13.7747410426571,4.62877683884532));
#95268=CARTESIAN_POINT('Ctrl Pts',(-9.65521195172755,13.775360512601,4.62615575446605));
#95269=CARTESIAN_POINT('Ctrl Pts',(-9.6521119858812,13.7755821870185,4.62520198712178));
#95270=CARTESIAN_POINT('Ctrl Pts',(-9.64633640990524,13.7759943340786,4.62339886385133));
#95271=CARTESIAN_POINT('Ctrl Pts',(-9.64365991029343,13.7761849794942,4.62255275288277));
#95272=CARTESIAN_POINT('Ctrl Pts',(-9.63755906893324,13.7766187613243,4.62060009980835));
#95273=CARTESIAN_POINT('Ctrl Pts',(-9.63413675550088,13.7768615403301,4.61948742707967));
#95274=CARTESIAN_POINT('Ctrl Pts',(-9.62504913291682,13.7775048749432,4.61648670794037));
#95275=CARTESIAN_POINT('Ctrl Pts',(-9.61939290317957,13.7779039019124,4.61457120151641));
#95276=CARTESIAN_POINT('Ctrl Pts',(-9.5745383056594,13.7810589832932,4.59899972014237));
#95277=CARTESIAN_POINT('Ctrl Pts',(-9.53606748865475,13.7837090559223,4.58332150630182));
#95278=CARTESIAN_POINT('Ctrl Pts',(-9.40892768768725,13.7925296261455,4.52348858821099));
#95279=CARTESIAN_POINT('Ctrl Pts',(-9.32502927893121,13.7984922310723,4.47021156070371));
#95280=CARTESIAN_POINT('Ctrl Pts',(-9.22688979229238,13.8066510846131,4.38893404794141));
#95281=CARTESIAN_POINT('Ctrl Pts',(-9.20566170672081,13.8084963334957,4.37001701294896));
#95282=CARTESIAN_POINT('Ctrl Pts',(-9.178974172662,13.8109372647052,4.34444335479706));
#95283=CARTESIAN_POINT('Ctrl Pts',(-9.17287298940522,13.8115039685292,4.33846818102104));
#95284=CARTESIAN_POINT('Ctrl Pts',(-9.16301582504219,13.8124341841259,4.32860231045058));
#95285=CARTESIAN_POINT('Ctrl Pts',(-9.15922063680212,13.8127959665367,4.32475108898084));
#95286=CARTESIAN_POINT('Ctrl Pts',(-9.15193534143306,13.8134976062578,4.31725568644012));
#95287=CARTESIAN_POINT('Ctrl Pts',(-9.148441863977,13.8138373067466,4.31361493455832));
#95288=CARTESIAN_POINT('Ctrl Pts',(-9.14043045396525,13.8146239446295,4.30515766636802));
#95289=CARTESIAN_POINT('Ctrl Pts',(-9.13592945747042,13.8150715887553,4.3003254129583));
#95290=CARTESIAN_POINT('Ctrl Pts',(-9.12149239871536,13.8165262068976,4.28456208646076));
#95291=CARTESIAN_POINT('Ctrl Pts',(-9.11172162932854,13.8175400017292,4.27348223941367));
#95292=CARTESIAN_POINT('Ctrl Pts',(-9.04501330910967,13.8246736787696,4.1949050630136));
#95293=CARTESIAN_POINT('Ctrl Pts',(-8.995626923395,13.8310972106859,4.1213868490978));
#95294=CARTESIAN_POINT('Ctrl Pts',(-8.92286403594545,13.8426862350412,3.98136041730383));
#95295=CARTESIAN_POINT('Ctrl Pts',(-8.89632618578527,13.8477973819049,3.91693644362181));
#95296=CARTESIAN_POINT('Ctrl Pts',(-8.87348693407732,13.8531387845478,3.84367869390256));
#95297=CARTESIAN_POINT('Ctrl Pts',(-8.87141027540495,13.8536360632117,3.83679663350687));
#95298=CARTESIAN_POINT('Ctrl Pts',(-8.86840942961839,13.8543720453029,3.82651227589115));
#95299=CARTESIAN_POINT('Ctrl Pts',(-8.8674373431335,13.8546133515125,3.82312430174083));
#95300=CARTESIAN_POINT('Ctrl Pts',(-8.8657961656235,13.855025731446,3.81730596949489));
#95301=CARTESIAN_POINT('Ctrl Pts',(-8.86511965278477,13.8551972259385,3.81487777651457));
#95302=CARTESIAN_POINT('Ctrl Pts',(-8.86359991743127,13.8555859293475,3.80935449702826));
#95303=CARTESIAN_POINT('Ctrl Pts',(-8.86276154060812,13.8558028585223,3.80625812576336));
#95304=CARTESIAN_POINT('Ctrl Pts',(-8.86051264451303,13.8563917600933,3.79781571158757));
#95305=CARTESIAN_POINT('Ctrl Pts',(-8.85912708047707,13.8567623413735,3.79246301624323));
#95306=CARTESIAN_POINT('Ctrl Pts',(-8.85240486067107,13.8586009027975,3.76571887764112));
#95307=CARTESIAN_POINT('Ctrl Pts',(-8.84763150986869,13.8600396522329,3.74418873900679));
#95308=CARTESIAN_POINT('Ctrl Pts',(-8.83929991925633,13.8628740845775,3.70088882330947));
#95309=CARTESIAN_POINT('Ctrl Pts',(-8.83574307899585,13.8642692075345,3.67912820921873));
#95310=CARTESIAN_POINT('Ctrl Pts',(-8.81951972453853,13.8718885244967,3.55873166698399));
#95311=CARTESIAN_POINT('Ctrl Pts',(-8.81877412799166,13.8778773812607,3.45890256575597));
#95312=CARTESIAN_POINT('Ctrl Pts',(-8.83384492767943,13.8860128287073,3.33286768864652));
#95313=CARTESIAN_POINT('Ctrl Pts',(-8.83806359829453,13.8877986916465,3.30569490219117));
#95314=CARTESIAN_POINT('Ctrl Pts',(-8.84481367003323,13.8901713674797,3.27041178464878));
#95315=CARTESIAN_POINT('Ctrl Pts',(-8.84648748461026,13.8907311671799,3.26214484186287));
#95316=CARTESIAN_POINT('Ctrl Pts',(-8.84937393933931,13.8916525775312,3.24863638678061));
#95317=CARTESIAN_POINT('Ctrl Pts',(-8.8505339738379,13.8920125148162,3.24338384582235));
#95318=CARTESIAN_POINT('Ctrl Pts',(-8.85285201063279,13.8927123750817,3.23321914989296));
#95319=CARTESIAN_POINT('Ctrl Pts',(-8.85400568666601,13.8930521533253,3.22830612091752));
#95320=CARTESIAN_POINT('Ctrl Pts',(-8.85675126789243,13.893841612703,3.21694251054581));
#95321=CARTESIAN_POINT('Ctrl Pts',(-8.85836624035557,13.8942920221327,3.21049773490765));
#95322=CARTESIAN_POINT('Ctrl Pts',(-8.86381274788838,13.8957672421158,3.18951722155798));
#95323=CARTESIAN_POINT('Ctrl Pts',(-8.86786791994183,13.8967991633061,3.17504162658661));
#95324=CARTESIAN_POINT('Ctrl Pts',(-8.89567888278933,13.9034819468154,3.08261473276687));
#95325=CARTESIAN_POINT('Ctrl Pts',(-8.92718991450157,13.9093869741405,3.00724294296085));
#95326=CARTESIAN_POINT('Ctrl Pts',(-8.99234167440492,13.9193681275152,2.88787836535474));
#95327=CARTESIAN_POINT('Ctrl Pts',(-9.02175873092889,13.9233853947298,2.84188694652679));
#95328=CARTESIAN_POINT('Ctrl Pts',(-9.0638617489985,13.9284507956855,2.78515741740613));
#95329=CARTESIAN_POINT('Ctrl Pts',(-9.07373064219927,13.9295960702767,2.77241503962706));
#95330=CARTESIAN_POINT('Ctrl Pts',(-9.09062058950655,13.9314827335434,2.75150822335539));
#95331=CARTESIAN_POINT('Ctrl Pts',(-9.09749743467583,13.9322317757757,2.74323055548128));
#95332=CARTESIAN_POINT('Ctrl Pts',(-9.10717724766102,13.9332587311535,2.73189860642526));
#95333=CARTESIAN_POINT('Ctrl Pts',(-9.109884075508,13.9335430220645,2.72876342139365));
#95334=CARTESIAN_POINT('Ctrl Pts',(-9.11449743501834,13.934022600436,2.72347663714609));
#95335=CARTESIAN_POINT('Ctrl Pts',(-9.11639539096728,13.9342185015318,2.72131763777697));
#95336=CARTESIAN_POINT('Ctrl Pts',(-9.12005448079591,13.9345934720572,2.7171858850478));
#95337=CARTESIAN_POINT('Ctrl Pts',(-9.1218143695892,13.9347726335102,2.71521209602311));
#95338=CARTESIAN_POINT('Ctrl Pts',(-9.12605217987942,13.9352012684823,2.7104913199606));
#95339=CARTESIAN_POINT('Ctrl Pts',(-9.1285364448156,13.9354502765422,2.70775002615424));
#95340=CARTESIAN_POINT('Ctrl Pts',(-9.13761476888779,13.9363522463308,2.69782680458505));
#95341=CARTESIAN_POINT('Ctrl Pts',(-9.14428524894664,13.9369998050882,2.69071488192203));
#95342=CARTESIAN_POINT('Ctrl Pts',(-9.19362088137094,13.9416872011651,2.63940641375144));
#95343=CARTESIAN_POINT('Ctrl Pts',(-9.23960328365098,13.9455113311542,2.59851930416609));
#95344=CARTESIAN_POINT('Ctrl Pts',(-9.34179465846534,13.9534495045036,2.52106134062607));
#95345=CARTESIAN_POINT('Ctrl Pts',(-9.39834918957576,13.9575489475891,2.48532229443791));
#95346=CARTESIAN_POINT('Ctrl Pts',(-9.48841018205785,13.9639993488808,2.43859825527454));
#95347=CARTESIAN_POINT('Ctrl Pts',(-9.51988218467226,13.966238642925,2.42399613012846));
#95348=CARTESIAN_POINT('Ctrl Pts',(-9.56037982440296,13.9691265666893,2.40733708591038));
#95349=CARTESIAN_POINT('Ctrl Pts',(-9.56884908011646,13.969730814859,2.40396760122025));
#95350=CARTESIAN_POINT('Ctrl Pts',(-9.58252058453984,13.9707071043735,2.39871138615557));
#95351=CARTESIAN_POINT('Ctrl Pts',(-9.58769861987652,13.9710770709956,2.39676238122097));
#95352=CARTESIAN_POINT('Ctrl Pts',(-9.59758876495487,13.9717841870312,2.39311909694426));
#95353=CARTESIAN_POINT('Ctrl Pts',(-9.6022983353999,13.9721211100489,2.39141823924401));
#95354=CARTESIAN_POINT('Ctrl Pts',(-9.61309449953994,13.9728940032584,2.38759686327273));
#95355=CARTESIAN_POINT('Ctrl Pts',(-9.61918789655179,13.9733306141381,2.38549618938032));
#95356=CARTESIAN_POINT('Ctrl Pts',(-9.63812054231927,13.9746885706761,2.37914262674409));
#95357=CARTESIAN_POINT('Ctrl Pts',(-9.65101564356648,13.9756154411713,2.37506094142421));
#95358=CARTESIAN_POINT('Ctrl Pts',(-9.71230321476705,13.9800316165875,2.35681675951342));
#95359=CARTESIAN_POINT('Ctrl Pts',(-9.76144827564538,13.9836081681662,2.34556553370857));
#95360=CARTESIAN_POINT('Ctrl Pts',(-9.81110406371067,13.9872487449619,2.3374969300026));
#95361=CARTESIAN_POINT('Origin',(-10.,12.3756328852638,3.5));
#95362=CARTESIAN_POINT('',(-9.81110404096668,14.5872589185639,2.33749693369829));
#95363=CARTESIAN_POINT('',(-9.81110406371066,14.4889165240206,2.3374969300026));
#95364=CARTESIAN_POINT('',(-9.81110406371068,12.3756328852638,2.3374969300026));
#95365=CARTESIAN_POINT('Ctrl Pts',(-9.81110404084991,14.5872589202102,2.33749693371726));
#95366=CARTESIAN_POINT('Ctrl Pts',(-9.73264000287283,14.5815501908489,2.35024661166853));
#95367=CARTESIAN_POINT('Ctrl Pts',(-9.65565256030276,14.5756541343893,2.37091040782615));
#95368=CARTESIAN_POINT('Ctrl Pts',(-9.54248844072707,14.566835354911,2.41394988717991));
#95369=CARTESIAN_POINT('Ctrl Pts',(-9.50445426554587,14.5638473808157,2.4307680800128));
#95370=CARTESIAN_POINT('Ctrl Pts',(-9.46175911294319,14.560523640647,2.45241630542129));
#95371=CARTESIAN_POINT('Ctrl Pts',(-9.45615611418438,14.5600881018448,2.45531407497928));
#95372=CARTESIAN_POINT('Ctrl Pts',(-9.4476170202585,14.5594256245441,2.45981765969876));
#95373=CARTESIAN_POINT('Ctrl Pts',(-9.44466414517122,14.5591967743601,2.46139114849266));
#95374=CARTESIAN_POINT('Ctrl Pts',(-9.43926218842847,14.5587786122528,2.46429929617265));
#95375=CARTESIAN_POINT('Ctrl Pts',(-9.43681114171983,14.5585890714669,2.46563007028998));
#95376=CARTESIAN_POINT('Ctrl Pts',(-9.43129738739931,14.5581631114296,2.46864912345498));
#95377=CARTESIAN_POINT('Ctrl Pts',(-9.42823745994013,14.557927007139,2.47034234295588));
#95378=CARTESIAN_POINT('Ctrl Pts',(-9.42037562274466,14.5573210099128,2.474738566366));
#95379=CARTESIAN_POINT('Ctrl Pts',(-9.41558499322758,14.5569523458842,2.47746172258458));
#95380=CARTESIAN_POINT('Ctrl Pts',(-9.38510554727746,14.5546094912099,2.49507145204672));
#95381=CARTESIAN_POINT('Ctrl Pts',(-9.35996585795815,14.5526893191643,2.51089271967742));
#95382=CARTESIAN_POINT('Ctrl Pts',(-9.26634638223819,14.5454794389545,2.57487673608849));
#95383=CARTESIAN_POINT('Ctrl Pts',(-9.20247190936922,14.5404184714153,2.62933851271936));
#95384=CARTESIAN_POINT('Ctrl Pts',(-9.12061717821991,14.532972886158,2.7157623252128));
#95385=CARTESIAN_POINT('Ctrl Pts',(-9.09749400375314,14.530738680265,2.74248728932871));
#95386=CARTESIAN_POINT('Ctrl Pts',(-9.0662397686027,14.5274852900465,2.78207558837813));
#95387=CARTESIAN_POINT('Ctrl Pts',(-9.0571013367366,14.5265024860349,2.79412061263111));
#95388=CARTESIAN_POINT('Ctrl Pts',(-9.04120268350903,14.5247321993151,2.81593580783669));
#95389=CARTESIAN_POINT('Ctrl Pts',(-9.03435356697208,14.5239481248307,2.82563877433802));
#95390=CARTESIAN_POINT('Ctrl Pts',(-9.02419888976221,14.5227515617678,2.84049661202843));
#95391=CARTESIAN_POINT('Ctrl Pts',(-9.02078472668893,14.5223431556051,2.8455766113511));
#95392=CARTESIAN_POINT('Ctrl Pts',(-9.01466695704583,14.521600025742,2.85483442564166));
#95393=CARTESIAN_POINT('Ctrl Pts',(-9.01194991969964,14.5212658114497,2.85900322825458));
#95394=CARTESIAN_POINT('Ctrl Pts',(-9.00615673021706,14.5205440661581,2.86801618272543));
#95395=CARTESIAN_POINT('Ctrl Pts',(-9.00308941099939,14.5201562209205,2.87286583117512));
#95396=CARTESIAN_POINT('Ctrl Pts',(-8.99488133353557,14.5191026229107,2.88605577197509));
#95397=CARTESIAN_POINT('Ctrl Pts',(-8.98980910245449,14.5184344028053,2.89443795593845));
#95398=CARTESIAN_POINT('Ctrl Pts',(-8.96438691808017,14.5149948828639,2.93765812262217));
#95399=CARTESIAN_POINT('Ctrl Pts',(-8.94573446475574,14.5121640843382,2.97345811443405));
#95400=CARTESIAN_POINT('Ctrl Pts',(-8.89335665811802,14.5031613765447,3.08797857263325));
#95401=CARTESIAN_POINT('Ctrl Pts',(-8.86634984066145,14.496809411726,3.16946136577115));
#95402=CARTESIAN_POINT('Ctrl Pts',(-8.84054923377066,14.4878467864521,3.2898183750055));
#95403=CARTESIAN_POINT('Ctrl Pts',(-8.83444225197902,14.4851474660677,3.32685813938582));
#95404=CARTESIAN_POINT('Ctrl Pts',(-8.82913102193451,14.481932028478,3.37258951061053));
#95405=CARTESIAN_POINT('Ctrl Pts',(-8.82824025575684,14.481341377353,3.38106006174251));
#95406=CARTESIAN_POINT('Ctrl Pts',(-8.82708727728855,14.4804957438544,3.39329917761145));
#95407=CARTESIAN_POINT('Ctrl Pts',(-8.82675120554481,14.4802369409126,3.3970602705151));
#95408=CARTESIAN_POINT('Ctrl Pts',(-8.82619613198177,14.4797869049151,3.40362848453897));
#95409=CARTESIAN_POINT('Ctrl Pts',(-8.82596909934797,14.4795952350433,3.40643486458907));
#95410=CARTESIAN_POINT('Ctrl Pts',(-8.82550866394301,14.4791896966777,3.41239209149528));
#95411=CARTESIAN_POINT('Ctrl Pts',(-8.82527787407733,14.4789759730277,3.41554307862269));
#95412=CARTESIAN_POINT('Ctrl Pts',(-8.82468395314806,14.4783958551932,3.42412584259327));
#95413=CARTESIAN_POINT('Ctrl Pts',(-8.82434579237486,14.4780308109477,3.4295593533412));
#95414=CARTESIAN_POINT('Ctrl Pts',(-8.8229250170195,14.4763136658107,3.45526154763617));
#95415=CARTESIAN_POINT('Ctrl Pts',(-8.82232873498976,14.4749861523923,3.47555502651146));
#95416=CARTESIAN_POINT('Ctrl Pts',(-8.82187983523047,14.466762875616,3.60311004156625));
#95417=CARTESIAN_POINT('Ctrl Pts',(-8.83615443400348,14.4603707737357,3.70992193752649));
#95418=CARTESIAN_POINT('Ctrl Pts',(-8.87573150267509,14.4509768423277,3.85332168356678));
#95419=CARTESIAN_POINT('Ctrl Pts',(-8.88887151538865,14.4483130949146,3.89269424801518));
#95420=CARTESIAN_POINT('Ctrl Pts',(-8.90757945971336,14.4449476375499,3.94023267430271));
#95421=CARTESIAN_POINT('Ctrl Pts',(-8.91120844680046,14.4443109870414,3.94913293022181));
#95422=CARTESIAN_POINT('Ctrl Pts',(-8.91713951200369,14.4432949032357,3.96318468038759));
#95423=CARTESIAN_POINT('Ctrl Pts',(-8.91937042827779,14.4429178632868,3.96836589483924));
#95424=CARTESIAN_POINT('Ctrl Pts',(-8.92364343451001,14.4422051398109,3.97809672030202));
#95425=CARTESIAN_POINT('Ctrl Pts',(-8.92567737296342,14.4418697387309,3.98264979204127));
#95426=CARTESIAN_POINT('Ctrl Pts',(-8.9303290908312,14.4411111536934,3.99288779552198));
#95427=CARTESIAN_POINT('Ctrl Pts',(-8.93296337693814,14.4406874139692,3.99856501613632));
#95428=CARTESIAN_POINT('Ctrl Pts',(-8.93984186190897,14.4395955920379,4.01308477468371));
#95429=CARTESIAN_POINT('Ctrl Pts',(-8.94415142862732,14.4389252845774,4.02189562937801));
#95430=CARTESIAN_POINT('Ctrl Pts',(-8.97624552973583,14.4340295424099,4.08548669269776));
#95431=CARTESIAN_POINT('Ctrl Pts',(-9.00816324131603,14.4296595554093,4.13806388105814));
#95432=CARTESIAN_POINT('Ctrl Pts',(-9.08854031040138,14.419658475103,4.2497624626265));
#95433=CARTESIAN_POINT('Ctrl Pts',(-9.13894833428935,14.4139960358093,4.30715071585918));
#95434=CARTESIAN_POINT('Ctrl Pts',(-9.21531167254281,14.4064546780836,4.37873169194922));
#95435=CARTESIAN_POINT('Ctrl Pts',(-9.23677802794976,14.4044321151721,4.39743951654077));
#95436=CARTESIAN_POINT('Ctrl Pts',(-9.2633893762249,14.4020586383702,4.41898485868214));
#95437=CARTESIAN_POINT('Ctrl Pts',(-9.26790236514378,14.4016605694306,4.42258410890734));
#95438=CARTESIAN_POINT('Ctrl Pts',(-9.27498271756564,14.4010431780308,4.42814624045627));
#95439=CARTESIAN_POINT('Ctrl Pts',(-9.27753192946841,14.4008223167546,4.43013192139706));
#95440=CARTESIAN_POINT('Ctrl Pts',(-9.28230582032924,14.4004114125545,4.43381902447509));
#95441=CARTESIAN_POINT('Ctrl Pts',(-9.28452837927286,14.4002211993335,4.43552299072252));
#95442=CARTESIAN_POINT('Ctrl Pts',(-9.28961498517904,14.3997883240167,4.43939400213159));
#95443=CARTESIAN_POINT('Ctrl Pts',(-9.29248288275444,14.3995460192511,4.44155588797786));
#95444=CARTESIAN_POINT('Ctrl Pts',(-9.30013106146574,14.3989043528509,4.44726658089956));
#95445=CARTESIAN_POINT('Ctrl Pts',(-9.30492851287194,14.3985065116086,4.45079237367361));
#95446=CARTESIAN_POINT('Ctrl Pts',(-9.34307555762783,14.3953778621256,4.47838474720255));
#95447=CARTESIAN_POINT('Ctrl Pts',(-9.37764224990899,14.3927512729352,4.50072877069635));
#95448=CARTESIAN_POINT('Ctrl Pts',(-9.49828100304296,14.3840154862437,4.57003546326752));
#95449=CARTESIAN_POINT('Ctrl Pts',(-9.58900820655437,14.3781136227497,4.60805425962421));
#95450=CARTESIAN_POINT('Ctrl Pts',(-9.71199951890322,14.3699505493562,4.64238021054537));
#95451=CARTESIAN_POINT('Ctrl Pts',(-9.74089044610851,14.3680252040898,4.64927752374096));
#95452=CARTESIAN_POINT('Ctrl Pts',(-9.7785090328746,14.3654930393325,4.6567678779022));
#95453=CARTESIAN_POINT('Ctrl Pts',(-9.78702697339062,14.3649180666082,4.65836637344915));
#95454=CARTESIAN_POINT('Ctrl Pts',(-9.8009133653959,14.3639777425019,4.66081398410473));
#95455=CARTESIAN_POINT('Ctrl Pts',(-9.80627152323963,14.3636141956293,4.6617202199232));
#95456=CARTESIAN_POINT('Ctrl Pts',(-9.81660584461781,14.3629115536109,4.66339460081994));
#95457=CARTESIAN_POINT('Ctrl Pts',(-9.82158104883559,14.3625726313256,4.66416798184521));
#95458=CARTESIAN_POINT('Ctrl Pts',(-9.83302771798309,14.3617912863312,4.66587223359262));
#95459=CARTESIAN_POINT('Ctrl Pts',(-9.83950223165438,14.3613481863132,4.66678115830852));
#95460=CARTESIAN_POINT('Ctrl Pts',(-9.85687772268891,14.3601558057525,4.66907305895338));
#95461=CARTESIAN_POINT('Ctrl Pts',(-9.8677908216153,14.3594034823178,4.67035743358119));
#95462=CARTESIAN_POINT('Ctrl Pts',(-9.96419430095064,14.3527257314768,4.68033773816634));
#95463=CARTESIAN_POINT('Ctrl Pts',(-10.050363621197,14.3465069882368,4.67980387788985));
#95464=CARTESIAN_POINT('Ctrl Pts',(-10.189721208297,14.3362107372443,4.66364062834722));
#95465=CARTESIAN_POINT('Ctrl Pts',(-10.2432553713255,14.3322039410379,4.65363817832549));
#95466=CARTESIAN_POINT('Ctrl Pts',(-10.311488669028,14.3271498289074,4.63592647942645));
#95467=CARTESIAN_POINT('Ctrl Pts',(-10.3269850636592,14.3260059201405,4.63156306955655));
#95468=CARTESIAN_POINT('Ctrl Pts',(-10.3526776703631,14.324121049715,4.62375672489656));
#95469=CARTESIAN_POINT('Ctrl Pts',(-10.3629245853431,14.3233724665536,4.62048939390675));
#95470=CARTESIAN_POINT('Ctrl Pts',(-10.3770566629269,14.3223457842745,4.61576902245199));
#95471=CARTESIAN_POINT('Ctrl Pts',(-10.3809806915762,14.3220613244956,4.61443526168062));
#95472=CARTESIAN_POINT('Ctrl Pts',(-10.3876172557555,14.3215813719677,4.61214037156372));
#95473=CARTESIAN_POINT('Ctrl Pts',(-10.3903334349332,14.3213852658928,4.61118997172978));
#95474=CARTESIAN_POINT('Ctrl Pts',(-10.3955403583679,14.3210099915795,4.60934660413308));
#95475=CARTESIAN_POINT('Ctrl Pts',(-10.3980316021944,14.3208307308099,4.60845518953512));
#95476=CARTESIAN_POINT('Ctrl Pts',(-10.4040027081984,14.3204017170422,4.60629588757482));
#95477=CARTESIAN_POINT('Ctrl Pts',(-10.4074796626152,14.3201524311404,4.60501995664189));
#95478=CARTESIAN_POINT('Ctrl Pts',(-10.4201117850419,14.3192484721804,4.6003166420171));
#95479=CARTESIAN_POINT('Ctrl Pts',(-10.4292305172535,14.3185992334928,4.59679159507934));
#95480=CARTESIAN_POINT('Ctrl Pts',(-10.4943381814432,14.3139801973661,4.57068638787015));
#95481=CARTESIAN_POINT('Ctrl Pts',(-10.5485691008014,14.3102184417342,4.54394130243486));
#95482=CARTESIAN_POINT('Ctrl Pts',(-10.6452222952771,14.3032610814468,4.48665298970563));
#95483=CARTESIAN_POINT('Ctrl Pts',(-10.6881248406501,14.300067138377,4.45722512778002));
#95484=CARTESIAN_POINT('Ctrl Pts',(-10.7543034527767,14.2947795072184,4.40507672135662));
#95485=CARTESIAN_POINT('Ctrl Pts',(-10.7788297166669,14.2927302248712,4.38405972772681));
#95486=CARTESIAN_POINT('Ctrl Pts',(-10.8179429628558,14.2892768660397,4.34765074966016));
#95487=CARTESIAN_POINT('Ctrl Pts',(-10.8330336614378,14.2878947452755,4.33282489931588));
#95488=CARTESIAN_POINT('Ctrl Pts',(-10.8530453213413,14.2859871013514,4.31207614809921));
#95489=CARTESIAN_POINT('Ctrl Pts',(-10.8583201137776,14.2854768522161,4.30649895734428));
#95490=CARTESIAN_POINT('Ctrl Pts',(-10.8670914668152,14.2846155292308,4.29704123427556));
#95491=CARTESIAN_POINT('Ctrl Pts',(-10.87061746483,14.28426571181,4.29318823074503));
#95492=CARTESIAN_POINT('Ctrl Pts',(-10.8775300331416,14.2835727227812,4.285532958229));
#95493=CARTESIAN_POINT('Ctrl Pts',(-10.880917806817,14.2832296122469,4.28173192576248));
#95494=CARTESIAN_POINT('Ctrl Pts',(-10.8883325728885,14.28247084347,4.27330326081019));
#95495=CARTESIAN_POINT('Ctrl Pts',(-10.8923482496271,14.2820547318367,4.26866591712193));
#95496=CARTESIAN_POINT('Ctrl Pts',(-10.9060170551065,14.2806202331725,4.25262957441468));
#95497=CARTESIAN_POINT('Ctrl Pts',(-10.915489109805,14.2795945958962,4.24107883153981));
#95498=CARTESIAN_POINT('Ctrl Pts',(-10.9701801319536,14.2734789660804,4.17173655161925));
#95499=CARTESIAN_POINT('Ctrl Pts',(-11.0101300409236,14.2681871430813,4.1100109374925));
#95500=CARTESIAN_POINT('Ctrl Pts',(-11.0813607104884,14.2569090456861,3.97354749953727));
#95501=CARTESIAN_POINT('Ctrl Pts',(-11.1112207757846,14.250934765998,3.89847034186178));
#95502=CARTESIAN_POINT('Ctrl Pts',(-11.135657489991,14.2446599959377,3.81218533621349));
#95503=CARTESIAN_POINT('Ctrl Pts',(-11.1380322124491,14.2440289071239,3.80341442745451));
#95504=CARTESIAN_POINT('Ctrl Pts',(-11.1412055172124,14.2431553772587,3.79113223984228));
#95505=CARTESIAN_POINT('Ctrl Pts',(-11.1420897950362,14.2429084116384,3.78764372846369));
#95506=CARTESIAN_POINT('Ctrl Pts',(-11.143589865252,14.2424832902934,3.78160990698921));
#95507=CARTESIAN_POINT('Ctrl Pts',(-11.1442131781064,14.2423047159504,3.77906652076811));
#95508=CARTESIAN_POINT('Ctrl Pts',(-11.1455098777837,14.2419291324763,3.77369803927709));
#95509=CARTESIAN_POINT('Ctrl Pts',(-11.1461813071118,14.2417322405769,3.77087249466002));
#95510=CARTESIAN_POINT('Ctrl Pts',(-11.1478159194166,14.2412467709209,3.76387872031982));
#95511=CARTESIAN_POINT('Ctrl Pts',(-11.1487668683433,14.2409588802991,3.75970761930416));
#95512=CARTESIAN_POINT('Ctrl Pts',(-11.1522262548034,14.2398904122838,3.74414303342827));
#95513=CARTESIAN_POINT('Ctrl Pts',(-11.1545881917732,14.2391176247597,3.73271720174538));
#95514=CARTESIAN_POINT('Ctrl Pts',(-11.170645175723,14.2335115634591,3.64876801158867));
#95515=CARTESIAN_POINT('Ctrl Pts',(-11.1776676828325,14.2289782333121,3.57512540585017));
#95516=CARTESIAN_POINT('Ctrl Pts',(-11.1778343182737,14.2196579903429,3.4243659146739));
#95517=CARTESIAN_POINT('Ctrl Pts',(-11.1703809414087,14.2148850839714,3.34761672360479));
#95518=CARTESIAN_POINT('Ctrl Pts',(-11.1525760591207,14.2088833636551,3.25732374774894));
#95519=CARTESIAN_POINT('Ctrl Pts',(-11.1493682062061,14.2078898815263,3.2425586900629));
#95520=CARTESIAN_POINT('Ctrl Pts',(-11.1443378381732,14.2064453880234,3.22137773996852));
#95521=CARTESIAN_POINT('Ctrl Pts',(-11.1427433951577,14.2060016082332,3.21490881912036));
#95522=CARTESIAN_POINT('Ctrl Pts',(-11.1398428676096,14.205218040621,3.20355632657173));
#95523=CARTESIAN_POINT('Ctrl Pts',(-11.13856005592,14.2048790041677,3.1986669416483));
#95524=CARTESIAN_POINT('Ctrl Pts',(-11.1358464168614,14.20417686628,3.18858877735184));
#95525=CARTESIAN_POINT('Ctrl Pts',(-11.1344114177484,14.2038136377548,3.18340125409942));
#95526=CARTESIAN_POINT('Ctrl Pts',(-11.1306382009037,14.2028786519867,3.170116144415));
#95527=CARTESIAN_POINT('Ctrl Pts',(-11.1282485588497,14.2023052489765,3.16203360738232));
#95528=CARTESIAN_POINT('Ctrl Pts',(-11.1177310394658,14.1998577387704,3.12781520676106));
#95529=CARTESIAN_POINT('Ctrl Pts',(-11.1087807353527,14.1979572603398,3.10194314153882));
#95530=CARTESIAN_POINT('Ctrl Pts',(-11.0630907116562,14.1890086969138,2.98340806077523));
#95531=CARTESIAN_POINT('Ctrl Pts',(-11.0155856838082,14.1816147802925,2.89534404959143));
#95532=CARTESIAN_POINT('Ctrl Pts',(-10.9447216564346,14.1727423995181,2.79637820105156));
#95533=CARTESIAN_POINT('Ctrl Pts',(-10.9313632835441,14.1711432197283,2.77878909356808));
#95534=CARTESIAN_POINT('Ctrl Pts',(-10.9037640573488,14.167994227367,2.74449566162142));
#95535=CARTESIAN_POINT('Ctrl Pts',(-10.8895345617414,14.1664447361073,2.72779232639233));
#95536=CARTESIAN_POINT('Ctrl Pts',(-10.8711474158172,14.1645420760754,2.70739180168754));
#95537=CARTESIAN_POINT('Ctrl Pts',(-10.8674202359574,14.1641612841618,2.70331454552107));
#95538=CARTESIAN_POINT('Ctrl Pts',(-10.8614826587253,14.1635625439229,2.69691034814909));
#95539=CARTESIAN_POINT('Ctrl Pts',(-10.8592912594282,14.1633432342188,2.69456602238922));
#95540=CARTESIAN_POINT('Ctrl Pts',(-10.8553597161028,14.1629527912163,2.69039442621587));
#95541=CARTESIAN_POINT('Ctrl Pts',(-10.8536232908956,14.1627813898922,2.68856380013272));
#95542=CARTESIAN_POINT('Ctrl Pts',(-10.8494426876443,14.1623712008741,2.68418467093694));
#95543=CARTESIAN_POINT('Ctrl Pts',(-10.8469929177981,14.1621328450294,2.68164156462753));
#95544=CARTESIAN_POINT('Ctrl Pts',(-10.8395029468061,14.1614100305416,2.67393588673134));
#95545=CARTESIAN_POINT('Ctrl Pts',(-10.8344265965686,14.1609282501319,2.66880845871165));
#95546=CARTESIAN_POINT('Ctrl Pts',(-10.7795990552481,14.1558063571191,2.61443780877662));
#95547=CARTESIAN_POINT('Ctrl Pts',(-10.7255913048443,14.1514675998386,2.56966922032444));
#95548=CARTESIAN_POINT('Ctrl Pts',(-10.5958008768419,14.1417215395552,2.48030243568998));
#95549=CARTESIAN_POINT('Ctrl Pts',(-10.5183800343025,14.1363337793593,2.43884886398708));
#95550=CARTESIAN_POINT('Ctrl Pts',(-10.4233475476614,14.1296562862507,2.40086817281709));
#95551=CARTESIAN_POINT('Ctrl Pts',(-10.4095085243001,14.1286831545855,2.39563744349147));
#95552=CARTESIAN_POINT('Ctrl Pts',(-10.3893517944854,14.1272629752923,2.38844977740205));
#95553=CARTESIAN_POINT('Ctrl Pts',(-10.3831099973379,14.1268228186416,2.38628305024445));
#95554=CARTESIAN_POINT('Ctrl Pts',(-10.3720698246499,14.1260434689013,2.38255444481612));
#95555=CARTESIAN_POINT('Ctrl Pts',(-10.3672789828027,14.1257050018039,2.38097065693091));
#95556=CARTESIAN_POINT('Ctrl Pts',(-10.3573358331121,14.1250018984862,2.37775431590113));
#95557=CARTESIAN_POINT('Ctrl Pts',(-10.3521821782253,14.1246371220853,2.37612634840046));
#95558=CARTESIAN_POINT('Ctrl Pts',(-10.3388654028385,14.1236935641894,2.37202035602145));
#95559=CARTESIAN_POINT('Ctrl Pts',(-10.3306863547233,14.1231130782288,2.36959548541245));
#95560=CARTESIAN_POINT('Ctrl Pts',(-10.2952191691576,14.1205912410778,2.35949826835654));
#95561=CARTESIAN_POINT('Ctrl Pts',(-10.2676873751124,14.1186214777836,2.35272418820644));
#95562=CARTESIAN_POINT('Ctrl Pts',(-10.1430641459899,14.1096442071177,2.32679114032415));
#95563=CARTESIAN_POINT('Ctrl Pts',(-10.0440427943208,14.1023015267758,2.31892384650854));
#95564=CARTESIAN_POINT('Ctrl Pts',(-9.9035096090453,14.0920496315411,2.32546654411423));
#95565=CARTESIAN_POINT('Ctrl Pts',(-9.86191931004656,14.0890442405331,2.32962665928955));
#95566=CARTESIAN_POINT('Ctrl Pts',(-9.81745516870227,14.0859176075736,2.33647828112878));
#95567=CARTESIAN_POINT('Ctrl Pts',(-9.81427858297399,14.0856947208985,2.33698110014891));
#95568=CARTESIAN_POINT('Ctrl Pts',(-9.81110406370735,14.0854724903439,2.33749693000314));
#95569=CARTESIAN_POINT('Ctrl Pts',(-9.81110406371067,13.9872487449619,2.3374969300026));
#95570=CARTESIAN_POINT('Ctrl Pts',(-9.86124441765218,13.9909248483166,2.32934958884876));
#95571=CARTESIAN_POINT('Ctrl Pts',(-9.9119055057115,13.9946661155459,2.32444717642581));
#95572=CARTESIAN_POINT('Ctrl Pts',(-10.0208057350382,14.0026584757658,2.32100320952519));
#95573=CARTESIAN_POINT('Ctrl Pts',(-10.0789026720657,14.0068920700218,2.32346173844195));
#95574=CARTESIAN_POINT('Ctrl Pts',(-10.1437676225063,14.0114381200553,2.33103541673644));
#95575=CARTESIAN_POINT('Ctrl Pts',(-10.1509405615333,14.0119382666453,2.33193995032179));
#95576=CARTESIAN_POINT('Ctrl Pts',(-10.161607551557,14.0126777724616,2.33338500128518));
#95577=CARTESIAN_POINT('Ctrl Pts',(-10.1651080690645,14.0129197649254,2.33387527155025));
#95578=CARTESIAN_POINT('Ctrl Pts',(-10.1711042591549,14.0133330466796,2.33474261859003));
#95579=CARTESIAN_POINT('Ctrl Pts',(-10.1736009802462,14.0135047600154,2.33511196566433));
#95580=CARTESIAN_POINT('Ctrl Pts',(-10.1792675158447,14.0138936266207,2.33596885561682));
#95581=CARTESIAN_POINT('Ctrl Pts',(-10.1824365385879,14.0141105020084,2.33646132108109));
#95582=CARTESIAN_POINT('Ctrl Pts',(-10.1910511306301,14.014698517306,2.33783608737362));
#95583=CARTESIAN_POINT('Ctrl Pts',(-10.1964926607555,14.0150682766817,2.33874372700941));
#95584=CARTESIAN_POINT('Ctrl Pts',(-10.2234585441452,14.0168932601214,2.34343657468214));
#95585=CARTESIAN_POINT('Ctrl Pts',(-10.2448825682992,14.0183198153569,2.34778241932385));
#95586=CARTESIAN_POINT('Ctrl Pts',(-10.2876817824523,14.0211450565449,2.35771207602066));
#95587=CARTESIAN_POINT('Ctrl Pts',(-10.3090452867247,14.0225427448135,2.36330583821056));
#95588=CARTESIAN_POINT('Ctrl Pts',(-10.4257321549664,14.030168792839,2.39739213910172));
#95589=CARTESIAN_POINT('Ctrl Pts',(-10.5173020255948,14.0361605532385,2.43727187470033));
#95590=CARTESIAN_POINT('Ctrl Pts',(-10.6264657589625,14.0443042109425,2.50230443900004));
#95591=CARTESIAN_POINT('Ctrl Pts',(-10.6496560097137,14.0460958192273,2.51724740777894));
#95592=CARTESIAN_POINT('Ctrl Pts',(-10.6792364247331,14.0484753759896,2.53781273600919));
#95593=CARTESIAN_POINT('Ctrl Pts',(-10.6861215265834,14.0490361501417,2.54271023391761));
#95594=CARTESIAN_POINT('Ctrl Pts',(-10.6973081030162,14.0499589929479,2.55085012838058));
#95595=CARTESIAN_POINT('Ctrl Pts',(-10.7016411638545,14.0503193828548,2.55404876189564));
#95596=CARTESIAN_POINT('Ctrl Pts',(-10.7099952497496,14.0510200049291,2.56030466526437));
#95597=CARTESIAN_POINT('Ctrl Pts',(-10.7140188516814,14.0513600914138,2.56335831031084));
#95598=CARTESIAN_POINT('Ctrl Pts',(-10.7232918405558,14.0521500982644,2.57049036341979));
#95599=CARTESIAN_POINT('Ctrl Pts',(-10.7285265471381,14.0526007462271,2.57458748761704));
#95600=CARTESIAN_POINT('Ctrl Pts',(-10.7454827106333,14.0540760397504,2.58809184890397));
#95601=CARTESIAN_POINT('Ctrl Pts',(-10.7570584194219,14.0551077843701,2.59767884813536));
#95602=CARTESIAN_POINT('Ctrl Pts',(-10.8303369987689,14.0618027892043,2.66077097309791));
#95603=CARTESIAN_POINT('Ctrl Pts',(-10.8865054160675,14.0677212011073,2.72034082963975));
#95604=CARTESIAN_POINT('Ctrl Pts',(-10.9690377057046,14.0777021233809,2.8284235714345));
#95605=CARTESIAN_POINT('Ctrl Pts',(-10.9989943956614,14.0817057328223,2.87385325523932));
#95606=CARTESIAN_POINT('Ctrl Pts',(-11.0336141511362,14.0867561715488,2.93520296624978));
#95607=CARTESIAN_POINT('Ctrl Pts',(-11.0412333895511,14.0878995107753,2.94937582160306));
#95608=CARTESIAN_POINT('Ctrl Pts',(-11.0534550830143,14.0897834850433,2.97327141525539));
#95609=CARTESIAN_POINT('Ctrl Pts',(-11.0582189230439,14.0905317359289,2.98290876493007));
#95610=CARTESIAN_POINT('Ctrl Pts',(-11.0646350366111,14.0915579678811,2.99634886824414));
#95611=CARTESIAN_POINT('Ctrl Pts',(-11.0664000217299,14.0918423051335,3.00009679070665));
#95612=CARTESIAN_POINT('Ctrl Pts',(-11.0693569240626,14.0923220497143,3.00646266130837));
#95613=CARTESIAN_POINT('Ctrl Pts',(-11.0705590827288,14.0925180699404,3.00907578305116));
#95614=CARTESIAN_POINT('Ctrl Pts',(-11.0728481225529,14.0928931663177,3.01409984371837));
#95615=CARTESIAN_POINT('Ctrl Pts',(-11.0739364681581,14.0930723350003,3.01651006354552));
#95616=CARTESIAN_POINT('Ctrl Pts',(-11.0765286456436,14.0935011159065,3.02230256587238));
#95617=CARTESIAN_POINT('Ctrl Pts',(-11.0780246806979,14.093750261528,3.02568833854362));
#95618=CARTESIAN_POINT('Ctrl Pts',(-11.0834105133549,14.0946535881988,3.03803448298171));
#95619=CARTESIAN_POINT('Ctrl Pts',(-11.0872048919799,14.0953023423085,3.04703640595085));
#95620=CARTESIAN_POINT('Ctrl Pts',(-11.1136900810083,14.0999294657895,3.11212170010008));
#95621=CARTESIAN_POINT('Ctrl Pts',(-11.1321446621535,14.1036988020779,3.1698400850009));
#95622=CARTESIAN_POINT('Ctrl Pts',(-11.1581037221486,14.1106773611151,3.2795130995613));
#95623=CARTESIAN_POINT('Ctrl Pts',(-11.166735159857,14.1138847214632,3.33103972618087));
#95624=CARTESIAN_POINT('Ctrl Pts',(-11.1751092255998,14.119174579023,3.41489498456272));
#95625=CARTESIAN_POINT('Ctrl Pts',(-11.1769913383375,14.1212115022148,3.4469367533419));
#95626=CARTESIAN_POINT('Ctrl Pts',(-11.1779381857702,14.1246459503731,3.50006529730578));
#95627=CARTESIAN_POINT('Ctrl Pts',(-11.1777487610663,14.1260218330418,3.52112204678003));
#95628=CARTESIAN_POINT('Ctrl Pts',(-11.1767208575517,14.1279220686643,3.54981742425372));
#95629=CARTESIAN_POINT('Ctrl Pts',(-11.1763719213343,14.1284312981153,3.55747043081901));
#95630=CARTESIAN_POINT('Ctrl Pts',(-11.1756598487533,14.1292912679029,3.5703292923863));
#95631=CARTESIAN_POINT('Ctrl Pts',(-11.1753367261083,14.1296407590123,3.57553719681896));
#95632=CARTESIAN_POINT('Ctrl Pts',(-11.1746299796621,14.1303333882333,3.58582186804063));
#95633=CARTESIAN_POINT('Ctrl Pts',(-11.1742480225125,14.1306764671015,3.59089863791457));
#95634=CARTESIAN_POINT('Ctrl Pts',(-11.1732398049759,14.131512748283,3.6032300523452));
#95635=CARTESIAN_POINT('Ctrl Pts',(-11.1725791642262,14.1320070096822,3.61048159650023));
#95636=CARTESIAN_POINT('Ctrl Pts',(-11.1705118774866,14.1334168620048,3.63105941542356));
#95637=CARTESIAN_POINT('Ctrl Pts',(-11.1689450178714,14.1343373821485,3.64436808903332));
#95638=CARTESIAN_POINT('Ctrl Pts',(-11.1556729142305,14.1412007155932,3.74262931842275));
#95639=CARTESIAN_POINT('Ctrl Pts',(-11.1349492511425,14.147429627284,3.82608861520466));
#95640=CARTESIAN_POINT('Ctrl Pts',(-11.0806119755649,14.1589875392999,3.97382739129924));
#95641=CARTESIAN_POINT('Ctrl Pts',(-11.0497708035041,14.1642648947757,4.03871895862753));
#95642=CARTESIAN_POINT('Ctrl Pts',(-11.0095366195933,14.1697587935403,4.10661598469172));
#95643=CARTESIAN_POINT('Ctrl Pts',(-11.0058006477705,14.170258040153,4.11279050471137));
#95644=CARTESIAN_POINT('Ctrl Pts',(-11.0001527490662,14.1709963651452,4.12193408392853));
#95645=CARTESIAN_POINT('Ctrl Pts',(-10.9982839292167,14.1712380689487,4.12492937497591));
#95646=CARTESIAN_POINT('Ctrl Pts',(-10.9950568967927,14.1716509532859,4.13005015391677));
#95647=CARTESIAN_POINT('Ctrl Pts',(-10.993705297902,14.1718225564764,4.13217972576435));
#95648=CARTESIAN_POINT('Ctrl Pts',(-10.9906194604626,14.1722113338039,4.13700740484274));
#95649=CARTESIAN_POINT('Ctrl Pts',(-10.9888810358292,14.1724282292428,4.13970278010215));
#95650=CARTESIAN_POINT('Ctrl Pts',(-10.9841213206592,14.17301643108,4.14701680658657));
#95651=CARTESIAN_POINT('Ctrl Pts',(-10.981078494559,14.1733863550082,4.15162144859135));
#95652=CARTESIAN_POINT('Ctrl Pts',(-10.9658070460457,14.1752138471674,4.17438192095784));
#95653=CARTESIAN_POINT('Ctrl Pts',(-10.9531053974664,14.1766426458147,4.19221707235233));
#95654=CARTESIAN_POINT('Ctrl Pts',(-10.9266128776836,14.179469584075,4.22730379330148));
#95655=CARTESIAN_POINT('Ctrl Pts',(-10.9128195366583,14.1808668063854,4.24454202275886));
#95656=CARTESIAN_POINT('Ctrl Pts',(-10.8342482834542,14.1884909664596,4.33726817824236));
#95657=CARTESIAN_POINT('Ctrl Pts',(-10.7605964704871,14.1944815888736,4.40469978321671));
#95658=CARTESIAN_POINT('Ctrl Pts',(-10.6568112680421,14.202624201462,4.47798514697378));
#95659=CARTESIAN_POINT('Ctrl Pts',(-10.6337273943094,14.2044160455217,4.49309888129395));
#95660=CARTESIAN_POINT('Ctrl Pts',(-10.6029080403816,14.2067958883378,4.51176497156991));
#95661=CARTESIAN_POINT('Ctrl Pts',(-10.5956337094675,14.2073567045455,4.51606443733364));
#95662=CARTESIAN_POINT('Ctrl Pts',(-10.583647911618,14.2082796093998,4.52297565363541));
#95663=CARTESIAN_POINT('Ctrl Pts',(-10.5789635900421,14.2086400190183,4.52563406360709));
#95664=CARTESIAN_POINT('Ctrl Pts',(-10.5698510433297,14.2093406745037,4.53072322540899));
#95665=CARTESIAN_POINT('Ctrl Pts',(-10.5654250828965,14.2096807746465,4.5331578065533));
#95666=CARTESIAN_POINT('Ctrl Pts',(-10.5551385670223,14.2104708065821,4.5387301983694));
#95667=CARTESIAN_POINT('Ctrl Pts',(-10.5492668807946,14.2109214659424,4.54184698689971));
#95668=CARTESIAN_POINT('Ctrl Pts',(-10.5300348161396,14.2123967732912,4.55184791868687));
#95669=CARTESIAN_POINT('Ctrl Pts',(-10.516569462522,14.2134285197689,4.55852581659148));
#95670=CARTESIAN_POINT('Ctrl Pts',(-10.4292371402673,14.220115589636,4.59977348770738));
#95671=CARTESIAN_POINT('Ctrl Pts',(-10.3520888121434,14.2260252485267,4.62684298723955));
#95672=CARTESIAN_POINT('Ctrl Pts',(-10.2198556405815,14.2360011851153,4.65832560628215));
#95673=CARTESIAN_POINT('Ctrl Pts',(-10.1661203530108,14.2400086752141,4.667244325078));
#95674=CARTESIAN_POINT('Ctrl Pts',(-10.0959347546297,14.2450634897697,4.67394663301471));
#95675=CARTESIAN_POINT('Ctrl Pts',(-10.0798801462141,14.2462074282894,4.67514824222193));
#95676=CARTESIAN_POINT('Ctrl Pts',(-10.0530670054817,14.248092303797,4.67660299268477));
#95677=CARTESIAN_POINT('Ctrl Pts',(-10.0423209096188,14.2488408627486,4.67703851706378));
#95678=CARTESIAN_POINT('Ctrl Pts',(-10.0274276409572,14.2498674756354,4.67743787843442));
#95679=CARTESIAN_POINT('Ctrl Pts',(-10.0232847556705,14.2501518895618,4.67752709290414));
#95680=CARTESIAN_POINT('Ctrl Pts',(-10.016264866399,14.2506317508259,4.6776411988785));
#95681=CARTESIAN_POINT('Ctrl Pts',(-10.0133881094558,14.2508278113248,4.67767741694235));
#95682=CARTESIAN_POINT('Ctrl Pts',(-10.0078664196317,14.2512029717302,4.67772669889318));
#95683=CARTESIAN_POINT('Ctrl Pts',(-10.0052215484168,14.2513821642553,4.67774139505611));
#95684=CARTESIAN_POINT('Ctrl Pts',(-9.99887473123479,14.2518109961491,4.67775528030774));
#95685=CARTESIAN_POINT('Ctrl Pts',(-9.99517276563141,14.2520601689187,4.67774592559472));
#95686=CARTESIAN_POINT('Ctrl Pts',(-9.98170264885298,14.2529635409298,4.67764837369698));
#95687=CARTESIAN_POINT('Ctrl Pts',(-9.97193531930477,14.2536123140564,4.67745610285185));
#95688=CARTESIAN_POINT('Ctrl Pts',(-9.90170261206705,14.2582395178387,4.67519909089871));
#95689=CARTESIAN_POINT('Ctrl Pts',(-9.8414653117913,14.2620089485544,4.66859914659879));
#95690=CARTESIAN_POINT('Ctrl Pts',(-9.73070380691363,14.268987971793,4.64773637442113));
#95691=CARTESIAN_POINT('Ctrl Pts',(-9.68011268705498,14.2721956942608,4.63467666516678));
#95692=CARTESIAN_POINT('Ctrl Pts',(-9.60009646774952,14.2774854886338,4.6082424032536));
#95693=CARTESIAN_POINT('Ctrl Pts',(-9.57006338673536,14.2795219586975,4.59694044102107));
#95694=CARTESIAN_POINT('Ctrl Pts',(-9.52114698590922,14.2829557383333,4.57621467551545));
#95695=CARTESIAN_POINT('Ctrl Pts',(-9.50198810591725,14.2843314211539,4.56748409898914));
#95696=CARTESIAN_POINT('Ctrl Pts',(-9.47619068453028,14.2862314603736,4.55488272108867));
#95697=CARTESIAN_POINT('Ctrl Pts',(-9.46934010158477,14.2867407005199,4.55145319525144));
#95698=CARTESIAN_POINT('Ctrl Pts',(-9.4578802740995,14.2876007144442,4.5455756773821));
#95699=CARTESIAN_POINT('Ctrl Pts',(-9.45325289484323,14.287950239259,4.54316340802868));
#95700=CARTESIAN_POINT('Ctrl Pts',(-9.44414228403918,14.2886429562213,4.53833674196264));
#95701=CARTESIAN_POINT('Ctrl Pts',(-9.43965837403794,14.2889860892448,4.53592386347199));
#95702=CARTESIAN_POINT('Ctrl Pts',(-9.42879922859871,14.2898225403397,4.52998921685848));
#95703=CARTESIAN_POINT('Ctrl Pts',(-9.42244081052756,14.2903169180181,4.52643727845557));
#95704=CARTESIAN_POINT('Ctrl Pts',(-9.40447443733385,14.2917272053611,4.51618111227948));
#95705=CARTESIAN_POINT('Ctrl Pts',(-9.39294774915114,14.2926480475002,4.50933754893369));
#95706=CARTESIAN_POINT('Ctrl Pts',(-9.3086497098293,14.2995045737172,4.45732223127635));
#95707=CARTESIAN_POINT('Ctrl Pts',(-9.2408957002926,14.3057255541152,4.4045366082221));
#95708=CARTESIAN_POINT('Ctrl Pts',(-9.12797791106919,14.3172825909929,4.29487457317117));
#95709=CARTESIAN_POINT('Ctrl Pts',(-9.08115606939346,14.3225671590039,4.24025412018268));
#95710=CARTESIAN_POINT('Ctrl Pts',(-9.03541931818327,14.3280676499016,4.17581895354549));
#95711=CARTESIAN_POINT('Ctrl Pts',(-9.03129594819529,14.3285669474665,4.16989522782331));
#95712=CARTESIAN_POINT('Ctrl Pts',(-9.02523676292711,14.3293053488152,4.16101751904551));
#95713=CARTESIAN_POINT('Ctrl Pts',(-9.02325945089602,14.3295470782624,4.15809226510691));
#95714=CARTESIAN_POINT('Ctrl Pts',(-9.01989213304503,14.3299599976533,4.15306201399799));
#95715=CARTESIAN_POINT('Ctrl Pts',(-9.01849570534121,14.3301316104022,4.15096140054772));
#95716=CARTESIAN_POINT('Ctrl Pts',(-9.01533907458191,14.3305203884803,4.14617970440153));
#95717=CARTESIAN_POINT('Ctrl Pts',(-9.01358306741671,14.3307372752179,4.1434959084252));
#95718=CARTESIAN_POINT('Ctrl Pts',(-9.00883527110182,14.3313254569691,4.13617450439704));
#95719=CARTESIAN_POINT('Ctrl Pts',(-9.00586503392264,14.331695369507,4.13152291490327));
#95720=CARTESIAN_POINT('Ctrl Pts',(-8.99127689375568,14.3335228418838,4.10831892481742));
#95721=CARTESIAN_POINT('Ctrl Pts',(-8.98014424647803,14.3349516307007,4.08946468071107));
#95722=CARTESIAN_POINT('Ctrl Pts',(-8.95885477731884,14.3377785585864,4.05099805787925));
#95723=CARTESIAN_POINT('Ctrl Pts',(-8.94871115641225,14.3391757799869,4.0313888399015));
#95724=CARTESIAN_POINT('Ctrl Pts',(-8.89593019320576,14.3467993358334,3.92191967356889));
#95725=CARTESIAN_POINT('Ctrl Pts',(-8.86425836478119,14.3527893819415,3.82722740622177));
#95726=CARTESIAN_POINT('Ctrl Pts',(-8.83948194661727,14.3609317004653,3.70261829754677));
#95727=CARTESIAN_POINT('Ctrl Pts',(-8.83505423995319,14.3627239268073,3.67537819574988));
#95728=CARTESIAN_POINT('Ctrl Pts',(-8.83052534360589,14.365104179563,3.63962626733462));
#95729=CARTESIAN_POINT('Ctrl Pts',(-8.8295536848012,14.3656650084218,3.63123217414234));
#95730=CARTESIAN_POINT('Ctrl Pts',(-8.82811076054309,14.3665879087885,3.61747204103559));
#95731=CARTESIAN_POINT('Ctrl Pts',(-8.82758582238143,14.3669483009046,3.61211183906176));
#95732=CARTESIAN_POINT('Ctrl Pts',(-8.8266398769313,14.3676489038822,3.6017182157676));
#95733=CARTESIAN_POINT('Ctrl Pts',(-8.82621444727896,14.3679889689138,3.59668530746457));
#95734=CARTESIAN_POINT('Ctrl Pts',(-8.82530418990082,14.3687788914421,3.58502348461544));
#95735=CARTESIAN_POINT('Ctrl Pts',(-8.82484308190171,14.3692294762038,3.57839294545722));
#95736=CARTESIAN_POINT('Ctrl Pts',(-8.82352265841797,14.3707044110595,3.55676165121913));
#95737=CARTESIAN_POINT('Ctrl Pts',(-8.82289430376089,14.3717358557591,3.54174881853642));
#95738=CARTESIAN_POINT('Ctrl Pts',(-8.82069852831664,14.3784346367233,3.44502086357339));
#95739=CARTESIAN_POINT('Ctrl Pts',(-8.82735400030145,14.3843575378299,3.36335666573198));
#95740=CARTESIAN_POINT('Ctrl Pts',(-8.85240249491681,14.3943377502013,3.22970095472508));
#95741=CARTESIAN_POINT('Ctrl Pts',(-8.86607848956628,14.3983361495799,3.17710034152597));
#95742=CARTESIAN_POINT('Ctrl Pts',(-8.88844526655302,14.4033807550033,3.11038530247083));
#95743=CARTESIAN_POINT('Ctrl Pts',(-8.89386758271315,14.4045232570814,3.09524739916394));
#95744=CARTESIAN_POINT('Ctrl Pts',(-8.90342779610554,14.4064060080679,3.07018620823077));
#95745=CARTESIAN_POINT('Ctrl Pts',(-8.90739450844109,14.4071538597087,3.06020032481886));
#95746=CARTESIAN_POINT('Ctrl Pts',(-8.91307911525705,14.4081796526779,3.04644161511211));
#95747=CARTESIAN_POINT('Ctrl Pts',(-8.91468095229681,14.4084639422263,3.04262183677734));
#95748=CARTESIAN_POINT('Ctrl Pts',(-8.91742928129862,14.4089436416149,3.03616384896349));
#95749=CARTESIAN_POINT('Ctrl Pts',(-8.91856533801684,14.4091396638902,3.03352126678986));
#95750=CARTESIAN_POINT('Ctrl Pts',(-8.92076468430593,14.409514802616,3.02845658470013));
#95751=CARTESIAN_POINT('Ctrl Pts',(-8.92182646257291,14.4096940113884,3.02603388022038));
#95752=CARTESIAN_POINT('Ctrl Pts',(-8.92439419035087,14.4101229275648,3.02022826643694));
#95753=CARTESIAN_POINT('Ctrl Pts',(-8.92590796121905,14.4103721679381,3.01684881534942));
#95754=CARTESIAN_POINT('Ctrl Pts',(-8.93147651334137,14.4112761778437,3.00457269863229));
#95755=CARTESIAN_POINT('Ctrl Pts',(-8.9356262332478,14.4119255107363,2.99571917299419));
#95756=CARTESIAN_POINT('Ctrl Pts',(-8.96616586049697,14.4165416240331,2.93261914276511));
#95757=CARTESIAN_POINT('Ctrl Pts',(-8.99658243553144,14.4203006873666,2.88041209228893));
#95758=CARTESIAN_POINT('Ctrl Pts',(-9.06035263249913,14.4272500283245,2.78806606760435));
#95759=CARTESIAN_POINT('Ctrl Pts',(-9.09262364128079,14.4304387260986,2.7473679155282));
#95760=CARTESIAN_POINT('Ctrl Pts',(-9.14921582110835,14.4357257867934,2.68494829616653));
#95761=CARTESIAN_POINT('Ctrl Pts',(-9.17193737867348,14.437780201694,2.66187408347965));
#95762=CARTESIAN_POINT('Ctrl Pts',(-9.2059889899222,14.4407929008442,2.63003178162712));
#95763=CARTESIAN_POINT('Ctrl Pts',(-9.21657426661279,14.441720786512,2.62048747683075));
#95764=CARTESIAN_POINT('Ctrl Pts',(-9.23588409826136,14.4434004412192,2.60370182259106));
#95765=CARTESIAN_POINT('Ctrl Pts',(-9.2445450514665,14.4441492933545,2.59638982952307));
#95766=CARTESIAN_POINT('Ctrl Pts',(-9.2579561617186,14.4453028176267,2.58539511215086));
#95767=CARTESIAN_POINT('Ctrl Pts',(-9.26263138094728,14.4457038473326,2.58162171400793));
#95768=CARTESIAN_POINT('Ctrl Pts',(-9.27118911851519,14.4464360423981,2.5748221841838));
#95769=CARTESIAN_POINT('Ctrl Pts',(-9.27506215064433,14.4467667314772,2.57178428953339));
#95770=CARTESIAN_POINT('Ctrl Pts',(-9.28354691567197,14.4474897629631,2.56521457998554));
#95771=CARTESIAN_POINT('Ctrl Pts',(-9.28816594199024,14.4478824727722,2.5616924410005));
#95772=CARTESIAN_POINT('Ctrl Pts',(-9.30089711404038,14.4489625415048,2.55213266983955));
#95773=CARTESIAN_POINT('Ctrl Pts',(-9.30906110376885,14.4496525812715,2.54616523899348));
#95774=CARTESIAN_POINT('Ctrl Pts',(-9.35412532739765,14.4534486071042,2.51410789136402));
#95775=CARTESIAN_POINT('Ctrl Pts',(-9.39242242888004,14.4566300549821,2.49005647991694));
#95776=CARTESIAN_POINT('Ctrl Pts',(-9.50430495861425,14.4658014963135,2.42846204853772));
#95777=CARTESIAN_POINT('Ctrl Pts',(-9.5805894708448,14.471929999649,2.39636962951048));
#95778=CARTESIAN_POINT('Ctrl Pts',(-9.68468909199254,14.4798355932033,2.3649398952871));
#95779=CARTESIAN_POINT('Ctrl Pts',(-9.71003520052362,14.4817245372623,2.35820185277116));
#95780=CARTESIAN_POINT('Ctrl Pts',(-9.74557920676294,14.4843066413364,2.35001292473762));
#95781=CARTESIAN_POINT('Ctrl Pts',(-9.75560177731054,14.4850274220478,2.34784127037439));
#95782=CARTESIAN_POINT('Ctrl Pts',(-9.77312777195125,14.4862736728282,2.34428279898195));
#95783=CARTESIAN_POINT('Ctrl Pts',(-9.78061855489875,14.4868018559942,2.34283750241962));
#95784=CARTESIAN_POINT('Ctrl Pts',(-9.79167502191317,14.4875743620624,2.34081545724837));
#95785=CARTESIAN_POINT('Ctrl Pts',(-9.79522997733308,14.4878216665144,2.34018219562515));
#95786=CARTESIAN_POINT('Ctrl Pts',(-9.80151767638914,14.4882571084843,2.33909194777495));
#95787=CARTESIAN_POINT('Ctrl Pts',(-9.80424917933254,14.4884456145673,2.33862824414529));
#95788=CARTESIAN_POINT('Ctrl Pts',(-9.80835586790926,14.4887280279149,2.33794598763162));
#95789=CARTESIAN_POINT('Ctrl Pts',(-9.80972976349543,14.4888223435607,2.33772024100504));
#95790=CARTESIAN_POINT('Ctrl Pts',(-9.81110406371064,14.4889165240206,2.33749693000261));
#95791=CARTESIAN_POINT('Origin',(-10.,12.3756328852638,3.5));
#95792=CARTESIAN_POINT('',(-9.81110406371068,15.0871826612189,2.3374969300026));
#95793=CARTESIAN_POINT('',(-9.81110406371068,14.9873061497326,2.3374969300026));
#95794=CARTESIAN_POINT('',(-9.81110406371068,12.3756328852638,2.3374969300026));
#95795=CARTESIAN_POINT('Ctrl Pts',(-9.81110406371068,15.0871826612189,2.3374969300026));
#95796=CARTESIAN_POINT('Ctrl Pts',(-9.79515642301048,15.086163901984,2.3400882732854));
#95797=CARTESIAN_POINT('Ctrl Pts',(-9.77925508557964,15.0851380650591,2.34300891814498));
#95798=CARTESIAN_POINT('Ctrl Pts',(-9.73492997612474,15.0822433730758,2.35209835980764));
#95799=CARTESIAN_POINT('Ctrl Pts',(-9.70667787143568,15.0803573243553,2.35899070974895));
#95800=CARTESIAN_POINT('Ctrl Pts',(-9.67043288027128,15.0778698994534,2.36926810425282));
#95801=CARTESIAN_POINT('Ctrl Pts',(-9.66218053588176,15.0772989562322,2.37170610672386));
#95802=CARTESIAN_POINT('Ctrl Pts',(-9.64877427818331,15.0763635739621,2.37582699727071));
#95803=CARTESIAN_POINT('Ctrl Pts',(-9.64360386412048,15.0760009032648,2.37745546173498));
#95804=CARTESIAN_POINT('Ctrl Pts',(-9.63364852141444,15.0752988008422,2.3806666912685));
#95805=CARTESIAN_POINT('Ctrl Pts',(-9.62886213944729,15.0749595342949,2.38224459339228));
#95806=CARTESIAN_POINT('Ctrl Pts',(-9.61786078480123,15.0741757290523,2.38594980670179));
#95807=CARTESIAN_POINT('Ctrl Pts',(-9.61165323633449,15.0737304990385,2.38809847509248));
#95808=CARTESIAN_POINT('Ctrl Pts',(-9.5917276463968,15.0722915898774,2.3951826897708));
#95809=CARTESIAN_POINT('Ctrl Pts',(-9.57808362769048,15.0712912911195,2.40032088986485));
#95810=CARTESIAN_POINT('Ctrl Pts',(-9.47990134218978,15.0639804426116,2.43939150843279));
#95811=CARTESIAN_POINT('Ctrl Pts',(-9.3994725387176,15.0573441213353,2.48277165602932));
#95812=CARTESIAN_POINT('Ctrl Pts',(-9.2694598080945,15.0456926755982,2.57372921502584));
#95813=CARTESIAN_POINT('Ctrl Pts',(-9.2174929237763,15.0407320728207,2.61719122026143));
#95814=CARTESIAN_POINT('Ctrl Pts',(-9.16478291082366,15.0355647769559,2.66960704415242));
#95815=CARTESIAN_POINT('Ctrl Pts',(-9.16006739343266,15.0351012581966,2.67437704193263));
#95816=CARTESIAN_POINT('Ctrl Pts',(-9.15300305419007,15.0344053202665,2.6816461685585));
#95817=CARTESIAN_POINT('Ctrl Pts',(-9.15062407321736,15.0341706885431,2.68411559923894));
#95818=CARTESIAN_POINT('Ctrl Pts',(-9.14651984857847,15.0337654900398,2.6884132751252));
#95819=CARTESIAN_POINT('Ctrl Pts',(-9.14478965157078,15.0335945477369,2.69023667582861));
#95820=CARTESIAN_POINT('Ctrl Pts',(-9.14081082490376,15.0332011546344,2.69445681434044));
#95821=CARTESIAN_POINT('Ctrl Pts',(-9.13856638147964,15.032979021896,2.69685743226108));
#95822=CARTESIAN_POINT('Ctrl Pts',(-9.13234608103675,15.032362672994,2.70356663193275));
#95823=CARTESIAN_POINT('Ctrl Pts',(-9.12839223458599,15.0319700666775,2.7078956257733));
#95824=CARTESIAN_POINT('Ctrl Pts',(-9.10666602591954,15.0298068467001,2.73204291737873));
#95825=CARTESIAN_POINT('Ctrl Pts',(-9.0895356739129,15.028079171243,2.75243151858018));
#95826=CARTESIAN_POINT('Ctrl Pts',(-9.01086387259382,15.0199379171547,2.85278745603675));
#95827=CARTESIAN_POINT('Ctrl Pts',(-8.9590757653736,15.0138973467825,2.93986233630128));
#95828=CARTESIAN_POINT('Ctrl Pts',(-8.90285572880089,15.004947601507,3.06985178960889));
#95829=CARTESIAN_POINT('Ctrl Pts',(-8.88864274116309,15.0023313389695,3.10803377493285));
#95830=CARTESIAN_POINT('Ctrl Pts',(-8.87356934886499,14.9990191740848,3.15599350390052));
#95831=CARTESIAN_POINT('Ctrl Pts',(-8.87081380929607,14.998385799955,3.16514925862222));
#95832=CARTESIAN_POINT('Ctrl Pts',(-8.86661330892795,14.9973737413982,3.17974795932868));
#95833=CARTESIAN_POINT('Ctrl Pts',(-8.86509534370761,14.9969974173279,3.18516960072175));
#95834=CARTESIAN_POINT('Ctrl Pts',(-8.86230588049519,14.9962852939782,3.19541497652682));
#95835=CARTESIAN_POINT('Ctrl Pts',(-8.86102603857296,14.995949771631,3.20023632649516));
#95836=CARTESIAN_POINT('Ctrl Pts',(-8.85820530041689,14.9951898938875,3.21114136449993));
#95837=CARTESIAN_POINT('Ctrl Pts',(-8.8566823347847,14.994764974924,3.21722949047381));
#95838=CARTESIAN_POINT('Ctrl Pts',(-8.85289074525709,14.9936680825427,3.23291811381712));
#95839=CARTESIAN_POINT('Ctrl Pts',(-8.85069399348628,14.992993848856,3.24253530471152));
#95840=CARTESIAN_POINT('Ctrl Pts',(-8.83263750569812,14.987095227857,3.3264260314709));
#95841=CARTESIAN_POINT('Ctrl Pts',(-8.8238787719305,14.9816440419769,3.40203080089322));
#95842=CARTESIAN_POINT('Ctrl Pts',(-8.82143546749479,14.9720997059448,3.53244505879391));
#95843=CARTESIAN_POINT('Ctrl Pts',(-8.8241999708502,14.9680731150544,3.58695672538426));
#95844=CARTESIAN_POINT('Ctrl Pts',(-8.833553584781,14.9624127024092,3.66447865739957));
#95845=CARTESIAN_POINT('Ctrl Pts',(-8.83707848897994,14.9607200427715,3.68778756764681));
#95846=CARTESIAN_POINT('Ctrl Pts',(-8.8430107503973,14.9583801437462,3.7203680233814));
#95847=CARTESIAN_POINT('Ctrl Pts',(-8.84483496536203,14.9577102092966,3.72973886364951));
#95848=CARTESIAN_POINT('Ctrl Pts',(-8.84823775873616,14.9565433731508,3.74615211986347));
#95849=CARTESIAN_POINT('Ctrl Pts',(-8.84976747950936,14.9560441886145,3.75320403206441));
#95850=CARTESIAN_POINT('Ctrl Pts',(-8.85214223665456,14.9553058688401,3.76368558376098));
#95851=CARTESIAN_POINT('Ctrl Pts',(-8.85293800895049,14.955064109725,3.76712604041762));
#95852=CARTESIAN_POINT('Ctrl Pts',(-8.8543289137695,14.9546511048689,3.773018664837));
#95853=CARTESIAN_POINT('Ctrl Pts',(-8.85491646419467,14.9544794364198,3.77547254971057));
#95854=CARTESIAN_POINT('Ctrl Pts',(-8.85626917212068,14.954090479467,3.78104297456336));
#95855=CARTESIAN_POINT('Ctrl Pts',(-8.85703918324864,14.9538734700838,3.78415828720341));
#95856=CARTESIAN_POINT('Ctrl Pts',(-8.85916925416681,14.9532848366537,3.79262738035619));
#95857=CARTESIAN_POINT('Ctrl Pts',(-8.86055428177709,14.9529145979175,3.79797488580829));
#95858=CARTESIAN_POINT('Ctrl Pts',(-8.86762568667007,14.951083873887,3.82450666385443));
#95859=CARTESIAN_POINT('Ctrl Pts',(-8.8738658668647,14.9496522769765,3.8455404807236));
#95860=CARTESIAN_POINT('Ctrl Pts',(-8.88755421287155,14.9468232500441,3.88735801601474));
#95861=CARTESIAN_POINT('Ctrl Pts',(-8.89500624158797,14.9454266357613,3.90813080358829));
#95862=CARTESIAN_POINT('Ctrl Pts',(-8.93930142230548,14.9377929389679,4.02147830061559));
#95863=CARTESIAN_POINT('Ctrl Pts',(-8.98719089542334,14.9317925662774,4.10929409034255));
#95864=CARTESIAN_POINT('Ctrl Pts',(-9.06162314088735,14.9236489446797,4.21224657555268));
#95865=CARTESIAN_POINT('Ctrl Pts',(-9.07845121220709,14.921868263407,4.23388960888349));
#95866=CARTESIAN_POINT('Ctrl Pts',(-9.10142305284339,14.9195010855006,4.26139716372696));
#95867=CARTESIAN_POINT('Ctrl Pts',(-9.1068974794257,14.9189413996988,4.26781120888467));
#95868=CARTESIAN_POINT('Ctrl Pts',(-9.11597880088583,14.918019813943,4.27822269455469));
#95869=CARTESIAN_POINT('Ctrl Pts',(-9.11954513056321,14.9176595828078,4.28225524226391));
#95870=CARTESIAN_POINT('Ctrl Pts',(-9.12651336288774,14.9169588856068,4.29002639585914));
#95871=CARTESIAN_POINT('Ctrl Pts',(-9.12991193966858,14.916618562821,4.29376783587075));
#95872=CARTESIAN_POINT('Ctrl Pts',(-9.13784436342581,14.915827437928,4.30238836057797));
#95873=CARTESIAN_POINT('Ctrl Pts',(-9.14239568800388,14.9153759028332,4.30725105372781));
#95874=CARTESIAN_POINT('Ctrl Pts',(-9.15739683132253,14.9138951531157,4.32300841541441));
#95875=CARTESIAN_POINT('Ctrl Pts',(-9.16801453891312,14.9128587681617,4.33374043166603));
#95876=CARTESIAN_POINT('Ctrl Pts',(-9.23063595178446,14.9068098215102,4.39464844342418));
#95877=CARTESIAN_POINT('Ctrl Pts',(-9.2869547928158,14.9016022255556,4.44014898235957));
#95878=CARTESIAN_POINT('Ctrl Pts',(-9.39845520858646,14.8917900714712,4.51442098560932));
#95879=CARTESIAN_POINT('Ctrl Pts',(-9.45244614392866,14.8872265215785,4.54455317484718));
#95880=CARTESIAN_POINT('Ctrl Pts',(-9.52420053704212,14.8815545142569,4.57750009150391));
#95881=CARTESIAN_POINT('Ctrl Pts',(-9.54000591131022,14.8803285958587,4.58434177253366));
#95882=CARTESIAN_POINT('Ctrl Pts',(-9.5664273085294,14.8783239245719,4.59509706862887));
#95883=CARTESIAN_POINT('Ctrl Pts',(-9.57695946965197,14.8775363382036,4.59920862529774));
#95884=CARTESIAN_POINT('Ctrl Pts',(-9.59150822018195,14.8764656743147,4.60464808369285));
#95885=CARTESIAN_POINT('Ctrl Pts',(-9.59547477636411,14.8761755178754,4.60610680669362));
#95886=CARTESIAN_POINT('Ctrl Pts',(-9.602170366465,14.8756887714325,4.6085283120383));
#95887=CARTESIAN_POINT('Ctrl Pts',(-9.60489522542583,14.8754915282382,4.6095024351739));
#95888=CARTESIAN_POINT('Ctrl Pts',(-9.61010207160125,14.8751162683432,4.61134224122461));
#95889=CARTESIAN_POINT('Ctrl Pts',(-9.61258339793891,14.8749381462774,4.61220966930437));
#95890=CARTESIAN_POINT('Ctrl Pts',(-9.61850538934226,14.8745146755478,4.61425767042309));
#95891=CARTESIAN_POINT('Ctrl Pts',(-9.62194868648402,14.8742697672294,4.61543063400866));
#95892=CARTESIAN_POINT('Ctrl Pts',(-9.6342298585833,14.8734007465502,4.61955082894055));
#95893=CARTESIAN_POINT('Ctrl Pts',(-9.64309748662113,14.8727815287675,4.62240922316525));
#95894=CARTESIAN_POINT('Ctrl Pts',(-9.72462454454528,14.8671558968509,4.64762473748706));
#95895=CARTESIAN_POINT('Ctrl Pts',(-9.79926601994208,14.8624854762799,4.66300621121937));
#95896=CARTESIAN_POINT('Ctrl Pts',(-9.95809474724053,14.8526108967361,4.67997584784296));
#95897=CARTESIAN_POINT('Ctrl Pts',(-10.04200932194,14.8474183703074,4.67997104891288));
#95898=CARTESIAN_POINT('Ctrl Pts',(-10.1363867317225,14.8411862355522,4.66988037047647));
#95899=CARTESIAN_POINT('Ctrl Pts',(-10.1475459805805,14.8404434683745,4.66852539173069));
#95900=CARTESIAN_POINT('Ctrl Pts',(-10.1646189485755,14.8392972973858,4.66620390213083));
#95901=CARTESIAN_POINT('Ctrl Pts',(-10.1705477420818,14.838897461752,4.66535162290304));
#95902=CARTESIAN_POINT('Ctrl Pts',(-10.181337350597,14.8381663906088,4.6637164887199));
#95903=CARTESIAN_POINT('Ctrl Pts',(-10.1862002780894,14.8378356223811,4.66294830324269));
#95904=CARTESIAN_POINT('Ctrl Pts',(-10.1968094614368,14.8371111572974,4.66120414638569));
#95905=CARTESIAN_POINT('Ctrl Pts',(-10.2025535497538,14.8367170843323,4.66021596742087));
#95906=CARTESIAN_POINT('Ctrl Pts',(-10.2183238428585,14.8356300080596,4.65738225803243));
#95907=CARTESIAN_POINT('Ctrl Pts',(-10.2283335899786,14.8349342675502,4.65544915589988));
#95908=CARTESIAN_POINT('Ctrl Pts',(-10.2841024986952,14.8310247604404,4.64392598990509));
#95909=CARTESIAN_POINT('Ctrl Pts',(-10.3292783006312,14.8277299586301,4.63174894848617));
#95910=CARTESIAN_POINT('Ctrl Pts',(-10.476822735941,14.8165426094329,4.58239586390702));
#95911=CARTESIAN_POINT('Ctrl Pts',(-10.5747448547489,14.8083573658706,4.53373434003219));
#95912=CARTESIAN_POINT('Ctrl Pts',(-10.6723249607545,14.8000100018984,4.46703774132654));
#95913=CARTESIAN_POINT('Ctrl Pts',(-10.6799969562568,14.7993527401163,4.46165846229797));
#95914=CARTESIAN_POINT('Ctrl Pts',(-10.6933774718435,14.7982058108819,4.45203640185931));
#95915=CARTESIAN_POINT('Ctrl Pts',(-10.6991131966574,14.7977139621432,4.44783246064298));
#95916=CARTESIAN_POINT('Ctrl Pts',(-10.7076231564636,14.7969843345878,4.44147589157585));
#95917=CARTESIAN_POINT('Ctrl Pts',(-10.710426284981,14.7967440190397,4.43936248615759));
#95918=CARTESIAN_POINT('Ctrl Pts',(-10.71522611727,14.7963326163181,4.43570990106464));
#95919=CARTESIAN_POINT('Ctrl Pts',(-10.7172273669088,14.7961611159705,4.43417681536315));
#95920=CARTESIAN_POINT('Ctrl Pts',(-10.721776311964,14.7957713641499,4.43066879635044));
#95921=CARTESIAN_POINT('Ctrl Pts',(-10.7243208313539,14.7955533991702,4.42868982276645));
#95922=CARTESIAN_POINT('Ctrl Pts',(-10.7312529820739,14.7949596205046,4.42325259202769));
#95923=CARTESIAN_POINT('Ctrl Pts',(-10.7356242528647,14.7945852326823,4.41977346893174));
#95924=CARTESIAN_POINT('Ctrl Pts',(-10.7576336585479,14.7926994121515,4.40199875750753));
#95925=CARTESIAN_POINT('Ctrl Pts',(-10.7748818732901,14.7912189859528,4.38722531843091));
#95926=CARTESIAN_POINT('Ctrl Pts',(-10.869264255462,14.7830326072881,4.30153124285035));
#95927=CARTESIAN_POINT('Ctrl Pts',(-10.9370953648259,14.7767771739846,4.22106110241961));
#95928=CARTESIAN_POINT('Ctrl Pts',(-11.0155227059407,14.7675554195729,4.09791834561534));
#95929=CARTESIAN_POINT('Ctrl Pts',(-11.0358150443397,14.7649090600559,4.06203143521413));
#95930=CARTESIAN_POINT('Ctrl Pts',(-11.0584617860244,14.7615631137386,4.01657113892318));
#95931=CARTESIAN_POINT('Ctrl Pts',(-11.0626342524439,14.7609276528238,4.00793260437782));
#95932=CARTESIAN_POINT('Ctrl Pts',(-11.0690901870508,14.7599130301367,3.99413865638992));
#95933=CARTESIAN_POINT('Ctrl Pts',(-11.0714430267532,14.7595362497053,3.98901603075218));
#95934=CARTESIAN_POINT('Ctrl Pts',(-11.0758079984053,14.7588237438712,3.97932983049848));
#95935=CARTESIAN_POINT('Ctrl Pts',(-11.0778281000815,14.7584882989153,3.97476996661136));
#95936=CARTESIAN_POINT('Ctrl Pts',(-11.0823202761151,14.7577292464072,3.96445358246608));
#95937=CARTESIAN_POINT('Ctrl Pts',(-11.0847754866775,14.7573050802712,3.9586899292822));
#95938=CARTESIAN_POINT('Ctrl Pts',(-11.0909641894919,14.7562114267376,3.94383420555174));
#95939=CARTESIAN_POINT('Ctrl Pts',(-11.0946299981132,14.7555397014751,3.93471464410521));
#95940=CARTESIAN_POINT('Ctrl Pts',(-11.1207624757704,14.7505686146395,3.86727683397196));
#95941=CARTESIAN_POINT('Ctrl Pts',(-11.1386659770076,14.7461193389454,3.80730810563435));
#95942=CARTESIAN_POINT('Ctrl Pts',(-11.1674612877016,14.7361024974039,3.6726093977843));
#95943=CARTESIAN_POINT('Ctrl Pts',(-11.1761037620632,14.7305115454156,3.5976709588132));
#95944=CARTESIAN_POINT('Ctrl Pts',(-11.1778974117992,14.7237241244478,3.5034695223068));
#95945=CARTESIAN_POINT('Ctrl Pts',(-11.1778007149274,14.7223711317165,3.48451098465177));
#95946=CARTESIAN_POINT('Ctrl Pts',(-11.1768917369171,14.7201829942647,3.45343800782624));
#95947=CARTESIAN_POINT('Ctrl Pts',(-11.1763497864266,14.7193369822171,3.44131960701993));
#95948=CARTESIAN_POINT('Ctrl Pts',(-11.1753596703006,14.7182009157122,3.42487632274085));
#95949=CARTESIAN_POINT('Ctrl Pts',(-11.1750746734413,14.7179026400075,3.42054287450894));
#95950=CARTESIAN_POINT('Ctrl Pts',(-11.1745581420938,14.7174061486651,3.4133008327999));
#95951=CARTESIAN_POINT('Ctrl Pts',(-11.1743397596288,14.7172072223932,3.41039138284307));
#95952=CARTESIAN_POINT('Ctrl Pts',(-11.1739057530642,14.7168316903136,3.40488352823782));
#95953=CARTESIAN_POINT('Ctrl Pts',(-11.1736923091171,14.7166549618972,3.40228498510318));
#95954=CARTESIAN_POINT('Ctrl Pts',(-11.1731675700004,14.7162384846137,3.39614653253036));
#95955=CARTESIAN_POINT('Ctrl Pts',(-11.1728488774262,14.7159991425362,3.39260725561084));
#95956=CARTESIAN_POINT('Ctrl Pts',(-11.1716834089743,14.7151686670493,3.38028848612401));
#95957=CARTESIAN_POINT('Ctrl Pts',(-11.1707540076973,14.7145818816721,3.3715168403613));
#95958=CARTESIAN_POINT('Ctrl Pts',(-11.1599944723858,14.7084873102052,3.27981357669443));
#95959=CARTESIAN_POINT('Ctrl Pts',(-11.1414669996497,14.703390024718,3.19812810115913));
#95960=CARTESIAN_POINT('Ctrl Pts',(-11.0927454466446,14.6940697106799,3.05558436386053));
#95961=CARTESIAN_POINT('Ctrl Pts',(-11.0656582272927,14.689889638275,2.99406626589762));
#95962=CARTESIAN_POINT('Ctrl Pts',(-11.0249721304659,14.6843797878794,2.91961894232744));
#95963=CARTESIAN_POINT('Ctrl Pts',(-11.0161104588839,14.6832161548251,2.90424038279996));
#95964=CARTESIAN_POINT('Ctrl Pts',(-11.003182358922,14.6815646249533,2.88293296862757));
#95965=CARTESIAN_POINT('Ctrl Pts',(-10.9994037128228,14.6810870847356,2.87683165883304));
#95966=CARTESIAN_POINT('Ctrl Pts',(-10.9928318699743,14.6802650780787,2.86643374560969));
#95967=CARTESIAN_POINT('Ctrl Pts',(-10.9900659264629,14.6799216158254,2.86212008921976));
#95968=CARTESIAN_POINT('Ctrl Pts',(-10.9847400147653,14.6792649190055,2.8539321020965));
#95969=CARTESIAN_POINT('Ctrl Pts',(-10.9821851047133,14.6789518763997,2.85005458352763));
#95970=CARTESIAN_POINT('Ctrl Pts',(-10.9755215472582,14.6781404365828,2.84007050079291));
#95971=CARTESIAN_POINT('Ctrl Pts',(-10.9713785198365,14.677640761815,2.83398723735266));
#95972=CARTESIAN_POINT('Ctrl Pts',(-10.9593677994562,14.6762055933261,2.81670221532533));
#95973=CARTESIAN_POINT('Ctrl Pts',(-10.9513616893335,14.6752649125774,2.80559857014769));
#95974=CARTESIAN_POINT('Ctrl Pts',(-10.8985606635468,14.6691591906535,2.73499653709905));
#95975=CARTESIAN_POINT('Ctrl Pts',(-10.8484085349741,14.6637843427555,2.67973117641846));
#95976=CARTESIAN_POINT('Ctrl Pts',(-10.7685465747564,14.6558647563047,2.6069374200527));
#95977=CARTESIAN_POINT('Ctrl Pts',(-10.7427501549166,14.6533911746591,2.58537066266472));
#95978=CARTESIAN_POINT('Ctrl Pts',(-10.6798507471014,14.6475952447705,2.53720261894305));
#95979=CARTESIAN_POINT('Ctrl Pts',(-10.6420500350538,14.6442894169076,2.51159296237786));
#95980=CARTESIAN_POINT('Ctrl Pts',(-10.5948015385741,14.6404403631488,2.48344007535465));
#95981=CARTESIAN_POINT('Ctrl Pts',(-10.5866906047509,14.6397892327431,2.47873749756918));
#95982=CARTESIAN_POINT('Ctrl Pts',(-10.5751055582746,14.6388736721212,2.47220427027029));
#95983=CARTESIAN_POINT('Ctrl Pts',(-10.5716773708631,14.6386045189279,2.47029351270828));
#95984=CARTESIAN_POINT('Ctrl Pts',(-10.5657538125789,14.6381425825023,2.46703061987713));
#95985=CARTESIAN_POINT('Ctrl Pts',(-10.5632630078994,14.637949291647,2.46567031302051));
#95986=CARTESIAN_POINT('Ctrl Pts',(-10.558050104394,14.6375467694765,2.46284779771027));
#95987=CARTESIAN_POINT('Ctrl Pts',(-10.5553271484494,14.6373376432458,2.46138728657768));
#95988=CARTESIAN_POINT('Ctrl Pts',(-10.5480685382285,14.6367830902484,2.45753069468107));
#95989=CARTESIAN_POINT('Ctrl Pts',(-10.5435228608847,14.6364388190237,2.45515346713946));
#95990=CARTESIAN_POINT('Ctrl Pts',(-10.5236759054407,14.6349481298397,2.44493879028469));
#95991=CARTESIAN_POINT('Ctrl Pts',(-10.508218704477,14.6338191436672,2.43740674079702));
#95992=CARTESIAN_POINT('Ctrl Pts',(-10.4228116789766,14.627724088782,2.39807957301927));
#95993=CARTESIAN_POINT('Ctrl Pts',(-10.350037250603,14.6230382503442,2.37284654546187));
#95994=CARTESIAN_POINT('Ctrl Pts',(-10.2060823929743,14.6138685967608,2.33823601714495));
#95995=CARTESIAN_POINT('Ctrl Pts',(-10.1354909893856,14.6094124103385,2.32790541231677));
#95996=CARTESIAN_POINT('Ctrl Pts',(-10.0522982170698,14.6039508728099,2.32334926303576));
#95997=CARTESIAN_POINT('Ctrl Pts',(-10.0401829621124,14.6031507042883,2.32287325576203));
#95998=CARTESIAN_POINT('Ctrl Pts',(-10.0218937506142,14.6019345536166,2.3224373452307));
#95999=CARTESIAN_POINT('Ctrl Pts',(-10.0157236667524,14.6015228630233,2.32233879826242));
#96000=CARTESIAN_POINT('Ctrl Pts',(-10.0045738873246,14.6007762391687,2.32224835506252));
#96001=CARTESIAN_POINT('Ctrl Pts',(-9.99959444424118,14.6004418383323,2.32223954395832));
#96002=CARTESIAN_POINT('Ctrl Pts',(-9.98891417538958,14.5997224587871,2.32228837617336));
#96003=CARTESIAN_POINT('Ctrl Pts',(-9.98321354402233,14.5993371839392,2.32235583586629));
#96004=CARTESIAN_POINT('Ctrl Pts',(-9.96788113268124,14.5982973292879,2.32264862453965));
#96005=CARTESIAN_POINT('Ctrl Pts',(-9.95825143043,14.5976403893599,2.32295075283073));
#96006=CARTESIAN_POINT('Ctrl Pts',(-9.91073127949011,14.5943787740444,2.32502554782517));
#96007=CARTESIAN_POINT('Ctrl Pts',(-9.87294196459308,14.5917218418744,2.3285096816482));
#96008=CARTESIAN_POINT('Ctrl Pts',(-9.82727988855788,14.5884328955156,2.33495497532425));
#96009=CARTESIAN_POINT('Ctrl Pts',(-9.81918414308965,14.5878467961096,2.33618399209425));
#96010=CARTESIAN_POINT('Ctrl Pts',(-9.81110404084991,14.5872589202102,2.33749693371726));
#96011=CARTESIAN_POINT('Ctrl Pts',(-9.81110406371064,14.4889165240206,2.33749693000261));
#96012=CARTESIAN_POINT('Ctrl Pts',(-9.81293423381957,14.4890419451336,2.33719954438254));
#96013=CARTESIAN_POINT('Ctrl Pts',(-9.8147651215191,14.4891671265006,2.33690647822745));
#96014=CARTESIAN_POINT('Ctrl Pts',(-9.82221742167204,14.489675507847,2.33573164825552));
#96015=CARTESIAN_POINT('Ctrl Pts',(-9.82784462027069,14.4900567306634,2.33488628516173));
#96016=CARTESIAN_POINT('Ctrl Pts',(-9.85733721477413,14.492041919143,2.33067400898253));
#96017=CARTESIAN_POINT('Ctrl Pts',(-9.88129756629557,14.4936108365854,2.32799920258862));
#96018=CARTESIAN_POINT('Ctrl Pts',(-10.0083675087875,14.5017797674169,2.31775135642753));
#96019=CARTESIAN_POINT('Ctrl Pts',(-10.1120613637523,14.5079580194738,2.32304295719625));
#96020=CARTESIAN_POINT('Ctrl Pts',(-10.2540911247382,14.5170821721449,2.34925395510814));
#96021=CARTESIAN_POINT('Ctrl Pts',(-10.2940218817298,14.519718000193,2.35880355559414));
#96022=CARTESIAN_POINT('Ctrl Pts',(-10.3425582451398,14.523051989106,2.37312791845606));
#96023=CARTESIAN_POINT('Ctrl Pts',(-10.3517128223254,14.5236865838296,2.37595154858003));
#96024=CARTESIAN_POINT('Ctrl Pts',(-10.3661938515876,14.5247000611114,2.38061228501019));
#96025=CARTESIAN_POINT('Ctrl Pts',(-10.3715434553918,14.5250765705145,2.38237651586326));
#96026=CARTESIAN_POINT('Ctrl Pts',(-10.3816038490228,14.5257887112024,2.38577451827883));
#96027=CARTESIAN_POINT('Ctrl Pts',(-10.3863173357958,14.5261240633218,2.38739996564203));
#96028=CARTESIAN_POINT('Ctrl Pts',(-10.39693084664,14.5268831035451,2.3911356133887));
#96029=CARTESIAN_POINT('Ctrl Pts',(-10.402824597866,14.5273073513695,2.39326305490973));
#96030=CARTESIAN_POINT('Ctrl Pts',(-10.4179259514809,14.528401605434,2.39885073114363));
#96031=CARTESIAN_POINT('Ctrl Pts',(-10.4271075329751,14.5290738547771,2.40237941060042));
#96032=CARTESIAN_POINT('Ctrl Pts',(-10.5057251545043,14.5348914096565,2.43372963229322));
#96033=CARTESIAN_POINT('Ctrl Pts',(-10.5723959245945,14.5402563171763,2.46798765006031));
#96034=CARTESIAN_POINT('Ctrl Pts',(-10.680269948406,14.5496267222032,2.53710181888544));
#96035=CARTESIAN_POINT('Ctrl Pts',(-10.723175078213,14.553565868319,2.56889420816404));
#96036=CARTESIAN_POINT('Ctrl Pts',(-10.7707674678369,14.5581061783364,2.60944012662582));
#96037=CARTESIAN_POINT('Ctrl Pts',(-10.7776874022938,14.5587707980073,2.6154765754767));
#96038=CARTESIAN_POINT('Ctrl Pts',(-10.8056081713895,14.5614686907056,2.6404136084886));
#96039=CARTESIAN_POINT('Ctrl Pts',(-10.8259981874437,14.5634772388978,2.65998774845528));
#96040=CARTESIAN_POINT('Ctrl Pts',(-10.8498136540429,14.565851061767,2.68455697518382));
#96041=CARTESIAN_POINT('Ctrl Pts',(-10.8539288001622,14.5662622943024,2.68886734665599));
#96042=CARTESIAN_POINT('Ctrl Pts',(-10.8602768545219,14.5668980546799,2.69561841436734));
#96043=CARTESIAN_POINT('Ctrl Pts',(-10.8625324246797,14.56712422851,2.69803752033576));
#96044=CARTESIAN_POINT('Ctrl Pts',(-10.86667216758,14.5675397954912,2.70251507650378));
#96045=CARTESIAN_POINT('Ctrl Pts',(-10.8685592107731,14.5677293985858,2.70457071530617));
#96046=CARTESIAN_POINT('Ctrl Pts',(-10.8728245906383,14.5681583807778,2.70925045808031));
#96047=CARTESIAN_POINT('Ctrl Pts',(-10.8751984084862,14.5683974234896,2.7118785939477));
#96048=CARTESIAN_POINT('Ctrl Pts',(-10.8824096159105,14.569124659784,2.71993513169187));
#96049=CARTESIAN_POINT('Ctrl Pts',(-10.887208734679,14.5696101262677,2.72539778162062));
#96050=CARTESIAN_POINT('Ctrl Pts',(-10.93090392215,14.5740478705638,2.77607320849554));
#96051=CARTESIAN_POINT('Ctrl Pts',(-10.9663693508976,14.5777824413029,2.82414171107008));
#96052=CARTESIAN_POINT('Ctrl Pts',(-11.0508106610127,14.5876464167405,2.95891812747188));
#96053=CARTESIAN_POINT('Ctrl Pts',(-11.0926995897543,14.5937074532342,3.04946905615169));
#96054=CARTESIAN_POINT('Ctrl Pts',(-11.126881644185,14.6011027636083,3.15733032293103));
#96055=CARTESIAN_POINT('Ctrl Pts',(-11.1308115917176,14.6020098223008,3.17053093363708));
#96056=CARTESIAN_POINT('Ctrl Pts',(-11.136232881713,14.6033506763106,3.18998205254091));
#96057=CARTESIAN_POINT('Ctrl Pts',(-11.1379061056826,14.6037786297008,3.19618100597327));
#96058=CARTESIAN_POINT('Ctrl Pts',(-11.1407961178374,14.6045438366155,3.20724678682331));
#96059=CARTESIAN_POINT('Ctrl Pts',(-11.1420326659282,14.6048804482213,3.21210832780949));
#96060=CARTESIAN_POINT('Ctrl Pts',(-11.1445565337842,14.6055873135629,3.22230321504608));
#96061=CARTESIAN_POINT('Ctrl Pts',(-11.1458377157719,14.6059577542987,3.22763794178963));
#96062=CARTESIAN_POINT('Ctrl Pts',(-11.1491017603532,14.6069329896048,3.24165990363266));
#96063=CARTESIAN_POINT('Ctrl Pts',(-11.1510233572469,14.6075397132775,3.25036089147095));
#96064=CARTESIAN_POINT('Ctrl Pts',(-11.1594578830813,14.6103619483928,3.29072207339611));
#96065=CARTESIAN_POINT('Ctrl Pts',(-11.1647638707397,14.6126149812722,3.32261734028262));
#96066=CARTESIAN_POINT('Ctrl Pts',(-11.1763434941637,14.6192644761263,3.41575273252678));
#96067=CARTESIAN_POINT('Ctrl Pts',(-11.1791375169418,14.6237526012896,3.47731205517231));
#96068=CARTESIAN_POINT('Ctrl Pts',(-11.1748179598547,14.6333779572823,3.60835592588375));
#96069=CARTESIAN_POINT('Ctrl Pts',(-11.1663645580411,14.6385053416449,3.67757754631164));
#96070=CARTESIAN_POINT('Ctrl Pts',(-11.1498404660047,14.6440551964034,3.75505772550908));
#96071=CARTESIAN_POINT('Ctrl Pts',(-11.1477194673653,14.6447237242449,3.76443823420712));
#96072=CARTESIAN_POINT('Ctrl Pts',(-11.1446277623481,14.6456399096332,3.77737322405927));
#96073=CARTESIAN_POINT('Ctrl Pts',(-11.1437549982144,14.6458926785666,3.78095039551506));
#96074=CARTESIAN_POINT('Ctrl Pts',(-11.14222778275,14.6463250475456,3.78708486930395));
#96075=CARTESIAN_POINT('Ctrl Pts',(-11.1415814905393,14.6465050993879,3.78964414490782));
#96076=CARTESIAN_POINT('Ctrl Pts',(-11.1402117380909,14.6468806452424,3.79499246887314));
#96077=CARTESIAN_POINT('Ctrl Pts',(-11.1394866398779,14.6470760377021,3.7977810641469));
#96078=CARTESIAN_POINT('Ctrl Pts',(-11.1376878728838,14.647552593278,3.80459601156371));
#96079=CARTESIAN_POINT('Ctrl Pts',(-11.1366030414523,14.6478331247181,3.80861943206589));
#96080=CARTESIAN_POINT('Ctrl Pts',(-11.1326007551473,14.6488439815732,3.82315572261975));
#96081=CARTESIAN_POINT('Ctrl Pts',(-11.1295585046124,14.649567563875,3.8336340770661));
#96082=CARTESIAN_POINT('Ctrl Pts',(-11.1215761474008,14.6513628282342,3.85976573276624));
#96083=CARTESIAN_POINT('Ctrl Pts',(-11.1164534998664,14.6524258613976,3.87536126106499));
#96084=CARTESIAN_POINT('Ctrl Pts',(-11.0922976195768,14.6570897821305,3.94402609322861));
#96085=CARTESIAN_POINT('Ctrl Pts',(-11.0697931896519,14.660564878311,3.99579914885226));
#96086=CARTESIAN_POINT('Ctrl Pts',(-11.0070677092594,14.6689323507665,4.11574906915157));
#96087=CARTESIAN_POINT('Ctrl Pts',(-10.9635290856411,14.6738241333205,4.18186651266068));
#96088=CARTESIAN_POINT('Ctrl Pts',(-10.904187954839,14.679957554904,4.25482894444066));
#96089=CARTESIAN_POINT('Ctrl Pts',(-10.8944467441091,14.6809494502705,4.26634690655712));
#96090=CARTESIAN_POINT('Ctrl Pts',(-10.8800917572543,14.6823919644239,4.28267354379114));
#96091=CARTESIAN_POINT('Ctrl Pts',(-10.8756539176771,14.6828353779541,4.28763544278683));
#96092=CARTESIAN_POINT('Ctrl Pts',(-10.867774167674,14.6836184310265,4.29629679508238));
#96093=CARTESIAN_POINT('Ctrl Pts',(-10.8643500382866,14.6839573212684,4.30001225108902));
#96094=CARTESIAN_POINT('Ctrl Pts',(-10.8572294932593,14.6846592843272,4.30763953802919));
#96095=CARTESIAN_POINT('Ctrl Pts',(-10.8535299654313,14.6850224849354,4.31154828811887));
#96096=CARTESIAN_POINT('Ctrl Pts',(-10.8439660795996,14.6859576674552,4.32151531406117));
#96097=CARTESIAN_POINT('Ctrl Pts',(-10.8380633022015,14.6865312974635,4.32753613202968));
#96098=CARTESIAN_POINT('Ctrl Pts',(-10.8126936804446,14.6889822300687,4.35286325056157));
#96099=CARTESIAN_POINT('Ctrl Pts',(-10.7926219113799,14.6908860001182,4.37154863987784));
#96100=CARTESIAN_POINT('Ctrl Pts',(-10.6966923128343,14.6998335084222,4.45479595326924));
#96101=CARTESIAN_POINT('Ctrl Pts',(-10.6134963568994,14.7072222902762,4.51026320103002));
#96102=CARTESIAN_POINT('Ctrl Pts',(-10.5045672352622,14.716089569558,4.56442211459493));
#96103=CARTESIAN_POINT('Ctrl Pts',(-10.4845237998406,14.7176885834136,4.57369423657419));
#96104=CARTESIAN_POINT('Ctrl Pts',(-10.4440561498682,14.7208385313725,4.59105044667915));
#96105=CARTESIAN_POINT('Ctrl Pts',(-10.4236420457738,14.7223891122854,4.59913807586688));
#96106=CARTESIAN_POINT('Ctrl Pts',(-10.397821672339,14.7242928332241,4.60854115614481));
#96107=CARTESIAN_POINT('Ctrl Pts',(-10.3926177189635,14.7246736360258,4.61039493317248));
#96108=CARTESIAN_POINT('Ctrl Pts',(-10.3843709103189,14.7252723469188,4.61326742507414));
#96109=CARTESIAN_POINT('Ctrl Pts',(-10.3813366865582,14.7254916167272,4.61431040941936));
#96110=CARTESIAN_POINT('Ctrl Pts',(-10.3759095565038,14.7258819586494,4.61615116798269));
#96111=CARTESIAN_POINT('Ctrl Pts',(-10.3735183617617,14.726053298851,4.61695365081446));
#96112=CARTESIAN_POINT('Ctrl Pts',(-10.3677752047501,14.7264632983501,4.61886054358723));
#96113=CARTESIAN_POINT('Ctrl Pts',(-10.3644208374066,14.7267015264306,4.61995757567266));
#96114=CARTESIAN_POINT('Ctrl Pts',(-10.354200033012,14.7274237960078,4.62324946611672));
#96115=CARTESIAN_POINT('Ctrl Pts',(-10.3473181741079,14.7279051644054,4.62539642743313));
#96116=CARTESIAN_POINT('Ctrl Pts',(-10.2756307801387,14.7328724757502,4.64704079557005));
#96117=CARTESIAN_POINT('Ctrl Pts',(-10.209268916036,14.7370768447313,4.66098415906031));
#96118=CARTESIAN_POINT('Ctrl Pts',(-10.0526088267597,14.7468413105054,4.68002055041062));
#96119=CARTESIAN_POINT('Ctrl Pts',(-9.96220888246291,14.752375586307,4.68058705396627));
#96120=CARTESIAN_POINT('Ctrl Pts',(-9.85807423215819,14.759211889364,4.66925899073041));
#96121=CARTESIAN_POINT('Ctrl Pts',(-9.84354741707947,14.7601753391968,4.66740398717299));
#96122=CARTESIAN_POINT('Ctrl Pts',(-9.822549914558,14.761583847056,4.66432375905274));
#96123=CARTESIAN_POINT('Ctrl Pts',(-9.81604858625527,14.7620221726441,4.66331432688812));
#96124=CARTESIAN_POINT('Ctrl Pts',(-9.80458246338393,14.7627993048742,4.66143551297271));
#96125=CARTESIAN_POINT('Ctrl Pts',(-9.79961411075584,14.7631373977517,4.66058862584926));
#96126=CARTESIAN_POINT('Ctrl Pts',(-9.78932077478975,14.7638407385948,4.65876599587258));
#96127=CARTESIAN_POINT('Ctrl Pts',(-9.7839967870726,14.764206132854,4.65778537710453));
#96128=CARTESIAN_POINT('Ctrl Pts',(-9.77025545296731,14.7651534797669,4.65515629832833));
#96129=CARTESIAN_POINT('Ctrl Pts',(-9.76184913977029,14.76573716417,4.65345255275223));
#96130=CARTESIAN_POINT('Ctrl Pts',(-9.72528433804273,14.7682946193264,4.64562505033576));
#96131=CARTESIAN_POINT('Ctrl Pts',(-9.69733951064603,14.7702978151118,4.63856129770724));
#96132=CARTESIAN_POINT('Ctrl Pts',(-9.57506298427151,14.7792869260106,4.6028331995487));
#96133=CARTESIAN_POINT('Ctrl Pts',(-9.48429642910721,14.7866026902786,4.56341748961802));
#96134=CARTESIAN_POINT('Ctrl Pts',(-9.36374275962097,14.7968134426532,4.49196839633069));
#96135=CARTESIAN_POINT('Ctrl Pts',(-9.32911062641871,14.7998057207872,4.46888225025379));
#96136=CARTESIAN_POINT('Ctrl Pts',(-9.29098534403438,14.8031113213706,4.44044080147653));
#96137=CARTESIAN_POINT('Ctrl Pts',(-9.28622858114858,14.8035239464685,4.4368356573072));
#96138=CARTESIAN_POINT('Ctrl Pts',(-9.27865071997443,14.8041813360847,4.43100118336367));
#96139=CARTESIAN_POINT('Ctrl Pts',(-9.27581214181668,14.8044275975322,4.42879488270785));
#96140=CARTESIAN_POINT('Ctrl Pts',(-9.27078069243108,14.8048640556388,4.42484707103445));
#96141=CARTESIAN_POINT('Ctrl Pts',(-9.26858387747804,14.8050546015021,4.42311069740831));
#96142=CARTESIAN_POINT('Ctrl Pts',(-9.26386885074058,14.8054635152451,4.4193565172298));
#96143=CARTESIAN_POINT('Ctrl Pts',(-9.26135272977089,14.8056817015405,4.4173361900079));
#96144=CARTESIAN_POINT('Ctrl Pts',(-9.25437246248923,14.8062870270788,4.41168402189543));
#96145=CARTESIAN_POINT('Ctrl Pts',(-9.24992650935375,14.8066726116267,4.40802970351166));
#96146=CARTESIAN_POINT('Ctrl Pts',(-9.22387628788555,14.8089332918791,4.38629602245145));
#96147=CARTESIAN_POINT('Ctrl Pts',(-9.20289755326056,14.8107597283598,4.36747717169165));
#96148=CARTESIAN_POINT('Ctrl Pts',(-9.12900729872061,14.8173021317855,4.29624777018278));
#96149=CARTESIAN_POINT('Ctrl Pts',(-9.08041994396663,14.8218301556969,4.23960320358204));
#96150=CARTESIAN_POINT('Ctrl Pts',(-9.00095229601274,14.8304010415379,4.1269141621821));
#96151=CARTESIAN_POINT('Ctrl Pts',(-8.96865184613659,14.8344014863188,4.07222114662977));
#96152=CARTESIAN_POINT('Ctrl Pts',(-8.93660820337859,14.8392141266783,4.00634947520666));
#96153=CARTESIAN_POINT('Ctrl Pts',(-8.93241459642619,14.8398642674036,3.99744678171769));
#96154=CARTESIAN_POINT('Ctrl Pts',(-8.92573363936063,14.8409346830287,3.98278994282049));
#96155=CARTESIAN_POINT('Ctrl Pts',(-8.92317974014707,14.841352689457,3.97706652355469));
#96156=CARTESIAN_POINT('Ctrl Pts',(-8.91867632547232,14.8421060378849,3.96675371875761));
#96157=CARTESIAN_POINT('Ctrl Pts',(-8.91671002983823,14.8424408026741,3.96217178873578));
#96158=CARTESIAN_POINT('Ctrl Pts',(-8.91258472669379,14.8431558211076,3.95238789416552));
#96159=CARTESIAN_POINT('Ctrl Pts',(-8.91043382796299,14.8435363375505,3.94718266765402));
#96160=CARTESIAN_POINT('Ctrl Pts',(-8.90472690878862,14.8445672450048,3.93308615424925));
#96161=CARTESIAN_POINT('Ctrl Pts',(-8.90124192215698,14.8452199833791,3.92416675762203));
#96162=CARTESIAN_POINT('Ctrl Pts',(-8.88342201305638,14.848684774279,3.87686512721869));
#96163=CARTESIAN_POINT('Ctrl Pts',(-8.87099005429562,14.8515585665808,3.83780107855562));
#96164=CARTESIAN_POINT('Ctrl Pts',(-8.83456994791559,14.8618427957405,3.69863216364627));
#96165=CARTESIAN_POINT('Ctrl Pts',(-8.82167971737458,14.8695451621305,3.59612227437252));
#96166=CARTESIAN_POINT('Ctrl Pts',(-8.82241038998768,14.8786952191972,3.46864150248868));
#96167=CARTESIAN_POINT('Ctrl Pts',(-8.82332268216843,14.8804383357746,3.44404161405692));
#96168=CARTESIAN_POINT('Ctrl Pts',(-8.82539670375381,14.8825415351595,3.41377387075647));
#96169=CARTESIAN_POINT('Ctrl Pts',(-8.82582980620738,14.882936454466,3.40806410785191));
#96170=CARTESIAN_POINT('Ctrl Pts',(-8.82657437265931,14.8835523750952,3.39911416248918));
#96171=CARTESIAN_POINT('Ctrl Pts',(-8.82685764804543,14.8837748672258,3.39587182028009));
#96172=CARTESIAN_POINT('Ctrl Pts',(-8.82740926856241,14.8841871066834,3.38984621164526));
#96173=CARTESIAN_POINT('Ctrl Pts',(-8.82767408249321,14.8843770369204,3.3870627433592));
#96174=CARTESIAN_POINT('Ctrl Pts',(-8.82830387567952,14.8848111726653,3.38068397723092));
#96175=CARTESIAN_POINT('Ctrl Pts',(-8.82867549102864,14.8850550076705,3.37708939592085));
#96176=CARTESIAN_POINT('Ctrl Pts',(-8.82988463869388,14.8858118444432,3.36589733248134));
#96177=CARTESIAN_POINT('Ctrl Pts',(-8.83077960961855,14.8863217861112,3.35830606743831));
#96178=CARTESIAN_POINT('Ctrl Pts',(-8.83305142829184,14.8875092764791,3.34052656990169));
#96179=CARTESIAN_POINT('Ctrl Pts',(-8.83448791102983,14.8881839215533,3.33034644009327));
#96180=CARTESIAN_POINT('Ctrl Pts',(-8.84007543750577,14.8905661542634,3.29417817271374));
#96181=CARTESIAN_POINT('Ctrl Pts',(-8.84496417718864,14.8922429639983,3.26831043742945));
#96182=CARTESIAN_POINT('Ctrl Pts',(-8.86885246286306,14.8991245716152,3.1616388672475));
#96183=CARTESIAN_POINT('Ctrl Pts',(-8.89549862713555,14.9041474763056,3.08279426334177));
#96184=CARTESIAN_POINT('Ctrl Pts',(-8.94888091858975,14.9121800298246,2.96686228332463));
#96185=CARTESIAN_POINT('Ctrl Pts',(-8.96983612135003,14.9150366982327,2.92741915022942));
#96186=CARTESIAN_POINT('Ctrl Pts',(-8.99820566270971,14.9186362252825,2.88064159187921));
#96187=CARTESIAN_POINT('Ctrl Pts',(-9.00354475615701,14.9193034491926,2.8720878496451));
#96188=CARTESIAN_POINT('Ctrl Pts',(-9.01212802464166,14.9203609145502,2.85872183356845));
#96189=CARTESIAN_POINT('Ctrl Pts',(-9.01529914929462,14.9207484712044,2.85386304933259));
#96190=CARTESIAN_POINT('Ctrl Pts',(-9.0212268379329,14.9214673082475,2.84492565947373));
#96191=CARTESIAN_POINT('Ctrl Pts',(-9.02397333398012,14.9217982084992,2.84084050461848));
#96192=CARTESIAN_POINT('Ctrl Pts',(-9.03013288883432,14.9225356287542,2.8318016488143));
#96193=CARTESIAN_POINT('Ctrl Pts',(-9.03355843457985,14.9229426123702,2.82685666597219));
#96194=CARTESIAN_POINT('Ctrl Pts',(-9.04356834698078,14.9241230915321,2.81264066214283));
#96195=CARTESIAN_POINT('Ctrl Pts',(-9.05024913575004,14.9249002304131,2.80343869882319));
#96196=CARTESIAN_POINT('Ctrl Pts',(-9.1069787832802,14.9314137302726,2.72763423188245));
#96197=CARTESIAN_POINT('Ctrl Pts',(-9.16382208758642,14.9374250002639,2.66643109383375));
#96198=CARTESIAN_POINT('Ctrl Pts',(-9.28411001039993,14.9491220011564,2.5617011230202));
#96199=CARTESIAN_POINT('Ctrl Pts',(-9.34631482058239,14.9547585212957,2.5173500529682));
#96200=CARTESIAN_POINT('Ctrl Pts',(-9.42043600508338,14.9607458557213,2.47467703485501));
#96201=CARTESIAN_POINT('Ctrl Pts',(-9.42855329944845,14.9613922503499,2.4701309359869));
#96202=CARTESIAN_POINT('Ctrl Pts',(-9.43991588032141,14.9622833492175,2.46394302682071));
#96203=CARTESIAN_POINT('Ctrl Pts',(-9.44311592341879,14.9625328128592,2.46221948422438));
#96204=CARTESIAN_POINT('Ctrl Pts',(-9.44864273048926,14.9629610247593,2.45927567240799));
#96205=CARTESIAN_POINT('Ctrl Pts',(-9.45096566917556,14.9631402059725,2.45804833672202));
#96206=CARTESIAN_POINT('Ctrl Pts',(-9.45585524913933,14.9635156622435,2.4554857958263));
#96207=CARTESIAN_POINT('Ctrl Pts',(-9.45842273393063,14.963711827104,2.45415225879698));
#96208=CARTESIAN_POINT('Ctrl Pts',(-9.46475319388827,14.964193141046,2.4508938166906));
#96209=CARTESIAN_POINT('Ctrl Pts',(-9.46852171487081,14.964477628646,2.44897965713209));
#96210=CARTESIAN_POINT('Ctrl Pts',(-9.4824158605233,14.9655193316351,2.4420161902041));
#96211=CARTESIAN_POINT('Ctrl Pts',(-9.49260418409054,14.9662692526915,2.43709238753589));
#96212=CARTESIAN_POINT('Ctrl Pts',(-9.5184918678138,14.9681437681776,2.42503850091484));
#96213=CARTESIAN_POINT('Ctrl Pts',(-9.53428016873737,14.9692587043117,2.41810471426228));
#96214=CARTESIAN_POINT('Ctrl Pts',(-9.60741140232171,14.9743196859778,2.38788526934962));
#96215=CARTESIAN_POINT('Ctrl Pts',(-9.66638524333647,14.9781173908488,2.36879384822741));
#96216=CARTESIAN_POINT('Ctrl Pts',(-9.75456087925998,14.9837249510963,2.34774932249269));
#96217=CARTESIAN_POINT('Ctrl Pts',(-9.78275116732423,14.985506817339,2.34210401195159));
#96218=CARTESIAN_POINT('Ctrl Pts',(-9.81110406371068,14.9873061497326,2.3374969300026));
#96219=CARTESIAN_POINT('Origin',(-10.,12.3756328852638,3.5));
#96220=CARTESIAN_POINT('',(-9.81110406370779,15.5854602598056,2.33749693000307));
#96221=CARTESIAN_POINT('',(-9.81110406371068,15.4869977587645,2.3374969300026));
#96222=CARTESIAN_POINT('',(-9.81110406371068,12.3756328852638,2.3374969300026));
#96223=CARTESIAN_POINT('',(-11.177749800465,15.2252691226695,3.49931443112735));
#96224=CARTESIAN_POINT('Ctrl Pts',(-9.8111040637049,15.5854602598056,2.33749693000354));
#96225=CARTESIAN_POINT('Ctrl Pts',(-9.80497997839647,15.5850478740051,2.33849203690528));
#96226=CARTESIAN_POINT('Ctrl Pts',(-9.79886362718618,15.584637878246,2.33953555748687));
#96227=CARTESIAN_POINT('Ctrl Pts',(-9.77690176011872,15.5831715139842,2.34346136555285));
#96228=CARTESIAN_POINT('Ctrl Pts',(-9.76110689590806,15.5821277871477,2.34662036760273));
#96229=CARTESIAN_POINT('Ctrl Pts',(-9.69222399029384,15.5776042086662,2.36187294157862));
#96230=CARTESIAN_POINT('Ctrl Pts',(-9.63994279147801,15.5742425680384,2.37731615278718));
#96231=CARTESIAN_POINT('Ctrl Pts',(-9.51254385567699,15.5658386917472,2.42476831621584));
#96232=CARTESIAN_POINT('Ctrl Pts',(-9.43934172860403,15.5608006364909,2.46105974364422));
#96233=CARTESIAN_POINT('Ctrl Pts',(-9.35777022547683,15.5545056865252,2.51264901278325));
#96234=CARTESIAN_POINT('Ctrl Pts',(-9.34522040918453,15.5535170920549,2.52092660682595));
#96235=CARTESIAN_POINT('Ctrl Pts',(-9.32735333313186,15.5520784311383,2.53320853446642));
#96236=CARTESIAN_POINT('Ctrl Pts',(-9.321905847371,15.551635513586,2.5370214989951));
#96237=CARTESIAN_POINT('Ctrl Pts',(-9.31237623576086,15.5508529480452,2.54381270048421));
#96238=CARTESIAN_POINT('Ctrl Pts',(-9.30828040701381,15.5505140453434,2.54677148793252));
#96239=CARTESIAN_POINT('Ctrl Pts',(-9.29985686714895,15.5498116760611,2.55293945124579));
#96240=CARTESIAN_POINT('Ctrl Pts',(-9.29553189175542,15.5494480792905,2.55615214558587));
#96241=CARTESIAN_POINT('Ctrl Pts',(-9.28447857322339,15.5485110669654,2.56448110870179));
#96242=CARTESIAN_POINT('Ctrl Pts',(-9.27778308732061,15.5479359918963,2.56964026704523));
#96243=CARTESIAN_POINT('Ctrl Pts',(-9.24946641369543,15.545471199995,2.59194935026712));
#96244=CARTESIAN_POINT('Ctrl Pts',(-9.22839764286046,15.5435546453094,2.60978304409426));
#96245=CARTESIAN_POINT('Ctrl Pts',(-9.13433484186276,15.5345995569571,2.69525203735334));
#96246=CARTESIAN_POINT('Ctrl Pts',(-9.06947770343406,15.527217691094,2.77122172524814));
#96247=CARTESIAN_POINT('Ctrl Pts',(-9.00283768800216,15.5183566656608,2.87290281522489));
#96248=CARTESIAN_POINT('Ctrl Pts',(-8.99124471207531,15.5167561491735,2.89172669079959));
#96249=CARTESIAN_POINT('Ctrl Pts',(-8.96927072961381,15.5136141533542,2.92976447832821));
#96250=CARTESIAN_POINT('Ctrl Pts',(-8.95888012308026,15.5120727559877,2.94896376721643));
#96251=CARTESIAN_POINT('Ctrl Pts',(-8.9465394495763,15.5101785552789,2.97336317809581));
#96252=CARTESIAN_POINT('Ctrl Pts',(-8.94408505144539,15.5097984136241,2.97830171756258));
#96253=CARTESIAN_POINT('Ctrl Pts',(-8.94025833212916,15.5092004645616,2.98613917829176));
#96254=CARTESIAN_POINT('Ctrl Pts',(-8.93886304627302,15.5089813016404,2.98902670053372));
#96255=CARTESIAN_POINT('Ctrl Pts',(-8.93639086798018,15.5085909785756,2.99419663366376));
#96256=CARTESIAN_POINT('Ctrl Pts',(-8.93530952245058,15.5084195515121,2.99647679466824));
#96257=CARTESIAN_POINT('Ctrl Pts',(-8.93273131592822,15.5080091188783,3.00195872682732));
#96258=CARTESIAN_POINT('Ctrl Pts',(-8.93124152936349,15.5077705466124,3.00516377856169));
#96259=CARTESIAN_POINT('Ctrl Pts',(-8.92674767615076,15.5070464290515,3.01494659886172));
#96260=CARTESIAN_POINT('Ctrl Pts',(-8.92378967162901,15.5065635760108,3.02154552129065));
#96261=CARTESIAN_POINT('Ctrl Pts',(-8.89759106263942,15.5022259430144,3.08146371763057));
#96262=CARTESIAN_POINT('Ctrl Pts',(-8.87826593986942,15.4985782748313,3.13641685949991));
#96263=CARTESIAN_POINT('Ctrl Pts',(-8.83664217166861,15.4886820186467,3.29035262503834));
#96264=CARTESIAN_POINT('Ctrl Pts',(-8.82292928160331,15.4825140124548,3.39111505943759));
#96265=CARTESIAN_POINT('Ctrl Pts',(-8.82218706975079,15.4750067508844,3.50592792649185));
#96266=CARTESIAN_POINT('Ctrl Pts',(-8.82233308625764,15.4741146523486,3.51946932382251));
#96267=CARTESIAN_POINT('Ctrl Pts',(-8.82289324673785,15.4727871272006,3.53945038335277));
#96268=CARTESIAN_POINT('Ctrl Pts',(-8.82312687570919,15.4723572819168,3.54589431180603));
#96269=CARTESIAN_POINT('Ctrl Pts',(-8.82363591445121,15.4715907159037,3.55733823977421));
#96270=CARTESIAN_POINT('Ctrl Pts',(-8.8238903210968,15.4712546547294,3.56233905174174));
#96271=CARTESIAN_POINT('Ctrl Pts',(-8.82449280984534,15.4705453200025,3.57285941340306));
#96272=CARTESIAN_POINT('Ctrl Pts',(-8.82484789534452,15.4701718367676,3.57837842396655));
#96273=CARTESIAN_POINT('Ctrl Pts',(-8.82589047010176,15.4691801793425,3.59297736720144));
#96274=CARTESIAN_POINT('Ctrl Pts',(-8.82664440411178,15.4685599572445,3.60205202836472));
#96275=CARTESIAN_POINT('Ctrl Pts',(-8.83076578604388,15.4655687024723,3.64554054904665));
#96276=CARTESIAN_POINT('Ctrl Pts',(-8.83554216272774,15.4631544213527,3.67980049146867));
#96277=CARTESIAN_POINT('Ctrl Pts',(-8.85387899485703,15.4559798897554,3.77913444296485));
#96278=CARTESIAN_POINT('Ctrl Pts',(-8.8714458742821,15.4511138615483,3.84332658666985));
#96279=CARTESIAN_POINT('Ctrl Pts',(-8.91563961387797,15.4416929990599,3.96377338156195));
#96280=CARTESIAN_POINT('Ctrl Pts',(-8.94149831566611,15.4371562621329,4.02009512604862));
#96281=CARTESIAN_POINT('Ctrl Pts',(-8.97641790205619,15.4321366740237,4.08264035539016));
#96282=CARTESIAN_POINT('Ctrl Pts',(-8.98127576595169,15.4314588385059,4.09109309367742));
#96283=CARTESIAN_POINT('Ctrl Pts',(-8.98812161176306,15.4305322371013,4.10266979416489));
#96284=CARTESIAN_POINT('Ctrl Pts',(-8.99002003479769,15.4302782071096,4.10584587495526));
#96285=CARTESIAN_POINT('Ctrl Pts',(-8.99330112077183,15.4298442090149,4.11127688060304));
#96286=CARTESIAN_POINT('Ctrl Pts',(-8.99467645463314,15.4296637820819,4.11353616656569));
#96287=CARTESIAN_POINT('Ctrl Pts',(-8.99756438642479,15.4292880508206,4.11824444058674));
#96288=CARTESIAN_POINT('Ctrl Pts',(-8.9990783659331,15.4290928451208,4.12069254093943));
#96289=CARTESIAN_POINT('Ctrl Pts',(-9.00279620870083,15.4286177161067,4.12665530444166));
#96290=CARTESIAN_POINT('Ctrl Pts',(-9.00500972416929,15.4283384149822,4.13016396617993));
#96291=CARTESIAN_POINT('Ctrl Pts',(-9.01304220243794,15.4273373728062,4.14274847085491));
#96292=CARTESIAN_POINT('Ctrl Pts',(-9.01896739133281,15.4266222028266,4.15175634410521));
#96293=CARTESIAN_POINT('Ctrl Pts',(-9.03407546891208,15.424852136019,4.17405169813914));
#96294=CARTESIAN_POINT('Ctrl Pts',(-9.04340976598194,15.4238055785717,4.18723436330639));
#96295=CARTESIAN_POINT('Ctrl Pts',(-9.08554765861703,15.419261736104,4.24422211100597));
#96296=CARTESIAN_POINT('Ctrl Pts',(-9.12111233029219,15.415883741409,4.28590524180874));
#96297=CARTESIAN_POINT('Ctrl Pts',(-9.21627615992236,15.4074855073915,4.38286675718949));
#96298=CARTESIAN_POINT('Ctrl Pts',(-9.27892561369515,15.402468800792,4.43473332766982));
#96299=CARTESIAN_POINT('Ctrl Pts',(-9.35891722482121,15.3961973419562,4.48809626133481));
#96300=CARTESIAN_POINT('Ctrl Pts',(-9.37158929024165,15.395208122119,4.49620343937413));
#96301=CARTESIAN_POINT('Ctrl Pts',(-9.39008289854408,15.3937687142639,4.50754177490907));
#96302=CARTESIAN_POINT('Ctrl Pts',(-9.39578234549652,15.3933256856728,4.5109699905384));
#96303=CARTESIAN_POINT('Ctrl Pts',(-9.40586241323323,15.3925429905768,4.51691746161065));
#96304=CARTESIAN_POINT('Ctrl Pts',(-9.41023082066017,15.3922040701362,4.51945716412018));
#96305=CARTESIAN_POINT('Ctrl Pts',(-9.41928983776777,15.3915017292105,4.52464617782961));
#96306=CARTESIAN_POINT('Ctrl Pts',(-9.42398254383709,15.391138178932,4.52729157048406));
#96307=CARTESIAN_POINT('Ctrl Pts',(-9.43608195233882,15.3902014246819,4.53400333242571));
#96308=CARTESIAN_POINT('Ctrl Pts',(-9.44351445867763,15.3896265629591,4.53802229829774));
#96309=CARTESIAN_POINT('Ctrl Pts',(-9.4753786754746,15.3871639904873,4.55481159774689));
#96310=CARTESIAN_POINT('Ctrl Pts',(-9.50020969459478,15.3852495021509,4.56680104596345));
#96311=CARTESIAN_POINT('Ctrl Pts',(-9.6165223649936,15.3762952418274,4.6180092589184));
#96312=CARTESIAN_POINT('Ctrl Pts',(-9.71231518810764,15.3689118162868,4.64639928008942));
#96313=CARTESIAN_POINT('Ctrl Pts',(-9.83232309546905,15.3600493210264,4.66596221879791));
#96314=CARTESIAN_POINT('Ctrl Pts',(-9.85423129963794,15.3584489743901,4.66890334069077));
#96315=CARTESIAN_POINT('Ctrl Pts',(-9.89792808957471,15.3553060978113,4.67352175962943));
#96316=CARTESIAN_POINT('Ctrl Pts',(-9.91970731040881,15.3537636800646,4.67521284388546));
#96317=CARTESIAN_POINT('Ctrl Pts',(-9.94703157128658,15.3518684119954,4.6765712184568));
#96318=CARTESIAN_POINT('Ctrl Pts',(-9.95254255984136,15.351488187589,4.67680639058072));
#96319=CARTESIAN_POINT('Ctrl Pts',(-9.96126026912912,15.3508901375277,4.67711706372251));
#96320=CARTESIAN_POINT('Ctrl Pts',(-9.96446590889335,15.3506709556178,4.67721819449417));
#96321=CARTESIAN_POINT('Ctrl Pts',(-9.97019458475274,15.3502806165287,4.67737550004441));
#96322=CARTESIAN_POINT('Ctrl Pts',(-9.97271737522506,15.3501091922898,4.67743666048219));
#96323=CARTESIAN_POINT('Ctrl Pts',(-9.97877353729265,15.3496987892744,4.67756400600079));
#96324=CARTESIAN_POINT('Ctrl Pts',(-9.98230703057967,15.3494602436205,4.67762239729099));
#96325=CARTESIAN_POINT('Ctrl Pts',(-9.99306942488246,15.3487362881248,4.67775179487399));
#96326=CARTESIAN_POINT('Ctrl Pts',(-10.0002989300676,15.3482535687784,4.67777215127619));
#96327=CARTESIAN_POINT('Ctrl Pts',(-10.0656196288155,15.3439207760291,4.67735460125613));
#96328=CARTESIAN_POINT('Ctrl Pts',(-10.1236124619663,15.3402773097701,4.67268566257046));
#96329=CARTESIAN_POINT('Ctrl Pts',(-10.2812022703571,15.3303794258593,4.64817136583203));
#96330=CARTESIAN_POINT('Ctrl Pts',(-10.3789309832042,15.3242062154971,4.61972383351043));
#96331=CARTESIAN_POINT('Ctrl Pts',(-10.4842049936918,15.3166935073353,4.57369625673667));
#96332=CARTESIAN_POINT('Ctrl Pts',(-10.4965072739199,15.3158021538,4.56806302715288));
#96333=CARTESIAN_POINT('Ctrl Pts',(-10.5145230441135,15.3144755276765,4.55943506183962));
#96334=CARTESIAN_POINT('Ctrl Pts',(-10.5203136554389,15.3140458253088,4.55660319437225));
#96335=CARTESIAN_POINT('Ctrl Pts',(-10.5304012041859,15.3132913254447,4.55156690012374));
#96336=CARTESIAN_POINT('Ctrl Pts',(-10.5347084114321,15.3129672548892,4.54938329336373));
#96337=CARTESIAN_POINT('Ctrl Pts',(-10.5391410849613,15.3126317331571,4.54710170349962));
#96338=CARTESIAN_POINT('Ctrl Pts',(-10.539280142287,15.3126212054605,4.54703009273848));
#96339=CARTESIAN_POINT('Ctrl Pts',(-10.5395852440368,15.3125981024381,4.54687289668485));
#96340=CARTESIAN_POINT('Ctrl Pts',(-10.5397512823491,15.3125855267004,4.54678729959723));
#96341=CARTESIAN_POINT('Ctrl Pts',(-10.5400344625771,15.3125640736426,4.54664122750279));
#96342=CARTESIAN_POINT('Ctrl Pts',(-10.5401516147559,15.3125551970149,4.5465807723038));
#96343=CARTESIAN_POINT('Ctrl Pts',(-10.5403511731348,15.3125400739787,4.54647774978475));
#96344=CARTESIAN_POINT('Ctrl Pts',(-10.5404335844838,15.312533827917,4.54643519238637));
#96345=CARTESIAN_POINT('Ctrl Pts',(-10.5406174607539,15.3125198900865,4.54634021076868));
#96346=CARTESIAN_POINT('Ctrl Pts',(-10.5407189230572,15.3125121981432,4.54628778153586));
#96347=CARTESIAN_POINT('Ctrl Pts',(-10.5457612505635,15.312129880544,4.54368129963983));
#96348=CARTESIAN_POINT('Ctrl Pts',(-10.5506838942261,15.3117540373113,4.54109233242541));
#96349=CARTESIAN_POINT('Ctrl Pts',(-10.563981795412,15.3107315611732,4.53397786277853));
#96350=CARTESIAN_POINT('Ctrl Pts',(-10.5723206695486,15.31008259189,4.52938560715));
#96351=CARTESIAN_POINT('Ctrl Pts',(-10.5906765951926,15.3086363238807,4.51898492898944));
#96352=CARTESIAN_POINT('Ctrl Pts',(-10.6006653957554,15.307837386662,4.51312891155158));
#96353=CARTESIAN_POINT('Ctrl Pts',(-10.6310474746586,15.3053699275826,4.49470991677268));
#96354=CARTESIAN_POINT('Ctrl Pts',(-10.6511441510626,15.3036850291149,4.481671987425));
#96355=CARTESIAN_POINT('Ctrl Pts',(-10.7334473066008,15.2965603845836,4.42463737969575));
#96356=CARTESIAN_POINT('Ctrl Pts',(-10.7917023962785,15.2909473658913,4.37527373097714));
#96357=CARTESIAN_POINT('Ctrl Pts',(-10.8830895676957,15.2813345391011,4.2811986764104));
#96358=CARTESIAN_POINT('Ctrl Pts',(-10.9185990278178,15.2773365879844,4.23911829785002));
#96359=CARTESIAN_POINT('Ctrl Pts',(-10.954977091309,15.2730489588954,4.18931730291256));
#96360=CARTESIAN_POINT('Ctrl Pts',(-10.9588673609428,15.2725877271738,4.18389544401191));
#96361=CARTESIAN_POINT('Ctrl Pts',(-10.9647077442405,15.2718914740571,4.17560790432105));
#96362=CARTESIAN_POINT('Ctrl Pts',(-10.9666915578758,15.2716542912104,4.17276630778495));
#96363=CARTESIAN_POINT('Ctrl Pts',(-10.9702486305052,15.271227826574,4.16762296996047));
#96364=CARTESIAN_POINT('Ctrl Pts',(-10.9718262750049,15.2710382568555,4.16532437704725));
#96365=CARTESIAN_POINT('Ctrl Pts',(-10.9752950118096,15.2706205122952,4.16023184107989));
#96366=CARTESIAN_POINT('Ctrl Pts',(-10.9771822670968,15.2703925928189,4.15743536688117));
#96367=CARTESIAN_POINT('Ctrl Pts',(-10.982637162785,15.269731837673,4.14927709389871));
#96368=CARTESIAN_POINT('Ctrl Pts',(-10.9861729434346,15.2693010500652,4.14389398865759));
#96369=CARTESIAN_POINT('Ctrl Pts',(-11.0149389975124,15.2657730747218,4.09930582152382));
#96370=CARTESIAN_POINT('Ctrl Pts',(-11.0378684037033,15.2628107266906,4.05865815634376));
#96371=CARTESIAN_POINT('Ctrl Pts',(-11.0965276287925,15.2544515883057,3.93852187180898));
#96372=CARTESIAN_POINT('Ctrl Pts',(-11.1259330724032,15.2491782937948,3.8562991985869));
#96373=CARTESIAN_POINT('Ctrl Pts',(-11.1539622040777,15.2414494534809,3.7380249982986));
#96374=CARTESIAN_POINT('Ctrl Pts',(-11.16043689709,15.2392221904702,3.70413358519621));
#96375=CARTESIAN_POINT('Ctrl Pts',(-11.1667307815935,15.2363467634431,3.66098895369808));
#96376=CARTESIAN_POINT('Ctrl Pts',(-11.1679418508406,15.235742458922,3.65195389186633));
#96377=CARTESIAN_POINT('Ctrl Pts',(-11.1697192067958,15.2347661204175,3.63741415344351));
#96378=CARTESIAN_POINT('Ctrl Pts',(-11.1703518080219,15.2343961625815,3.6319178380571));
#96379=CARTESIAN_POINT('Ctrl Pts',(-11.1714661979238,15.2336996369797,3.62159575784115));
#96380=CARTESIAN_POINT('Ctrl Pts',(-11.1719569527852,15.2333733565928,3.61677106152563));
#96381=CARTESIAN_POINT('Ctrl Pts',(-11.1728779720587,15.2327195351027,3.60712495298329));
#96382=CARTESIAN_POINT('Ctrl Pts',(-11.173308337893,15.2323920038548,3.60230364562684));
#96383=CARTESIAN_POINT('Ctrl Pts',(-11.1742220445471,15.2316428848166,3.59130213796457));
#96384=CARTESIAN_POINT('Ctrl Pts',(-11.1746863330126,15.2312207131845,3.58512054258543));
#96385=CARTESIAN_POINT('Ctrl Pts',(-11.1758162101567,15.2300684504547,3.56830025548825));
#96386=CARTESIAN_POINT('Ctrl Pts',(-11.1763861882568,15.2293354365132,3.55765594578078));
#96387=CARTESIAN_POINT('Ctrl Pts',(-11.1774464169547,15.2274976079971,3.53111256017193));
#96388=CARTESIAN_POINT('Ctrl Pts',(-11.177759058463,15.2263882685434,3.51521889493337));
#96389=CARTESIAN_POINT('Ctrl Pts',(-11.177749800465,15.2252691226695,3.49931443112713));
#96390=CARTESIAN_POINT('Ctrl Pts',(-11.177749800465,15.2252691226695,3.49931443112735));
#96391=CARTESIAN_POINT('Ctrl Pts',(-11.1776833668831,15.2172383509074,3.38518711153303));
#96392=CARTESIAN_POINT('Ctrl Pts',(-11.1610284219822,15.2087014221751,3.27169185811116));
#96393=CARTESIAN_POINT('Ctrl Pts',(-11.1196692688029,15.1982875511688,3.13346584831714));
#96394=CARTESIAN_POINT('Ctrl Pts',(-11.1099049574073,15.1961385686007,3.10488242312908));
#96395=CARTESIAN_POINT('Ctrl Pts',(-11.0969444877652,15.1936381828625,3.07123172618874));
#96396=CARTESIAN_POINT('Ctrl Pts',(-11.0947962321001,15.19323374056,3.06577580027221));
#96397=CARTESIAN_POINT('Ctrl Pts',(-11.0913936342866,15.1926086592552,3.05732001782686));
#96398=CARTESIAN_POINT('Ctrl Pts',(-11.0901675028691,15.192386420441,3.0543090219499));
#96399=CARTESIAN_POINT('Ctrl Pts',(-11.087863039499,15.1919743269229,3.04871638972749));
#96400=CARTESIAN_POINT('Ctrl Pts',(-11.0867879837102,15.1917842916463,3.04613353470317));
#96401=CARTESIAN_POINT('Ctrl Pts',(-11.0842999670474,15.1913494933342,3.04021552567359));
#96402=CARTESIAN_POINT('Ctrl Pts',(-11.0828808167649,15.1911051043933,3.03688303968229));
#96403=CARTESIAN_POINT('Ctrl Pts',(-11.0790991015843,15.1904631606693,3.02811514582162));
#96404=CARTESIAN_POINT('Ctrl Pts',(-11.0767108082343,15.1900670903676,3.02269084895906));
#96405=CARTESIAN_POINT('Ctrl Pts',(-11.0577517766247,15.186992851637,2.98049757709027));
#96406=CARTESIAN_POINT('Ctrl Pts',(-11.0393412493931,15.1844148917533,2.94457932968132));
#96407=CARTESIAN_POINT('Ctrl Pts',(-10.970505839098,15.1757855565023,2.8257440998208));
#96408=CARTESIAN_POINT('Ctrl Pts',(-10.9117102467698,15.1699440992857,2.74814376419847));
#96409=CARTESIAN_POINT('Ctrl Pts',(-10.8296294692402,15.1624334948981,2.66379523812977));
#96410=CARTESIAN_POINT('Ctrl Pts',(-10.8148068776277,15.1610998030292,2.64934546605115));
#96411=CARTESIAN_POINT('Ctrl Pts',(-10.7919360972944,15.1590685768218,2.62819636412402));
#96412=CARTESIAN_POINT('Ctrl Pts',(-10.7841663285791,15.1583829389213,2.62120109255491));
#96413=CARTESIAN_POINT('Ctrl Pts',(-10.7697377617936,15.1571168901355,2.608554491469));
#96414=CARTESIAN_POINT('Ctrl Pts',(-10.7631072063315,15.1565377883769,2.60287197042473));
#96415=CARTESIAN_POINT('Ctrl Pts',(-10.7523154979748,15.1555992184905,2.59382945952206));
#96416=CARTESIAN_POINT('Ctrl Pts',(-10.7481934929498,15.1552416351816,2.59042309152715));
#96417=CARTESIAN_POINT('Ctrl Pts',(-10.7403779595496,15.1545652683916,2.58405351627686));
#96418=CARTESIAN_POINT('Ctrl Pts',(-10.736689468107,15.1542467353907,2.58108427454734));
#96419=CARTESIAN_POINT('Ctrl Pts',(-10.7280779298954,15.153504550736,2.57423714468381));
#96420=CARTESIAN_POINT('Ctrl Pts',(-10.723141674674,15.15308024196,2.57037617715715));
#96421=CARTESIAN_POINT('Ctrl Pts',(-10.7103796434105,15.1519859748301,2.56055731330556));
#96422=CARTESIAN_POINT('Ctrl Pts',(-10.7025097546642,15.1513137743737,2.55465782187964));
#96423=CARTESIAN_POINT('Ctrl Pts',(-10.6440044194409,15.1463343595559,2.51193457949146));
#96424=CARTESIAN_POINT('Ctrl Pts',(-10.5905866073816,15.1418766655007,2.47910818689937));
#96425=CARTESIAN_POINT('Ctrl Pts',(-10.4678597453528,15.1318586558835,2.41655592939871));
#96426=CARTESIAN_POINT('Ctrl Pts',(-10.3977866085547,15.1262758118892,2.38891520076487));
#96427=CARTESIAN_POINT('Ctrl Pts',(-10.2983712036894,15.1188237831731,2.36032023452068));
#96428=CARTESIAN_POINT('Ctrl Pts',(-10.2709086493638,15.1168138484527,2.35348172774307));
#96429=CARTESIAN_POINT('Ctrl Pts',(-10.2375855139173,15.1144530957466,2.34644835608135));
#96430=CARTESIAN_POINT('Ctrl Pts',(-10.2319382004814,15.1140556933246,2.34529962926442));
#96431=CARTESIAN_POINT('Ctrl Pts',(-10.2231135140134,15.1134391061994,2.34357194343144));
#96432=CARTESIAN_POINT('Ctrl Pts',(-10.2199419015342,15.1132183890078,2.34296454214207));
#96433=CARTESIAN_POINT('Ctrl Pts',(-10.2140146625963,15.1128076066233,2.34185465845969));
#96434=CARTESIAN_POINT('Ctrl Pts',(-10.2112597624101,15.1126173722187,2.34134896497963));
#96435=CARTESIAN_POINT('Ctrl Pts',(-10.2049652466684,15.112184265859,2.34021673112485));
#96436=CARTESIAN_POINT('Ctrl Pts',(-10.2014245459301,15.1119417526786,2.33959656314632));
#96437=CARTESIAN_POINT('Ctrl Pts',(-10.1920015758282,15.1112991647921,2.33799052103239));
#96438=CARTESIAN_POINT('Ctrl Pts',(-10.1861144706314,15.1109006174054,2.33703308653611));
#96439=CARTESIAN_POINT('Ctrl Pts',(-10.1392815540829,15.1077514198969,2.32978127344454));
#96440=CARTESIAN_POINT('Ctrl Pts',(-10.0980318741861,15.1051065180071,2.32560577691198));
#96441=CARTESIAN_POINT('Ctrl Pts',(-9.974492121498,15.0973427768696,2.31965729954626));
#96442=CARTESIAN_POINT('Ctrl Pts',(-9.89219890068557,15.0923631211769,2.32431977326732));
#96443=CARTESIAN_POINT('Ctrl Pts',(-9.81110406371068,15.0871826612189,2.3374969300026));
#96444=CARTESIAN_POINT('Ctrl Pts',(-9.81110406371068,14.9873061497326,2.3374969300026));
#96445=CARTESIAN_POINT('Ctrl Pts',(-9.85382366066147,14.9900172221248,2.33055539283837));
#96446=CARTESIAN_POINT('Ctrl Pts',(-9.89691233808748,14.9927689462918,2.32597078310509));
#96447=CARTESIAN_POINT('Ctrl Pts',(-9.95524335233313,14.9965779852906,2.32300403118289));
#96448=CARTESIAN_POINT('Ctrl Pts',(-9.97032322240293,14.9975700414155,2.32252731531612));
#96449=CARTESIAN_POINT('Ctrl Pts',(-9.99206440473281,14.9990127471275,2.32225791899193));
#96450=CARTESIAN_POINT('Ctrl Pts',(-9.99872172368918,14.9994561887225,2.32223187935902));
#96451=CARTESIAN_POINT('Ctrl Pts',(-10.0104314715965,15.0002392741427,2.32228535841672));
#96452=CARTESIAN_POINT('Ctrl Pts',(-10.0154838812806,15.0005781684674,2.32234094889161));
#96453=CARTESIAN_POINT('Ctrl Pts',(-10.0259166256504,15.0012801231873,2.32252288596704));
#96454=CARTESIAN_POINT('Ctrl Pts',(-10.0312967558706,15.0016433112713,2.32265360366425));
#96455=CARTESIAN_POINT('Ctrl Pts',(-10.0451024508674,15.0025784259567,2.32308372852481));
#96456=CARTESIAN_POINT('Ctrl Pts',(-10.0535259180664,15.0031520001999,2.32343673744501));
#96457=CARTESIAN_POINT('Ctrl Pts',(-10.0893160365843,15.0056023608956,2.32532175580102));
#96458=CARTESIAN_POINT('Ctrl Pts',(-10.11662656937,15.007505599446,2.32771831074809));
#96459=CARTESIAN_POINT('Ctrl Pts',(-10.24268799486,15.0164528770807,2.3432290209597));
#96460=CARTESIAN_POINT('Ctrl Pts',(-10.3395969898255,15.0238420411843,2.3678849584096));
#96461=CARTESIAN_POINT('Ctrl Pts',(-10.4527630746817,15.0327096782441,2.41253133482747));
#96462=CARTESIAN_POINT('Ctrl Pts',(-10.4730696612519,15.0343086433027,2.42121008141764));
#96463=CARTESIAN_POINT('Ctrl Pts',(-10.5130598745858,15.0374588522303,2.43964784663435));
#96464=CARTESIAN_POINT('Ctrl Pts',(-10.5327392455676,15.0390097340415,2.44939723410744));
#96465=CARTESIAN_POINT('Ctrl Pts',(-10.5570156841951,15.0409137689563,2.46228177757084));
#96466=CARTESIAN_POINT('Ctrl Pts',(-10.561877240778,15.0412945955104,2.46490601832155));
#96467=CARTESIAN_POINT('Ctrl Pts',(-10.5695328867124,15.041893335113,2.46910832389682));
#96468=CARTESIAN_POINT('Ctrl Pts',(-10.5723392251657,15.0421126100963,2.47066372410792));
#96469=CARTESIAN_POINT('Ctrl Pts',(-10.5773402922241,15.0425029561764,2.47346231858933));
#96470=CARTESIAN_POINT('Ctrl Pts',(-10.5795373725677,15.0426742954003,2.4747010882871));
#96471=CARTESIAN_POINT('Ctrl Pts',(-10.584798991138,15.043084285936,2.47769003900725));
#96472=CARTESIAN_POINT('Ctrl Pts',(-10.5878596601965,15.0433225060838,2.47944694546925));
#96473=CARTESIAN_POINT('Ctrl Pts',(-10.5971475350763,15.0440447275684,2.48483408293118));
#96474=CARTESIAN_POINT('Ctrl Pts',(-10.6033494957051,15.0445260563251,2.48850782984524));
#96475=CARTESIAN_POINT('Ctrl Pts',(-10.6671563875382,15.0494725565345,2.52709971393274));
#96476=CARTESIAN_POINT('Ctrl Pts',(-10.7217073613132,15.053658770948,2.56684736044128));
#96477=CARTESIAN_POINT('Ctrl Pts',(-10.8408497092787,15.0634261184581,2.67039100710969));
#96478=CARTESIAN_POINT('Ctrl Pts',(-10.9020601655457,15.068980379451,2.73739620740219));
#96479=CARTESIAN_POINT('Ctrl Pts',(-10.9635536025526,15.0758382424028,2.82259813766731));
#96480=CARTESIAN_POINT('Ctrl Pts',(-10.9718882924676,15.076800183266,2.83461143368669));
#96481=CARTESIAN_POINT('Ctrl Pts',(-10.9836436743103,15.0782068850301,2.85224741145965));
#96482=CARTESIAN_POINT('Ctrl Pts',(-10.9872445049607,15.0786449381334,2.85774881981766));
#96483=CARTESIAN_POINT('Ctrl Pts',(-10.9935234281681,15.079421754592,2.86751944262066));
#96484=CARTESIAN_POINT('Ctrl Pts',(-10.996220559926,15.0797598060807,2.87177627200917));
#96485=CARTESIAN_POINT('Ctrl Pts',(-11.0017591927968,15.0804632270825,2.88064314977036));
#96486=CARTESIAN_POINT('Ctrl Pts',(-11.0045963776939,15.0808287439061,2.88525574056514));
#96487=CARTESIAN_POINT('Ctrl Pts',(-11.0118490657507,15.0817767690765,2.89723119040767));
#96488=CARTESIAN_POINT('Ctrl Pts',(-11.0162159855994,15.082361013878,2.90462294846806));
#96489=CARTESIAN_POINT('Ctrl Pts',(-11.0349269406528,15.0849245555859,2.9371000929038));
#96490=CARTESIAN_POINT('Ctrl Pts',(-11.0484247057341,15.0869334516445,2.962658896209));
#96491=CARTESIAN_POINT('Ctrl Pts',(-11.103740418389,15.0959250991095,3.07743815501205));
#96492=CARTESIAN_POINT('Ctrl Pts',(-11.1352028175276,15.103236849838,3.17119853312383));
#96493=CARTESIAN_POINT('Ctrl Pts',(-11.1628179518424,15.1134404830624,3.30849067507048));
#96494=CARTESIAN_POINT('Ctrl Pts',(-11.1688508492515,15.1164299244796,3.34963413837847));
#96495=CARTESIAN_POINT('Ctrl Pts',(-11.1732487382952,15.1197327678433,3.39695600462471));
#96496=CARTESIAN_POINT('Ctrl Pts',(-11.1737557553988,15.1201452955867,3.40290161033677));
#96497=CARTESIAN_POINT('Ctrl Pts',(-11.1744957784003,15.1208025605947,3.41243487661072));
#96498=CARTESIAN_POINT('Ctrl Pts',(-11.1747575758616,15.1210487939129,3.41602010278482));
#96499=CARTESIAN_POINT('Ctrl Pts',(-11.1751940944341,15.121485220909,3.42240010629715));
#96500=CARTESIAN_POINT('Ctrl Pts',(-11.1753752685559,15.1216757636012,3.42519437330717));
#96501=CARTESIAN_POINT('Ctrl Pts',(-11.1757437917784,15.1220846921656,3.43121037493215));
#96502=CARTESIAN_POINT('Ctrl Pts',(-11.1759278661915,15.122302896313,3.43443224443988));
#96503=CARTESIAN_POINT('Ctrl Pts',(-11.1764033998383,15.1229083221537,3.44340286621349));
#96504=CARTESIAN_POINT('Ctrl Pts',(-11.1766659664153,15.123293988316,3.44915315602665));
#96505=CARTESIAN_POINT('Ctrl Pts',(-11.1779658474826,15.1255562194959,3.48307758155231));
#96506=CARTESIAN_POINT('Ctrl Pts',(-11.178033495014,15.1273840473419,3.51128226157366));
#96507=CARTESIAN_POINT('Ctrl Pts',(-11.1745892818148,15.1339360561513,3.6140106429075));
#96508=CARTESIAN_POINT('Ctrl Pts',(-11.1650139715779,15.1384716896318,3.68815535785766));
#96509=CARTESIAN_POINT('Ctrl Pts',(-11.1344722447445,15.1470419270055,3.8226006253844));
#96510=CARTESIAN_POINT('Ctrl Pts',(-11.1155087412005,15.1510332579587,3.88306274652448));
#96511=CARTESIAN_POINT('Ctrl Pts',(-11.0880939317458,15.1558358038783,3.95082530759093));
#96512=CARTESIAN_POINT('Ctrl Pts',(-11.0842899718103,15.1564858062412,3.95989902120511));
#96513=CARTESIAN_POINT('Ctrl Pts',(-11.0778777571775,15.1575560401017,3.97467238703678));
#96514=CARTESIAN_POINT('Ctrl Pts',(-11.0753368433064,15.1579740044518,3.98040087978508));
#96515=CARTESIAN_POINT('Ctrl Pts',(-11.070692443946,15.1587273070269,3.99065019408407));
#96516=CARTESIAN_POINT('Ctrl Pts',(-11.0686057227055,15.1590620683366,3.99517848354624));
#96517=CARTESIAN_POINT('Ctrl Pts',(-11.0641005731521,15.1597771117106,4.00479377798365));
#96518=CARTESIAN_POINT('Ctrl Pts',(-11.0616742866537,15.1601576567807,4.00987694125349));
#96519=CARTESIAN_POINT('Ctrl Pts',(-11.055023989345,15.1611887226017,4.02355628111543));
#96520=CARTESIAN_POINT('Ctrl Pts',(-11.0507315026505,15.1618415919515,4.03211849947542));
#96521=CARTESIAN_POINT('Ctrl Pts',(-11.0275147145909,15.1653084914841,4.07705249852453));
#96522=CARTESIAN_POINT('Ctrl Pts',(-11.0068072664957,15.168184351883,4.11246591954439));
#96523=CARTESIAN_POINT('Ctrl Pts',(-10.9276709934895,15.1784874209678,4.23290929970419));
#96524=CARTESIAN_POINT('Ctrl Pts',(-10.8599792347659,15.186208086191,4.31127150756626));
#96525=CARTESIAN_POINT('Ctrl Pts',(-10.7647471084255,15.1953554618111,4.39601958719909));
#96526=CARTESIAN_POINT('Ctrl Pts',(-10.7460373822594,15.1970816742009,4.41165655036606));
#96527=CARTESIAN_POINT('Ctrl Pts',(-10.7223616923607,15.1991674893352,4.43022644975674));
#96528=CARTESIAN_POINT('Ctrl Pts',(-10.7178434352604,15.1995612679325,4.43371755267993));
#96529=CARTESIAN_POINT('Ctrl Pts',(-10.7107129941767,15.200175799264,4.43914464851306));
#96530=CARTESIAN_POINT('Ctrl Pts',(-10.708117952842,15.2003980321963,4.44110286177138));
#96531=CARTESIAN_POINT('Ctrl Pts',(-10.7032968348339,15.2008082306458,4.44470963647622));
#96532=CARTESIAN_POINT('Ctrl Pts',(-10.7010730639282,15.2009963879725,4.44636108035955));
#96533=CARTESIAN_POINT('Ctrl Pts',(-10.695942254151,15.2014281318097,4.45014337442574));
#96534=CARTESIAN_POINT('Ctrl Pts',(-10.6930312440266,15.2016713423006,4.45226873767299));
#96535=CARTESIAN_POINT('Ctrl Pts',(-10.6839565151991,15.2024242821144,4.45883065280589));
#96536=CARTESIAN_POINT('Ctrl Pts',(-10.6777594600841,15.2029309962893,4.46322108426798));
#96537=CARTESIAN_POINT('Ctrl Pts',(-10.6631446141224,15.2041097615554,4.47336438394347));
#96538=CARTESIAN_POINT('Ctrl Pts',(-10.6546936138136,15.2047789670157,4.47906858331985));
#96539=CARTESIAN_POINT('Ctrl Pts',(-10.6244392640184,15.2071350988749,4.49892252431281));
#96540=CARTESIAN_POINT('Ctrl Pts',(-10.6022416172956,15.2087919720935,4.51246028209265));
#96541=CARTESIAN_POINT('Ctrl Pts',(-10.5087269246475,15.2155577450496,4.56532752015965));
#96542=CARTESIAN_POINT('Ctrl Pts',(-10.4338753579854,15.2204889629681,4.59794303460385));
#96543=CARTESIAN_POINT('Ctrl Pts',(-10.3119283092016,15.2285285081471,4.63664355106482));
#96544=CARTESIAN_POINT('Ctrl Pts',(-10.2668119269487,15.2315007092127,4.64807162142226));
#96545=CARTESIAN_POINT('Ctrl Pts',(-10.2111430260604,15.2352290347448,4.65871364571938));
#96546=CARTESIAN_POINT('Ctrl Pts',(-10.2011202217855,15.2359025533648,4.66049529767797));
#96547=CARTESIAN_POINT('Ctrl Pts',(-10.1853290531485,15.2369678107395,4.66309162271102));
#96548=CARTESIAN_POINT('Ctrl Pts',(-10.1795754320136,15.2373567978227,4.66399383285021));
#96549=CARTESIAN_POINT('Ctrl Pts',(-10.1689476949566,15.2380769898298,4.66557966755463));
#96550=CARTESIAN_POINT('Ctrl Pts',(-10.1640755070351,15.238407804204,4.66627548708473));
#96551=CARTESIAN_POINT('Ctrl Pts',(-10.1532636382531,15.2391434198352,4.66775048955194));
#96552=CARTESIAN_POINT('Ctrl Pts',(-10.1473221182794,15.2395486732193,4.66851492922595));
#96553=CARTESIAN_POINT('Ctrl Pts',(-10.1302059099205,15.2407191472101,4.67058449442906));
#96554=CARTESIAN_POINT('Ctrl Pts',(-10.1190182746367,15.2414879163002,4.67177483868667));
#96555=CARTESIAN_POINT('Ctrl Pts',(-10.093755958055,15.2432327347495,4.67409719693852));
#96556=CARTESIAN_POINT('Ctrl Pts',(-10.0796747279584,15.2442115096691,4.67513672206575));
#96557=CARTESIAN_POINT('Ctrl Pts',(-10.0336997147781,15.2474281823065,4.67770065107144));
#96558=CARTESIAN_POINT('Ctrl Pts',(-10.0017642241214,15.2496959021146,4.67818125734417));
#96559=CARTESIAN_POINT('Ctrl Pts',(-9.91751246579765,15.2557605114777,4.67602380162299));
#96560=CARTESIAN_POINT('Ctrl Pts',(-9.86532477286585,15.2596029916686,4.67119514750037));
#96561=CARTESIAN_POINT('Ctrl Pts',(-9.75380805791747,15.2678955066511,4.65332380723034));
#96562=CARTESIAN_POINT('Ctrl Pts',(-9.69480362607636,15.2723346584006,4.63913254637539));
#96563=CARTESIAN_POINT('Ctrl Pts',(-9.62785761028928,15.2772658435852,4.617452673635));
#96564=CARTESIAN_POINT('Ctrl Pts',(-9.6186041099383,15.2779449110793,4.61432832981488));
#96565=CARTESIAN_POINT('Ctrl Pts',(-9.6058981758352,15.2788728206988,4.6098614849761));
#96566=CARTESIAN_POINT('Ctrl Pts',(-9.60241192341497,15.2791269479137,4.60861737580304));
#96567=CARTESIAN_POINT('Ctrl Pts',(-9.59644487348197,15.2795610299417,4.60645619750104));
#96568=CARTESIAN_POINT('Ctrl Pts',(-9.59396122058463,15.2797414443404,4.60554717994859));
#96569=CARTESIAN_POINT('Ctrl Pts',(-9.5887824610702,15.2801170532314,4.60363194677012));
#96570=CARTESIAN_POINT('Ctrl Pts',(-9.58608795269781,15.2803121496529,4.60262421322578));
#96571=CARTESIAN_POINT('Ctrl Pts',(-9.57952138450873,15.2807868497534,4.60014088472318));
#96572=CARTESIAN_POINT('Ctrl Pts',(-9.57565331811511,15.2810658333237,4.59865468969866));
#96573=CARTESIAN_POINT('Ctrl Pts',(-9.56177421135269,15.2820648312136,4.59323780082984));
#96574=CARTESIAN_POINT('Ctrl Pts',(-9.55180891105699,15.2827783082046,4.58919029514864));
#96575=CARTESIAN_POINT('Ctrl Pts',(-9.52706848874539,15.2845434299411,4.57874465719054));
#96576=CARTESIAN_POINT('Ctrl Pts',(-9.51236612842047,15.2855867933907,4.57217886147675));
#96577=CARTESIAN_POINT('Ctrl Pts',(-9.44858127803158,15.2901082329093,4.5421101431506));
#96578=CARTESIAN_POINT('Ctrl Pts',(-9.40102353283894,15.2934681983367,4.51552168333167));
#96579=CARTESIAN_POINT('Ctrl Pts',(-9.28722433921445,15.3018731321247,4.4411136783521));
#96580=CARTESIAN_POINT('Ctrl Pts',(-9.22380397606758,15.3069138439129,4.3895289294965));
#96581=CARTESIAN_POINT('Ctrl Pts',(-9.15560716399373,15.3132116203702,4.32117093782908));
#96582=CARTESIAN_POINT('Ctrl Pts',(-9.14519680747071,15.3142000342822,4.31032859953318));
#96583=CARTESIAN_POINT('Ctrl Pts',(-9.13048577262265,15.3156383903409,4.29440811939364));
#96584=CARTESIAN_POINT('Ctrl Pts',(-9.12601588323514,15.3160811859421,4.2894878164768));
#96585=CARTESIAN_POINT('Ctrl Pts',(-9.11822329559463,15.3168635173597,4.28076271659858));
#96586=CARTESIAN_POINT('Ctrl Pts',(-9.11488294540117,15.3172023082004,4.2769738569345));
#96587=CARTESIAN_POINT('Ctrl Pts',(-9.10803159084474,15.3179044264327,4.26910104956554));
#96588=CARTESIAN_POINT('Ctrl Pts',(-9.10452402639036,15.3182678838146,4.26501427855584));
#96589=CARTESIAN_POINT('Ctrl Pts',(-9.09558624507283,15.3192044935746,4.25445490460956));
#96590=CARTESIAN_POINT('Ctrl Pts',(-9.09019750214581,15.3197793037959,4.2479477599469));
#96591=CARTESIAN_POINT('Ctrl Pts',(-9.06751961445727,15.3222424866097,4.21995548941208));
#96592=CARTESIAN_POINT('Ctrl Pts',(-9.05091920904114,15.3241576581896,4.19792621982383));
#96593=CARTESIAN_POINT('Ctrl Pts',(-8.97806526624932,15.3331096812273,4.09383559929586));
#96594=CARTESIAN_POINT('Ctrl Pts',(-8.93158424697668,15.3404897974257,4.00544353385562));
#96595=CARTESIAN_POINT('Ctrl Pts',(-8.88903661479931,15.3493488933348,3.8915910043721));
#96596=CARTESIAN_POINT('Ctrl Pts',(-8.88188618651963,15.3509488256291,3.87068146944805));
#96597=CARTESIAN_POINT('Ctrl Pts',(-8.86883496738365,15.3540939664585,3.82869323054041));
#96598=CARTESIAN_POINT('Ctrl Pts',(-8.86292474037613,15.3556389861618,3.80762570546016));
#96599=CARTESIAN_POINT('Ctrl Pts',(-8.8562626290168,15.3575368922542,3.78105218930253));
#96600=CARTESIAN_POINT('Ctrl Pts',(-8.85495844701473,15.3579172458359,3.77569068143855));
#96601=CARTESIAN_POINT('Ctrl Pts',(-8.85295589799316,15.3585154082273,3.76719875557004));
#96602=CARTESIAN_POINT('Ctrl Pts',(-8.85223257515441,15.3587345747292,3.76407439484788));
#96603=CARTESIAN_POINT('Ctrl Pts',(-8.85096310927288,15.3591248290546,3.75848723262089));
#96604=CARTESIAN_POINT('Ctrl Pts',(-8.85041211922633,15.3592961842075,3.75602564371142));
#96605=CARTESIAN_POINT('Ctrl Pts',(-8.84910876155452,15.3597063430142,3.75011375363553));
#96606=CARTESIAN_POINT('Ctrl Pts',(-8.84836399836514,15.3599447144712,3.74666181918884));
#96607=CARTESIAN_POINT('Ctrl Pts',(-8.84614391539979,15.3606678565961,3.73614258505591));
#96608=CARTESIAN_POINT('Ctrl Pts',(-8.84471800840283,15.3611499447194,3.72906486154128));
#96609=CARTESIAN_POINT('Ctrl Pts',(-8.83246109930156,15.3654636652005,3.66519770173727));
#96610=CARTESIAN_POINT('Ctrl Pts',(-8.82575868397126,15.3690906547556,3.6076874457981));
#96611=CARTESIAN_POINT('Ctrl Pts',(-8.81899614360149,15.3789955432675,3.44825322757513));
#96612=CARTESIAN_POINT('Ctrl Pts',(-8.82787510282304,15.3851897204474,3.34647792598946));
#96613=CARTESIAN_POINT('Ctrl Pts',(-8.85261521884932,15.3927242297761,3.23394554978417));
#96614=CARTESIAN_POINT('Ctrl Pts',(-8.85573568233757,15.3936124154542,3.22082988437279));
#96615=CARTESIAN_POINT('Ctrl Pts',(-8.86067726530692,15.3949351315317,3.20153696575602));
#96616=CARTESIAN_POINT('Ctrl Pts',(-8.86232508386034,15.395364138175,3.19531613266589));
#96617=CARTESIAN_POINT('Ctrl Pts',(-8.86534475325112,15.3961296649969,3.18428244223013));
#96618=CARTESIAN_POINT('Ctrl Pts',(-8.86669646427889,15.3964655309349,3.17946419879257));
#96619=CARTESIAN_POINT('Ctrl Pts',(-8.86960757792984,15.3971749230406,3.16933603037875));
#96620=CARTESIAN_POINT('Ctrl Pts',(-8.87117377844989,15.3975486616852,3.16402820295518));
#96621=CARTESIAN_POINT('Ctrl Pts',(-8.87542227618869,15.398542095509,3.14999524735485));
#96622=CARTESIAN_POINT('Ctrl Pts',(-8.87816865637252,15.3991638528738,3.14129007255412));
#96623=CARTESIAN_POINT('Ctrl Pts',(-8.89189402573273,15.4021769843532,3.09948490361637));
#96624=CARTESIAN_POINT('Ctrl Pts',(-8.90423729056878,15.404612388616,3.06685471310826));
#96625=CARTESIAN_POINT('Ctrl Pts',(-8.94466030829147,15.411883809643,2.97283170958428));
#96626=CARTESIAN_POINT('Ctrl Pts',(-8.97658751685163,15.4168293435335,2.91325195648752));
#96627=CARTESIAN_POINT('Ctrl Pts',(-9.04646018834736,15.4262224733724,2.80608851643903));
#96628=CARTESIAN_POINT('Ctrl Pts',(-9.08334109605991,15.4306522382477,2.75805035471875));
#96629=CARTESIAN_POINT('Ctrl Pts',(-9.13028117129571,15.4355752078499,2.70578359192119));
#96630=CARTESIAN_POINT('Ctrl Pts',(-9.13690073450279,15.4362546647628,2.69859484819586));
#96631=CARTESIAN_POINT('Ctrl Pts',(-9.14615078526604,15.4371830060588,2.68879701225992));
#96632=CARTESIAN_POINT('Ctrl Pts',(-9.14870502622069,15.4374371820127,2.6861169387618));
#96633=CARTESIAN_POINT('Ctrl Pts',(-9.15310566781629,15.4378713255455,2.68154288553122));
#96634=CARTESIAN_POINT('Ctrl Pts',(-9.15494586878972,15.43805175299,2.67964302051611));
#96635=CARTESIAN_POINT('Ctrl Pts',(-9.15880078804323,15.4384273644047,2.67568985015263));
#96636=CARTESIAN_POINT('Ctrl Pts',(-9.16081664823704,15.4386224504282,2.67363770675323));
#96637=CARTESIAN_POINT('Ctrl Pts',(-9.16575400781213,15.4390970849753,2.66864817916817));
#96638=CARTESIAN_POINT('Ctrl Pts',(-9.16868356350469,15.4393760137984,2.66571874694888));
#96639=CARTESIAN_POINT('Ctrl Pts',(-9.1792697581953,15.4403745943019,2.65524412764747));
#96640=CARTESIAN_POINT('Ctrl Pts',(-9.18701443329813,15.4410877158351,2.64778811188352));
#96641=CARTESIAN_POINT('Ctrl Pts',(-9.20660223167084,15.4428517799165,2.62944048014546));
#96642=CARTESIAN_POINT('Ctrl Pts',(-9.21856876661526,15.4438944539055,2.61868327047147));
#96643=CARTESIAN_POINT('Ctrl Pts',(-9.27190674756109,15.4484109718669,2.57267641565309));
#96644=CARTESIAN_POINT('Ctrl Pts',(-9.31547205575955,15.4517669665735,2.54006706179593));
#96645=CARTESIAN_POINT('Ctrl Pts',(-9.42971561267296,15.4601733496869,2.46630052507641));
#96646=CARTESIAN_POINT('Ctrl Pts',(-9.50270305363433,15.465219316615,2.42927477025493));
#96647=CARTESIAN_POINT('Ctrl Pts',(-9.59296155463226,15.4715228324607,2.39472149187044));
#96648=CARTESIAN_POINT('Ctrl Pts',(-9.60709642812175,15.4725110440725,2.3896182519908));
#96649=CARTESIAN_POINT('Ctrl Pts',(-9.62761857204557,15.473949158499,2.38264986839871));
#96650=CARTESIAN_POINT('Ctrl Pts',(-9.63393044806697,15.4743919181734,2.38056606958004));
#96651=CARTESIAN_POINT('Ctrl Pts',(-9.64506912951378,15.4751742076756,2.37699303104505));
#96652=CARTESIAN_POINT('Ctrl Pts',(-9.64988855125129,15.4755129927793,2.37548119302536));
#96653=CARTESIAN_POINT('Ctrl Pts',(-9.65986666577574,15.4762151201987,2.37242145077976));
#96654=CARTESIAN_POINT('Ctrl Pts',(-9.66502654106717,15.4765785926329,2.37087784103969));
#96655=CARTESIAN_POINT('Ctrl Pts',(-9.67830840056628,15.4775152859443,2.36700354151355));
#96656=CARTESIAN_POINT('Ctrl Pts',(-9.6864450910596,15.4780901652352,2.36472480310431));
#96657=CARTESIAN_POINT('Ctrl Pts',(-9.7212486712089,15.4805540667524,2.35538050302663));
#96658=CARTESIAN_POINT('Ctrl Pts',(-9.74813292105391,15.4824699074825,2.34916601961695));
#96659=CARTESIAN_POINT('Ctrl Pts',(-9.78714530463055,15.4852701831299,2.34158046861053));
#96660=CARTESIAN_POINT('Ctrl Pts',(-9.7991118959388,15.486131784317,2.33944554572489));
#96661=CARTESIAN_POINT('Ctrl Pts',(-9.81110406371067,15.4869977587645,2.3374969300026));
#96662=CARTESIAN_POINT('Origin',(-10.,12.3756328852638,3.5));
#96663=CARTESIAN_POINT('',(-9.81110382412687,16.0869811837922,2.33749696893276));
#96664=CARTESIAN_POINT('',(-9.81110406371106,15.9888353687451,2.33749693000254));
#96665=CARTESIAN_POINT('',(-9.81110406371068,12.3756328852638,2.3374969300026));
#96666=CARTESIAN_POINT('Ctrl Pts',(-9.81110382412688,16.0869811837922,2.33749696893276));
#96667=CARTESIAN_POINT('Ctrl Pts',(-9.71998275066426,16.0802638280491,2.35230331511729));
#96668=CARTESIAN_POINT('Ctrl Pts',(-9.63092842143902,16.0733690794726,2.3777681961223));
#96669=CARTESIAN_POINT('Ctrl Pts',(-9.53775860307175,16.0662516653844,2.41671656411454));
#96670=CARTESIAN_POINT('Ctrl Pts',(-9.52980263881095,16.0656449645949,2.42014604543945));
#96671=CARTESIAN_POINT('Ctrl Pts',(-9.51753861172157,16.0647121799927,2.42559379667557));
#96672=CARTESIAN_POINT('Ctrl Pts',(-9.51320389041452,16.0643829640415,2.42755082615761));
#96673=CARTESIAN_POINT('Ctrl Pts',(-9.50509866660381,16.0637684387193,2.43126942099416));
#96674=CARTESIAN_POINT('Ctrl Pts',(-9.50132542978528,16.0634827898069,2.43302481066971));
#96675=CARTESIAN_POINT('Ctrl Pts',(-9.49495592194608,16.0630014228457,2.43602921033503));
#96676=CARTESIAN_POINT('Ctrl Pts',(-9.49235480816932,16.0628050831729,2.43726780329201));
#96677=CARTESIAN_POINT('Ctrl Pts',(-9.4873769775607,16.0624298297448,2.43966058273671));
#96678=CARTESIAN_POINT('Ctrl Pts',(-9.48499957417099,16.0622508207162,2.44081323427598));
#96679=CARTESIAN_POINT('Ctrl Pts',(-9.47931185066821,16.061823017062,2.44359452672951));
#96680=CARTESIAN_POINT('Ctrl Pts',(-9.47600523892815,16.0615746836938,2.44523075315276));
#96681=CARTESIAN_POINT('Ctrl Pts',(-9.46406477850062,16.0606790909595,2.45120931630991));
#96682=CARTESIAN_POINT('Ctrl Pts',(-9.4554764814352,16.0600371317322,2.45564248821605));
#96683=CARTESIAN_POINT('Ctrl Pts',(-9.38655498868761,16.0548953857802,2.49230029977449));
#96684=CARTESIAN_POINT('Ctrl Pts',(-9.32907057330553,16.0506647259872,2.52962389580546));
#96685=CARTESIAN_POINT('Ctrl Pts',(-9.2373201360961,16.0434671706792,2.60126885869721));
#96686=CARTESIAN_POINT('Ctrl Pts',(-9.2013364172409,16.040507731606,2.6330891264525));
#96687=CARTESIAN_POINT('Ctrl Pts',(-9.14624599267034,16.0356053192525,2.68815435488495));
#96688=CARTESIAN_POINT('Ctrl Pts',(-9.12591059438921,16.0337019704557,2.71009065824297));
#96689=CARTESIAN_POINT('Ctrl Pts',(-9.09347048028087,16.0304785568442,2.74787285724886));
#96690=CARTESIAN_POINT('Ctrl Pts',(-9.08089336842273,16.0291769838373,2.76329521961175));
#96691=CARTESIAN_POINT('Ctrl Pts',(-9.06430026014541,16.0273826882613,2.78472869942786));
#96692=CARTESIAN_POINT('Ctrl Pts',(-9.05993952838316,16.0269034756245,2.79046963248325));
#96693=CARTESIAN_POINT('Ctrl Pts',(-9.05284819493209,16.0261112245714,2.79998555528696));
#96694=CARTESIAN_POINT('Ctrl Pts',(-9.0500867545275,16.0257993846198,2.80373741328203));
#96695=CARTESIAN_POINT('Ctrl Pts',(-9.04438036225703,16.0251479316422,2.81158759536892));
#96696=CARTESIAN_POINT('Ctrl Pts',(-9.04143935380294,16.0248081765118,2.81568865486148));
#96697=CARTESIAN_POINT('Ctrl Pts',(-9.03470628789245,16.0240209447511,2.8252060849612));
#96698=CARTESIAN_POINT('Ctrl Pts',(-9.03093333321431,16.0235727572941,2.83063569662474));
#96699=CARTESIAN_POINT('Ctrl Pts',(-9.01885230257836,16.0221143246272,2.84833759634299));
#96700=CARTESIAN_POINT('Ctrl Pts',(-9.01073038195427,16.0210972056754,2.86073457747773));
#96701=CARTESIAN_POINT('Ctrl Pts',(-8.95549232020234,16.0139125633871,2.94862232384264));
#96702=CARTESIAN_POINT('Ctrl Pts',(-8.91683969518205,16.0074363066258,3.02907373728262));
#96703=CARTESIAN_POINT('Ctrl Pts',(-8.87155694883815,15.9973144032274,3.15926365353578));
#96704=CARTESIAN_POINT('Ctrl Pts',(-8.85838639747998,15.9937244479054,3.20639496989813));
#96705=CARTESIAN_POINT('Ctrl Pts',(-8.84501920029073,15.9891402766251,3.26903632565814));
#96706=CARTESIAN_POINT('Ctrl Pts',(-8.84214191792509,15.9880646452468,3.28392229407242));
#96707=CARTESIAN_POINT('Ctrl Pts',(-8.83782696231029,15.9862929198105,3.30881683654593));
#96708=CARTESIAN_POINT('Ctrl Pts',(-8.8362293526486,15.9855899503777,3.31879550490512));
#96709=CARTESIAN_POINT('Ctrl Pts',(-8.83415730792606,15.9846077453011,3.33289797487026));
#96710=CARTESIAN_POINT('Ctrl Pts',(-8.83357598155575,15.9843230255583,3.33700527623731));
#96711=CARTESIAN_POINT('Ctrl Pts',(-8.8326280595956,15.983842764384,3.34396763193602));
#96712=CARTESIAN_POINT('Ctrl Pts',(-8.8322502111005,15.9836466078098,3.34682109045668));
#96713=CARTESIAN_POINT('Ctrl Pts',(-8.83154521964688,15.9832713413337,3.35229934047037));
#96714=CARTESIAN_POINT('Ctrl Pts',(-8.83121645414841,15.98309213829,3.35492387565429));
#96715=CARTESIAN_POINT('Ctrl Pts',(-8.83044896384256,15.9826633968753,3.36122273571014));
#96716=CARTESIAN_POINT('Ctrl Pts',(-8.83001870488549,15.9824143243031,3.3648980930338));
#96717=CARTESIAN_POINT('Ctrl Pts',(-8.82851771953156,15.9815122518474,3.37826503997729));
#96718=CARTESIAN_POINT('Ctrl Pts',(-8.82754999725294,15.9808646559533,3.3879681284794));
#96719=CARTESIAN_POINT('Ctrl Pts',(-8.82138590023867,15.9761922004064,3.45865317726463));
#96720=CARTESIAN_POINT('Ctrl Pts',(-8.82082885873209,15.9723814409384,3.51995407413669));
#96721=CARTESIAN_POINT('Ctrl Pts',(-8.82964564142442,15.9644475499155,3.64780426985037));
#96722=CARTESIAN_POINT('Ctrl Pts',(-8.83993457777486,15.9603393754895,3.71406312086657));
#96723=CARTESIAN_POINT('Ctrl Pts',(-8.86402268495667,15.9538771608337,3.81281967166299));
#96724=CARTESIAN_POINT('Ctrl Pts',(-8.87373731125307,15.9516353703548,3.84616845761532));
#96725=CARTESIAN_POINT('Ctrl Pts',(-8.88784427563159,15.9487446499486,3.88766975427016));
#96726=CARTESIAN_POINT('Ctrl Pts',(-8.89087869084375,15.9481402248224,3.89626772195071));
#96727=CARTESIAN_POINT('Ctrl Pts',(-8.89591442867788,15.9471637381456,3.91002527726144));
#96728=CARTESIAN_POINT('Ctrl Pts',(-8.89785286294132,15.9467937538902,3.9152076146846));
#96729=CARTESIAN_POINT('Ctrl Pts',(-8.90161476020985,15.9460866635381,3.92505293139028));
#96730=CARTESIAN_POINT('Ctrl Pts',(-8.90343158672009,15.9457497842992,3.92971832999723));
#96731=CARTESIAN_POINT('Ctrl Pts',(-8.90765445430549,15.9449770773057,3.94036097347338));
#96732=CARTESIAN_POINT('Ctrl Pts',(-8.91007989267944,15.9445406094011,3.94633029804));
#96733=CARTESIAN_POINT('Ctrl Pts',(-8.91774450894765,15.9431834343641,3.96475885494576));
#96734=CARTESIAN_POINT('Ctrl Pts',(-8.92314910985567,15.9422572086239,3.97714764493938));
#96735=CARTESIAN_POINT('Ctrl Pts',(-8.97094580219988,15.9343142031851,4.08175993414274));
#96736=CARTESIAN_POINT('Ctrl Pts',(-9.02487578376481,15.9268798897526,4.16822256572122));
#96737=CARTESIAN_POINT('Ctrl Pts',(-9.12597641048341,15.9151813967729,4.29154465538999));
#96738=CARTESIAN_POINT('Ctrl Pts',(-9.16602278442699,15.9109515826147,4.33363288211195));
#96739=CARTESIAN_POINT('Ctrl Pts',(-9.21436700924182,15.9064093279908,4.37745546452834));
#96740=CARTESIAN_POINT('Ctrl Pts',(-9.21976607901131,15.9059093567241,4.38225978232027));
#96741=CARTESIAN_POINT('Ctrl Pts',(-9.2278703712304,15.9051701055201,4.3893387340985));
#96742=CARTESIAN_POINT('Ctrl Pts',(-9.23054203712947,15.9049281922815,4.39165127252324));
#96743=CARTESIAN_POINT('Ctrl Pts',(-9.23513951749828,15.9045150158027,4.39559470339104));
#96744=CARTESIAN_POINT('Ctrl Pts',(-9.23706020547129,15.904343328837,4.39723146445229));
#96745=CARTESIAN_POINT('Ctrl Pts',(-9.24143416611643,15.9039544539304,4.40093464035289));
#96746=CARTESIAN_POINT('Ctrl Pts',(-9.2438906285,15.903737544337,4.40299721454425));
#96747=CARTESIAN_POINT('Ctrl Pts',(-9.25059525372561,15.9031494476794,4.40858022666024));
#96748=CARTESIAN_POINT('Ctrl Pts',(-9.25485984274685,15.9027796417248,4.41208094543831));
#96749=CARTESIAN_POINT('Ctrl Pts',(-9.27613889256795,15.9009545404701,4.4292996417067));
#96750=CARTESIAN_POINT('Ctrl Pts',(-9.29350953197979,15.8995279219435,4.44257312359106));
#96751=CARTESIAN_POINT('Ctrl Pts',(-9.3291498482908,15.8967026534067,4.46826782092348));
#96752=CARTESIAN_POINT('Ctrl Pts',(-9.34741928345548,15.8953049985431,4.48067375052159));
#96753=CARTESIAN_POINT('Ctrl Pts',(-9.44988778413838,15.8876776012046,4.54612294421872));
#96754=CARTESIAN_POINT('Ctrl Pts',(-9.54019460628715,15.8816846086777,4.58884165819584));
#96755=CARTESIAN_POINT('Ctrl Pts',(-9.6610116058061,15.8735400296484,4.62824736939657));
#96756=CARTESIAN_POINT('Ctrl Pts',(-9.68751452588286,15.8717490354282,4.63587318634894));
#96757=CARTESIAN_POINT('Ctrl Pts',(-9.72245647253351,15.8693700689526,4.64461174801248));
#96758=CARTESIAN_POINT('Ctrl Pts',(-9.73067555305444,15.8688092512808,4.64657350371413));
#96759=CARTESIAN_POINT('Ctrl Pts',(-9.74416791600781,15.8678862791553,4.6496408256885));
#96760=CARTESIAN_POINT('Ctrl Pts',(-9.74942903135062,15.8675258034306,4.65079897085346));
#96761=CARTESIAN_POINT('Ctrl Pts',(-9.75964001936648,15.8668249723267,4.6529734060432));
#96762=CARTESIAN_POINT('Ctrl Pts',(-9.76458885943727,15.8664847624602,4.65399401595487));
#96763=CARTESIAN_POINT('Ctrl Pts',(-9.77606627986435,15.8656944051191,4.65628412797902));
#96764=CARTESIAN_POINT('Ctrl Pts',(-9.78259929879314,15.8652435290264,4.65753022750587));
#96765=CARTESIAN_POINT('Ctrl Pts',(-9.80394076442455,15.8637671911042,4.66141382886268));
#96766=CARTESIAN_POINT('Ctrl Pts',(-9.8187887235298,15.8627346180929,4.66382289999578));
#96767=CARTESIAN_POINT('Ctrl Pts',(-9.91405450019217,15.8560718427049,4.67741252316573));
#96768=CARTESIAN_POINT('Ctrl Pts',(-9.99538651645026,15.8501898026005,4.68053422357338));
#96769=CARTESIAN_POINT('Ctrl Pts',(-10.1309447336209,15.8402205057052,4.6717246587711));
#96770=CARTESIAN_POINT('Ctrl Pts',(-10.1852010487014,15.8361917886511,4.66438238714015));
#96771=CARTESIAN_POINT('Ctrl Pts',(-10.2545610959831,15.8311131453877,4.65002361639674));
#96772=CARTESIAN_POINT('Ctrl Pts',(-10.2703011483669,15.8299658153285,4.64642619217887));
#96773=CARTESIAN_POINT('Ctrl Pts',(-10.2964180611546,15.8280759243388,4.63988927114941));
#96774=CARTESIAN_POINT('Ctrl Pts',(-10.306837128272,15.8273256929406,4.63712893503009));
#96775=CARTESIAN_POINT('Ctrl Pts',(-10.3212119147047,15.8262971469425,4.6331086327221));
#96776=CARTESIAN_POINT('Ctrl Pts',(-10.3252006886351,15.8260124420374,4.63197030929356));
#96777=CARTESIAN_POINT('Ctrl Pts',(-10.3319469896852,15.8255321985119,4.63000643490599));
#96778=CARTESIAN_POINT('Ctrl Pts',(-10.3347076322705,15.8253360448523,4.6291918120791));
#96779=CARTESIAN_POINT('Ctrl Pts',(-10.3399994678797,15.8249607781266,4.62760916130065));
#96780=CARTESIAN_POINT('Ctrl Pts',(-10.3425310860537,15.8247815719529,4.62684271939236));
#96781=CARTESIAN_POINT('Ctrl Pts',(-10.3485982968419,15.8243528154349,4.62498354833706));
#96782=CARTESIAN_POINT('Ctrl Pts',(-10.3521313912093,15.8241037309626,4.62388266328753));
#96783=CARTESIAN_POINT('Ctrl Pts',(-10.3649558881408,15.8232015526282,4.61982023610184));
#96784=CARTESIAN_POINT('Ctrl Pts',(-10.3742159179805,15.822553864465,4.61675987725334));
#96785=CARTESIAN_POINT('Ctrl Pts',(-10.4422222015541,15.8178174470215,4.59334348108205));
#96786=CARTESIAN_POINT('Ctrl Pts',(-10.4993203726699,15.8139498119805,4.56847633383445));
#96787=CARTESIAN_POINT('Ctrl Pts',(-10.612612972518,15.8060028955478,4.50805939417687));
#96788=CARTESIAN_POINT('Ctrl Pts',(-10.6682975163286,15.8019370827577,4.47203713412819));
#96789=CARTESIAN_POINT('Ctrl Pts',(-10.7479553126756,15.7955331295536,4.41041140204768));
#96790=CARTESIAN_POINT('Ctrl Pts',(-10.7743077107265,15.7933045105246,4.38810657223371));
#96791=CARTESIAN_POINT('Ctrl Pts',(-10.8063224276096,15.7904286617853,4.35849986703975));
#96792=CARTESIAN_POINT('Ctrl Pts',(-10.8129317135178,15.7898253639941,4.35224403807633));
#96793=CARTESIAN_POINT('Ctrl Pts',(-10.8234390306121,15.7888502623246,4.34206519805909));
#96794=CARTESIAN_POINT('Ctrl Pts',(-10.8273831711333,15.7884805250204,4.33819014624981));
#96795=CARTESIAN_POINT('Ctrl Pts',(-10.8348470614639,15.787773618958,4.3307529851347));
#96796=CARTESIAN_POINT('Ctrl Pts',(-10.8383716738139,15.787436675053,4.32719591002215));
#96797=CARTESIAN_POINT('Ctrl Pts',(-10.8463843401985,15.7866634108876,4.31900562852991));
#96798=CARTESIAN_POINT('Ctrl Pts',(-10.8508571959665,15.78622644718,4.31435784523298));
#96799=CARTESIAN_POINT('Ctrl Pts',(-10.8646094431631,15.7848661739024,4.2998307807205));
#96800=CARTESIAN_POINT('Ctrl Pts',(-10.8737563565465,15.7839373093408,4.28982818997498));
#96801=CARTESIAN_POINT('Ctrl Pts',(-10.9497232832532,15.7760117740848,4.20381984382201));
#96802=CARTESIAN_POINT('Ctrl Pts',(-11.0066499632571,15.7686004130611,4.11966449275862));
#96803=CARTESIAN_POINT('Ctrl Pts',(-11.0782853583566,15.7569064498529,3.97727084799873));
#96804=CARTESIAN_POINT('Ctrl Pts',(-11.1005667522556,15.7526592161766,3.92336888561802));
#96805=CARTESIAN_POINT('Ctrl Pts',(-11.1210302576074,15.7481004956167,3.86116276698205));
#96806=CARTESIAN_POINT('Ctrl Pts',(-11.1232272998644,15.7476000664878,3.85427083163141));
#96807=CARTESIAN_POINT('Ctrl Pts',(-11.1264032819796,15.7468602732757,3.84398139925853));
#96808=CARTESIAN_POINT('Ctrl Pts',(-11.1274305969391,15.7466182703996,3.84059918761211));
#96809=CARTESIAN_POINT('Ctrl Pts',(-11.1291652475585,15.7462049940557,3.83479437701117));
#96810=CARTESIAN_POINT('Ctrl Pts',(-11.1298800391705,15.7460332962705,3.83237407946572));
#96811=CARTESIAN_POINT('Ctrl Pts',(-11.1314854149415,15.7456444688356,3.82687321807539));
#96812=CARTESIAN_POINT('Ctrl Pts',(-11.1323712012782,15.7454276170846,3.82379130324512));
#96813=CARTESIAN_POINT('Ctrl Pts',(-11.1347457233965,15.7448398315151,3.81540070284795));
#96814=CARTESIAN_POINT('Ctrl Pts',(-11.1362098102458,15.7444702763736,3.81008503702247));
#96815=CARTESIAN_POINT('Ctrl Pts',(-11.1432802550694,15.7426484233139,3.78369174819178));
#96816=CARTESIAN_POINT('Ctrl Pts',(-11.1483381055273,15.7412246803085,3.76246998298149));
#96817=CARTESIAN_POINT('Ctrl Pts',(-11.1573256594095,15.7384015791782,3.71949985782572));
#96818=CARTESIAN_POINT('Ctrl Pts',(-11.161238572333,15.7370033199704,3.69775728898744));
#96819=CARTESIAN_POINT('Ctrl Pts',(-11.1793904245861,15.7293794955202,3.57759506762583));
#96820=CARTESIAN_POINT('Ctrl Pts',(-11.181731813801,15.7233907062356,3.477792172738));
#96821=CARTESIAN_POINT('Ctrl Pts',(-11.1686603807797,15.7152455481874,3.35136177602668));
#96822=CARTESIAN_POINT('Ctrl Pts',(-11.1648468264498,15.7134486450765,3.32395430885453));
#96823=CARTESIAN_POINT('Ctrl Pts',(-11.1586119391436,15.7110629261981,3.28837532079456));
#96824=CARTESIAN_POINT('Ctrl Pts',(-11.1570619866676,15.7105014630184,3.28005868242311));
#96825=CARTESIAN_POINT('Ctrl Pts',(-11.1543782070616,15.7095777001602,3.26647256807064));
#96826=CARTESIAN_POINT('Ctrl Pts',(-11.1532975450868,15.7092170848723,3.26119280317626));
#96827=CARTESIAN_POINT('Ctrl Pts',(-11.1511336908559,15.7085161766414,3.25097828996551));
#96828=CARTESIAN_POINT('Ctrl Pts',(-11.1500549053129,15.7081760304809,3.24604272074544));
#96829=CARTESIAN_POINT('Ctrl Pts',(-11.1474836648804,15.7073861076131,3.2346314591371));
#96830=CARTESIAN_POINT('Ctrl Pts',(-11.1459681017378,15.7069356047607,3.22816120530877));
#96831=CARTESIAN_POINT('Ctrl Pts',(-11.140850990343,15.7054617614826,3.2071188026942));
#96832=CARTESIAN_POINT('Ctrl Pts',(-11.1370257272322,15.7044313432077,3.19260312740125));
#96833=CARTESIAN_POINT('Ctrl Pts',(-11.1104395647892,15.6976954120639,3.09901443710512));
#96834=CARTESIAN_POINT('Ctrl Pts',(-11.0797263081074,15.6917304883363,3.02245226779789));
#96835=CARTESIAN_POINT('Ctrl Pts',(-11.0278376228702,15.6835790157976,2.92426173141924));
#96836=CARTESIAN_POINT('Ctrl Pts',(-11.0134498946367,15.6814612223146,2.8992970143392));
#96837=CARTESIAN_POINT('Ctrl Pts',(-10.9730336524859,15.6758969763483,2.83476183624392));
#96838=CARTESIAN_POINT('Ctrl Pts',(-10.9455064599881,15.6724763196917,2.79618545131465));
#96839=CARTESIAN_POINT('Ctrl Pts',(-10.9116681131499,15.6687385378231,2.75434726659731));
#96840=CARTESIAN_POINT('Ctrl Pts',(-10.9075666651507,15.6682925856455,2.74936060561022));
#96841=CARTESIAN_POINT('Ctrl Pts',(-10.9012577450849,15.667617633815,2.7418173414062));
#96842=CARTESIAN_POINT('Ctrl Pts',(-10.8990800227074,15.6673866127442,2.73923618621772));
#96843=CARTESIAN_POINT('Ctrl Pts',(-10.895084310839,15.6669663482554,2.73454137209523));
#96844=CARTESIAN_POINT('Ctrl Pts',(-10.893269914678,15.6667768604249,2.73242479557206));
#96845=CARTESIAN_POINT('Ctrl Pts',(-10.8891856043175,15.6663533114187,2.72769435614263));
#96846=CARTESIAN_POINT('Ctrl Pts',(-10.8869116735679,15.6661195483231,2.72508404938227));
#96847=CARTESIAN_POINT('Ctrl Pts',(-10.8802323944914,15.6654387299402,2.7174846383343));
#96848=CARTESIAN_POINT('Ctrl Pts',(-10.8757961355965,15.6649938663248,2.71252270285092));
#96849=CARTESIAN_POINT('Ctrl Pts',(-10.8373922456707,15.6612022320795,2.6702941133651));
#96850=CARTESIAN_POINT('Ctrl Pts',(-10.8011010943487,15.6580124676607,2.63520174157808));
#96851=CARTESIAN_POINT('Ctrl Pts',(-10.745704017538,15.6534803693136,2.58812493431397));
#96852=CARTESIAN_POINT('Ctrl Pts',(-10.7283352447967,15.6521025758694,2.57419309748382));
#96853=CARTESIAN_POINT('Ctrl Pts',(-10.6424293103732,15.6454419608596,2.50920086500072));
#96854=CARTESIAN_POINT('Ctrl Pts',(-10.5688764255294,15.6401749527133,2.46521704315764));
#96855=CARTESIAN_POINT('Ctrl Pts',(-10.4790261717907,15.6337256763909,2.42398471392351));
#96856=CARTESIAN_POINT('Ctrl Pts',(-10.4667413170832,15.6328441892421,2.41859929334936));
#96857=CARTESIAN_POINT('Ctrl Pts',(-10.4476449681182,15.6314729880157,2.4106138697164));
#96858=CARTESIAN_POINT('Ctrl Pts',(-10.4408965612099,15.6309882437529,2.4078652204735));
#96859=CARTESIAN_POINT('Ctrl Pts',(-10.4293880254143,15.6301610652618,2.40330180380957));
#96860=CARTESIAN_POINT('Ctrl Pts',(-10.4246407761381,15.6298197099727,2.40145495324764));
#96861=CARTESIAN_POINT('Ctrl Pts',(-10.4150047303251,15.6291264535887,2.39777797833501));
#96862=CARTESIAN_POINT('Ctrl Pts',(-10.4101154527308,15.6287745087678,2.39594944628848));
#96863=CARTESIAN_POINT('Ctrl Pts',(-10.3980193011543,15.6279032386187,2.39151706532146));
#96864=CARTESIAN_POINT('Ctrl Pts',(-10.3907989475913,15.6273826831983,2.38895096494578));
#96865=CARTESIAN_POINT('Ctrl Pts',(-10.3636492034279,15.625423169241,2.37959938599999));
#96866=CARTESIAN_POINT('Ctrl Pts',(-10.3435651343849,15.6239692299577,2.37327857111096));
#96867=CARTESIAN_POINT('Ctrl Pts',(-10.2924785715365,15.6202574989402,2.3586935961774));
#96868=CARTESIAN_POINT('Ctrl Pts',(-10.2612892618296,15.617978820873,2.35115204083168));
#96869=CARTESIAN_POINT('Ctrl Pts',(-10.1786411376612,15.6119138761872,2.33470742023526));
#96870=CARTESIAN_POINT('Ctrl Pts',(-10.1268315242213,15.6080829426248,2.32793663037627));
#96871=CARTESIAN_POINT('Ctrl Pts',(-10.014371927807,15.5998090410717,2.3207848103437));
#96872=CARTESIAN_POINT('Ctrl Pts',(-9.95378383888036,15.595376948158,2.32160253464665));
#96873=CARTESIAN_POINT('Ctrl Pts',(-9.8837907050311,15.5904518679028,2.32795651354185));
#96874=CARTESIAN_POINT('Ctrl Pts',(-9.87407071524542,15.5897724439979,2.32896098903557));
#96875=CARTESIAN_POINT('Ctrl Pts',(-9.86068562549131,15.5888440813364,2.3305128134094));
#96876=CARTESIAN_POINT('Ctrl Pts',(-9.85700925496088,15.5885898520667,2.33095662086036));
#96877=CARTESIAN_POINT('Ctrl Pts',(-9.85070987419604,15.588155602528,2.33174723601867));
#96878=CARTESIAN_POINT('Ctrl Pts',(-9.8480858559742,15.5879751222836,2.33208555304258));
#96879=CARTESIAN_POINT('Ctrl Pts',(-9.84261010286847,15.5875993808907,2.33281031353234));
#96880=CARTESIAN_POINT('Ctrl Pts',(-9.83975861644863,15.5874042178622,2.33319837026518));
#96881=CARTESIAN_POINT('Ctrl Pts',(-9.83280344615905,15.5869293575943,2.33417087174944));
#96882=CARTESIAN_POINT('Ctrl Pts',(-9.82870131775477,15.5866502808701,2.33476654414031));
#96883=CARTESIAN_POINT('Ctrl Pts',(-9.82009890055875,15.5860669644847,2.33606211595207));
#96884=CARTESIAN_POINT('Ctrl Pts',(-9.81559939849938,15.5857629682338,2.3367664799111));
#96885=CARTESIAN_POINT('Ctrl Pts',(-9.8111040637049,15.5854602598056,2.33749693000354));
#96886=CARTESIAN_POINT('',(-11.1777498238975,15.6247875272409,3.49935594293548));
#96887=CARTESIAN_POINT('Ctrl Pts',(-9.81110406371067,15.4869977587645,2.3374969300026));
#96888=CARTESIAN_POINT('Ctrl Pts',(-9.89721051432613,15.4932156492593,2.32350543266437));
#96889=CARTESIAN_POINT('Ctrl Pts',(-9.98463361579959,15.4996878786372,2.31911987310096));
#96890=CARTESIAN_POINT('Ctrl Pts',(-10.0938106552571,15.5076604291426,2.32578419522931));
#96891=CARTESIAN_POINT('Ctrl Pts',(-10.115822188047,15.509260416155,2.32775066230818));
#96892=CARTESIAN_POINT('Ctrl Pts',(-10.1594864733125,15.5124052718222,2.33289356272436));
#96893=CARTESIAN_POINT('Ctrl Pts',(-10.1811328843666,15.5139499614132,2.33605653096591));
#96894=CARTESIAN_POINT('Ctrl Pts',(-10.2081151940926,15.5158475222848,2.34077026924418));
#96895=CARTESIAN_POINT('Ctrl Pts',(-10.2135435402494,15.5162278491646,2.3417579432186));
#96896=CARTESIAN_POINT('Ctrl Pts',(-10.2221158132083,15.5168259789667,2.34337996218021));
#96897=CARTESIAN_POINT('Ctrl Pts',(-10.2252643487936,15.5170451393421,2.34398904842987));
#96898=CARTESIAN_POINT('Ctrl Pts',(-10.2308850601435,15.5174353884894,2.34510021440993));
#96899=CARTESIAN_POINT('Ctrl Pts',(-10.2333580980304,15.5176067445459,2.34559737352311));
#96900=CARTESIAN_POINT('Ctrl Pts',(-10.2392894895475,15.5180169128745,2.34680961086563));
#96901=CARTESIAN_POINT('Ctrl Pts',(-10.2427462442213,15.5182552928914,2.34753230191249));
#96902=CARTESIAN_POINT('Ctrl Pts',(-10.2532604401807,15.5189784871239,2.34977987179638));
#96903=CARTESIAN_POINT('Ctrl Pts',(-10.2603073179555,15.5194606182302,2.35135414484638));
#96904=CARTESIAN_POINT('Ctrl Pts',(-10.3236652186813,15.5237758844522,2.36612133576886));
#96905=CARTESIAN_POINT('Ctrl Pts',(-10.3789558064251,15.5274042164427,2.38338261408851));
#96906=CARTESIAN_POINT('Ctrl Pts',(-10.527363584146,15.5373085702841,2.44201633451099));
#96907=CARTESIAN_POINT('Ctrl Pts',(-10.6167152720149,15.5435010747445,2.49148523909094));
#96908=CARTESIAN_POINT('Ctrl Pts',(-10.7094557296208,15.5510338374472,2.55981412659028));
#96909=CARTESIAN_POINT('Ctrl Pts',(-10.7201737257285,15.5519222690396,2.56799855727563));
#96910=CARTESIAN_POINT('Ctrl Pts',(-10.7357959124247,15.5532452819511,2.58035829740622));
#96911=CARTESIAN_POINT('Ctrl Pts',(-10.7408104349942,15.5536743358638,2.58439288855875));
#96912=CARTESIAN_POINT('Ctrl Pts',(-10.7496647316474,15.5544399156844,2.59163724412344));
#96913=CARTESIAN_POINT('Ctrl Pts',(-10.7535176198342,15.5547757870199,2.5948307885187));
#96914=CARTESIAN_POINT('Ctrl Pts',(-10.7614237631754,15.5554707354966,2.60146941511489));
#96915=CARTESIAN_POINT('Ctrl Pts',(-10.765474258161,15.5558299335185,2.60491759173413));
#96916=CARTESIAN_POINT('Ctrl Pts',(-10.7760401490486,15.5567753478283,2.61403648164033));
#96917=CARTESIAN_POINT('Ctrl Pts',(-10.7825166631317,15.557363376825,2.61975154996116));
#96918=CARTESIAN_POINT('Ctrl Pts',(-10.7965930004396,15.5586605765982,2.63245104846236));
#96919=CARTESIAN_POINT('Ctrl Pts',(-10.8041649825817,15.5593709551679,2.63946513103956));
#96920=CARTESIAN_POINT('Ctrl Pts',(-10.8263713766596,15.5614925092383,2.66058442476375));
#96921=CARTESIAN_POINT('Ctrl Pts',(-10.8407332908581,15.5629152328664,2.67496932915081));
#96922=CARTESIAN_POINT('Ctrl Pts',(-10.893434286723,15.5683322622743,2.73056026180022));
#96923=CARTESIAN_POINT('Ctrl Pts',(-10.9291719772552,15.5724206476545,2.77412089884531));
#96924=CARTESIAN_POINT('Ctrl Pts',(-11.006303335247,15.5822167179053,2.88321031515338));
#96925=CARTESIAN_POINT('Ctrl Pts',(-11.0446261002811,15.5879400390013,2.95060559192743));
#96926=CARTESIAN_POINT('Ctrl Pts',(-11.0798243951516,15.5940012599102,3.02972367831895));
#96927=CARTESIAN_POINT('Ctrl Pts',(-11.0834830188067,15.5946436053673,3.03821530520902));
#96928=CARTESIAN_POINT('Ctrl Pts',(-11.0884364190084,15.5955300407066,3.05009516109995));
#96929=CARTESIAN_POINT('Ctrl Pts',(-11.0898160055766,15.5957788275126,3.05344734111691));
#96930=CARTESIAN_POINT('Ctrl Pts',(-11.0921678045177,15.5962061901211,3.05923766233175));
#96931=CARTESIAN_POINT('Ctrl Pts',(-11.0931473735835,15.596385195041,3.06167275751346));
#96932=CARTESIAN_POINT('Ctrl Pts',(-11.0951905053741,15.5967606445765,3.06680119530579));
#96933=CARTESIAN_POINT('Ctrl Pts',(-11.0962522889287,15.5969569771928,3.0694952186432));
#96934=CARTESIAN_POINT('Ctrl Pts',(-11.0988440681521,15.5974393101586,3.07614300865987));
#96935=CARTESIAN_POINT('Ctrl Pts',(-11.1003626917843,15.5977246426164,3.08010122274846));
#96936=CARTESIAN_POINT('Ctrl Pts',(-11.1058868482925,15.5987730343144,3.09473544489942));
#96937=CARTESIAN_POINT('Ctrl Pts',(-11.1097588089668,15.5995286766528,3.10546167398037));
#96938=CARTESIAN_POINT('Ctrl Pts',(-11.1362624617959,15.6048669527807,3.18236225887081));
#96939=CARTESIAN_POINT('Ctrl Pts',(-11.1531188908204,15.6091789480721,3.25038918427057));
#96940=CARTESIAN_POINT('Ctrl Pts',(-11.1730673575496,15.6172258453243,3.37902675307541));
#96941=CARTESIAN_POINT('Ctrl Pts',(-11.1777168954739,15.6209453489766,3.43914164328542));
#96942=CARTESIAN_POINT('Ctrl Pts',(-11.1777498238975,15.624787527241,3.49935594293634));
#96943=CARTESIAN_POINT('Ctrl Pts',(-11.1777498238975,15.6247875272409,3.49935594293517));
#96944=CARTESIAN_POINT('Ctrl Pts',(-11.177761752659,15.6261794076629,3.52116937766792));
#96945=CARTESIAN_POINT('Ctrl Pts',(-11.1771680268943,15.6275849209456,3.54296784548813));
#96946=CARTESIAN_POINT('Ctrl Pts',(-11.175246262625,15.6298669495826,3.57787233849004));
#96947=CARTESIAN_POINT('Ctrl Pts',(-11.1743038763382,15.6307313594839,3.59098495780553));
#96948=CARTESIAN_POINT('Ctrl Pts',(-11.1726551053185,15.6319678083066,3.60956939399694));
#96949=CARTESIAN_POINT('Ctrl Pts',(-11.1721294427284,15.6323342813098,3.61505657691785));
#96950=CARTESIAN_POINT('Ctrl Pts',(-11.1710871171421,15.6330135732415,3.62518727707632));
#96951=CARTESIAN_POINT('Ctrl Pts',(-11.1705813034157,15.633326050214,3.62983181929543));
#96952=CARTESIAN_POINT('Ctrl Pts',(-11.169478262422,15.6339739831744,3.63942935272278));
#96953=CARTESIAN_POINT('Ctrl Pts',(-11.1688771732535,15.6343095534268,3.64438179665939));
#96954=CARTESIAN_POINT('Ctrl Pts',(-11.1674463569776,15.6350708687104,3.65557540231151));
#96955=CARTESIAN_POINT('Ctrl Pts',(-11.1665980168341,15.6354971871617,3.66181398786713));
#96956=CARTESIAN_POINT('Ctrl Pts',(-11.1639388808185,15.6367638231177,3.68025992376714));
#96957=CARTESIAN_POINT('Ctrl Pts',(-11.1619862387588,15.6376085455769,3.69244562648848));
#96958=CARTESIAN_POINT('Ctrl Pts',(-11.1539363650213,15.6408029794404,3.738079434383));
#96959=CARTESIAN_POINT('Ctrl Pts',(-11.1465837651145,15.6431911029996,3.77128624116019));
#96960=CARTESIAN_POINT('Ctrl Pts',(-11.1114071437773,15.6529131263646,3.90289019330814));
#96961=CARTESIAN_POINT('Ctrl Pts',(-11.0722666418055,15.6605583058709,3.9977815892684));
#96962=CARTESIAN_POINT('Ctrl Pts',(-11.0077369069689,15.6698853218501,4.11017331970739));
#96963=CARTESIAN_POINT('Ctrl Pts',(-10.9932744057967,15.6718294850041,4.13344406667698));
#96964=CARTESIAN_POINT('Ctrl Pts',(-10.974830726469,15.6741237219133,4.16093322318884));
#96965=CARTESIAN_POINT('Ctrl Pts',(-10.9716146310392,15.6745174626311,4.16565207342345));
#96966=CARTESIAN_POINT('Ctrl Pts',(-10.966533153882,15.6751295816648,4.1729926260965));
#96967=CARTESIAN_POINT('Ctrl Pts',(-10.9646911891974,15.6753494582162,4.17563031492671));
#96968=CARTESIAN_POINT('Ctrl Pts',(-10.9612248437051,15.6757594532525,4.18055103605163));
#96969=CARTESIAN_POINT('Ctrl Pts',(-10.9596031373696,15.675949735098,4.18283580149064));
#96970=CARTESIAN_POINT('Ctrl Pts',(-10.9558732693428,15.6763839195652,4.18805115166247));
#96971=CARTESIAN_POINT('Ctrl Pts',(-10.9537597742006,15.6766274559703,4.19097784938161));
#96972=CARTESIAN_POINT('Ctrl Pts',(-10.948086408654,15.6772747294821,4.19875851095811));
#96973=CARTESIAN_POINT('Ctrl Pts',(-10.9445026705007,15.6776769031198,4.20359505689349));
#96974=CARTESIAN_POINT('Ctrl Pts',(-10.9141763203613,15.6810266707566,4.24387364491772));
#96975=CARTESIAN_POINT('Ctrl Pts',(-10.885482896287,15.6838526043509,4.27780933790015));
#96976=CARTESIAN_POINT('Ctrl Pts',(-10.8090440451889,15.6908111577061,4.35848425102891));
#96977=CARTESIAN_POINT('Ctrl Pts',(-10.7591165231001,15.6948791396483,4.40293407589315));
#96978=CARTESIAN_POINT('Ctrl Pts',(-10.6767515444984,15.7013088343361,4.4645771830992));
#96979=CARTESIAN_POINT('Ctrl Pts',(-10.6468306971383,15.7035930851849,4.48489163386621));
#96980=CARTESIAN_POINT('Ctrl Pts',(-10.6029398222404,15.7069131051099,4.51182722503868));
#96981=CARTESIAN_POINT('Ctrl Pts',(-10.589699579295,15.7079107273866,4.51960047837317));
#96982=CARTESIAN_POINT('Ctrl Pts',(-10.5689143399039,15.7094733442095,4.53126305266973));
#96983=CARTESIAN_POINT('Ctrl Pts',(-10.5614725888179,15.7100321213202,4.53533353847116));
#96984=CARTESIAN_POINT('Ctrl Pts',(-10.5474543211416,15.7110838483694,4.54280565828641));
#96985=CARTESIAN_POINT('Ctrl Pts',(-10.5408884052169,15.7115761111437,4.54622636346372));
#96986=CARTESIAN_POINT('Ctrl Pts',(-10.5297340212421,15.7124120145146,4.55190449857282));
#96987=CARTESIAN_POINT('Ctrl Pts',(-10.5251622491513,15.7127545168353,4.55419439290754));
#96988=CARTESIAN_POINT('Ctrl Pts',(-10.516007276883,15.7134402450845,4.55870557359808));
#96989=CARTESIAN_POINT('Ctrl Pts',(-10.5114242911437,15.7137834554678,4.5609270447985));
#96990=CARTESIAN_POINT('Ctrl Pts',(-10.5002475324582,15.7146203790946,4.56625540960634));
#96991=CARTESIAN_POINT('Ctrl Pts',(-10.4936391170729,15.7151151548021,4.56933091706173));
#96992=CARTESIAN_POINT('Ctrl Pts',(-10.4747780588764,15.7165273266611,4.57789661922381));
#96993=CARTESIAN_POINT('Ctrl Pts',(-10.4624598308059,15.717449674415,4.5832387575681));
#96994=CARTESIAN_POINT('Ctrl Pts',(-10.3709071359389,15.7243076460911,4.62109687655362));
#96995=CARTESIAN_POINT('Ctrl Pts',(-10.2884415160426,15.7305284726804,4.64508800541817));
#96996=CARTESIAN_POINT('Ctrl Pts',(-10.133459201567,15.7420824978954,4.67236152475451));
#96997=CARTESIAN_POINT('Ctrl Pts',(-10.0618003882636,15.7473642515622,4.67831482822884));
#96998=CARTESIAN_POINT('Ctrl Pts',(-9.98282219017373,15.7528622073854,4.67764683668524));
#96999=CARTESIAN_POINT('Ctrl Pts',(-9.97560582810824,15.7533615015853,4.67751946056978));
#97000=CARTESIAN_POINT('Ctrl Pts',(-9.96486133799105,15.7540999018741,4.67723098986928));
#97001=CARTESIAN_POINT('Ctrl Pts',(-9.9613321913639,15.7543416335015,4.6771203551359));
#97002=CARTESIAN_POINT('Ctrl Pts',(-9.95528271212342,15.7547545581452,4.67690347496911));
#97003=CARTESIAN_POINT('Ctrl Pts',(-9.95276217138632,15.7549261739566,4.67680500220719));
#97004=CARTESIAN_POINT('Ctrl Pts',(-9.94703749135996,15.755314961416,4.67656292722283));
#97005=CARTESIAN_POINT('Ctrl Pts',(-9.94383361040631,15.7555318544521,4.67641433446639));
#97006=CARTESIAN_POINT('Ctrl Pts',(-9.93511827008212,15.75612005951,4.67597444011749));
#97007=CARTESIAN_POINT('Ctrl Pts',(-9.92960810135573,15.7564899889378,4.67565747829089));
#97008=CARTESIAN_POINT('Ctrl Pts',(-9.9022537832048,15.7583176303144,4.67389096482123));
#97009=CARTESIAN_POINT('Ctrl Pts',(-9.88044920179295,15.7597465657476,4.67187118545924));
#97010=CARTESIAN_POINT('Ctrl Pts',(-9.83679984521038,15.7625736047331,4.66659672743324));
#97011=CARTESIAN_POINT('Ctrl Pts',(-9.81496534681935,15.763970795932,4.66333335266161));
#97012=CARTESIAN_POINT('Ctrl Pts',(-9.69531446341559,15.7715949375259,4.64199607309003));
#97013=CARTESIAN_POINT('Ctrl Pts',(-9.60000441121922,15.7775855796425,4.61220156614234));
#97014=CARTESIAN_POINT('Ctrl Pts',(-9.48449557989681,15.7857279704919,4.55929738146958));
#97015=CARTESIAN_POINT('Ctrl Pts',(-9.45983291139068,15.7875195351527,4.54693604140466));
#97016=CARTESIAN_POINT('Ctrl Pts',(-9.42821244978103,15.7898990369194,4.52967249480587));
#97017=CARTESIAN_POINT('Ctrl Pts',(-9.4208405843612,15.7904597991368,4.52554415518738));
#97018=CARTESIAN_POINT('Ctrl Pts',(-9.4088434932997,15.79138262182,4.51865502148231));
#97019=CARTESIAN_POINT('Ctrl Pts',(-9.40419157339058,15.7917430035306,4.51594113281503));
#97020=CARTESIAN_POINT('Ctrl Pts',(-9.39521316460938,15.7924436092373,4.51062033399013));
#97021=CARTESIAN_POINT('Ctrl Pts',(-9.39088450379328,15.7927836875505,4.50801730473551));
#97022=CARTESIAN_POINT('Ctrl Pts',(-9.38089830387563,15.7935736749092,4.50192431802121));
#97023=CARTESIAN_POINT('Ctrl Pts',(-9.37525334595228,15.7940243115255,4.49841417472535));
#97024=CARTESIAN_POINT('Ctrl Pts',(-9.35694323219308,15.7954995678635,4.48681251080593));
#97025=CARTESIAN_POINT('Ctrl Pts',(-9.34440363509876,15.7965312862809,4.47852660059326));
#97026=CARTESIAN_POINT('Ctrl Pts',(-9.26482807917204,15.8032207955286,4.4237284779901));
#97027=CARTESIAN_POINT('Ctrl Pts',(-9.20263221955389,15.8091331884359,4.37060442993804));
#97028=CARTESIAN_POINT('Ctrl Pts',(-9.10896140987051,15.8191106589038,4.27207713806588));
#97029=CARTESIAN_POINT('Ctrl Pts',(-9.0742619757164,15.8231169123413,4.23011133406531));
#97030=CARTESIAN_POINT('Ctrl Pts',(-9.03321296510913,15.8281703167998,4.17281268673037));
#97031=CARTESIAN_POINT('Ctrl Pts',(-9.02410877069685,15.8293140522766,4.1595380545915));
#97032=CARTESIAN_POINT('Ctrl Pts',(-9.00938064686383,15.8311986162026,4.13709023893374));
#97033=CARTESIAN_POINT('Ctrl Pts',(-9.00360533997464,15.8319470648426,4.12801940845524));
#97034=CARTESIAN_POINT('Ctrl Pts',(-8.99577767109306,15.8329735357652,4.11534522278951));
#97035=CARTESIAN_POINT('Ctrl Pts',(-8.99361909551352,15.833257916871,4.11180855296335));
#97036=CARTESIAN_POINT('Ctrl Pts',(-8.98999351512012,15.8337377268542,4.10579719222085));
#97037=CARTESIAN_POINT('Ctrl Pts',(-8.98851684418025,15.833933768788,4.10332840457926));
#97038=CARTESIAN_POINT('Ctrl Pts',(-8.98569988824821,15.8343089075533,4.09857943574135));
#97039=CARTESIAN_POINT('Ctrl Pts',(-8.984358224542,15.8344880969254,4.09630012736003));
#97040=CARTESIAN_POINT('Ctrl Pts',(-8.9811571554265,15.8349169218492,4.09081978991472));
#97041=CARTESIAN_POINT('Ctrl Pts',(-8.97930512685464,15.8351660908035,4.08761445093899));
#97042=CARTESIAN_POINT('Ctrl Pts',(-8.9726210488151,15.8360694659802,4.07591924587095));
#97043=CARTESIAN_POINT('Ctrl Pts',(-8.96787939606275,15.8367182457984,4.06737779419613));
#97044=CARTESIAN_POINT('Ctrl Pts',(-8.93454089350355,15.8413454093333,4.00552160051157));
#97045=CARTESIAN_POINT('Ctrl Pts',(-8.9099796488634,15.8451147933833,3.95012527521383));
#97046=CARTESIAN_POINT('Ctrl Pts',(-8.87236327705549,15.8520936324839,3.84388142084387));
#97047=CARTESIAN_POINT('Ctrl Pts',(-8.85823416080146,15.8553012199524,3.79358062218364));
#97048=CARTESIAN_POINT('Ctrl Pts',(-8.84088206119212,15.8605910562537,3.7111157614684));
#97049=CARTESIAN_POINT('Ctrl Pts',(-8.83556215866905,15.8626277161817,3.67946737174046));
#97050=CARTESIAN_POINT('Ctrl Pts',(-8.82890168419637,15.866061789561,3.62675581642737));
#97051=CARTESIAN_POINT('Ctrl Pts',(-8.82682312079678,15.8674375711779,3.6058027584884));
#97052=CARTESIAN_POINT('Ctrl Pts',(-8.82475562427758,15.8693377264903,3.57716485642819));
#97053=CARTESIAN_POINT('Ctrl Pts',(-8.82427854369114,15.869846981453,3.56951841680842));
#97054=CARTESIAN_POINT('Ctrl Pts',(-8.8236019772305,15.8707070140562,3.55665674705193));
#97055=CARTESIAN_POINT('Ctrl Pts',(-8.82336248989264,15.8710565426199,3.5514437875224));
#97056=CARTESIAN_POINT('Ctrl Pts',(-8.82295778895651,15.8717492620643,3.54114150411683));
#97057=CARTESIAN_POINT('Ctrl Pts',(-8.82279092081317,15.87209239379,3.5360523565532));
#97058=CARTESIAN_POINT('Ctrl Pts',(-8.82246559326226,15.8729288330372,3.52368178288959));
#97059=CARTESIAN_POINT('Ctrl Pts',(-8.82234166654363,15.8734232000805,3.51639973738332));
#97060=CARTESIAN_POINT('Ctrl Pts',(-8.82218152583615,15.8748334349755,3.49571344286522));
#97061=CARTESIAN_POINT('Ctrl Pts',(-8.82230659714929,15.8757542347223,3.4823094447475));
#97062=CARTESIAN_POINT('Ctrl Pts',(-8.82492145912527,15.8826110869499,3.38328479435956));
#97063=CARTESIAN_POINT('Ctrl Pts',(-8.83651643837456,15.8888324734114,3.29817643161657));
#97064=CARTESIAN_POINT('Ctrl Pts',(-8.87459256600722,15.9003891345095,3.14545130232369));
#97065=CARTESIAN_POINT('Ctrl Pts',(-8.89828716821528,15.9056729141352,3.07753375536569));
#97066=CARTESIAN_POINT('Ctrl Pts',(-8.93101100335317,15.9111727028667,3.00562193106713));
#97067=CARTESIAN_POINT('Ctrl Pts',(-8.93406067510026,15.9116720013875,2.99908033362235));
#97068=CARTESIAN_POINT('Ctrl Pts',(-8.93869163338618,15.912410406792,2.98938068963488));
#97069=CARTESIAN_POINT('Ctrl Pts',(-8.94022722977,15.912652139266,2.98620120137853));
#97070=CARTESIAN_POINT('Ctrl Pts',(-8.94288435041313,15.9130650648525,2.98076216563614));
#97071=CARTESIAN_POINT('Ctrl Pts',(-8.94399885758412,15.9132366807656,2.97849926855728));
#97072=CARTESIAN_POINT('Ctrl Pts',(-8.9465469661601,15.9136254677741,2.97336724895143));
#97073=CARTESIAN_POINT('Ctrl Pts',(-8.94798502215157,15.9138423602619,2.97050039094686));
#97074=CARTESIAN_POINT('Ctrl Pts',(-8.95192948105874,15.9144305623703,2.96271636018252));
#97075=CARTESIAN_POINT('Ctrl Pts',(-8.95445880375256,15.9148004894201,2.95781079666966));
#97076=CARTESIAN_POINT('Ctrl Pts',(-8.96719141551378,15.9166280998969,2.93353664802352));
#97077=CARTESIAN_POINT('Ctrl Pts',(-8.97789959592997,15.9180570079712,2.91443598660133));
#97078=CARTESIAN_POINT('Ctrl Pts',(-9.00046079605369,15.920884026304,2.87669943184795));
#97079=CARTESIAN_POINT('Ctrl Pts',(-9.01231760843708,15.922281223223,2.85807647714523));
#97080=CARTESIAN_POINT('Ctrl Pts',(-9.08044728321178,15.9299053305923,2.75742948122007));
#97081=CARTESIAN_POINT('Ctrl Pts',(-9.14640992292165,15.935895932523,2.68245939409084));
#97082=CARTESIAN_POINT('Ctrl Pts',(-9.24169781415504,15.944038328813,2.59842715571879));
#97083=CARTESIAN_POINT('Ctrl Pts',(-9.26301731027366,15.9458299498601,2.58091778251157));
#97084=CARTESIAN_POINT('Ctrl Pts',(-9.2916440442888,15.9482095160661,2.55904394855642));
#97085=CARTESIAN_POINT('Ctrl Pts',(-9.29841250159619,15.9487702844499,2.55398656106795));
#97086=CARTESIAN_POINT('Ctrl Pts',(-9.30958344558528,15.9496931146866,2.54582546155538));
#97087=CARTESIAN_POINT('Ctrl Pts',(-9.3139539260595,15.9500534977304,2.54267829272718));
#97088=CARTESIAN_POINT('Ctrl Pts',(-9.32246484202575,15.9507541041723,2.53663782233348));
#97089=CARTESIAN_POINT('Ctrl Pts',(-9.32660261429722,15.9510941818756,2.53374095853776));
#97090=CARTESIAN_POINT('Ctrl Pts',(-9.33622863092652,15.9518841650775,2.52709362315991));
#97091=CARTESIAN_POINT('Ctrl Pts',(-9.34173020396016,15.9523347981234,2.52336285091671));
#97092=CARTESIAN_POINT('Ctrl Pts',(-9.35977250766573,15.9538100305901,2.51134956264405));
#97093=CARTESIAN_POINT('Ctrl Pts',(-9.37243980266421,15.9548417283877,2.50326077052136));
#97094=CARTESIAN_POINT('Ctrl Pts',(-9.45486104241834,15.961531955599,2.45282412212095));
#97095=CARTESIAN_POINT('Ctrl Pts',(-9.52868969252329,15.9674451611739,2.41758797531464));
#97096=CARTESIAN_POINT('Ctrl Pts',(-9.65678882607535,15.9774228400901,2.3720558129096));
#97097=CARTESIAN_POINT('Ctrl Pts',(-9.70922826639941,15.9814284824155,2.35741329801038));
#97098=CARTESIAN_POINT('Ctrl Pts',(-9.77825614559363,15.9864812027241,2.343201096522));
#97099=CARTESIAN_POINT('Ctrl Pts',(-9.79408401900635,15.9876248425736,2.34027904069928));
#97100=CARTESIAN_POINT('Ctrl Pts',(-9.81034639637981,15.9887815099625,2.33762023398126));
#97101=CARTESIAN_POINT('Ctrl Pts',(-9.81072521498865,15.9888084433933,2.33755848939621));
#97102=CARTESIAN_POINT('Ctrl Pts',(-9.81110406371144,15.9888353687451,2.33749693000248));
#97103=CARTESIAN_POINT('Origin',(-10.,12.3756328852638,3.5));
#97104=CARTESIAN_POINT('',(-9.81110406371068,16.5874147438851,2.3374969300026));
#97105=CARTESIAN_POINT('',(-9.81110406371068,16.4876146309988,2.3374969300026));
#97106=CARTESIAN_POINT('',(-9.81110406371068,12.3756328852638,2.3374969300026));
#97107=CARTESIAN_POINT('Ctrl Pts',(-9.81110406371068,16.5874147438851,2.3374969300026));
#97108=CARTESIAN_POINT('Ctrl Pts',(-9.79408468926281,16.5863079989926,2.34026242005107));
#97109=CARTESIAN_POINT('Ctrl Pts',(-9.77711811835858,16.5851910491628,2.34340294741657));
#97110=CARTESIAN_POINT('Ctrl Pts',(-9.74696993641862,16.5831775822287,2.34967225854604));
#97111=CARTESIAN_POINT('Ctrl Pts',(-9.73377215044021,16.5822862330308,2.35265487610149));
#97112=CARTESIAN_POINT('Ctrl Pts',(-9.71436711100458,16.5809596121411,2.35739312721334));
#97113=CARTESIAN_POINT('Ctrl Pts',(-9.70811788197619,16.5805299106053,2.35897351502779));
#97114=CARTESIAN_POINT('Ctrl Pts',(-9.69703807990843,16.5797635059656,2.36187249933278));
#97115=CARTESIAN_POINT('Ctrl Pts',(-9.69220231246993,16.5794274614067,2.36317076259259));
#97116=CARTESIAN_POINT('Ctrl Pts',(-9.68204187876341,16.5787180639963,2.36596812472266));
#97117=CARTESIAN_POINT('Ctrl Pts',(-9.67671921482961,16.578344500852,2.36747397683905));
#97118=CARTESIAN_POINT('Ctrl Pts',(-9.66265810669044,16.5773524023741,2.3715592518712));
#97119=CARTESIAN_POINT('Ctrl Pts',(-9.65393879282778,16.5767318158725,2.37420263467108));
#97120=CARTESIAN_POINT('Ctrl Pts',(-9.61221804355026,16.5737357786153,2.38738133802136));
#97121=CARTESIAN_POINT('Ctrl Pts',(-9.57966459656168,16.5713169106818,2.3992671295671));
#97122=CARTESIAN_POINT('Ctrl Pts',(-9.48613439787508,16.564121547153,2.43817085903942));
#97123=CARTESIAN_POINT('Ctrl Pts',(-9.4268749206994,16.5592384804651,2.46894967299835));
#97124=CARTESIAN_POINT('Ctrl Pts',(-9.31850085655684,16.5498232420847,2.53747964696441));
#97125=CARTESIAN_POINT('Ctrl Pts',(-9.26911361717667,16.5453091615741,2.57442279852042));
#97126=CARTESIAN_POINT('Ctrl Pts',(-9.21551297330088,16.5403103584506,2.62149546971246));
#97127=CARTESIAN_POINT('Ctrl Pts',(-9.20826765431734,16.5396324873437,2.62801948813788));
#97128=CARTESIAN_POINT('Ctrl Pts',(-9.19838513695731,16.5387058464639,2.63714290568825));
#97129=CARTESIAN_POINT('Ctrl Pts',(-9.19567817661452,16.5384518119952,2.63966567009587));
#97130=CARTESIAN_POINT('Ctrl Pts',(-9.19105668636879,16.5380178082519,2.64401356691796));
#97131=CARTESIAN_POINT('Ctrl Pts',(-9.18913635396772,16.5378373801215,2.64583244841163));
#97132=CARTESIAN_POINT('Ctrl Pts',(-9.18513904347096,16.5374616486359,2.64964421027428));
#97133=CARTESIAN_POINT('Ctrl Pts',(-9.18306322311956,16.5372664438976,2.65163825497827));
#97134=CARTESIAN_POINT('Ctrl Pts',(-9.17801360693692,16.5367913209343,2.65652466488151));
#97135=CARTESIAN_POINT('Ctrl Pts',(-9.17504770412508,16.5365120248615,2.65942520727319));
#97136=CARTESIAN_POINT('Ctrl Pts',(-9.16442970244067,16.5355110212583,2.66991954732166));
#97137=CARTESIAN_POINT('Ctrl Pts',(-9.15686634441118,16.5347958841342,2.6776029308858));
#97138=CARTESIAN_POINT('Ctrl Pts',(-9.1382393716952,16.533025915166,2.69705263048693));
#97139=CARTESIAN_POINT('Ctrl Pts',(-9.12730999438134,16.5319794215196,2.70894496576112));
#97140=CARTESIAN_POINT('Ctrl Pts',(-9.08043974925024,16.5274360366953,2.76209899527789));
#97141=CARTESIAN_POINT('Ctrl Pts',(-9.04715240375305,16.5240584114185,2.80561440427617));
#97142=CARTESIAN_POINT('Ctrl Pts',(-8.97231947764012,16.5156600511642,2.91900872634387));
#97143=CARTESIAN_POINT('Ctrl Pts',(-8.93475204657371,16.5106428630481,2.99115541704199));
#97144=CARTESIAN_POINT('Ctrl Pts',(-8.8993629247579,16.5043708741205,3.0805725705774));
#97145=CARTESIAN_POINT('Ctrl Pts',(-8.8940959378516,16.5033816679124,3.09466370537582));
#97146=CARTESIAN_POINT('Ctrl Pts',(-8.88689155917966,16.5019422763355,3.1151248289143));
#97147=CARTESIAN_POINT('Ctrl Pts',(-8.8847358802319,16.5014992501638,3.12141680115294));
#97148=CARTESIAN_POINT('Ctrl Pts',(-8.88103643866512,16.5007165578909,3.13252055284595));
#97149=CARTESIAN_POINT('Ctrl Pts',(-8.87947012161172,16.500377637837,3.13732468246038));
#97150=CARTESIAN_POINT('Ctrl Pts',(-8.87629793577131,16.4996752962943,3.14727099174285));
#97151=CARTESIAN_POINT('Ctrl Pts',(-8.87469633850272,16.4993117450035,3.15241439878776));
#97152=CARTESIAN_POINT('Ctrl Pts',(-8.8706734003786,16.4983749851343,3.16565304178214));
#97153=CARTESIAN_POINT('Ctrl Pts',(-8.86830382397239,16.4978001187663,3.17376355849627));
#97154=CARTESIAN_POINT('Ctrl Pts',(-8.85857577489246,16.4953374979942,3.20844243424092));
#97155=CARTESIAN_POINT('Ctrl Pts',(-8.85206464246632,16.4934229646919,3.23523733102931));
#97156=CARTESIAN_POINT('Ctrl Pts',(-8.82640825252528,16.484468686366,3.35970703827271));
#97157=CARTESIAN_POINT('Ctrl Pts',(-8.81875521127112,16.4770852947845,3.45932427098685));
#97158=CARTESIAN_POINT('Ctrl Pts',(-8.82481469572238,16.4682228315322,3.58076473921803));
#97159=CARTESIAN_POINT('Ctrl Pts',(-8.82653708329256,16.4666224812038,3.60280233222635));
#97160=CARTESIAN_POINT('Ctrl Pts',(-8.83119239825596,16.463479623788,3.64649495526358));
#97161=CARTESIAN_POINT('Ctrl Pts',(-8.83410985987507,16.4619372282388,3.66814372477024));
#97162=CARTESIAN_POINT('Ctrl Pts',(-8.83851636563263,16.4600419833879,3.6951441860628));
#97163=CARTESIAN_POINT('Ctrl Pts',(-8.83944304568615,16.4596617607809,3.70058176648894));
#97164=CARTESIAN_POINT('Ctrl Pts',(-8.84096891532767,16.4590637129155,3.70917048831032));
#97165=CARTESIAN_POINT('Ctrl Pts',(-8.84154281942247,16.4588445314184,3.71232595180354));
#97166=CARTESIAN_POINT('Ctrl Pts',(-8.84259132210304,16.4584541926773,3.71796004958876));
#97167=CARTESIAN_POINT('Ctrl Pts',(-8.84306099457255,16.4582827683767,3.720439490082));
#97168=CARTESIAN_POINT('Ctrl Pts',(-8.84420752393593,16.4578723647165,3.72638750690595));
#97169=CARTESIAN_POINT('Ctrl Pts',(-8.84489202664998,16.4576338184834,3.72985456648329));
#97170=CARTESIAN_POINT('Ctrl Pts',(-8.84702427888503,16.4569098594624,3.74040447241923));
#97171=CARTESIAN_POINT('Ctrl Pts',(-8.8485216777548,16.4564271372083,3.74747727919922));
#97172=CARTESIAN_POINT('Ctrl Pts',(-8.86263946094417,16.4520942392961,3.8112570915323));
#97173=CARTESIAN_POINT('Ctrl Pts',(-8.8793762232298,16.4484506817385,3.86697988372485));
#97174=CARTESIAN_POINT('Ctrl Pts',(-8.93641930215884,16.4385528055183,4.01591470650515));
#97175=CARTESIAN_POINT('Ctrl Pts',(-8.98474350453736,16.4323796812434,4.10549490890791));
#97176=CARTESIAN_POINT('Ctrl Pts',(-9.0518394195919,16.4248670774143,4.19876293572158));
#97177=CARTESIAN_POINT('Ctrl Pts',(-9.05992910494375,16.4239757264364,4.20960891639439));
#97178=CARTESIAN_POINT('Ctrl Pts',(-9.07214594089555,16.4226491033988,4.22541261230133));
#97179=CARTESIAN_POINT('Ctrl Pts',(-9.07613003742487,16.4222194015214,4.23047991248821));
#97180=CARTESIAN_POINT('Ctrl Pts',(-9.08328239131766,16.4214529964984,4.23942474853006));
#97181=CARTESIAN_POINT('Ctrl Pts',(-9.08643418231023,16.4211169519,4.24331529530101));
#97182=CARTESIAN_POINT('Ctrl Pts',(-9.09311998300004,16.4204075546388,4.25146143995624));
#97183=CARTESIAN_POINT('Ctrl Pts',(-9.09665934894785,16.4200339916846,4.25571246339029));
#97184=CARTESIAN_POINT('Ctrl Pts',(-9.1061073833304,16.4190418942558,4.26689899247183));
#97185=CARTESIAN_POINT('Ctrl Pts',(-9.11206671329609,16.418421308621,4.2737910215464));
#97186=CARTESIAN_POINT('Ctrl Pts',(-9.1410659093832,16.4154252827519,4.30655275719454));
#97187=CARTESIAN_POINT('Ctrl Pts',(-9.16515754406224,16.4130064257417,4.33146423052054));
#97188=CARTESIAN_POINT('Ctrl Pts',(-9.23871953175109,16.4058111118984,4.40110540981117));
#97189=CARTESIAN_POINT('Ctrl Pts',(-9.29092797697519,16.4009280858699,4.44273746547733));
#97190=CARTESIAN_POINT('Ctrl Pts',(-9.39759254244523,16.3915128341171,4.51389933169584));
#97191=CARTESIAN_POINT('Ctrl Pts',(-9.45142135247845,16.3869986996223,4.54400652067674));
#97192=CARTESIAN_POINT('Ctrl Pts',(-9.51621781116061,16.3819998469364,4.57384584486822));
#97193=CARTESIAN_POINT('Ctrl Pts',(-9.5251235969447,16.3813219758873,4.57781376966188));
#97194=CARTESIAN_POINT('Ctrl Pts',(-9.53747630924262,16.3803953350716,4.58313461275248));
#97195=CARTESIAN_POINT('Ctrl Pts',(-9.54088157399948,16.3801413006102,4.58458241996252));
#97196=CARTESIAN_POINT('Ctrl Pts',(-9.54673260082257,16.3797072968761,4.58703759048707));
#97197=CARTESIAN_POINT('Ctrl Pts',(-9.54917501022853,16.3795268687476,4.58805279616416));
#97198=CARTESIAN_POINT('Ctrl Pts',(-9.55428247776101,16.3791511372624,4.5901556026388));
#97199=CARTESIAN_POINT('Ctrl Pts',(-9.55694812910274,16.3789559325226,4.59124167237633));
#97200=CARTESIAN_POINT('Ctrl Pts',(-9.56346519749256,16.3784808095495,4.59386911353));
#97201=CARTESIAN_POINT('Ctrl Pts',(-9.56732087741935,16.3782015134684,4.59539994957133));
#97202=CARTESIAN_POINT('Ctrl Pts',(-9.58122510704826,16.3772005098025,4.60083553228126));
#97203=CARTESIAN_POINT('Ctrl Pts',(-9.59131943710219,16.3764853726251,4.60462278538938));
#97204=CARTESIAN_POINT('Ctrl Pts',(-9.61666128407167,16.374715403498,4.61373573509516));
#97205=CARTESIAN_POINT('Ctrl Pts',(-9.63196937591183,16.3736689097479,4.61888756043132));
#97206=CARTESIAN_POINT('Ctrl Pts',(-9.69958577349557,16.3691255241802,4.64010536406049));
#97207=CARTESIAN_POINT('Ctrl Pts',(-9.75287462376389,16.3657478983034,4.65283084047908));
#97208=CARTESIAN_POINT('Ctrl Pts',(-9.88689639807948,16.3573495382542,4.67511092631538));
#97209=CARTESIAN_POINT('Ctrl Pts',(-9.96808428688454,16.3523323509203,4.6801090614651));
#97210=CARTESIAN_POINT('Ctrl Pts',(-10.0641661153907,16.3460603628537,4.67609695586526));
#97211=CARTESIAN_POINT('Ctrl Pts',(-10.0791815476522,16.3450711566235,4.67518151318752));
#97212=CARTESIAN_POINT('Ctrl Pts',(-10.1008044976608,16.3436317650201,4.67344695303873));
#97213=CARTESIAN_POINT('Ctrl Pts',(-10.1074294628925,16.3431887388445,4.67285898802661));
#97214=CARTESIAN_POINT('Ctrl Pts',(-10.1190782688419,16.342406046567,4.67172563408231));
#97215=CARTESIAN_POINT('Ctrl Pts',(-10.1241042879964,16.3420671265125,4.67120396174805));
#97216=CARTESIAN_POINT('Ctrl Pts',(-10.1344812665587,16.3413647849708,4.670059345231));
#97217=CARTESIAN_POINT('Ctrl Pts',(-10.1398316111107,16.3410012336816,4.66943199942673));
#97218=CARTESIAN_POINT('Ctrl Pts',(-10.1535624792038,16.3400644738216,4.66772643288611));
#97219=CARTESIAN_POINT('Ctrl Pts',(-10.1619359232643,16.3394896074611,4.66659470569483));
#97220=CARTESIAN_POINT('Ctrl Pts',(-10.1975749006267,16.3370269867675,4.6613867720959));
#97221=CARTESIAN_POINT('Ctrl Pts',(-10.2247029905823,16.3351124535383,4.65644430126276));
#97222=CARTESIAN_POINT('Ctrl Pts',(-10.3488549121657,16.3261581752415,4.62929179367547));
#97223=CARTESIAN_POINT('Ctrl Pts',(-10.4429821669369,16.3187747836049,4.5957922092073));
#97224=CARTESIAN_POINT('Ctrl Pts',(-10.5514746902357,16.3099123203006,4.54089341842305));
#97225=CARTESIAN_POINT('Ctrl Pts',(-10.570909496116,16.3083119699782,4.53036201581735));
#97226=CARTESIAN_POINT('Ctrl Pts',(-10.6089375213839,16.3051691125312,4.50834868814557));
#97227=CARTESIAN_POINT('Ctrl Pts',(-10.6275313071981,16.303626716946,4.49688343828562));
#97228=CARTESIAN_POINT('Ctrl Pts',(-10.6504094721501,16.3017314720575,4.48188237828943));
#97229=CARTESIAN_POINT('Ctrl Pts',(-10.6550009112291,16.3013512494475,4.47882546735543));
#97230=CARTESIAN_POINT('Ctrl Pts',(-10.662227873313,16.3007532015785,4.4739402405816));
#97231=CARTESIAN_POINT('Ctrl Pts',(-10.6648776231661,16.3005340200808,4.4721332703153));
#97232=CARTESIAN_POINT('Ctrl Pts',(-10.6695990948661,16.3001436813391,4.46888517536519));
#97233=CARTESIAN_POINT('Ctrl Pts',(-10.6716735556494,16.2999722570386,4.46744822378684));
#97234=CARTESIAN_POINT('Ctrl Pts',(-10.6766419978878,16.2995618533794,4.46398296546346));
#97235=CARTESIAN_POINT('Ctrl Pts',(-10.6795314857109,16.2993233071472,4.46194828954442));
#97236=CARTESIAN_POINT('Ctrl Pts',(-10.6883038280757,16.2985993481319,4.45571186248531));
#97237=CARTESIAN_POINT('Ctrl Pts',(-10.694157328634,16.2981166258825,4.45146882945426));
#97238=CARTESIAN_POINT('Ctrl Pts',(-10.7466920010841,16.2937837281405,4.41264507233434));
#97239=CARTESIAN_POINT('Ctrl Pts',(-10.7908007315756,16.2901401707307,4.37470342789388));
#97240=CARTESIAN_POINT('Ctrl Pts',(-10.9036902665696,16.2802422944522,4.26204710351733));
#97241=CARTESIAN_POINT('Ctrl Pts',(-10.965893739435,16.2740691699931,4.18148303065883));
#97242=CARTESIAN_POINT('Ctrl Pts',(-11.0238364116459,16.2665565659719,4.08226894881557));
#97243=CARTESIAN_POINT('Ctrl Pts',(-11.0304577206909,16.265665215021,4.07046909453154));
#97244=CARTESIAN_POINT('Ctrl Pts',(-11.0399311240431,16.2643385920159,4.0528832339002));
#97245=CARTESIAN_POINT('Ctrl Pts',(-11.0429414898042,16.2639088901437,4.04718338712117));
#97246=CARTESIAN_POINT('Ctrl Pts',(-11.0482067967452,16.2631424851265,4.03701270382011));
#97247=CARTESIAN_POINT('Ctrl Pts',(-11.0504803186663,16.2628064405287,4.03255162338894));
#97248=CARTESIAN_POINT('Ctrl Pts',(-11.0552055336801,16.2620970432652,4.02313185973158));
#97249=CARTESIAN_POINT('Ctrl Pts',(-11.0576508700904,16.2617234803081,4.01817014210034));
#97250=CARTESIAN_POINT('Ctrl Pts',(-11.0640311911888,16.2607313828635,4.00499079097704));
#97251=CARTESIAN_POINT('Ctrl Pts',(-11.0679058603511,16.2601107972156,3.99674454208771));
#97252=CARTESIAN_POINT('Ctrl Pts',(-11.0860515789608,16.257114771174,3.9569322599231));
#97253=CARTESIAN_POINT('Ctrl Pts',(-11.0990196096179,16.2546959139986,3.92479476304034));
#97254=CARTESIAN_POINT('Ctrl Pts',(-11.1327470344868,16.2475005994033,3.82927658261698));
#97255=CARTESIAN_POINT('Ctrl Pts',(-11.1495632569813,16.2426175727593,3.76465332402885));
#97256=CARTESIAN_POINT('Ctrl Pts',(-11.1712247110378,16.233202321209,3.63827246531873));
#97257=CARTESIAN_POINT('Ctrl Pts',(-11.1768524600664,16.2286881875312,3.57685332554508));
#97258=CARTESIAN_POINT('Ctrl Pts',(-11.1777774019412,16.2236893355954,3.50552234152789));
#97259=CARTESIAN_POINT('Ctrl Pts',(-11.177782768323,16.2230114645455,3.49577260209303));
#97260=CARTESIAN_POINT('Ctrl Pts',(-11.1776231566506,16.2220848237288,3.48232360968427));
#97261=CARTESIAN_POINT('Ctrl Pts',(-11.1775618094444,16.2218307892673,3.47862385154178));
#97262=CARTESIAN_POINT('Ctrl Pts',(-11.1774267116539,16.221396785533,3.47228002573966));
#97263=CARTESIAN_POINT('Ctrl Pts',(-11.17736148911,16.2212163574045,3.46963583355809));
#97264=CARTESIAN_POINT('Ctrl Pts',(-11.1772066876413,16.2208406259193,3.46411459672561));
#97265=CARTESIAN_POINT('Ctrl Pts',(-11.1771154687181,16.2206454211796,3.46123763241353));
#97266=CARTESIAN_POINT('Ctrl Pts',(-11.1768670390667,16.2201702982065,3.45421524605915));
#97267=CARTESIAN_POINT('Ctrl Pts',(-11.1766984698143,16.2198910021255,3.45007021155055));
#97268=CARTESIAN_POINT('Ctrl Pts',(-11.1760130389459,16.2188899984606,3.43515701789258));
#97269=CARTESIAN_POINT('Ctrl Pts',(-11.1753702193692,16.2181748612839,3.42439478912335));
#97270=CARTESIAN_POINT('Ctrl Pts',(-11.1733955579491,16.2164048921591,3.39753672198264));
#97271=CARTESIAN_POINT('Ctrl Pts',(-11.17188023436,16.2153583984105,3.38145621285716));
#97272=CARTESIAN_POINT('Ctrl Pts',(-11.1637817864671,16.2108150128535,3.31105317648322));
#97273=CARTESIAN_POINT('Ctrl Pts',(-11.1537480058582,16.2074373869853,3.25719259216043));
#97274=CARTESIAN_POINT('Ctrl Pts',(-11.1196418042736,16.1990424188514,3.12573880379287));
#97275=CARTESIAN_POINT('Ctrl Pts',(-11.0912322294689,16.1940286445765,3.04957871392895));
#97276=CARTESIAN_POINT('Ctrl Pts',(-11.0485315156706,16.1877581862416,2.96343302109303));
#97277=CARTESIAN_POINT('Ctrl Pts',(-11.0415757573983,16.1867665725221,2.95005239337552));
#97278=CARTESIAN_POINT('Ctrl Pts',(-11.0311816900047,16.1853243057663,2.93096247280851));
#97279=CARTESIAN_POINT('Ctrl Pts',(-11.0279486510086,16.1848808525471,2.92514266728035));
#97280=CARTESIAN_POINT('Ctrl Pts',(-11.022174739153,16.1840976618363,2.91495349821784));
#97281=CARTESIAN_POINT('Ctrl Pts',(-11.0196547342581,16.1837586733844,2.91057245725058));
#97282=CARTESIAN_POINT('Ctrl Pts',(-11.0147577968373,16.1831052577301,2.90218449286436));
#97283=CARTESIAN_POINT('Ctrl Pts',(-11.0123851295821,16.1827909886554,2.89817517902933));
#97284=CARTESIAN_POINT('Ctrl Pts',(-11.0061964560348,16.1819771542547,2.88785777160712));
#97285=CARTESIAN_POINT('Ctrl Pts',(-11.0023449418329,16.1814763097253,2.8815713224651));
#97286=CARTESIAN_POINT('Ctrl Pts',(-10.9876822974165,16.1795901425581,2.8581357549737));
#97287=CARTESIAN_POINT('Ctrl Pts',(-10.9764885523315,16.1781909210222,2.84123141525989));
#97288=CARTESIAN_POINT('Ctrl Pts',(-10.9473006139978,16.174638326209,2.79953247481193));
#97289=CARTESIAN_POINT('Ctrl Pts',(-10.9287657176189,16.172466070771,2.77513644367566));
#97290=CARTESIAN_POINT('Ctrl Pts',(-10.8621339944376,16.1649341722304,2.69419088002059));
#97291=CARTESIAN_POINT('Ctrl Pts',(-10.8096567822685,16.159442653724,2.64147936607834));
#97292=CARTESIAN_POINT('Ctrl Pts',(-10.7173604083933,16.1506797736799,2.56480750142563));
#97293=CARTESIAN_POINT('Ctrl Pts',(-10.6804649503172,16.1473746905649,2.53762823785868));
#97294=CARTESIAN_POINT('Ctrl Pts',(-10.6370360887088,16.1437739843242,2.50938593056304));
#97295=CARTESIAN_POINT('Ctrl Pts',(-10.6319704890512,16.1433582589938,2.50614663171684));
#97296=CARTESIAN_POINT('Ctrl Pts',(-10.6238252127735,16.142696856501,2.50102543151368));
#97297=CARTESIAN_POINT('Ctrl Pts',(-10.6207613892584,16.1424496547698,2.49911869681951));
#97298=CARTESIAN_POINT('Ctrl Pts',(-10.6153026851348,16.1420120954631,2.4957562437264));
#97299=CARTESIAN_POINT('Ctrl Pts',(-10.6129113148018,16.1418213827023,2.49429495518447));
#97300=CARTESIAN_POINT('Ctrl Pts',(-10.6077610925512,16.1414127559472,2.49117301524958));
#97301=CARTESIAN_POINT('Ctrl Pts',(-10.6050006367243,16.1411950194844,2.48951513570398));
#97302=CARTESIAN_POINT('Ctrl Pts',(-10.5973173725961,16.1405924381029,2.48494347834722));
#97303=CARTESIAN_POINT('Ctrl Pts',(-10.5923800008438,16.140209124375,2.482054164676));
#97304=CARTESIAN_POINT('Ctrl Pts',(-10.563786695884,16.138010577551,2.46560006922446));
#97305=CARTESIAN_POINT('Ctrl Pts',(-10.5396843002631,16.1362408546049,2.45282294520855));
#97306=CARTESIAN_POINT('Ctrl Pts',(-10.4758661271673,16.1317115594384,2.42178128547248));
#97307=CARTESIAN_POINT('Ctrl Pts',(-10.4355386100046,16.1290004131391,2.40486951348911));
#97308=CARTESIAN_POINT('Ctrl Pts',(-10.3496063399594,16.123358642311,2.37433286219889));
#97309=CARTESIAN_POINT('Ctrl Pts',(-10.303930128911,16.1204339985987,2.36115084987585));
#97310=CARTESIAN_POINT('Ctrl Pts',(-10.2102449955396,16.1144105367713,2.34015273091622));
#97311=CARTESIAN_POINT('Ctrl Pts',(-10.1623007627449,16.1113148567481,2.33247859112658));
#97312=CARTESIAN_POINT('Ctrl Pts',(-10.1046987783066,16.1075085993253,2.32687553621102));
#97313=CARTESIAN_POINT('Ctrl Pts',(-10.0953634708839,16.1068891345141,2.32607979750357));
#97314=CARTESIAN_POINT('Ctrl Pts',(-10.0799113289411,16.1058590051262,2.3249481898576));
#97315=CARTESIAN_POINT('Ctrl Pts',(-10.0737994812606,16.1054503235702,2.32454850751636));
#97316=CARTESIAN_POINT('Ctrl Pts',(-10.0627167799741,16.1047069027666,2.32391053404979));
#97317=CARTESIAN_POINT('Ctrl Pts',(-10.0577469736507,16.1043726748621,2.32365604003823));
#97318=CARTESIAN_POINT('Ctrl Pts',(-10.0480886605663,16.1037214111156,2.32322280936124));
#97319=CARTESIAN_POINT('Ctrl Pts',(-10.0434003979779,16.10340449037,2.32304057842494));
#97320=CARTESIAN_POINT('Ctrl Pts',(-10.0330862992218,16.1027054818534,2.32270138309461));
#97321=CARTESIAN_POINT('Ctrl Pts',(-10.0274602017258,16.1023230194205,2.32255672239816));
#97322=CARTESIAN_POINT('Ctrl Pts',(-10.0135673260802,16.1013756067731,2.32229912919589));
#97323=CARTESIAN_POINT('Ctrl Pts',(-10.0053000890746,16.1008092290808,2.32223291079363));
#97324=CARTESIAN_POINT('Ctrl Pts',(-9.93473820482176,16.0959522031599,2.32241067037843));
#97325=CARTESIAN_POINT('Ctrl Pts',(-9.87257431215225,16.0915127275951,2.32750857337014));
#97326=CARTESIAN_POINT('Ctrl Pts',(-9.81110382412688,16.0869811837922,2.33749696893276));
#97327=CARTESIAN_POINT('Ctrl Pts',(-9.81110406371144,15.9888353687451,2.33749693000248));
#97328=CARTESIAN_POINT('Ctrl Pts',(-9.82133771573714,15.9895626898729,2.33583405673277));
#97329=CARTESIAN_POINT('Ctrl Pts',(-9.83159334100925,15.990284118573,2.33430631312731));
#97330=CARTESIAN_POINT('Ctrl Pts',(-9.84597389410354,15.9912840874479,2.33235785149294));
#97331=CARTESIAN_POINT('Ctrl Pts',(-9.85008252380784,15.9915684616825,2.33182322403291));
#97332=CARTESIAN_POINT('Ctrl Pts',(-9.85704846604702,15.9920482634948,2.33095415126994));
#97333=CARTESIAN_POINT('Ctrl Pts',(-9.8599043141404,15.992244304081,2.33060847575621));
#97334=CARTESIAN_POINT('Ctrl Pts',(-9.86538829123958,15.9926194429707,2.32996506651554));
#97335=CARTESIAN_POINT('Ctrl Pts',(-9.8680161832272,15.9927986337989,2.32966571862036));
#97336=CARTESIAN_POINT('Ctrl Pts',(-9.87432461832978,15.9932274657452,2.32896863186599));
#97337=CARTESIAN_POINT('Ctrl Pts',(-9.87800610081821,15.9934766402319,2.32857938544761));
#97338=CARTESIAN_POINT('Ctrl Pts',(-9.89140921393852,15.9943800648311,2.3272261338329));
#97339=CARTESIAN_POINT('Ctrl Pts',(-9.90114123387,15.9950288877394,2.32636570446306));
#97340=CARTESIAN_POINT('Ctrl Pts',(-9.97119418477143,15.9996551213019,2.32104976953188));
#97341=CARTESIAN_POINT('Ctrl Pts',(-10.0317764879289,16.0034236396761,2.32112527908273));
#97342=CARTESIAN_POINT('Ctrl Pts',(-10.1440973668961,16.0103999893853,2.32993493739083));
#97343=CARTESIAN_POINT('Ctrl Pts',(-10.1957731744748,16.0136059774717,2.33746442224576));
#97344=CARTESIAN_POINT('Ctrl Pts',(-10.2781717815971,16.0188955734774,2.35512171145559));
#97345=CARTESIAN_POINT('Ctrl Pts',(-10.3092744674143,16.0209337320896,2.36312933802495));
#97346=CARTESIAN_POINT('Ctrl Pts',(-10.3601775249149,16.0243700859389,2.37847829188075));
#97347=CARTESIAN_POINT('Ctrl Pts',(-10.3801776063132,16.0257466106985,2.38509924653422));
#97348=CARTESIAN_POINT('Ctrl Pts',(-10.4071958585967,16.0276476315504,2.39485507065346));
#97349=CARTESIAN_POINT('Ctrl Pts',(-10.4143775518253,16.0281569906098,2.39752776813885));
#97350=CARTESIAN_POINT('Ctrl Pts',(-10.4264055923121,16.0290171492364,2.40213818300635));
#97351=CARTESIAN_POINT('Ctrl Pts',(-10.4312661338857,16.0293666989009,2.40403840458048));
#97352=CARTESIAN_POINT('Ctrl Pts',(-10.4408435141628,16.0300594211834,2.40785624422752));
#97353=CARTESIAN_POINT('Ctrl Pts',(-10.4455608671857,16.030402534406,2.40977227173452));
#97354=CARTESIAN_POINT('Ctrl Pts',(-10.4569941187558,16.0312388596365,2.41450266651829));
#97355=CARTESIAN_POINT('Ctrl Pts',(-10.4636965554463,16.0317331304739,2.41734881614791));
#97356=CARTESIAN_POINT('Ctrl Pts',(-10.4826559440417,16.0331429095534,2.42560815684214));
#97357=CARTESIAN_POINT('Ctrl Pts',(-10.4948471717376,16.0340633450591,2.43116846798682));
#97358=CARTESIAN_POINT('Ctrl Pts',(-10.5843742428374,16.0409288710067,2.47386097513836));
#97359=CARTESIAN_POINT('Ctrl Pts',(-10.6575276511688,16.0471602678752,2.51912964463413));
#97360=CARTESIAN_POINT('Ctrl Pts',(-10.7815667375091,16.0587176951414,2.61604153736333));
#97361=CARTESIAN_POINT('Ctrl Pts',(-10.8338917785618,16.0639920374312,2.6652210792401));
#97362=CARTESIAN_POINT('Ctrl Pts',(-10.8862120951529,16.0694832877704,2.72425824640106));
#97363=CARTESIAN_POINT('Ctrl Pts',(-10.8909490987023,16.0699825662486,2.72970339743013));
#97364=CARTESIAN_POINT('Ctrl Pts',(-10.8979287029348,16.0707209479235,2.7378769304044));
#97365=CARTESIAN_POINT('Ctrl Pts',(-10.9002094624161,16.0709626764705,2.74057228562283));
#97366=CARTESIAN_POINT('Ctrl Pts',(-10.9040988093348,16.0713755976844,2.7452107789829));
#97367=CARTESIAN_POINT('Ctrl Pts',(-10.9057133090767,16.071547213126,2.74714886769814));
#97368=CARTESIAN_POINT('Ctrl Pts',(-10.9093665185266,16.0719360022265,2.75156303925267));
#97369=CARTESIAN_POINT('Ctrl Pts',(-10.9114013482751,16.0721528972581,2.75404227183201));
#97370=CARTESIAN_POINT('Ctrl Pts',(-10.9169101267477,16.0727411130499,2.76081034666278));
#97371=CARTESIAN_POINT('Ctrl Pts',(-10.9203641506507,16.073111051132,2.76511541225862));
#97372=CARTESIAN_POINT('Ctrl Pts',(-10.9373683627061,16.0749388049652,2.78661725459034));
#97373=CARTESIAN_POINT('Ctrl Pts',(-10.9504684471702,16.0763678399686,2.80416649384458));
#97374=CARTESIAN_POINT('Ctrl Pts',(-10.9757770783032,16.0791949541197,2.84012024148955));
#97375=CARTESIAN_POINT('Ctrl Pts',(-10.9879723691913,16.0805921245025,2.85852287862174));
#97376=CARTESIAN_POINT('Ctrl Pts',(-11.0522376619671,16.0882163907024,2.96168346345309));
#97377=CARTESIAN_POINT('Ctrl Pts',(-11.0939233510033,16.094207179116,3.05242768150119));
#97378=CARTESIAN_POINT('Ctrl Pts',(-11.1319664499123,16.1023495501806,3.17364509011271));
#97379=CARTESIAN_POINT('Ctrl Pts',(-11.1392969674781,16.1041409095899,3.20023709407712));
#97380=CARTESIAN_POINT('Ctrl Pts',(-11.1476450808248,16.1065201767902,3.23527899252488));
#97381=CARTESIAN_POINT('Ctrl Pts',(-11.1495145066207,16.1070809165594,3.24351835109228));
#97382=CARTESIAN_POINT('Ctrl Pts',(-11.1524301602058,16.1080037117448,3.25704158123248));
#97383=CARTESIAN_POINT('Ctrl Pts',(-11.1535290946224,16.1083640886026,3.26231387583481));
#97384=CARTESIAN_POINT('Ctrl Pts',(-11.1555885514673,16.1090646916328,3.27254522258486));
#97385=CARTESIAN_POINT('Ctrl Pts',(-11.1565534093225,16.1094047721667,3.27750328976581));
#97386=CARTESIAN_POINT('Ctrl Pts',(-11.1587141358635,16.1101947746593,3.28900046672267));
#97387=CARTESIAN_POINT('Ctrl Pts',(-11.1598865847367,16.1106454242749,3.29554374773423));
#97388=CARTESIAN_POINT('Ctrl Pts',(-11.1635291675291,16.1121207675244,3.31691300770058));
#97389=CARTESIAN_POINT('Ctrl Pts',(-11.165770810196,16.1131525610158,3.33177588709594));
#97390=CARTESIAN_POINT('Ctrl Pts',(-11.1783439126348,16.1198394444715,3.42753423208055));
#97391=CARTESIAN_POINT('Ctrl Pts',(-11.1805317880148,16.1257488657217,3.50926088729189));
#97392=CARTESIAN_POINT('Ctrl Pts',(-11.1700811702948,16.1357255743591,3.64479689409002));
#97393=CARTESIAN_POINT('Ctrl Pts',(-11.1621426596776,16.1397340630886,3.69869850937178));
#97394=CARTESIAN_POINT('Ctrl Pts',(-11.1470621793525,16.1447899698767,3.7675866089842));
#97395=CARTESIAN_POINT('Ctrl Pts',(-11.143297178715,16.145934055025,3.78324168552712));
#97396=CARTESIAN_POINT('Ctrl Pts',(-11.1364835253495,16.1478191321952,3.80921824525672));
#97397=CARTESIAN_POINT('Ctrl Pts',(-11.133612380222,16.1485677494038,3.81958366444777));
#97398=CARTESIAN_POINT('Ctrl Pts',(-11.1294388211204,16.1495944109884,3.83388647983951));
#97399=CARTESIAN_POINT('Ctrl Pts',(-11.1282571136758,16.1498788172146,3.83785813416692));
#97400=CARTESIAN_POINT('Ctrl Pts',(-11.1262195250046,16.1503586570704,3.8445764349187));
#97401=CARTESIAN_POINT('Ctrl Pts',(-11.1253745036843,16.1505547039314,3.84732630930728));
#97402=CARTESIAN_POINT('Ctrl Pts',(-11.1237332759864,16.150929842244,3.85259832898702));
#97403=CARTESIAN_POINT('Ctrl Pts',(-11.1229386420303,16.1511090262942,3.8551209142694));
#97404=CARTESIAN_POINT('Ctrl Pts',(-11.121011483844,16.1515378255512,3.86116757457415));
#97405=CARTESIAN_POINT('Ctrl Pts',(-11.1198708213881,16.151786974285,3.86468905681593));
#97406=CARTESIAN_POINT('Ctrl Pts',(-11.1156603241457,16.1526901688692,3.87748176270571));
#97407=CARTESIAN_POINT('Ctrl Pts',(-11.1124917019643,16.1533387912383,3.8867204008253));
#97408=CARTESIAN_POINT('Ctrl Pts',(-11.0888520214821,16.1579694826666,3.95294944607229));
#97409=CARTESIAN_POINT('Ctrl Pts',(-11.0641247160084,16.1617421454723,4.0083330126374));
#97410=CARTESIAN_POINT('Ctrl Pts',(-11.0103106359171,16.1687304137825,4.10753740695604));
#97411=CARTESIAN_POINT('Ctrl Pts',(-10.9823448350934,16.1719441137074,4.15178808421861));
#97412=CARTESIAN_POINT('Ctrl Pts',(-10.9326821906513,16.1772348495155,4.2198765342117));
#97413=CARTESIAN_POINT('Ctrl Pts',(-10.9127882786581,16.1792658194929,4.24494000853302));
#97414=CARTESIAN_POINT('Ctrl Pts',(-10.878179474341,16.1826912328201,4.28507149849349));
#97415=CARTESIAN_POINT('Ctrl Pts',(-10.8640363677881,16.1840641907022,4.30061071307899));
#97416=CARTESIAN_POINT('Ctrl Pts',(-10.8441835819076,16.1859610568706,4.32128420480624));
#97417=CARTESIAN_POINT('Ctrl Pts',(-10.8388276255506,16.1864699158548,4.32675381766051));
#97418=CARTESIAN_POINT('Ctrl Pts',(-10.8297324574212,16.1873294691158,4.33586262694271));
#97419=CARTESIAN_POINT('Ctrl Pts',(-10.8260216427965,16.1876789174567,4.3395299435722));
#97420=CARTESIAN_POINT('Ctrl Pts',(-10.8186405311911,16.1883716263678,4.34672822138231));
#97421=CARTESIAN_POINT('Ctrl Pts',(-10.8149714523703,16.1887148286992,4.35026027227464));
#97422=CARTESIAN_POINT('Ctrl Pts',(-10.805996154168,16.1895517027643,4.35878890472202));
#97423=CARTESIAN_POINT('Ctrl Pts',(-10.8006662949916,16.1900464366609,4.36376018854541));
#97424=CARTESIAN_POINT('Ctrl Pts',(-10.7853895098545,16.1914584102911,4.37774630951553));
#97425=CARTESIAN_POINT('Ctrl Pts',(-10.7753343968011,16.1923805996083,4.38664074646383));
#97426=CARTESIAN_POINT('Ctrl Pts',(-10.7004023843767,16.1992034854541,4.45067381455465));
#97427=CARTESIAN_POINT('Ctrl Pts',(-10.6298796753538,16.2053857323667,4.49879458241126));
#97428=CARTESIAN_POINT('Ctrl Pts',(-10.5157505747271,16.214885050189,4.55974358664123));
#97429=CARTESIAN_POINT('Ctrl Pts',(-10.4755515643365,16.2181406035232,4.57838125565397));
#97430=CARTESIAN_POINT('Ctrl Pts',(-10.4063321908636,16.2235156770109,4.60584849291678));
#97431=CARTESIAN_POINT('Ctrl Pts',(-10.3778462985437,16.22566487498,4.61590289523009));
#97432=CARTESIAN_POINT('Ctrl Pts',(-10.3434039232958,16.2281653776134,4.6265891767042));
#97433=CARTESIAN_POINT('Ctrl Pts',(-10.3377920052598,16.2285697349649,4.62828453519778));
#97434=CARTESIAN_POINT('Ctrl Pts',(-10.3290493868186,16.2291946674267,4.63085460006933));
#97435=CARTESIAN_POINT('Ctrl Pts',(-10.3259274266984,16.2294168418209,4.63175833932777));
#97436=CARTESIAN_POINT('Ctrl Pts',(-10.320112123416,16.2298288029068,4.63341568386164));
#97437=CARTESIAN_POINT('Ctrl Pts',(-10.3174198541804,16.2300187701505,4.63417261490602));
#97438=CARTESIAN_POINT('Ctrl Pts',(-10.311236126593,16.2304533901902,4.63588742531048));
#97439=CARTESIAN_POINT('Ctrl Pts',(-10.3077429278617,16.2306976693299,4.63683880154835));
#97440=CARTESIAN_POINT('Ctrl Pts',(-10.2985232293794,16.231339277372,4.63930418581432));
#97441=CARTESIAN_POINT('Ctrl Pts',(-10.2927895116566,16.2317351236611,4.64079115167677));
#97442=CARTESIAN_POINT('Ctrl Pts',(-10.2479922378394,16.2348049499646,4.65204874816163));
#97443=CARTESIAN_POINT('Ctrl Pts',(-10.2084574287688,16.2373790340174,4.65985461624273));
#97444=CARTESIAN_POINT('Ctrl Pts',(-10.0727546103486,16.2459952586544,4.67948276372478));
#97445=CARTESIAN_POINT('Ctrl Pts',(-9.97557150159121,16.2518276129777,4.68147232377816));
#97446=CARTESIAN_POINT('Ctrl Pts',(-9.84797169967027,16.2600117410299,4.66831951699021));
#97447=CARTESIAN_POINT('Ctrl Pts',(-9.81684836518294,16.2620468129897,4.66384633915313));
#97448=CARTESIAN_POINT('Ctrl Pts',(-9.77726026334366,16.2647035082044,4.65652930816957));
#97449=CARTESIAN_POINT('Ctrl Pts',(-9.76859588091271,16.2652891528382,4.65482689506701));
#97450=CARTESIAN_POINT('Ctrl Pts',(-9.75459766416253,16.266242492794,4.65191261113007));
#97451=CARTESIAN_POINT('Ctrl Pts',(-9.74925158365039,16.2666082859979,4.65076070496727));
#97452=CARTESIAN_POINT('Ctrl Pts',(-9.73901245936488,16.2673122324694,4.6484797696836));
#97453=CARTESIAN_POINT('Ctrl Pts',(-9.73411822306649,16.2676501926585,4.64735659543492));
#97454=CARTESIAN_POINT('Ctrl Pts',(-9.72294748559648,16.2684250184578,4.64471771967401));
#97455=CARTESIAN_POINT('Ctrl Pts',(-9.71667601261238,16.2688625252691,4.6431816429413));
#97456=CARTESIAN_POINT('Ctrl Pts',(-9.69687841022296,16.2702517525231,4.63815968520796));
#97457=CARTESIAN_POINT('Ctrl Pts',(-9.68340192795734,16.2712094699663,4.63448481645923));
#97458=CARTESIAN_POINT('Ctrl Pts',(-9.57622341298217,16.2789261701173,4.60320018852827));
#97459=CARTESIAN_POINT('Ctrl Pts',(-9.48623922667448,16.2860672923297,4.56427416158616));
#97460=CARTESIAN_POINT('Ctrl Pts',(-9.34955970974919,16.2977113381803,4.48373932751434));
#97461=CARTESIAN_POINT('Ctrl Pts',(-9.2994859919604,16.3021688878292,4.44873468758854));
#97462=CARTESIAN_POINT('Ctrl Pts',(-9.24669884863713,16.3069257639448,4.40536503090052));
#97463=CARTESIAN_POINT('Ctrl Pts',(-9.24109563625759,16.3074314118141,4.4006734354316));
#97464=CARTESIAN_POINT('Ctrl Pts',(-9.23283679958694,16.3081773297637,4.39362647629217));
#97465=CARTESIAN_POINT('Ctrl Pts',(-9.23014769754052,16.3084203019459,4.3913108820338));
#97466=CARTESIAN_POINT('Ctrl Pts',(-9.22536242867823,16.3088527859221,4.38715245862571));
#97467=CARTESIAN_POINT('Ctrl Pts',(-9.22326231131236,16.3090426262816,4.38531430309483));
#97468=CARTESIAN_POINT('Ctrl Pts',(-9.21869183028347,16.3094558476884,4.38128514615377));
#97469=CARTESIAN_POINT('Ctrl Pts',(-9.21622413908398,16.3096790086034,4.37909121564128));
#97470=CARTESIAN_POINT('Ctrl Pts',(-9.2093472967844,16.3103011656198,4.37292530132507));
#97471=CARTESIAN_POINT('Ctrl Pts',(-9.20495881471525,16.3106985022221,4.36893025966334));
#97472=CARTESIAN_POINT('Ctrl Pts',(-9.18016407865495,16.3129464759562,4.34601333449227));
#97473=CARTESIAN_POINT('Ctrl Pts',(-9.16040152362958,16.3147500995326,4.32640437104746));
#97474=CARTESIAN_POINT('Ctrl Pts',(-9.07308786107419,16.3228810530056,4.23340012776656));
#97475=CARTESIAN_POINT('Ctrl Pts',(-9.01433434755161,16.3288572348687,4.15230967285393));
#97476=CARTESIAN_POINT('Ctrl Pts',(-8.94705074494222,16.3377250535337,4.02918625624462));
#97477=CARTESIAN_POINT('Ctrl Pts',(-8.92945381013598,16.3403315303219,3.99261600887378));
#97478=CARTESIAN_POINT('Ctrl Pts',(-8.91008861238699,16.343632572551,3.94640722097116));
#97479=CARTESIAN_POINT('Ctrl Pts',(-8.90650526802961,16.3442651225191,3.93755628446393));
#97480=CARTESIAN_POINT('Ctrl Pts',(-8.90098227911052,16.345276087643,3.92342267952988));
#97481=CARTESIAN_POINT('Ctrl Pts',(-8.89897213910695,16.3456521501793,3.91816786586369));
#97482=CARTESIAN_POINT('Ctrl Pts',(-8.89525142569963,16.3463639176573,3.90822851383324));
#97483=CARTESIAN_POINT('Ctrl Pts',(-8.89353280024487,16.3466993468808,3.90354710564479));
#97484=CARTESIAN_POINT('Ctrl Pts',(-8.88971831324223,16.3474592008359,3.89294915177128));
#97485=CARTESIAN_POINT('Ctrl Pts',(-8.88763992847873,16.3478841901918,3.88702652165376));
#97486=CARTESIAN_POINT('Ctrl Pts',(-8.88241478252164,16.3489816342205,3.87174695175587));
#97487=CARTESIAN_POINT('Ctrl Pts',(-8.87933819909121,16.3496563540756,3.86236670944295));
#97488=CARTESIAN_POINT('Ctrl Pts',(-8.85643098424019,16.3549107463391,3.7894411739625));
#97489=CARTESIAN_POINT('Ctrl Pts',(-8.84190555417357,16.3596617099307,3.72436748884922));
#97490=CARTESIAN_POINT('Ctrl Pts',(-8.83208570707783,16.3649821538915,3.65202938328167));
#97491=CARTESIAN_POINT('Ctrl Pts',(-8.8312700210513,16.365453344705,3.64562611035618));
#97492=CARTESIAN_POINT('Ctrl Pts',(-8.82273383045644,16.3707317182036,3.57391755127616));
#97493=CARTESIAN_POINT('Ctrl Pts',(-8.82044311593317,16.3756014686227,3.50808180334307));
#97494=CARTESIAN_POINT('Ctrl Pts',(-8.82499438793023,16.3822979207438,3.41513618323579));
#97495=CARTESIAN_POINT('Ctrl Pts',(-8.8272767507511,16.3842352875929,3.38792631427647));
#97496=CARTESIAN_POINT('Ctrl Pts',(-8.83117710238743,16.3865226469574,3.35515303568866));
#97497=CARTESIAN_POINT('Ctrl Pts',(-8.8318924622395,16.3869160095783,3.34949288192472));
#97498=CARTESIAN_POINT('Ctrl Pts',(-8.83307535350468,16.3875276718815,3.34065046547315));
#97499=CARTESIAN_POINT('Ctrl Pts',(-8.83351482633561,16.3877474662511,3.33746463460998));
#97500=CARTESIAN_POINT('Ctrl Pts',(-8.83436162215641,16.3881573925859,3.33150642121161));
#97501=CARTESIAN_POINT('Ctrl Pts',(-8.83476578594771,16.3883476872922,3.3287337143047));
#97502=CARTESIAN_POINT('Ctrl Pts',(-8.83571357511416,16.3887820073147,3.32239023550879));
#97503=CARTESIAN_POINT('Ctrl Pts',(-8.83626373388499,16.3890256655683,3.31882049945662));
#97504=CARTESIAN_POINT('Ctrl Pts',(-8.83777552325451,16.3896734803508,3.30930223752508));
#97505=CARTESIAN_POINT('Ctrl Pts',(-8.8387664126618,16.3900760692815,3.303358370721));
#97506=CARTESIAN_POINT('Ctrl Pts',(-8.8478453478716,16.3935828563476,3.25136177888419));
#97507=CARTESIAN_POINT('Ctrl Pts',(-8.85862469037331,16.3965518524802,3.20581496961919));
#97508=CARTESIAN_POINT('Ctrl Pts',(-8.89191910443324,16.4037818806706,3.09503036160322));
#97509=CARTESIAN_POINT('Ctrl Pts',(-8.91750609203828,16.407980916882,3.030904204702));
#97510=CARTESIAN_POINT('Ctrl Pts',(-8.96354710870661,16.4143869389582,2.9396715097105));
#97511=CARTESIAN_POINT('Ctrl Pts',(-8.97979241931128,16.4164967461762,2.91061146398605));
#97512=CARTESIAN_POINT('Ctrl Pts',(-9.0048620471992,16.4195837411277,2.86991555773456));
#97513=CARTESIAN_POINT('Ctrl Pts',(-9.01270644770618,16.4205287454575,2.85769371584797));
#97514=CARTESIAN_POINT('Ctrl Pts',(-9.02716639027976,16.4222366843771,2.83605559575335));
#97515=CARTESIAN_POINT('Ctrl Pts',(-9.03369781929854,16.4229965531211,2.82658520628969));
#97516=CARTESIAN_POINT('Ctrl Pts',(-9.04387015332391,16.4241635237356,2.81228836156548));
#97517=CARTESIAN_POINT('Ctrl Pts',(-9.04741135321145,16.4245668478608,2.80739156152264));
#97518=CARTESIAN_POINT('Ctrl Pts',(-9.05364826772389,16.4252722753384,2.79890542047901));
#97519=CARTESIAN_POINT('Ctrl Pts',(-9.05632713247397,16.4255737260021,2.7953038039316));
#97520=CARTESIAN_POINT('Ctrl Pts',(-9.0624078464814,16.4262545891716,2.78722540036863));
#97521=CARTESIAN_POINT('Ctrl Pts',(-9.06582127797874,16.426634447486,2.78275750987397));
#97522=CARTESIAN_POINT('Ctrl Pts',(-9.07510762337179,16.4276617083086,2.77078122636609));
#97523=CARTESIAN_POINT('Ctrl Pts',(-9.08103981209053,16.4283114297584,2.76331954560225));
#97524=CARTESIAN_POINT('Ctrl Pts',(-9.10929080948203,16.4313763221343,2.72865688474996));
#97525=CARTESIAN_POINT('Ctrl Pts',(-9.13272863742849,16.4338360162314,2.70239546192801));
#97526=CARTESIAN_POINT('Ctrl Pts',(-9.21289066595661,16.4419967215126,2.62029265697193));
#97527=CARTESIAN_POINT('Ctrl Pts',(-9.27409832693256,16.4478674125842,2.5691454845482));
#97528=CARTESIAN_POINT('Ctrl Pts',(-9.37961365346763,16.4571966177346,2.49774981730174));
#97529=CARTESIAN_POINT('Ctrl Pts',(-9.42084540212068,16.4606707835839,2.47337174494598));
#97530=CARTESIAN_POINT('Ctrl Pts',(-9.47198862096057,16.4646933608285,2.4471984774303));
#97531=CARTESIAN_POINT('Ctrl Pts',(-9.48058051179468,16.4653597867481,2.44293308044216));
#97532=CARTESIAN_POINT('Ctrl Pts',(-9.49279198696394,16.466292855256,2.43705561077228));
#97533=CARTESIAN_POINT('Ctrl Pts',(-9.49636878467829,16.4665644634172,2.43535623649025));
#97534=CARTESIAN_POINT('Ctrl Pts',(-9.50252832256023,16.4670292099546,2.4324677633927));
#97535=CARTESIAN_POINT('Ctrl Pts',(-9.505106902609,16.4672228730952,2.43126992700627));
#97536=CARTESIAN_POINT('Ctrl Pts',(-9.51048228042158,16.4676246990225,2.42879651173683));
#97537=CARTESIAN_POINT('Ctrl Pts',(-9.51327975695162,16.4678327657488,2.42752253328754));
#97538=CARTESIAN_POINT('Ctrl Pts',(-9.52069575729485,16.4683816437886,2.42418025984194));
#97539=CARTESIAN_POINT('Ctrl Pts',(-9.52532274187637,16.4687213404432,2.42213072530875));
#97540=CARTESIAN_POINT('Ctrl Pts',(-9.54516890525096,16.4701672103479,2.41349239913891));
#97541=CARTESIAN_POINT('Ctrl Pts',(-9.56051397076029,16.4712572096055,2.40719526437053));
#97542=CARTESIAN_POINT('Ctrl Pts',(-9.65201486779166,16.4776221027912,2.37188552873384));
#97543=CARTESIAN_POINT('Ctrl Pts',(-9.73081204459537,16.4825706016215,2.35054363630281));
#97544=CARTESIAN_POINT('Ctrl Pts',(-9.81110406371068,16.4876146309988,2.3374969300026));
#97545=CARTESIAN_POINT('Origin',(-10.,12.3756328852638,3.5));
#97546=CARTESIAN_POINT('',(-9.81110406370895,17.0855891663962,2.33749693000288));
#97547=CARTESIAN_POINT('',(-9.81110406885758,16.9868193101849,2.33749692916628));
#97548=CARTESIAN_POINT('',(-9.81110406371068,12.3756328852638,2.3374969300026));
#97549=CARTESIAN_POINT('Ctrl Pts',(-9.81110406370722,17.0855891663962,2.33749693000316));
#97550=CARTESIAN_POINT('Ctrl Pts',(-9.81046679021848,17.0855476087213,2.33760048101772));
#97551=CARTESIAN_POINT('Ctrl Pts',(-9.80982959701639,17.0855060696787,2.3377045568435));
#97552=CARTESIAN_POINT('Ctrl Pts',(-9.76283177728797,17.0824432182907,2.34542061936591));
#97553=CARTESIAN_POINT('Ctrl Pts',(-9.71696418175036,17.0795222872894,2.35579995459459));
#97554=CARTESIAN_POINT('Ctrl Pts',(-9.58354864230442,17.0709238242386,2.39450729211066));
#97555=CARTESIAN_POINT('Ctrl Pts',(-9.49857442148061,17.0652861251475,2.43036640670373));
#97556=CARTESIAN_POINT('Ctrl Pts',(-9.40726731086784,17.0584326538379,2.48219159926921));
#97557=CARTESIAN_POINT('Ctrl Pts',(-9.39600613613032,17.0575730746573,2.4888336577192));
#97558=CARTESIAN_POINT('Ctrl Pts',(-9.37933497045112,17.056277664753,2.49904448959465));
#97559=CARTESIAN_POINT('Ctrl Pts',(-9.37383982298063,17.0558468810358,2.50247283614688));
#97560=CARTESIAN_POINT('Ctrl Pts',(-9.36439534825505,17.0550997654432,2.50847390233251));
#97561=CARTESIAN_POINT('Ctrl Pts',(-9.36043263155815,17.0547842168966,2.51102535128617));
#97562=CARTESIAN_POINT('Ctrl Pts',(-9.35224138241517,17.0541275732871,2.51636921902322));
#97563=CARTESIAN_POINT('Ctrl Pts',(-9.34801535146255,17.0537863481409,2.51916527558025));
#97564=CARTESIAN_POINT('Ctrl Pts',(-9.33811450053976,17.0529810539607,2.52580820714844));
#97565=CARTESIAN_POINT('Ctrl Pts',(-9.33245501695078,17.0525161531781,2.52967749907337));
#97566=CARTESIAN_POINT('Ctrl Pts',(-9.31386648797026,17.0509737389932,2.54262575233408));
#97567=CARTESIAN_POINT('Ctrl Pts',(-9.30108681563627,17.0498883142975,2.55191510667831));
#97568=CARTESIAN_POINT('Ctrl Pts',(-9.27111397333765,17.0472809548921,2.57463730049556));
#97569=CARTESIAN_POINT('Ctrl Pts',(-9.25410012807943,17.0457507143835,2.58829596837442));
#97570=CARTESIAN_POINT('Ctrl Pts',(-9.18893916043329,17.0396886509674,2.64365225908095));
#97571=CARTESIAN_POINT('Ctrl Pts',(-9.14383180479926,17.035036225825,2.68875068801303));
#97572=CARTESIAN_POINT('Ctrl Pts',(-9.05948926780255,17.0254733597546,2.78798524486116));
#97573=CARTESIAN_POINT('Ctrl Pts',(-9.02075587557147,17.0205783027184,2.84227048072301));
#97574=CARTESIAN_POINT('Ctrl Pts',(-8.98186453342811,17.0152333760837,2.90789402753671));
#97575=CARTESIAN_POINT('Ctrl Pts',(-8.97701822646156,17.0145583836961,2.91630691522565));
#97576=CARTESIAN_POINT('Ctrl Pts',(-8.97047167186255,17.0136349384507,2.92800337698872));
#97577=CARTESIAN_POINT('Ctrl Pts',(-8.9686821850994,17.0133812685793,2.93123618190912));
#97578=CARTESIAN_POINT('Ctrl Pts',(-8.96563854419849,17.0129477247704,2.93679628045461));
#97579=CARTESIAN_POINT('Ctrl Pts',(-8.96437697117387,17.0127673940706,2.93911944812095));
#97580=CARTESIAN_POINT('Ctrl Pts',(-8.96175755669441,17.0123916803676,2.94398202955287));
#97581=CARTESIAN_POINT('Ctrl Pts',(-8.96040119252868,17.0121963969138,2.94652220072547));
#97582=CARTESIAN_POINT('Ctrl Pts',(-8.95711069943527,17.0117207792727,2.95273934015649));
#97583=CARTESIAN_POINT('Ctrl Pts',(-8.95518665920033,17.0114410703212,2.95642166411791));
#97584=CARTESIAN_POINT('Ctrl Pts',(-8.94832139200565,17.0104369100489,2.96973188175211));
#97585=CARTESIAN_POINT('Ctrl Pts',(-8.94349324999972,17.0097190837273,2.97941794156666));
#97586=CARTESIAN_POINT('Ctrl Pts',(-8.93175853462316,17.0079411016092,3.00379568119295));
#97587=CARTESIAN_POINT('Ctrl Pts',(-8.92502073140274,17.0068893812309,3.01856653462524));
#97588=CARTESIAN_POINT('Ctrl Pts',(-8.89671119883383,17.002308366018,3.08418800896803));
#97589=CARTESIAN_POINT('Ctrl Pts',(-8.87842523642352,16.9989003530262,3.13638370946908));
#97590=CARTESIAN_POINT('Ctrl Pts',(-8.84267024961867,16.990512187509,3.26728570992747));
#97591=CARTESIAN_POINT('Ctrl Pts',(-8.82948182836423,16.9855344942284,3.34685557577684));
#97592=CARTESIAN_POINT('Ctrl Pts',(-8.82357408891377,16.9793060239926,3.44217351806597));
#97593=CARTESIAN_POINT('Ctrl Pts',(-8.82293092809327,16.9783157737234,3.45721924953858));
#97594=CARTESIAN_POINT('Ctrl Pts',(-8.82241978420988,16.9768751352034,3.47892462630338));
#97595=CARTESIAN_POINT('Ctrl Pts',(-8.82231951261462,16.9764319237513,3.48557770572016));
#97596=CARTESIAN_POINT('Ctrl Pts',(-8.82224228858446,16.975649015259,3.49728455976286));
#97597=CARTESIAN_POINT('Ctrl Pts',(-8.82224147951256,16.9753100655643,3.50233804850006));
#97598=CARTESIAN_POINT('Ctrl Pts',(-8.82230699423253,16.9746077711272,3.51277711070213));
#97599=CARTESIAN_POINT('Ctrl Pts',(-8.82237773827805,16.9742442972441,3.51816252793057));
#97600=CARTESIAN_POINT('Ctrl Pts',(-8.8226542492298,16.9733079671012,3.53198989425409));
#97601=CARTESIAN_POINT('Ctrl Pts',(-8.82291387249395,16.9727334559864,3.54043033705297));
#97602=CARTESIAN_POINT('Ctrl Pts',(-8.82440608436641,16.9702745261167,3.57636330928275));
#97603=CARTESIAN_POINT('Ctrl Pts',(-8.82651122632238,16.9683634285255,3.60380890524678));
#97604=CARTESIAN_POINT('Ctrl Pts',(-8.84066218104489,16.9594105224648,3.73009297141684));
#97605=CARTESIAN_POINT('Ctrl Pts',(-8.86424927016994,16.9520245324512,3.82721748329565));
#97606=CARTESIAN_POINT('Ctrl Pts',(-8.90764195769683,16.9431596191998,3.94083688415836));
#97607=CARTESIAN_POINT('Ctrl Pts',(-8.91610465512185,16.9415595501064,3.96125288742253));
#97608=CARTESIAN_POINT('Ctrl Pts',(-8.93407343246574,16.9384152309937,4.00137167607303));
#97609=CARTESIAN_POINT('Ctrl Pts',(-8.94356427729184,16.9368711426358,4.02107266131937));
#97610=CARTESIAN_POINT('Ctrl Pts',(-8.95613105673537,16.9349741272279,4.04540181260195));
#97611=CARTESIAN_POINT('Ctrl Pts',(-8.9586977686307,16.9345937674811,4.05028644708646));
#97612=CARTESIAN_POINT('Ctrl Pts',(-8.96281074384057,16.9339955522381,4.05798189775149));
#97613=CARTESIAN_POINT('Ctrl Pts',(-8.9643342839033,16.9337763392741,4.06080466870141));
#97614=CARTESIAN_POINT('Ctrl Pts',(-8.9670769961956,16.933385973965,4.065836989529));
#97615=CARTESIAN_POINT('Ctrl Pts',(-8.96829173085685,16.9332145543318,4.06804883422881));
#97616=CARTESIAN_POINT('Ctrl Pts',(-8.97122436935443,16.9328041996942,4.07334827819133));
#97617=CARTESIAN_POINT('Ctrl Pts',(-8.97294906800792,16.9325656975155,4.07643206905023));
#97618=CARTESIAN_POINT('Ctrl Pts',(-8.97824309549261,16.9318420067423,4.08579868835872));
#97619=CARTESIAN_POINT('Ctrl Pts',(-8.98185647123968,16.9313595057719,4.09205661596405));
#97620=CARTESIAN_POINT('Ctrl Pts',(-9.01497844139211,16.9270346022845,4.1482197382639));
#97621=CARTESIAN_POINT('Ctrl Pts',(-9.04808122037493,16.9233979857228,4.19592301216969));
#97622=CARTESIAN_POINT('Ctrl Pts',(-9.14844621490731,16.9134973582773,4.31991415718598));
#97623=CARTESIAN_POINT('Ctrl Pts',(-9.22225185970603,16.9073155831472,4.39022966756044));
#97624=CARTESIAN_POINT('Ctrl Pts',(-9.31505716518735,16.8997939520322,4.4581914785933));
#97625=CARTESIAN_POINT('Ctrl Pts',(-9.32609361793744,16.8989038707488,4.46598538307242));
#97626=CARTESIAN_POINT('Ctrl Pts',(-9.3425868326372,16.89757878004,4.47721261375785));
#97627=CARTESIAN_POINT('Ctrl Pts',(-9.34794188568081,16.8971493218907,4.48079395281557));
#97628=CARTESIAN_POINT('Ctrl Pts',(-9.35751031529124,16.8963831903709,4.48708010479039));
#97629=CARTESIAN_POINT('Ctrl Pts',(-9.36171209775898,16.8960471738355,4.48980234428691));
#97630=CARTESIAN_POINT('Ctrl Pts',(-9.37059421653031,16.8953376697608,4.49547679151794));
#97631=CARTESIAN_POINT('Ctrl Pts',(-9.37527824601759,16.8949639708928,4.49842296197901));
#97632=CARTESIAN_POINT('Ctrl Pts',(-9.38773678053448,16.893971123284,4.50613716177724));
#97633=CARTESIAN_POINT('Ctrl Pts',(-9.39554607610083,16.8933499178334,4.5108480023971));
#97634=CARTESIAN_POINT('Ctrl Pts',(-9.43337190242116,16.8903457345872,4.53307081324012));
#97635=CARTESIAN_POINT('Ctrl Pts',(-9.46409612573927,16.8879190513826,4.54933755790757));
#97636=CARTESIAN_POINT('Ctrl Pts',(-9.55607265190508,16.8806880468126,4.59294025328928));
#97637=CARTESIAN_POINT('Ctrl Pts',(-9.61898898289087,16.8757757876425,4.61643119935718));
#97638=CARTESIAN_POINT('Ctrl Pts',(-9.74237087960147,16.8663704471067,4.6508479250894));
#97639=CARTESIAN_POINT('Ctrl Pts',(-9.80238121211423,16.8618953815804,4.66265732388629));
#97640=CARTESIAN_POINT('Ctrl Pts',(-9.87272857348907,16.8569321642153,4.67089374502967));
#97641=CARTESIAN_POINT('Ctrl Pts',(-9.88242924558254,16.856254027694,4.67190755239104));
#97642=CARTESIAN_POINT('Ctrl Pts',(-9.89582688899466,16.8553270924379,4.67313968492315));
#97643=CARTESIAN_POINT('Ctrl Pts',(-9.89951363945905,16.8550730245991,4.67346122631912));
#97644=CARTESIAN_POINT('Ctrl Pts',(-9.90583803991798,16.8546389787524,4.6739827870265));
#97645=CARTESIAN_POINT('Ctrl Pts',(-9.90847493173633,16.8544585416969,4.67419130519454));
#97646=CARTESIAN_POINT('Ctrl Pts',(-9.91398260215263,16.8540828085334,4.67460817051098));
#97647=CARTESIAN_POINT('Ctrl Pts',(-9.91685347022546,16.8538876109572,4.6748148797961));
#97648=CARTESIAN_POINT('Ctrl Pts',(-9.92386323218239,16.853412533073,4.67529377570485));
#97649=CARTESIAN_POINT('Ctrl Pts',(-9.92800291460935,16.8531332746362,4.67555462979052));
#97650=CARTESIAN_POINT('Ctrl Pts',(-9.94290273489976,16.8521325583753,4.67641451088555));
#97651=CARTESIAN_POINT('Ctrl Pts',(-9.95366999172257,16.8514176659999,4.67688773883022));
#97652=CARTESIAN_POINT('Ctrl Pts',(-9.98057695314446,16.8496484258148,4.67770045409712));
#97653=CARTESIAN_POINT('Ctrl Pts',(-9.99672037902721,16.848602407392,4.67785606622607));
#97654=CARTESIAN_POINT('Ctrl Pts',(-10.0675290814311,16.8440624300346,4.67708268764603));
#97655=CARTESIAN_POINT('Ctrl Pts',(-10.1220919961041,16.8406875552156,4.67267997470266));
#97656=CARTESIAN_POINT('Ctrl Pts',(-10.2564397305442,16.8322882533554,4.65235707231739));
#97657=CARTESIAN_POINT('Ctrl Pts',(-10.3352428314476,16.827267479155,4.63194447556328));
#97658=CARTESIAN_POINT('Ctrl Pts',(-10.4254097040959,16.8209915427536,4.59833868912679));
#97659=CARTESIAN_POINT('Ctrl Pts',(-10.4394011017941,16.8200024387464,4.59281651277357));
#97660=CARTESIAN_POINT('Ctrl Pts',(-10.4594208336997,16.8185631692356,4.58446843763205));
#97661=CARTESIAN_POINT('Ctrl Pts',(-10.4655373551823,16.8181201612076,4.58185685861638));
#97662=CARTESIAN_POINT('Ctrl Pts',(-10.4762614723831,16.817337490105,4.57717018392443));
#97663=CARTESIAN_POINT('Ctrl Pts',(-10.4808784859632,16.8169985729508,4.57511695902701));
#97664=CARTESIAN_POINT('Ctrl Pts',(-10.4903902274359,16.8162962267809,4.57081347975867));
#97665=CARTESIAN_POINT('Ctrl Pts',(-10.4952830060794,16.8159326678984,4.56855922897039));
#97666=CARTESIAN_POINT('Ctrl Pts',(-10.5078102857342,16.8149958658868,4.56268300979571));
#97667=CARTESIAN_POINT('Ctrl Pts',(-10.5154214733629,16.8144209646802,4.5590123530534));
#97668=CARTESIAN_POINT('Ctrl Pts',(-10.5476977342848,16.8119579816261,4.543016073541));
#97669=CARTESIAN_POINT('Ctrl Pts',(-10.571963578543,16.8100431110478,4.52990911378482));
#97670=CARTESIAN_POINT('Ctrl Pts',(-10.6815932910367,16.8010886977025,4.46562393297571));
#97671=CARTESIAN_POINT('Ctrl Pts',(-10.7607057414638,16.7937055608505,4.40461032025047));
#97672=CARTESIAN_POINT('Ctrl Pts',(-10.8468470943442,16.7848433376907,4.31880001230056));
#97673=CARTESIAN_POINT('Ctrl Pts',(-10.8620627146949,16.783242959674,4.30276486669209));
#97674=CARTESIAN_POINT('Ctrl Pts',(-10.8913974160486,16.780100245936,4.27005358770503));
#97675=CARTESIAN_POINT('Ctrl Pts',(-10.9055223159447,16.778558016823,4.25339323448425));
#97676=CARTESIAN_POINT('Ctrl Pts',(-10.9226252177633,16.7766629460656,4.23204384545968));
#97677=CARTESIAN_POINT('Ctrl Pts',(-10.9260434525632,16.7762827369521,4.22771492432781));
#97678=CARTESIAN_POINT('Ctrl Pts',(-10.9314010143762,16.7756847055555,4.22083111652511));
#97679=CARTESIAN_POINT('Ctrl Pts',(-10.9333604799095,16.7754655271546,4.21829211557647));
#97680=CARTESIAN_POINT('Ctrl Pts',(-10.936843211606,16.7750751910268,4.21374100890536));
#97681=CARTESIAN_POINT('Ctrl Pts',(-10.9383703745719,16.7749037662661,4.21173202206325));
#97682=CARTESIAN_POINT('Ctrl Pts',(-10.9420207048064,16.7744933577783,4.20689783079863));
#97683=CARTESIAN_POINT('Ctrl Pts',(-10.9441376257478,16.7742548072074,4.20406796258569));
#97684=CARTESIAN_POINT('Ctrl Pts',(-10.950546251639,16.7735308217706,4.19542012634587));
#97685=CARTESIAN_POINT('Ctrl Pts',(-10.9547972520781,16.7730480777251,4.18957199953112));
#97686=CARTESIAN_POINT('Ctrl Pts',(-10.9927246122265,16.7687143913825,4.13637187801061));
#97687=CARTESIAN_POINT('Ctrl Pts',(-11.0229123635074,16.7650701493455,4.08662043234762));
#97688=CARTESIAN_POINT('Ctrl Pts',(-11.0953357600117,16.7551725433633,3.94453164957282));
#97689=CARTESIAN_POINT('Ctrl Pts',(-11.1295103673736,16.7490002715889,3.84867333589759));
#97690=CARTESIAN_POINT('Ctrl Pts',(-11.1538597316411,16.741488557525,3.73640198469781));
#97691=CARTESIAN_POINT('Ctrl Pts',(-11.156499641678,16.7405970818425,3.72312940828241));
#97692=CARTESIAN_POINT('Ctrl Pts',(-11.1600586039224,16.7392703083143,3.70347150478398));
#97693=CARTESIAN_POINT('Ctrl Pts',(-11.1611548935878,16.7388405825096,3.69711907088149));
#97694=CARTESIAN_POINT('Ctrl Pts',(-11.1630099469832,16.7380741506288,3.68581710490591));
#97695=CARTESIAN_POINT('Ctrl Pts',(-11.1637894052295,16.7377381032681,3.68087109278601));
#97696=CARTESIAN_POINT('Ctrl Pts',(-11.1653635145414,16.7370287164568,3.67045098363258));
#97697=CARTESIAN_POINT('Ctrl Pts',(-11.1661511848225,16.7366551668167,3.66497597150673));
#97698=CARTESIAN_POINT('Ctrl Pts',(-11.1681339912614,16.735663142874,3.65046938974396));
#97699=CARTESIAN_POINT('Ctrl Pts',(-11.1692629314907,16.7350426179546,3.64142930285573));
#97700=CARTESIAN_POINT('Ctrl Pts',(-11.1741793485423,16.7320473896077,3.59796550185208));
#97701=CARTESIAN_POINT('Ctrl Pts',(-11.176551787351,16.7296292975671,3.56340224659274));
#97702=CARTESIAN_POINT('Ctrl Pts',(-11.1790266296173,16.7224374623504,3.46218243014048));
#97703=CARTESIAN_POINT('Ctrl Pts',(-11.1750002751843,16.7175572827372,3.39556595837009));
#97704=CARTESIAN_POINT('Ctrl Pts',(-11.1564527214182,16.7081410951167,3.26867812348355));
#97705=CARTESIAN_POINT('Ctrl Pts',(-11.1427664593981,16.7036231812674,3.20848829075931));
#97706=CARTESIAN_POINT('Ctrl Pts',(-11.121530290797,16.6986208585573,3.1403336121244));
#97707=CARTESIAN_POINT('Ctrl Pts',(-11.1185145966299,16.6979429912583,3.13106204269438));
#97708=CARTESIAN_POINT('Ctrl Pts',(-11.1141958876418,16.6970163546021,3.11832438148826));
#97709=CARTESIAN_POINT('Ctrl Pts',(-11.1129912463117,16.6967623206123,3.11482570131375));
#97710=CARTESIAN_POINT('Ctrl Pts',(-11.1108972591547,16.6963283174734,3.10883591948904));
#97711=CARTESIAN_POINT('Ctrl Pts',(-11.1100159830757,16.6961478894711,3.10634205717396));
#97712=CARTESIAN_POINT('Ctrl Pts',(-11.1081581261211,16.6957721580096,3.10114048197866));
#97713=CARTESIAN_POINT('Ctrl Pts',(-11.1071800108205,16.6955769531685,3.09843335362022));
#97714=CARTESIAN_POINT('Ctrl Pts',(-11.1047680207984,16.6951018295579,3.09183350012173));
#97715=CARTESIAN_POINT('Ctrl Pts',(-11.1033234665046,16.6948225329446,3.08794466273947));
#97716=CARTESIAN_POINT('Ctrl Pts',(-11.0980511117898,16.693821525215,3.07397765652204));
#97717=CARTESIAN_POINT('Ctrl Pts',(-11.0941053879199,16.6931063845762,3.06394415293198));
#97718=CARTESIAN_POINT('Ctrl Pts',(-11.0839062608045,16.6913364051416,3.03901943641439));
#97719=CARTESIAN_POINT('Ctrl Pts',(-11.077483151736,16.6902899046701,3.02419964865728));
#97720=CARTESIAN_POINT('Ctrl Pts',(-11.0479695418317,16.6857464708914,2.95976962277652));
#97721=CARTESIAN_POINT('Ctrl Pts',(-11.0217412384253,16.6823688060979,2.9116677703047));
#97722=CARTESIAN_POINT('Ctrl Pts',(-10.9485547014756,16.6739704593492,2.79720419022072));
#97723=CARTESIAN_POINT('Ctrl Pts',(-10.8979077056219,16.6689533227418,2.73355520751759));
#97724=CARTESIAN_POINT('Ctrl Pts',(-10.8305960363268,16.6626813905185,2.66487631750318));
#97725=CARTESIAN_POINT('Ctrl Pts',(-10.8198623820013,16.6616921828514,2.65433636611574));
#97726=CARTESIAN_POINT('Ctrl Pts',(-10.8040962078388,16.6602527895318,2.63943705231074));
#97727=CARTESIAN_POINT('Ctrl Pts',(-10.7992236974778,16.6598097631011,2.63490996033136));
#97728=CARTESIAN_POINT('Ctrl Pts',(-10.7905823466195,16.6590270705259,2.62701652427092));
#97729=CARTESIAN_POINT('Ctrl Pts',(-10.7868296633359,16.6586881504307,2.62363268248148));
#97730=CARTESIAN_POINT('Ctrl Pts',(-10.7790315116823,16.657985808954,2.61669145469603));
#97731=CARTESIAN_POINT('Ctrl Pts',(-10.7749831856604,16.6576222577716,2.6131374725043));
#97732=CARTESIAN_POINT('Ctrl Pts',(-10.7645227688135,16.6566854985039,2.60408069954595));
#97733=CARTESIAN_POINT('Ctrl Pts',(-10.7580756756847,16.6561106326332,2.59861899264845));
#97734=CARTESIAN_POINT('Ctrl Pts',(-10.7303451661364,16.6536480170318,2.57563480681284));
#97735=CARTESIAN_POINT('Ctrl Pts',(-10.7085103513033,16.6517334885434,2.55879442505093));
#97736=CARTESIAN_POINT('Ctrl Pts',(-10.6052158020769,16.6427792121441,2.48475936452987));
#97737=CARTESIAN_POINT('Ctrl Pts',(-10.5173100439291,16.6353958169266,2.4372751558358));
#97738=CARTESIAN_POINT('Ctrl Pts',(-10.4038914296623,16.626533350247,2.39344898207655));
#97739=CARTESIAN_POINT('Ctrl Pts',(-10.3830564164077,16.6249330003137,2.38606493996355));
#97740=CARTESIAN_POINT('Ctrl Pts',(-10.3412438324976,16.6217901408474,2.37255836956875));
#97741=CARTESIAN_POINT('Ctrl Pts',(-10.3202782676314,16.6202477429231,2.36642425760843));
#97742=CARTESIAN_POINT('Ctrl Pts',(-10.293817803174,16.6183524955878,2.35947530284271));
#97743=CARTESIAN_POINT('Ctrl Pts',(-10.2884730176084,16.6179722727882,2.35811173602826));
#97744=CARTESIAN_POINT('Ctrl Pts',(-10.2800055976925,16.6173742246878,2.35601476684285));
#97745=CARTESIAN_POINT('Ctrl Pts',(-10.2768892923251,16.6171550431465,2.35525650522019));
#97746=CARTESIAN_POINT('Ctrl Pts',(-10.2713154406445,16.6167647043681,2.35392436438285));
#97747=CARTESIAN_POINT('Ctrl Pts',(-10.268859160078,16.6165932800741,2.35334565665642));
#97748=CARTESIAN_POINT('Ctrl Pts',(-10.2629586486451,16.6161828764827,2.35197547930999));
#97749=CARTESIAN_POINT('Ctrl Pts',(-10.2595126957486,16.6159443303115,2.35119161190009));
#97750=CARTESIAN_POINT('Ctrl Pts',(-10.2490069459777,16.6152203716675,2.34885150192244));
#97751=CARTESIAN_POINT('Ctrl Pts',(-10.2419361407016,16.6147376497243,2.34734470283849));
#97752=CARTESIAN_POINT('Ctrl Pts',(-10.1779245920784,16.6104047630613,2.33431874292132));
#97753=CARTESIAN_POINT('Ctrl Pts',(-10.120209888092,16.6067612152698,2.32696059416005));
#97754=CARTESIAN_POINT('Ctrl Pts',(-9.9781878657002,16.5979348116902,2.31945190491373));
#97755=CARTESIAN_POINT('Ctrl Pts',(-9.89401868714965,16.5928065599172,2.32402407489297));
#97756=CARTESIAN_POINT('Ctrl Pts',(-9.81110406371068,16.5874147438851,2.3374969300026));
#97757=CARTESIAN_POINT('Ctrl Pts',(-9.81110406371068,16.4876146309988,2.3374969300026));
#97758=CARTESIAN_POINT('Ctrl Pts',(-9.84043589666133,16.4894572877002,2.33273077996714));
#97759=CARTESIAN_POINT('Ctrl Pts',(-9.86996731794527,16.4913110864639,2.32907162145681));
#97760=CARTESIAN_POINT('Ctrl Pts',(-9.94136912962896,16.495834756206,2.32296481369049));
#97761=CARTESIAN_POINT('Ctrl Pts',(-9.98325815175191,16.4985234875482,2.32162462695854));
#97762=CARTESIAN_POINT('Ctrl Pts',(-10.0347595407365,16.5019168373448,2.32272361916799));
#97763=CARTESIAN_POINT('Ctrl Pts',(-10.0443895711777,16.5025550401039,2.32304738438359));
#97764=CARTESIAN_POINT('Ctrl Pts',(-10.0596534743491,16.5035729508274,2.32374815934164));
#97765=CARTESIAN_POINT('Ctrl Pts',(-10.0652906150367,16.503950249227,2.32404759307271));
#97766=CARTESIAN_POINT('Ctrl Pts',(-10.0759004530038,16.5046630559957,2.32468769003998));
#97767=CARTESIAN_POINT('Ctrl Pts',(-10.0808735804975,16.5049982791467,2.32501941829976));
#97768=CARTESIAN_POINT('Ctrl Pts',(-10.0920751269581,16.5057559155183,2.32583805931086));
#97769=CARTESIAN_POINT('Ctrl Pts',(-10.0983020379568,16.5061788799648,2.32634298081222));
#97770=CARTESIAN_POINT('Ctrl Pts',(-10.114260630331,16.5072676169004,2.32776490627188));
#97771=CARTESIAN_POINT('Ctrl Pts',(-10.1239852845258,16.5079355945176,2.32875355035896));
#97772=CARTESIAN_POINT('Ctrl Pts',(-10.1934017033005,16.512737310385,2.33668485764861));
#97773=CARTESIAN_POINT('Ctrl Pts',(-10.2524877164907,16.5170091118756,2.34806501320835));
#97774=CARTESIAN_POINT('Ctrl Pts',(-10.3850973391729,16.5269918437485,2.38430065558665));
#97775=CARTESIAN_POINT('Ctrl Pts',(-10.4575594063496,16.5327444414498,2.4120091898609));
#97776=CARTESIAN_POINT('Ctrl Pts',(-10.5524051297034,16.5403865383794,2.45944025397595));
#97777=CARTESIAN_POINT('Ctrl Pts',(-10.5775579129523,16.5424229763872,2.47318785467457));
#97778=CARTESIAN_POINT('Ctrl Pts',(-10.6071548185714,16.5448103288036,2.49079659506886));
#97779=CARTESIAN_POINT('Ctrl Pts',(-10.6121015918612,16.5452090315615,2.49378922142488));
#97780=CARTESIAN_POINT('Ctrl Pts',(-10.6197796703402,16.5458271421038,2.49851177135092));
#97781=CARTESIAN_POINT('Ctrl Pts',(-10.6225261454795,16.5460480950102,2.50021666811123));
#97782=CARTESIAN_POINT('Ctrl Pts',(-10.6276378098159,16.546459000378,2.50341900574549));
#97783=CARTESIAN_POINT('Ctrl Pts',(-10.6300046629453,16.5466491242837,2.50491355987514));
#97784=CARTESIAN_POINT('Ctrl Pts',(-10.6353918610386,16.5470815793592,2.50834224253688));
#97785=CARTESIAN_POINT('Ctrl Pts',(-10.638408717639,16.5473235551547,2.51028173952976));
#97786=CARTESIAN_POINT('Ctrl Pts',(-10.6463974175029,16.5479639096544,2.51546929501592));
#97787=CARTESIAN_POINT('Ctrl Pts',(-10.6513537111808,16.5483607772141,2.51874127929687));
#97788=CARTESIAN_POINT('Ctrl Pts',(-10.6901105517581,16.5514626688213,2.54475033682414));
#97789=CARTESIAN_POINT('Ctrl Pts',(-10.7227396030225,16.5540654437644,2.56919242355692));
#97790=CARTESIAN_POINT('Ctrl Pts',(-10.8288601498307,16.5627426212095,2.65763861017187));
#97791=CARTESIAN_POINT('Ctrl Pts',(-10.8956547703164,16.5686088564547,2.72903625055273));
#97792=CARTESIAN_POINT('Ctrl Pts',(-10.9708474196005,16.5767801744582,2.83255476962529));
#97793=CARTESIAN_POINT('Ctrl Pts',(-10.9878271183314,16.578759020161,2.85795235554662));
#97794=CARTESIAN_POINT('Ctrl Pts',(-11.008374516686,16.5813518900519,2.89143414602323));
#97795=CARTESIAN_POINT('Ctrl Pts',(-11.0128660937018,16.5819320860766,2.89893940911814));
#97796=CARTESIAN_POINT('Ctrl Pts',(-11.0200202612042,16.5828787381954,2.91120170045053));
#97797=CARTESIAN_POINT('Ctrl Pts',(-11.0227342062049,16.5832433419926,2.91592850388133));
#97798=CARTESIAN_POINT('Ctrl Pts',(-11.0278880273074,16.5839464981197,2.92505083860827));
#97799=CARTESIAN_POINT('Ctrl Pts',(-11.0303327667285,16.5842848675001,2.92944349681924));
#97800=CARTESIAN_POINT('Ctrl Pts',(-11.0358717370442,16.5850627566659,2.93954750440325));
#97801=CARTESIAN_POINT('Ctrl Pts',(-11.0389469671856,16.5855029351368,2.94526902748707));
#97802=CARTESIAN_POINT('Ctrl Pts',(-11.0485843432739,16.5869093908239,2.96356080704401));
#97803=CARTESIAN_POINT('Ctrl Pts',(-11.0549666618798,16.5878818779922,2.97622386036367));
#97804=CARTESIAN_POINT('Ctrl Pts',(-11.1026279777996,16.5954767609312,3.07519483415787));
#97805=CARTESIAN_POINT('Ctrl Pts',(-11.1334722827278,16.6024634375274,3.16611186597216));
#97806=CARTESIAN_POINT('Ctrl Pts',(-11.1657561928442,16.6140811373697,3.32103470004886));
#97807=CARTESIAN_POINT('Ctrl Pts',(-11.1736228978305,16.618662645728,3.38326441783167));
#97808=CARTESIAN_POINT('Ctrl Pts',(-11.176841670879,16.6235359481354,3.4531730027869));
#97809=CARTESIAN_POINT('Ctrl Pts',(-11.1771110000903,16.6240445759606,3.46051853164459));
#97810=CARTESIAN_POINT('Ctrl Pts',(-11.1774085988683,16.624794016462,3.47142193889978));
#97811=CARTESIAN_POINT('Ctrl Pts',(-11.1774895396561,16.6250375674893,3.4749780275111));
#97812=CARTESIAN_POINT('Ctrl Pts',(-11.1776052472068,16.625470670861,3.48132550831094));
#97813=CARTESIAN_POINT('Ctrl Pts',(-11.1776462017009,16.6256605557712,3.48411670505494));
#97814=CARTESIAN_POINT('Ctrl Pts',(-11.177713866033,16.6260733972704,3.49020343362058));
#97815=CARTESIAN_POINT('Ctrl Pts',(-11.1777366683032,16.6262961369331,3.49349894125733));
#97816=CARTESIAN_POINT('Ctrl Pts',(-11.1777617125409,16.6269159951946,3.50270069460164));
#97817=CARTESIAN_POINT('Ctrl Pts',(-11.1777333603021,16.6273114737592,3.50860702746551));
#97818=CARTESIAN_POINT('Ctrl Pts',(-11.1773231640359,16.629527998126,3.54189238095982));
#97819=CARTESIAN_POINT('Ctrl Pts',(-11.1760310104486,16.6313035554873,3.56925417175664));
#97820=CARTESIAN_POINT('Ctrl Pts',(-11.1655746513147,16.6394385320587,3.69637722184154));
#97821=CARTESIAN_POINT('Ctrl Pts',(-11.1446618696418,16.6454387494863,3.79475483951794));
#97822=CARTESIAN_POINT('Ctrl Pts',(-11.0981205948617,16.6543371382356,3.92764021201669));
#97823=CARTESIAN_POINT('Ctrl Pts',(-11.0827210179461,16.6569472637629,3.96525222866824));
#97824=CARTESIAN_POINT('Ctrl Pts',(-11.0613392000724,16.6602524023186,4.01063236985401));
#97825=CARTESIAN_POINT('Ctrl Pts',(-11.0571627239435,16.6608852082787,4.01922372921883));
#97826=CARTESIAN_POINT('Ctrl Pts',(-11.0503607636862,16.6618964879533,4.03279357365334));
#97827=CARTESIAN_POINT('Ctrl Pts',(-11.0478032444792,16.6622726064819,4.03780580603991));
#97828=CARTESIAN_POINT('Ctrl Pts',(-11.0429116364252,16.6629844206594,4.04722504442373));
#97829=CARTESIAN_POINT('Ctrl Pts',(-11.0405852762432,16.6633198401581,4.05163594170854));
#97830=CARTESIAN_POINT('Ctrl Pts',(-11.0352683129236,16.6640795917644,4.06156385487913));
#97831=CARTESIAN_POINT('Ctrl Pts',(-11.032261506308,16.6645044878793,4.06707197320762));
#97832=CARTESIAN_POINT('Ctrl Pts',(-11.0244139495824,16.665601530537,4.08117853193341));
#97833=CARTESIAN_POINT('Ctrl Pts',(-11.0195089819841,16.6662759394777,4.08974049497201));
#97834=CARTESIAN_POINT('Ctrl Pts',(-10.9762627575724,16.6721283014211,4.16307761837722));
#97835=CARTESIAN_POINT('Ctrl Pts',(-10.9319080591171,16.6775287561384,4.22408864052207));
#97836=CARTESIAN_POINT('Ctrl Pts',(-10.8460774338943,16.6870041076273,4.3210933614824));
#97837=CARTESIAN_POINT('Ctrl Pts',(-10.80734150892,16.691013295666,4.35920959846473));
#97838=CARTESIAN_POINT('Ctrl Pts',(-10.7389020235556,16.6975499478174,4.41782491283068));
#97839=CARTESIAN_POINT('Ctrl Pts',(-10.7106370145213,16.7001135197421,4.43987997120893));
#97840=CARTESIAN_POINT('Ctrl Pts',(-10.6764222394302,16.703024428143,4.46415007816418));
#97841=CARTESIAN_POINT('Ctrl Pts',(-10.6714094803625,16.7034462667085,4.46764752515646));
#97842=CARTESIAN_POINT('Ctrl Pts',(-10.6636455257224,16.7040922475084,4.47297512468929));
#97843=CARTESIAN_POINT('Ctrl Pts',(-10.6609135686236,16.7043181614104,4.47483292546186));
#97844=CARTESIAN_POINT('Ctrl Pts',(-10.6558594501519,16.7047334882933,4.47823884235012));
#97845=CARTESIAN_POINT('Ctrl Pts',(-10.6535396106521,16.7049231093215,4.47979019623933));
#97846=CARTESIAN_POINT('Ctrl Pts',(-10.6482593822422,16.7053524317024,4.483294163309));
#97847=CARTESIAN_POINT('Ctrl Pts',(-10.645295675408,16.7055917943887,4.48524166090922));
#97848=CARTESIAN_POINT('Ctrl Pts',(-10.6375664434981,16.7062119973061,4.49027082072084));
#97849=CARTESIAN_POINT('Ctrl Pts',(-10.6327872930025,16.7065915097063,4.49333152231843));
#97850=CARTESIAN_POINT('Ctrl Pts',(-10.6000213200897,16.7091678252716,4.51398331888461));
#97851=CARTESIAN_POINT('Ctrl Pts',(-10.5713239094828,16.7112975434286,4.53042573704475));
#97852=CARTESIAN_POINT('Ctrl Pts',(-10.4705912570159,16.7184815584326,4.58263686128327));
#97853=CARTESIAN_POINT('Ctrl Pts',(-10.3956095828412,16.7233510383896,4.6122288929363));
#97854=CARTESIAN_POINT('Ctrl Pts',(-10.2844127420646,16.7305767854396,4.6434314677864));
#97855=CARTESIAN_POINT('Ctrl Pts',(-10.250226579719,16.732796547896,4.65139588980909));
#97856=CARTESIAN_POINT('Ctrl Pts',(-10.2009435606005,16.7360305897609,4.66057882813239));
#97857=CARTESIAN_POINT('Ctrl Pts',(-10.1860983931109,16.7370089878418,4.66305154120646));
#97858=CARTESIAN_POINT('Ctrl Pts',(-10.1595035660592,16.738771975091,4.66695916129907));
#97859=CARTESIAN_POINT('Ctrl Pts',(-10.1477718169157,16.7395531963628,4.66850269371443));
#97860=CARTESIAN_POINT('Ctrl Pts',(-10.1299495373803,16.7407462003292,4.67057486661874));
#97861=CARTESIAN_POINT('Ctrl Pts',(-10.1238746310674,16.7411539365664,4.67123331323167));
#97862=CARTESIAN_POINT('Ctrl Pts',(-10.1128460466836,16.7418962504058,4.6723419175228));
#97863=CARTESIAN_POINT('Ctrl Pts',(-10.1078940866256,16.7422303226669,4.67280802632025));
#97864=CARTESIAN_POINT('Ctrl Pts',(-10.097218894109,16.7429522155613,4.67374465923538));
#97865=CARTESIAN_POINT('Ctrl Pts',(-10.0914948964841,16.7433403532105,4.6742047182445));
#97866=CARTESIAN_POINT('Ctrl Pts',(-10.0759729611386,16.7443958690103,4.67533808881992));
#97867=CARTESIAN_POINT('Ctrl Pts',(-10.0661697774648,16.745065730814,4.67593072254415));
#97868=CARTESIAN_POINT('Ctrl Pts',(-10.0156773620735,16.7485334004444,4.67834978092408));
#97869=CARTESIAN_POINT('Ctrl Pts',(-9.97492515181614,16.7513919045274,4.67818697706407));
#97870=CARTESIAN_POINT('Ctrl Pts',(-9.84875696090734,16.7604290230137,4.67113425632181));
#97871=CARTESIAN_POINT('Ctrl Pts',(-9.76402742689186,16.7667860483353,4.65704114812612));
#97872=CARTESIAN_POINT('Ctrl Pts',(-9.64586402103088,16.7757199871113,4.62385924378747));
#97873=CARTESIAN_POINT('Ctrl Pts',(-9.61063041148041,16.778388869124,4.61214377377987));
#97874=CARTESIAN_POINT('Ctrl Pts',(-9.56810436611026,16.7815720572614,4.5957339777677));
#97875=CARTESIAN_POINT('Ctrl Pts',(-9.56023591467436,16.7821593590126,4.59259981156679));
#97876=CARTESIAN_POINT('Ctrl Pts',(-9.54891760312958,16.7830010439651,4.58794941139286));
#97877=CARTESIAN_POINT('Ctrl Pts',(-9.54544035437241,16.7832592007512,4.58650116432355));
#97878=CARTESIAN_POINT('Ctrl Pts',(-9.53937807924722,16.7837084498256,4.58394207600493));
#97879=CARTESIAN_POINT('Ctrl Pts',(-9.53679000317385,16.7838999748353,4.58283862026243));
#97880=CARTESIAN_POINT('Ctrl Pts',(-9.53130125111625,16.7843055707512,4.58047514832467));
#97881=CARTESIAN_POINT('Ctrl Pts',(-9.5284016819795,16.784519494624,4.57921271785944));
#97882=CARTESIAN_POINT('Ctrl Pts',(-9.52050928780687,16.7851009371588,4.57573860136166));
#97883=CARTESIAN_POINT('Ctrl Pts',(-9.51552662597563,16.7854670948301,4.57350381195629));
#97884=CARTESIAN_POINT('Ctrl Pts',(-9.49192025988727,16.7871982897797,4.56271820790776));
#97885=CARTESIAN_POINT('Ctrl Pts',(-9.47350500626852,16.78853824797,4.55371635511099));
#97886=CARTESIAN_POINT('Ctrl Pts',(-9.37652852392038,16.7955871822333,4.50313409174675));
#97887=CARTESIAN_POINT('Ctrl Pts',(-9.30262321056359,16.8009512096102,4.45323843364391));
#97888=CARTESIAN_POINT('Ctrl Pts',(-9.19130394942888,16.8100801831732,4.35814506163547));
#97889=CARTESIAN_POINT('Ctrl Pts',(-9.15037786375663,16.8137242253025,4.31764488987397));
#97890=CARTESIAN_POINT('Ctrl Pts',(-9.10620050862984,16.8181402424008,4.26701471366485));
#97891=CARTESIAN_POINT('Ctrl Pts',(-9.09991553251678,16.8187810595857,4.25962954389171));
#97892=CARTESIAN_POINT('Ctrl Pts',(-9.08974772249118,16.8198392185778,4.2473784790997));
#97893=CARTESIAN_POINT('Ctrl Pts',(-9.08581091788151,16.8202543802878,4.24255782223009));
#97894=CARTESIAN_POINT('Ctrl Pts',(-9.07879191149343,16.8210046359522,4.23382255476919));
#97895=CARTESIAN_POINT('Ctrl Pts',(-9.07569596949907,16.8213391725862,4.2299191339516));
#97896=CARTESIAN_POINT('Ctrl Pts',(-9.06913554421656,16.8220559200752,4.22153895985334));
#97897=CARTESIAN_POINT('Ctrl Pts',(-9.06567839471781,16.8224384079548,4.21705665159116));
#97898=CARTESIAN_POINT('Ctrl Pts',(-9.05638107553406,16.8234802515922,4.20482097635192));
#97899=CARTESIAN_POINT('Ctrl Pts',(-9.05060433743039,16.8241420408211,4.19702019295044));
#97900=CARTESIAN_POINT('Ctrl Pts',(-9.01975020190054,16.8277574395485,4.15426018797108));
#97901=CARTESIAN_POINT('Ctrl Pts',(-8.99650928176368,16.8307794356234,4.11802235711924));
#97902=CARTESIAN_POINT('Ctrl Pts',(-8.94750430064617,16.8378998179387,4.03153369143788));
#97903=CARTESIAN_POINT('Ctrl Pts',(-8.92326595028848,16.8420336963367,3.98053936019234));
#97904=CARTESIAN_POINT('Ctrl Pts',(-8.88012923748968,16.8507498031537,3.86995620610662));
#97905=CARTESIAN_POINT('Ctrl Pts',(-8.86212419171976,16.8553203228154,3.81019081123515));
#97906=CARTESIAN_POINT('Ctrl Pts',(-8.84686642946797,16.8603719294707,3.73973592385056));
#97907=CARTESIAN_POINT('Ctrl Pts',(-8.84491901362492,16.8610506668538,3.73017010039572));
#97908=CARTESIAN_POINT('Ctrl Pts',(-8.8423975347273,16.8619782105034,3.71694536558011));
#97909=CARTESIAN_POINT('Ctrl Pts',(-8.84172151860359,16.8622322963681,3.71330663308328));
#97910=CARTESIAN_POINT('Ctrl Pts',(-8.84059186301836,16.862666326221,3.7070623775473));
#97911=CARTESIAN_POINT('Ctrl Pts',(-8.84012983193483,16.8628467295573,3.70445843069239));
#97912=CARTESIAN_POINT('Ctrl Pts',(-8.8391835026173,16.8632223363297,3.69901858817384));
#97913=CARTESIAN_POINT('Ctrl Pts',(-8.83870081937706,16.8634174415895,3.69618244661031));
#97914=CARTESIAN_POINT('Ctrl Pts',(-8.83754817426291,16.8638921973797,3.68925641595282));
#97915=CARTESIAN_POINT('Ctrl Pts',(-8.83688939002838,16.8641712274547,3.68516465215995));
#97916=CARTESIAN_POINT('Ctrl Pts',(-8.83459801107458,16.8651705799912,3.67043777438382));
#97917=CARTESIAN_POINT('Ctrl Pts',(-8.83308951231817,16.8658843590189,3.65978349334769));
#97918=CARTESIAN_POINT('Ctrl Pts',(-8.8296877337726,16.8676503795956,3.63313057419807));
#97919=CARTESIAN_POINT('Ctrl Pts',(-8.82797622954559,16.8686943290159,3.61711057081211));
#97920=CARTESIAN_POINT('Ctrl Pts',(-8.82191962565787,16.8732199551265,3.54678721659312));
#97921=CARTESIAN_POINT('Ctrl Pts',(-8.82101598256565,16.8765832986265,3.49225140884443));
#97922=CARTESIAN_POINT('Ctrl Pts',(-8.82819048612073,16.8849870554861,3.35649342437771));
#97923=CARTESIAN_POINT('Ctrl Pts',(-8.84091768949865,16.8900233507699,3.27581757618939));
#97924=CARTESIAN_POINT('Ctrl Pts',(-8.86573174455414,16.8963162697899,3.18257826540587));
#97925=CARTESIAN_POINT('Ctrl Pts',(-8.8698753834095,16.8973048175612,3.16812750880261));
#97926=CARTESIAN_POINT('Ctrl Pts',(-8.8762486775669,16.8987433335029,3.14740643521586));
#97927=CARTESIAN_POINT('Ctrl Pts',(-8.87825677158056,16.8991861528746,3.14106911104731));
#97928=CARTESIAN_POINT('Ctrl Pts',(-8.88188486925952,16.8999685120267,3.12994712394239));
#97929=CARTESIAN_POINT('Ctrl Pts',(-8.88348221883078,16.900307306665,3.12515520593022));
#97930=CARTESIAN_POINT('Ctrl Pts',(-8.88684623235489,16.9010094188268,3.11527574107535));
#97931=CARTESIAN_POINT('Ctrl Pts',(-8.8886170632032,16.9013728662555,3.11018974877852));
#97932=CARTESIAN_POINT('Ctrl Pts',(-8.89325520646379,16.9023094207647,3.09715711003194));
#97933=CARTESIAN_POINT('Ctrl Pts',(-8.89617321163529,16.9028841853108,3.08922896057814));
#97934=CARTESIAN_POINT('Ctrl Pts',(-8.90897720176546,16.9053468929679,3.05556273085136));
#97935=CARTESIAN_POINT('Ctrl Pts',(-8.91967933335675,16.9072616221675,3.03014654436327));
#97936=CARTESIAN_POINT('Ctrl Pts',(-8.97306417933406,16.916213468084,2.91485465846848));
#97937=CARTESIAN_POINT('Ctrl Pts',(-9.02613241568994,16.923593918325,2.83024762396939));
#97938=CARTESIAN_POINT('Ctrl Pts',(-9.10319044162635,16.9324533292332,2.73624889568174));
#97939=CARTESIAN_POINT('Ctrl Pts',(-9.11767511191638,16.9340532253582,2.71956036817943));
#97940=CARTESIAN_POINT('Ctrl Pts',(-9.14742101542142,16.9371985547891,2.68717604736834));
#97941=CARTESIAN_POINT('Ctrl Pts',(-9.16266798842002,16.9387437928039,2.67147784866777));
#97942=CARTESIAN_POINT('Ctrl Pts',(-9.18229786246077,16.940641927194,2.65236285832559));
#97943=CARTESIAN_POINT('Ctrl Pts',(-9.18627820868674,16.94102229843,2.6485410409044));
#97944=CARTESIAN_POINT('Ctrl Pts',(-9.19261420330395,16.9416204823678,2.64254240770005));
#97945=CARTESIAN_POINT('Ctrl Pts',(-9.1949520726629,16.9418396529201,2.64034705688068));
#97946=CARTESIAN_POINT('Ctrl Pts',(-9.19914481614963,16.9422299106679,2.63644201113584));
#97947=CARTESIAN_POINT('Ctrl Pts',(-9.2009962059884,16.9424012652229,2.63472873446189));
#97948=CARTESIAN_POINT('Ctrl Pts',(-9.20545256970721,16.9428114177326,2.63063131359555));
#97949=CARTESIAN_POINT('Ctrl Pts',(-9.20806277631253,16.9430497835293,2.62825292289423));
#97950=CARTESIAN_POINT('Ctrl Pts',(-9.21604163929868,16.9437728912032,2.62104808613208));
#97951=CARTESIAN_POINT('Ctrl Pts',(-9.22144413222486,16.9442549509091,2.61625911862514));
#97952=CARTESIAN_POINT('Ctrl Pts',(-9.27049228186356,16.948567649966,2.57357994692236));
#97953=CARTESIAN_POINT('Ctrl Pts',(-9.31683428954731,16.9521937524185,2.5388953618999));
#97954=CARTESIAN_POINT('Ctrl Pts',(-9.45128160918327,16.9620989975324,2.45292790371797));
#97955=CARTESIAN_POINT('Ctrl Pts',(-9.54375421683804,16.968294283096,2.40945444944903));
#97956=CARTESIAN_POINT('Ctrl Pts',(-9.65349650000306,16.9758299482593,2.37429485988698));
#97957=CARTESIAN_POINT('Ctrl Pts',(-9.66640171398731,16.9767179693012,2.37040321476699));
#97958=CARTESIAN_POINT('Ctrl Pts',(-9.68556230143841,16.9780404866469,2.36498220097633));
#97959=CARTESIAN_POINT('Ctrl Pts',(-9.69176829564313,16.9784694616381,2.36328117635206));
#97960=CARTESIAN_POINT('Ctrl Pts',(-9.70282470168288,16.9792349529721,2.36034788345764));
#97961=CARTESIAN_POINT('Ctrl Pts',(-9.70766965228018,16.9795708152968,2.35909550305639));
#97962=CARTESIAN_POINT('Ctrl Pts',(-9.71788932268201,16.9802802214282,2.35652317152172));
#97963=CARTESIAN_POINT('Ctrl Pts',(-9.7232656458224,16.9806539778474,2.35521015599783));
#97964=CARTESIAN_POINT('Ctrl Pts',(-9.73753456166153,16.9816475097869,2.35183176369908));
#97965=CARTESIAN_POINT('Ctrl Pts',(-9.74644210851361,16.9822693482201,2.34983184157236));
#97966=CARTESIAN_POINT('Ctrl Pts',(-9.77386598258773,16.9841891891545,2.34400868280322));
#97967=CARTESIAN_POINT('Ctrl Pts',(-9.7924487921988,16.9854976396007,2.34052823793873));
#97968=CARTESIAN_POINT('Ctrl Pts',(-9.81110407400449,16.9868193101849,2.33749692832995));
#97969=CARTESIAN_POINT('Origin',(-10.,12.3756328852638,3.5));
#97970=CARTESIAN_POINT('',(-9.81110406371068,17.5866589100326,2.3374969300026));
#97971=CARTESIAN_POINT('',(-9.81110408996512,17.4886290554142,2.3374969257365));
#97972=CARTESIAN_POINT('',(-9.81110406371068,12.3756328852638,2.3374969300026));
#97973=CARTESIAN_POINT('Ctrl Pts',(-9.81110406371068,17.5866589100326,2.3374969300026));
#97974=CARTESIAN_POINT('Ctrl Pts',(-9.78887392557191,17.585007544161,2.34110912068488));
#97975=CARTESIAN_POINT('Ctrl Pts',(-9.76673711519424,17.5833509725145,2.34536062552661));
#97976=CARTESIAN_POINT('Ctrl Pts',(-9.68809404061539,17.5774412249151,2.36282171791141));
#97977=CARTESIAN_POINT('Ctrl Pts',(-9.63246607121775,17.5732116756579,2.3795625026358));
#97978=CARTESIAN_POINT('Ctrl Pts',(-9.57154547594279,17.5686696714859,2.40292479392918));
#97979=CARTESIAN_POINT('Ctrl Pts',(-9.56482171302421,17.5681697072018,2.40557451049974));
#97980=CARTESIAN_POINT('Ctrl Pts',(-9.55484727225082,17.5674304642641,2.40961172216935));
#97981=CARTESIAN_POINT('Ctrl Pts',(-9.5515779144827,17.5671885523928,2.41095216748817));
#97982=CARTESIAN_POINT('Ctrl Pts',(-9.54598406958716,17.5667753774371,2.41327511974972));
#97983=CARTESIAN_POINT('Ctrl Pts',(-9.54365665916232,17.5666036906361,2.41425040357337));
#97984=CARTESIAN_POINT('Ctrl Pts',(-9.53837805569299,17.5662148150041,2.4164823346419));
#97985=CARTESIAN_POINT('Ctrl Pts',(-9.53542885044088,17.5659979045272,2.41774356170651));
#97986=CARTESIAN_POINT('Ctrl Pts',(-9.52742084186209,17.565409803118,2.42120695128754));
#97987=CARTESIAN_POINT('Ctrl Pts',(-9.52237222236276,17.5650399933324,2.42343267203003));
#97988=CARTESIAN_POINT('Ctrl Pts',(-9.49740275064387,17.563214842405,2.43465087312125));
#97989=CARTESIAN_POINT('Ctrl Pts',(-9.47771782335303,17.5617881799024,2.44416183391481));
#97990=CARTESIAN_POINT('Ctrl Pts',(-9.43870353075812,17.5589628781992,2.46437035237047));
#97991=CARTESIAN_POINT('Ctrl Pts',(-9.41938789454087,17.557565232559,2.47507455202477));
#97992=CARTESIAN_POINT('Ctrl Pts',(-9.31473773265837,17.5499377802119,2.53697741297212));
#97993=CARTESIAN_POINT('Ctrl Pts',(-9.23586022919132,17.5439447230707,2.59828619785502));
#97994=CARTESIAN_POINT('Ctrl Pts',(-9.1461710617582,17.5358001527505,2.68831574899577));
#97995=CARTESIAN_POINT('Ctrl Pts',(-9.12740613111295,17.5340092491634,2.70852357699786));
#97996=CARTESIAN_POINT('Ctrl Pts',(-9.10383967271742,17.5316303862701,2.73575977038211));
#97997=CARTESIAN_POINT('Ctrl Pts',(-9.09837984840599,17.5310695785164,2.74220876435746));
#97998=CARTESIAN_POINT('Ctrl Pts',(-9.08955360993892,17.5301466185398,2.7528645010714));
#97999=CARTESIAN_POINT('Ctrl Pts',(-9.08614576919978,17.529786144959,2.75703665895224));
#98000=CARTESIAN_POINT('Ctrl Pts',(-9.07959711032305,17.5290853150358,2.7651672869647));
#98001=CARTESIAN_POINT('Ctrl Pts',(-9.07645290375853,17.5287451041865,2.76912288644115));
#98002=CARTESIAN_POINT('Ctrl Pts',(-9.06922939932403,17.5279547401514,2.77833152649115));
#98003=CARTESIAN_POINT('Ctrl Pts',(-9.06516898303976,17.5275038583093,2.78359909037378));
#98004=CARTESIAN_POINT('Ctrl Pts',(-9.05207152951936,17.5260274819366,2.80089132826344));
#98005=CARTESIAN_POINT('Ctrl Pts',(-9.04322051832201,17.5249948757097,2.81305436384805));
#98006=CARTESIAN_POINT('Ctrl Pts',(-8.9881101163067,17.5183333498422,2.89191881920148));
#98007=CARTESIAN_POINT('Ctrl Pts',(-8.94862636918629,17.5124527201826,2.96307094596309));
#98008=CARTESIAN_POINT('Ctrl Pts',(-8.89530570297037,17.5024837820357,3.08800819492469));
#98009=CARTESIAN_POINT('Ctrl Pts',(-8.87736550802768,17.49845399928,3.13975132557812));
#98010=CARTESIAN_POINT('Ctrl Pts',(-8.85887135079861,17.4933741638347,3.20814190214777));
#98011=CARTESIAN_POINT('Ctrl Pts',(-8.85497735761024,17.4922266678515,3.22381356512481));
#98012=CARTESIAN_POINT('Ctrl Pts',(-8.84902314943137,17.490336533415,3.25007294813138));
#98013=CARTESIAN_POINT('Ctrl Pts',(-8.84678394812961,17.4895862221165,3.26061746048637));
#98014=CARTESIAN_POINT('Ctrl Pts',(-8.84388385806192,17.488557585768,3.27526073893597));
#98015=CARTESIAN_POINT('Ctrl Pts',(-8.84309947269726,17.4882728689747,3.27933409789126));
#98016=CARTESIAN_POINT('Ctrl Pts',(-8.84180729118898,17.4877926113087,3.28624079824013));
#98017=CARTESIAN_POINT('Ctrl Pts',(-8.84128833555495,17.4875964553139,3.28907198755132));
#98018=CARTESIAN_POINT('Ctrl Pts',(-8.84031240942297,17.4872211887882,3.29450851388123));
#98019=CARTESIAN_POINT('Ctrl Pts',(-8.83985383122251,17.4870419851224,3.29711351442347));
#98020=CARTESIAN_POINT('Ctrl Pts',(-8.83877476143978,17.4866132407057,3.303366582556));
#98021=CARTESIAN_POINT('Ctrl Pts',(-8.8381626743251,17.4863641657683,3.3070161014059));
#98022=CARTESIAN_POINT('Ctrl Pts',(-8.83600028880896,17.4854620722707,3.32029242709073));
#98023=CARTESIAN_POINT('Ctrl Pts',(-8.83455230370117,17.4848144580397,3.32993583022431));
#98024=CARTESIAN_POINT('Ctrl Pts',(-8.82489256659193,17.4801438139359,3.40020079690838));
#98025=CARTESIAN_POINT('Ctrl Pts',(-8.82129430365647,17.4763346840672,3.46137061038701));
#98026=CARTESIAN_POINT('Ctrl Pts',(-8.82374788231328,17.4684011814472,3.58949377070016));
#98027=CARTESIAN_POINT('Ctrl Pts',(-8.83073596767701,17.4642918125875,3.65620236613935));
#98028=CARTESIAN_POINT('Ctrl Pts',(-8.84989785458853,17.4578279569619,3.7560587256701));
#98029=CARTESIAN_POINT('Ctrl Pts',(-8.8579469485252,17.455585797464,3.78985424123171));
#98030=CARTESIAN_POINT('Ctrl Pts',(-8.86997909914695,17.4526946604607,3.83201049087118));
#98031=CARTESIAN_POINT('Ctrl Pts',(-8.87258331145889,17.4520902038654,3.84074888858841));
#98032=CARTESIAN_POINT('Ctrl Pts',(-8.87693042473741,17.4511136785261,3.8547399147036));
#98033=CARTESIAN_POINT('Ctrl Pts',(-8.87860937676447,17.450743687377,3.86001214744429));
#98034=CARTESIAN_POINT('Ctrl Pts',(-8.88187818201808,17.4500365918664,3.87003206533961));
#98035=CARTESIAN_POINT('Ctrl Pts',(-8.88346128517356,17.4496997144187,3.87478183812311));
#98036=CARTESIAN_POINT('Ctrl Pts',(-8.8871508347497,17.4489270229105,3.88562068277207));
#98037=CARTESIAN_POINT('Ctrl Pts',(-8.88927704474634,17.4484905687919,3.89170280747755));
#98038=CARTESIAN_POINT('Ctrl Pts',(-8.89601743838281,17.4471334798399,3.91048777856399));
#98039=CARTESIAN_POINT('Ctrl Pts',(-8.90080030547283,17.4462073274082,3.92312848849395));
#98040=CARTESIAN_POINT('Ctrl Pts',(-8.9433501107718,17.4382638215607,4.02999047314875));
#98041=CARTESIAN_POINT('Ctrl Pts',(-8.99292861335939,17.4308288532457,4.11902954823949));
#98042=CARTESIAN_POINT('Ctrl Pts',(-9.08778949001508,17.4191302342665,4.24721576570229));
#98043=CARTESIAN_POINT('Ctrl Pts',(-9.12569443611389,17.4149009197151,4.29123371856727));
#98044=CARTESIAN_POINT('Ctrl Pts',(-9.1718001265536,17.410359137448,4.33739611613007));
#98045=CARTESIAN_POINT('Ctrl Pts',(-9.17695404947359,17.409859179351,4.34246225765363));
#98046=CARTESIAN_POINT('Ctrl Pts',(-9.1846969787712,17.4091199437378,4.349934427415));
#98047=CARTESIAN_POINT('Ctrl Pts',(-9.1872505914906,17.4088780330782,4.35237664627971));
#98048=CARTESIAN_POINT('Ctrl Pts',(-9.19164672718939,17.4084648594721,4.35654329531557));
#98049=CARTESIAN_POINT('Ctrl Pts',(-9.19348383902302,17.4082931728171,4.35827333230182));
#98050=CARTESIAN_POINT('Ctrl Pts',(-9.19766869567849,17.4079042965421,4.36218897510374));
#98051=CARTESIAN_POINT('Ctrl Pts',(-9.20001981699484,17.4076873852823,4.36437090308806));
#98052=CARTESIAN_POINT('Ctrl Pts',(-9.2064392841798,17.4070992796627,4.37027977888195));
#98053=CARTESIAN_POINT('Ctrl Pts',(-9.2105250152603,17.4067294664824,4.3739878458312));
#98054=CARTESIAN_POINT('Ctrl Pts',(-9.23092461690728,17.4049042715374,4.39224202946819));
#98055=CARTESIAN_POINT('Ctrl Pts',(-9.24761632788545,17.4034775700653,4.40636181615246));
#98056=CARTESIAN_POINT('Ctrl Pts',(-9.28193884524745,17.4006522389711,4.43379369587739));
#98057=CARTESIAN_POINT('Ctrl Pts',(-9.29957011397894,17.3992546015039,4.44709057680385));
#98058=CARTESIAN_POINT('Ctrl Pts',(-9.39866683575855,17.3916271004004,4.51754385318835));
#98059=CARTESIAN_POINT('Ctrl Pts',(-9.48674502806125,17.385633985992,4.56469098493683));
#98060=CARTESIAN_POINT('Ctrl Pts',(-9.60545786822042,17.3774894233854,4.61004126747157));
#98061=CARTESIAN_POINT('Ctrl Pts',(-9.6315472832876,17.3756986001208,4.61897163229955));
#98062=CARTESIAN_POINT('Ctrl Pts',(-9.66600979393032,17.3733198290264,4.6294321585371));
#98063=CARTESIAN_POINT('Ctrl Pts',(-9.67412114728714,17.3727590300628,4.63179919847052));
#98064=CARTESIAN_POINT('Ctrl Pts',(-9.68744437545077,17.3718360808536,4.63553206215525));
#98065=CARTESIAN_POINT('Ctrl Pts',(-9.69264149093973,17.3714756091729,4.63694979127751));
#98066=CARTESIAN_POINT('Ctrl Pts',(-9.70273198541095,17.370774780296,4.63962815123988));
#98067=CARTESIAN_POINT('Ctrl Pts',(-9.70762411903777,17.3704345685756,4.64089304426637));
#98068=CARTESIAN_POINT('Ctrl Pts',(-9.71897395989665,17.3696441986072,4.64374982513937));
#98069=CARTESIAN_POINT('Ctrl Pts',(-9.7254372618932,17.3691933116691,4.64531855717552));
#98070=CARTESIAN_POINT('Ctrl Pts',(-9.74656079153286,17.3677169012153,4.65025644981767));
#98071=CARTESIAN_POINT('Ctrl Pts',(-9.76127182316552,17.3666842655474,4.65339939043725));
#98072=CARTESIAN_POINT('Ctrl Pts',(-9.85571246984516,17.3600238510747,4.67169205978603));
#98073=CARTESIAN_POINT('Ctrl Pts',(-9.9367538682482,17.3541444757962,4.67884543735176));
#98074=CARTESIAN_POINT('Ctrl Pts',(-10.072573854551,17.3441758565844,4.67678423744503));
#98075=CARTESIAN_POINT('Ctrl Pts',(-10.1271544461293,17.3401451258496,4.67214351736855));
#98076=CARTESIAN_POINT('Ctrl Pts',(-10.197172178646,17.335064229951,4.66124025964057));
#98077=CARTESIAN_POINT('Ctrl Pts',(-10.2130756020305,17.3339165864049,4.6584276635007));
#98078=CARTESIAN_POINT('Ctrl Pts',(-10.2394910266992,17.3320262354655,4.65319352737478));
#98079=CARTESIAN_POINT('Ctrl Pts',(-10.2500363135098,17.3312758531124,4.650953138097));
#98080=CARTESIAN_POINT('Ctrl Pts',(-10.2645952650024,17.3302471364168,4.64765047645644));
#98081=CARTESIAN_POINT('Ctrl Pts',(-10.2686359198,17.3299624090523,4.64671139101308));
#98082=CARTESIAN_POINT('Ctrl Pts',(-10.2754717259502,17.3294821388121,4.64508457130949));
#98083=CARTESIAN_POINT('Ctrl Pts',(-10.2782694473831,17.3292859807406,4.64440790917339));
#98084=CARTESIAN_POINT('Ctrl Pts',(-10.2836332805925,17.3289107143922,4.64308976925107));
#98085=CARTESIAN_POINT('Ctrl Pts',(-10.2861997385486,17.3287315129559,4.64244989755956));
#98086=CARTESIAN_POINT('Ctrl Pts',(-10.292351388053,17.328302779298,4.64089413202167));
#98087=CARTESIAN_POINT('Ctrl Pts',(-10.2959344896023,17.3280537128375,4.63996997037849));
#98088=CARTESIAN_POINT('Ctrl Pts',(-10.3089424265636,17.3271516947453,4.63654946961392));
#98089=CARTESIAN_POINT('Ctrl Pts',(-10.318340843798,17.3265041462254,4.63395292768797));
#98090=CARTESIAN_POINT('Ctrl Pts',(-10.3865819802538,17.3218255247025,4.6141843080896));
#98091=CARTESIAN_POINT('Ctrl Pts',(-10.4440445506291,17.3180092313213,4.59255605531946));
#98092=CARTESIAN_POINT('Ctrl Pts',(-10.560120283288,17.3100740337127,4.53818655485231));
#98093=CARTESIAN_POINT('Ctrl Pts',(-10.6181435769748,17.305969929319,4.50472083093807));
#98094=CARTESIAN_POINT('Ctrl Pts',(-10.7014896163509,17.2995133069973,4.44668449474595));
#98095=CARTESIAN_POINT('Ctrl Pts',(-10.7290739835956,17.2972727749235,4.42560789716553));
#98096=CARTESIAN_POINT('Ctrl Pts',(-10.7626779642778,17.2943834751922,4.39749678909456));
#98097=CARTESIAN_POINT('Ctrl Pts',(-10.76960169914,17.2937791574269,4.39156681217848));
#98098=CARTESIAN_POINT('Ctrl Pts',(-10.7806157794854,17.2928028026519,4.38190967656783));
#98099=CARTESIAN_POINT('Ctrl Pts',(-10.7847500024759,17.2924328419155,4.37823294440812));
#98100=CARTESIAN_POINT('Ctrl Pts',(-10.7925758421223,17.2917257691566,4.37117372825135));
#98101=CARTESIAN_POINT('Ctrl Pts',(-10.7962721045915,17.2913888838012,4.36779655704949));
#98102=CARTESIAN_POINT('Ctrl Pts',(-10.8046761327539,17.2906161239496,4.36001913253735));
#98103=CARTESIAN_POINT('Ctrl Pts',(-10.8093695086785,17.2901796089906,4.35560363633394));
#98104=CARTESIAN_POINT('Ctrl Pts',(-10.8237967333067,17.2888221400999,4.34180566671745));
#98105=CARTESIAN_POINT('Ctrl Pts',(-10.8334051423428,17.2878956641149,4.33229422714102));
#98106=CARTESIAN_POINT('Ctrl Pts',(-10.9137217752634,17.2799542891264,4.25000267635647));
#98107=CARTESIAN_POINT('Ctrl Pts',(-10.9749011388234,17.2725221230667,4.16854374949347));
#98108=CARTESIAN_POINT('Ctrl Pts',(-11.0534675886108,17.2608240591044,4.02978173965813));
#98109=CARTESIAN_POINT('Ctrl Pts',(-11.0782917205095,17.2565926211596,3.97723287836739));
#98110=CARTESIAN_POINT('Ctrl Pts',(-11.1017382619598,17.2520488313538,3.9163173060824));
#98111=CARTESIAN_POINT('Ctrl Pts',(-11.1042723586862,17.2515488172985,3.90954836297565));
#98112=CARTESIAN_POINT('Ctrl Pts',(-11.1079524306741,17.25080951544,3.89943580185742));
#98113=CARTESIAN_POINT('Ctrl Pts',(-11.1091458709735,17.2505675938226,3.89610981579618));
#98114=CARTESIAN_POINT('Ctrl Pts',(-11.1111659252887,17.2501544080104,3.89039943260829));
#98115=CARTESIAN_POINT('Ctrl Pts',(-11.1119998627632,17.2499827200348,3.88801770083609));
#98116=CARTESIAN_POINT('Ctrl Pts',(-11.1138763737146,17.2495938495733,3.88260263208626));
#98117=CARTESIAN_POINT('Ctrl Pts',(-11.1149142153731,17.2493769453927,3.87956770539574));
#98118=CARTESIAN_POINT('Ctrl Pts',(-11.1177034058787,17.2487888778477,3.87130121812602));
#98119=CARTESIAN_POINT('Ctrl Pts',(-11.1194304427223,17.2484190953651,3.86606144971446));
#98120=CARTESIAN_POINT('Ctrl Pts',(-11.1278148916153,17.2465942984114,3.84000898774695));
#98121=CARTESIAN_POINT('Ctrl Pts',(-11.1339294885263,17.2451679492855,3.81902445715034));
#98122=CARTESIAN_POINT('Ctrl Pts',(-11.1450412726649,17.2423428839156,3.77651947057751));
#98123=CARTESIAN_POINT('Ctrl Pts',(-11.1500240192672,17.2409451725356,3.75500467903139));
#98124=CARTESIAN_POINT('Ctrl Pts',(-11.174114333255,17.2333181119477,3.63583404759753));
#98125=CARTESIAN_POINT('Ctrl Pts',(-11.1813911463629,17.227325515038,3.53620508583269));
#98126=CARTESIAN_POINT('Ctrl Pts',(-11.1745765736589,17.2191808825607,3.40930483203998));
#98127=CARTESIAN_POINT('Ctrl Pts',(-11.1721307823067,17.2173893332852,3.38182648803447));
#98128=CARTESIAN_POINT('Ctrl Pts',(-11.1676786935231,17.2150097324581,3.34607486324095));
#98129=CARTESIAN_POINT('Ctrl Pts',(-11.1665441857005,17.2144488540573,3.33770047549173));
#98130=CARTESIAN_POINT('Ctrl Pts',(-11.164539037471,17.2135258075428,3.32400876252105));
#98131=CARTESIAN_POINT('Ctrl Pts',(-11.1637218426613,17.2131653186904,3.31868382109233));
#98132=CARTESIAN_POINT('Ctrl Pts',(-11.1620674307859,17.2124644803542,3.30837567799001));
#98133=CARTESIAN_POINT('Ctrl Pts',(-11.1612346191042,17.2121242765026,3.30339188088765));
#98134=CARTESIAN_POINT('Ctrl Pts',(-11.1592314952053,17.2113339601377,3.29186151397659));
#98135=CARTESIAN_POINT('Ctrl Pts',(-11.1580377619944,17.2108831192393,3.28531924287277));
#98136=CARTESIAN_POINT('Ctrl Pts',(-11.1539640865752,17.2094070166724,3.26401672729102));
#98137=CARTESIAN_POINT('Ctrl Pts',(-11.1508569370317,17.2083746469701,3.24930199012066));
#98138=CARTESIAN_POINT('Ctrl Pts',(-11.1291514781064,17.2017043210926,3.15543928573489));
#98139=CARTESIAN_POINT('Ctrl Pts',(-11.102684356821,17.1958137543111,3.07835109768309));
#98140=CARTESIAN_POINT('Ctrl Pts',(-11.0455341864625,17.1858422856597,2.9550833263934));
#98141=CARTESIAN_POINT('Ctrl Pts',(-11.0191520311363,17.1818200062232,2.90720524077042));
#98142=CARTESIAN_POINT('Ctrl Pts',(-10.9807953895367,17.1767485654876,2.84777639580538));
#98143=CARTESIAN_POINT('Ctrl Pts',(-10.9717706708856,17.1756022385524,2.83440474449362));
#98144=CARTESIAN_POINT('Ctrl Pts',(-10.9562661309363,17.1737138194675,2.81242007217052));
#98145=CARTESIAN_POINT('Ctrl Pts',(-10.9499378772116,17.1729640712155,2.80370328132348));
#98146=CARTESIAN_POINT('Ctrl Pts',(-10.9410085958841,17.1719360715791,2.79175210441003));
#98147=CARTESIAN_POINT('Ctrl Pts',(-10.938508961301,17.1716514385816,2.78844312243826));
#98148=CARTESIAN_POINT('Ctrl Pts',(-10.9342449720051,17.1711712805833,2.7828600708201));
#98149=CARTESIAN_POINT('Ctrl Pts',(-10.9324896788673,17.1709751410445,2.78057915986265));
#98150=CARTESIAN_POINT('Ctrl Pts',(-10.9291050400307,17.1705998730916,2.77621419976628));
#98151=CARTESIAN_POINT('Ctrl Pts',(-10.9274770179667,17.1704206517358,2.77412918399537));
#98152=CARTESIAN_POINT('Ctrl Pts',(-10.9235541674355,17.1699918219666,2.76913991568097));
#98153=CARTESIAN_POINT('Ctrl Pts',(-10.9212526276833,17.1697426797804,2.76624093876215));
#98154=CARTESIAN_POINT('Ctrl Pts',(-10.9128336325921,17.1688399874606,2.75573858464276));
#98155=CARTESIAN_POINT('Ctrl Pts',(-10.9066351989577,17.16819185133,2.74820020852376));
#98156=CARTESIAN_POINT('Ctrl Pts',(-10.8600677683204,17.1634351193504,2.69297979029275));
#98157=CARTESIAN_POINT('Ctrl Pts',(-10.8160499546143,17.1595497864289,2.64849383555287));
#98158=CARTESIAN_POINT('Ctrl Pts',(-10.7187214327034,17.1515991480519,2.56464602410488));
#98159=CARTESIAN_POINT('Ctrl Pts',(-10.665211674425,17.1475469045515,2.52586430782066));
#98160=CARTESIAN_POINT('Ctrl Pts',(-10.579252481404,17.1411616396978,2.47396493294573));
#98161=CARTESIAN_POINT('Ctrl Pts',(-10.5490025881403,17.1389372743217,2.45746597179674));
#98162=CARTESIAN_POINT('Ctrl Pts',(-10.5099077916215,17.1360662291564,2.43831651559632));
#98163=CARTESIAN_POINT('Ctrl Pts',(-10.5016943451274,17.1354632971443,2.43441070134914));
#98164=CARTESIAN_POINT('Ctrl Pts',(-10.4884172343356,17.1344886448504,2.42828444700081));
#98165=CARTESIAN_POINT('Ctrl Pts',(-10.4833816245031,17.1341189876688,2.4260038060321));
#98166=CARTESIAN_POINT('Ctrl Pts',(-10.4737539700971,17.1334121411884,2.42172484166972));
#98167=CARTESIAN_POINT('Ctrl Pts',(-10.469164858707,17.1330751760915,2.41972018658361));
#98168=CARTESIAN_POINT('Ctrl Pts',(-10.4586335687912,17.1323017301232,2.41519958022651));
#98169=CARTESIAN_POINT('Ctrl Pts',(-10.4526832621156,17.131864604729,2.41270309368438));
#98170=CARTESIAN_POINT('Ctrl Pts',(-10.4341604171754,17.1305033201419,2.40511012669013));
#98171=CARTESIAN_POINT('Ctrl Pts',(-10.4215205037104,17.1295735940546,2.40018204202376));
#98172=CARTESIAN_POINT('Ctrl Pts',(-10.3139818400233,17.1216538194914,2.36038066837943));
#98173=CARTESIAN_POINT('Ctrl Pts',(-10.2150582414701,17.1142500139131,2.33764964899599));
#98174=CARTESIAN_POINT('Ctrl Pts',(-10.0564379585503,17.1025575313189,2.32215861232979));
#98175=CARTESIAN_POINT('Ctrl Pts',(-9.99805208773803,17.0983045479692,2.32080815804299));
#98176=CARTESIAN_POINT('Ctrl Pts',(-9.93257457511583,17.0937403939624,2.32415935355092));
#98177=CARTESIAN_POINT('Ctrl Pts',(-9.92535194780163,17.0932398142679,2.3245957764874));
#98178=CARTESIAN_POINT('Ctrl Pts',(-9.91460699311278,17.0924998428301,2.32534447855696));
#98179=CARTESIAN_POINT('Ctrl Pts',(-9.91108147427308,17.092257810487,2.32560608981017));
#98180=CARTESIAN_POINT('Ctrl Pts',(-9.90504124398679,17.0918445013059,2.32608166124239));
#98181=CARTESIAN_POINT('Ctrl Pts',(-9.9025259898384,17.0916727999562,2.32628783375014));
#98182=CARTESIAN_POINT('Ctrl Pts',(-9.89681658379889,17.0912839880879,2.32677430743151));
#98183=CARTESIAN_POINT('Ctrl Pts',(-9.8936229018936,17.0910671553208,2.32705956813609));
#98184=CARTESIAN_POINT('Ctrl Pts',(-9.88494212510772,17.0904794718429,2.32787068469085));
#98185=CARTESIAN_POINT('Ctrl Pts',(-9.87945740769035,17.0901099990113,2.32842203299157));
#98186=CARTESIAN_POINT('Ctrl Pts',(-9.85294818461416,17.0883322527072,2.33127499243877));
#98187=CARTESIAN_POINT('Ctrl Pts',(-9.83198303316909,17.0869507190748,2.33410429166349));
#98188=CARTESIAN_POINT('Ctrl Pts',(-9.81110406370722,17.0855891663962,2.33749693000316));
#98189=CARTESIAN_POINT('Ctrl Pts',(-9.81110407400449,16.9868193101849,2.33749692832995));
#98190=CARTESIAN_POINT('Ctrl Pts',(-9.82687262829458,16.9879364648105,2.33493468506641));
#98191=CARTESIAN_POINT('Ctrl Pts',(-9.84269296230412,16.9890630504714,2.3326933323682));
#98192=CARTESIAN_POINT('Ctrl Pts',(-9.92559485983192,16.9949961523911,2.32266444726947));
#98193=CARTESIAN_POINT('Ctrl Pts',(-9.99320091986613,16.9999455831111,2.32033606303029));
#98194=CARTESIAN_POINT('Ctrl Pts',(-10.1209404481883,17.0093371042531,2.32692028691367));
#98195=CARTESIAN_POINT('Ctrl Pts',(-10.1809331922842,17.0137613931877,2.334664303754));
#98196=CARTESIAN_POINT('Ctrl Pts',(-10.2496419380673,17.0186795918734,2.34897023702307));
#98197=CARTESIAN_POINT('Ctrl Pts',(-10.2591868925245,17.0193592965465,2.35108190769054));
#98198=CARTESIAN_POINT('Ctrl Pts',(-10.2723098244549,17.0202879124601,2.35415702139561));
#98199=CARTESIAN_POINT('Ctrl Pts',(-10.275910877022,17.0205421193972,2.35501879448393));
#98200=CARTESIAN_POINT('Ctrl Pts',(-10.2820773387284,17.020976302027,2.35652528068629));
#98201=CARTESIAN_POINT('Ctrl Pts',(-10.2846447217656,17.0211567377636,2.3571616730881));
#98202=CARTESIAN_POINT('Ctrl Pts',(-10.2899996293392,17.0215323507873,2.35850819024454));
#98203=CARTESIAN_POINT('Ctrl Pts',(-10.2927867233921,17.0217274302065,2.35921988464087));
#98204=CARTESIAN_POINT('Ctrl Pts',(-10.2995809381463,17.0222020231084,2.36098135105936));
#98205=CARTESIAN_POINT('Ctrl Pts',(-10.3035852330447,17.0224809171499,2.36204207955225));
#98206=CARTESIAN_POINT('Ctrl Pts',(-10.3179569914633,17.0234792325595,2.36593038538513));
#98207=CARTESIAN_POINT('Ctrl Pts',(-10.3282916189902,17.0241921283395,2.36887879857151));
#98208=CARTESIAN_POINT('Ctrl Pts',(-10.3539873645198,17.0259555207915,2.37659151778332));
#98209=CARTESIAN_POINT('Ctrl Pts',(-10.3692943477133,17.0269977569866,2.38152987938963));
#98210=CARTESIAN_POINT('Ctrl Pts',(-10.4358262820918,17.0315111523539,2.40450941921656));
#98211=CARTESIAN_POINT('Ctrl Pts',(-10.4858729279928,17.0348646279584,2.42576883531757));
#98212=CARTESIAN_POINT('Ctrl Pts',(-10.6070761156188,17.0432718359703,2.48746525232517));
#98213=CARTESIAN_POINT('Ctrl Pts',(-10.6758133256797,17.0483210403588,2.53199056999242));
#98214=CARTESIAN_POINT('Ctrl Pts',(-10.7510835267188,17.0546281546339,2.59269939687553));
#98215=CARTESIAN_POINT('Ctrl Pts',(-10.7625975038567,17.055616306033,2.60235538088719));
#98216=CARTESIAN_POINT('Ctrl Pts',(-10.7789334426548,17.0570543485397,2.61659639223207));
#98217=CARTESIAN_POINT('Ctrl Pts',(-10.7839065453081,17.0574970975203,2.62100638939758));
#98218=CARTESIAN_POINT('Ctrl Pts',(-10.7925925869622,17.058279374547,2.62884125099657));
#98219=CARTESIAN_POINT('Ctrl Pts',(-10.7963213524118,17.0586181579439,2.63224837816067));
#98220=CARTESIAN_POINT('Ctrl Pts',(-10.803980610741,17.059320288101,2.63933790140317));
#98221=CARTESIAN_POINT('Ctrl Pts',(-10.8079079840038,17.0596837650181,2.6430234786624));
#98222=CARTESIAN_POINT('Ctrl Pts',(-10.8179318016278,17.0606204832105,2.65256030715612));
#98223=CARTESIAN_POINT('Ctrl Pts',(-10.8239907152286,17.0611953830694,2.65845038182173));
#98224=CARTESIAN_POINT('Ctrl Pts',(-10.8495600067438,17.0636594986468,2.68384802517512));
#98225=CARTESIAN_POINT('Ctrl Pts',(-10.8684436345414,17.0655755386833,2.70397130432733));
#98226=CARTESIAN_POINT('Ctrl Pts',(-10.9520794205608,17.0745279096467,2.79961848381354));
#98227=CARTESIAN_POINT('Ctrl Pts',(-11.0077996568005,17.0819073703161,2.8824861017343));
#98228=CARTESIAN_POINT('Ctrl Pts',(-11.0623527246101,17.0907658481259,2.99108950213175));
#98229=CARTESIAN_POINT('Ctrl Pts',(-11.0717129643809,17.0923658514626,3.01110878299789));
#98230=CARTESIAN_POINT('Ctrl Pts',(-11.089206372254,17.0955106220769,3.05144365997242));
#98231=CARTESIAN_POINT('Ctrl Pts',(-11.0973480784597,17.0970552132044,3.07174697196738));
#98232=CARTESIAN_POINT('Ctrl Pts',(-11.1068302271722,17.0989526711052,3.09744273743843));
#98233=CARTESIAN_POINT('Ctrl Pts',(-11.108703899626,17.0993329900199,3.10263220138506));
#98234=CARTESIAN_POINT('Ctrl Pts',(-11.1116088825349,17.0999311101014,3.11085858808792));
#98235=CARTESIAN_POINT('Ctrl Pts',(-11.1126643459147,17.1001502686497,3.11388680396861));
#98236=CARTESIAN_POINT('Ctrl Pts',(-11.1145279413001,17.1005405162536,3.1193047231226));
#98237=CARTESIAN_POINT('Ctrl Pts',(-11.1153407605827,17.1007118725803,3.12169269933319));
#98238=CARTESIAN_POINT('Ctrl Pts',(-11.1172731026307,17.1011220437513,3.12743007661678));
#98239=CARTESIAN_POINT('Ctrl Pts',(-11.1183852396983,17.101360426323,3.13078192065424));
#98240=CARTESIAN_POINT('Ctrl Pts',(-11.1217252777694,17.1020836361068,3.14100195276905));
#98241=CARTESIAN_POINT('Ctrl Pts',(-11.1239051620776,17.1025657800411,3.14788582843654));
#98242=CARTESIAN_POINT('Ctrl Pts',(-11.1429758088692,17.1068815077113,3.21009124580378));
#98243=CARTESIAN_POINT('Ctrl Pts',(-11.1558354034119,17.1105102404496,3.26657507215084));
#98244=CARTESIAN_POINT('Ctrl Pts',(-11.1797104012322,17.1204144291953,3.42434729725979));
#98245=CARTESIAN_POINT('Ctrl Pts',(-11.1818368910928,17.1266064289127,3.52644783762702));
#98246=CARTESIAN_POINT('Ctrl Pts',(-11.1693623135265,17.1341386674072,3.6409564495467));
#98247=CARTESIAN_POINT('Ctrl Pts',(-11.1676716426524,17.1350271761402,3.65433681195003));
#98248=CARTESIAN_POINT('Ctrl Pts',(-11.1648352529803,17.1363502821643,3.67405551476322));
#98249=CARTESIAN_POINT('Ctrl Pts',(-11.1638666741784,17.1367793509037,3.68041854330826));
#98250=CARTESIAN_POINT('Ctrl Pts',(-11.1620523849599,17.1375449473497,3.69171426922652));
#98251=CARTESIAN_POINT('Ctrl Pts',(-11.1612272910909,17.1378808203797,3.69665015513936));
#98252=CARTESIAN_POINT('Ctrl Pts',(-11.1594236613267,17.138590184991,3.70703250145479));
#98253=CARTESIAN_POINT('Ctrl Pts',(-11.1584381496537,17.1389638887839,3.71247760992541));
#98254=CARTESIAN_POINT('Ctrl Pts',(-11.1557258072524,17.1399571302396,3.72688367120089));
#98255=CARTESIAN_POINT('Ctrl Pts',(-11.1539331631769,17.1405787286631,3.73583169541007));
#98256=CARTESIAN_POINT('Ctrl Pts',(-11.1447953667268,17.1435897567271,3.77884188236983));
#98257=CARTESIAN_POINT('Ctrl Pts',(-11.136045670349,17.146023141685,3.81258442900027));
#98258=CARTESIAN_POINT('Ctrl Pts',(-11.1060262281172,17.1532852806912,3.91029361819776));
#98259=CARTESIAN_POINT('Ctrl Pts',(-11.0807498226625,17.1582231912283,3.97287715392995));
#98260=CARTESIAN_POINT('Ctrl Pts',(-11.0228408885473,17.1676194054333,4.08699643514581));
#98261=CARTESIAN_POINT('Ctrl Pts',(-10.9912813124837,17.1720598246634,4.13885144328646));
#98262=CARTESIAN_POINT('Ctrl Pts',(-10.9501619013483,17.1769921232222,4.19597613735019));
#98263=CARTESIAN_POINT('Ctrl Pts',(-10.9443583831479,17.1776711419506,4.20383071988942));
#98264=CARTESIAN_POINT('Ctrl Pts',(-10.936221161021,17.1785989975121,4.21456189420631));
#98265=CARTESIAN_POINT('Ctrl Pts',(-10.9339707844318,17.1788531186232,4.21750075801676));
#98266=CARTESIAN_POINT('Ctrl Pts',(-10.9300887829504,17.1792871929513,4.22252121964311));
#98267=CARTESIAN_POINT('Ctrl Pts',(-10.9284639505356,17.1794676057186,4.22460799741275));
#98268=CARTESIAN_POINT('Ctrl Pts',(-10.9250570652339,17.1798432143,4.22895319769596));
#98269=CARTESIAN_POINT('Ctrl Pts',(-10.92327374978,17.1800383120275,4.23121058634027));
#98270=CARTESIAN_POINT('Ctrl Pts',(-10.9189015815921,17.180513020354,4.23670354725031));
#98271=CARTESIAN_POINT('Ctrl Pts',(-10.9163038566028,17.1807920107929,4.2399320758402));
#98272=CARTESIAN_POINT('Ctrl Pts',(-10.9069024269054,17.1817910610512,4.25149100712855));
#98273=CARTESIAN_POINT('Ctrl Pts',(-10.9000014750169,17.1825045826406,4.25974213450892));
#98274=CARTESIAN_POINT('Ctrl Pts',(-10.8824904511935,17.1842698370897,4.28010569646978));
#98275=CARTESIAN_POINT('Ctrl Pts',(-10.8717429627807,17.1853132870545,4.29209756654184));
#98276=CARTESIAN_POINT('Ctrl Pts',(-10.823605359562,17.1898353444747,4.34364168445352));
#98277=CARTESIAN_POINT('Ctrl Pts',(-10.7837428566908,17.1931958084554,4.38079802170576));
#98278=CARTESIAN_POINT('Ctrl Pts',(-10.6781045261366,17.2016005682292,4.46639356104486));
#98279=CARTESIAN_POINT('Ctrl Pts',(-10.6096085871802,17.2066406280104,4.51099827877615));
#98280=CARTESIAN_POINT('Ctrl Pts',(-10.5236831149352,17.2129376874234,4.55502463241893));
#98281=CARTESIAN_POINT('Ctrl Pts',(-10.5101768129957,17.2139261212104,4.56162166797046));
#98282=CARTESIAN_POINT('Ctrl Pts',(-10.4905205877644,17.2153645010086,4.5707608535365));
#98283=CARTESIAN_POINT('Ctrl Pts',(-10.4844692149484,17.2158073001399,4.5735123796243));
#98284=CARTESIAN_POINT('Ctrl Pts',(-10.4737793434038,17.2165896356766,4.5782642115532));
#98285=CARTESIAN_POINT('Ctrl Pts',(-10.4691506221937,17.2169284270817,4.58028619748973));
#98286=CARTESIAN_POINT('Ctrl Pts',(-10.45956007375,17.217630544414,4.58440241873539));
#98287=CARTESIAN_POINT('Ctrl Pts',(-10.4545966102907,17.2179940003187,4.58649251603001));
#98288=CARTESIAN_POINT('Ctrl Pts',(-10.4418103342571,17.2189306018767,4.59177381818562));
#98289=CARTESIAN_POINT('Ctrl Pts',(-10.4339673150089,17.2195054053169,4.59491497594865));
#98290=CARTESIAN_POINT('Ctrl Pts',(-10.4003828475264,17.221968517575,4.60794814884276));
#98291=CARTESIAN_POINT('Ctrl Pts',(-10.3743339102746,17.2238836234645,4.61701809684796));
#98292=CARTESIAN_POINT('Ctrl Pts',(-10.252953543995,17.2328356201768,4.65455877366912));
#98293=CARTESIAN_POINT('Ctrl Pts',(-10.1545823256587,17.2402157859513,4.6717891575727));
#98294=CARTESIAN_POINT('Ctrl Pts',(-10.0331724901668,17.2490749286032,4.67749001702489));
#98295=CARTESIAN_POINT('Ctrl Pts',(-10.0110781180791,17.2506748555152,4.67790514190264));
#98296=CARTESIAN_POINT('Ctrl Pts',(-9.96710983856224,17.2538200244126,4.67749387588873));
#98297=CARTESIAN_POINT('Ctrl Pts',(-9.94524369011949,17.255365076605,4.67667985743916));
#98298=CARTESIAN_POINT('Ctrl Pts',(-9.91790528943456,17.2572630166728,4.67489827891918));
#98299=CARTESIAN_POINT('Ctrl Pts',(-9.9124017398964,17.257643372882,4.67450076846999));
#98300=CARTESIAN_POINT('Ctrl Pts',(-9.90370414561147,17.25824153848,4.67381108165236));
#98301=CARTESIAN_POINT('Ctrl Pts',(-9.90050823801416,17.2584607055848,4.67354451850083));
#98302=CARTESIAN_POINT('Ctrl Pts',(-9.89480048423873,17.258850960419,4.67304496399591));
#98303=CARTESIAN_POINT('Ctrl Pts',(-9.89228831064863,17.2590223154826,4.67281695836535));
#98304=CARTESIAN_POINT('Ctrl Pts',(-9.88626103793831,17.2594324733508,4.67225039172847));
#98305=CARTESIAN_POINT('Ctrl Pts',(-9.88274670873525,17.2596708439645,4.67190409117164));
#98306=CARTESIAN_POINT('Ctrl Pts',(-9.87205249856307,17.2603939809586,4.67080169985893));
#98307=CARTESIAN_POINT('Ctrl Pts',(-9.86487780036977,17.26087606485,4.66999537654611));
#98308=CARTESIAN_POINT('Ctrl Pts',(-9.80032379330966,17.265189633235,4.66213876912325));
#98309=CARTESIAN_POINT('Ctrl Pts',(-9.74352041525188,17.2688164906964,4.65093753852879));
#98310=CARTESIAN_POINT('Ctrl Pts',(-9.58965229426639,17.2787214322882,4.60863122574422));
#98311=CARTESIAN_POINT('Ctrl Pts',(-9.49546241337616,17.2849157745005,4.56905950376768));
#98312=CARTESIAN_POINT('Ctrl Pts',(-9.39588069493815,17.2924504559308,4.51109676171421));
#98313=CARTESIAN_POINT('Ctrl Pts',(-9.38434746939944,17.2933386171025,4.50411589644992));
#98314=CARTESIAN_POINT('Ctrl Pts',(-9.36748964129111,17.2946613035976,4.49351251718253));
#98315=CARTESIAN_POINT('Ctrl Pts',(-9.36207056644262,17.2950903055287,4.49004167119475));
#98316=CARTESIAN_POINT('Ctrl Pts',(-9.35248854127248,17.2958558270662,4.48379317744511));
#98317=CARTESIAN_POINT('Ctrl Pts',(-9.34831430576273,17.2961916924651,4.4810330574309));
#98318=CARTESIAN_POINT('Ctrl Pts',(-9.33956115870797,17.2969010866548,4.47516471737606));
#98319=CARTESIAN_POINT('Ctrl Pts',(-9.33498632304281,17.2972748279428,4.47205066573273));
#98320=CARTESIAN_POINT('Ctrl Pts',(-9.32292411781731,17.2982682763617,4.46371501841445));
#98321=CARTESIAN_POINT('Ctrl Pts',(-9.31547534105932,17.2988900457865,4.45843850615423));
#98322=CARTESIAN_POINT('Ctrl Pts',(-9.27986661192313,17.3019033369657,4.43258739286108));
#98323=CARTESIAN_POINT('Ctrl Pts',(-9.25257119611444,17.304338894553,4.41085733640836));
#98324=CARTESIAN_POINT('Ctrl Pts',(-9.17540268079448,17.3116110208776,4.34361635342126));
#98325=CARTESIAN_POINT('Ctrl Pts',(-9.12843293248147,17.3165571341783,4.29499575024614));
#98326=CARTESIAN_POINT('Ctrl Pts',(-9.04776862293908,17.3259500261124,4.19570498750087));
#98327=CARTESIAN_POINT('Ctrl Pts',(-9.0133135572525,17.330378977973,4.14591128741427));
#98328=CARTESIAN_POINT('Ctrl Pts',(-8.97790621627555,17.3353012383064,4.08524768353308));
#98329=CARTESIAN_POINT('Ctrl Pts',(-8.97308532936232,17.3359807311223,4.07674676298711));
#98330=CARTESIAN_POINT('Ctrl Pts',(-8.96658451774456,17.3369091122139,4.06494354614598));
#98331=CARTESIAN_POINT('Ctrl Pts',(-8.96481368844185,17.3371632926581,4.06169214930605));
#98332=CARTESIAN_POINT('Ctrl Pts',(-8.96180408813488,17.3375974418566,4.05610368348576));
#98333=CARTESIAN_POINT('Ctrl Pts',(-8.96055781773783,17.3377778705023,4.05377071815689));
#98334=CARTESIAN_POINT('Ctrl Pts',(-8.95797255652792,17.3381534821491,4.04889174188054));
#98335=CARTESIAN_POINT('Ctrl Pts',(-8.95663502096059,17.3383485672149,4.04634499906722));
#98336=CARTESIAN_POINT('Ctrl Pts',(-8.95339401928569,17.3388231957234,4.04011864065652));
#98337=CARTESIAN_POINT('Ctrl Pts',(-8.95150058689536,17.3391021195032,4.03643378609914));
#98338=CARTESIAN_POINT('Ctrl Pts',(-8.94476445295105,17.3401006615646,4.0231525046579));
#98339=CARTESIAN_POINT('Ctrl Pts',(-8.94003355744219,17.3408137503602,4.01349952654305));
#98340=CARTESIAN_POINT('Ctrl Pts',(-8.92855393456318,17.3425777170407,3.98924144625323));
#98341=CARTESIAN_POINT('Ctrl Pts',(-8.92197088422407,17.3436203275388,3.97455994696074));
#98342=CARTESIAN_POINT('Ctrl Pts',(-8.89447730638538,17.3481363925261,3.90971662513464));
#98343=CARTESIAN_POINT('Ctrl Pts',(-8.87675062626698,17.351492021793,3.85827352843769));
#98344=CARTESIAN_POINT('Ctrl Pts',(-8.84144259686948,17.3598984731633,3.72694673421329));
#98345=CARTESIAN_POINT('Ctrl Pts',(-8.82850314153887,17.3649448581125,3.64612689902622));
#98346=CARTESIAN_POINT('Ctrl Pts',(-8.82319971781619,17.3712488727301,3.5496183964485));
#98347=CARTESIAN_POINT('Ctrl Pts',(-8.82266244504893,17.3722371120225,3.53459967744389));
#98348=CARTESIAN_POINT('Ctrl Pts',(-8.82230221160309,17.3736752595121,3.51292921800282));
#98349=CARTESIAN_POINT('Ctrl Pts',(-8.82224799989554,17.3741180241031,3.50628241005698));
#98350=CARTESIAN_POINT('Ctrl Pts',(-8.8222516191197,17.3749003193418,3.49458459559518));
#98351=CARTESIAN_POINT('Ctrl Pts',(-8.82228567526641,17.375239105231,3.4895337099509));
#98352=CARTESIAN_POINT('Ctrl Pts',(-8.8224231775298,17.3759412313941,3.47909792897358));
#98353=CARTESIAN_POINT('Ctrl Pts',(-8.82253107346238,17.3763047017689,3.47371322075556));
#98354=CARTESIAN_POINT('Ctrl Pts',(-8.82290311180482,17.3772413836474,3.45988300138625));
#98355=CARTESIAN_POINT('Ctrl Pts',(-8.82322121166186,17.3778162534867,3.45143937178742));
#98356=CARTESIAN_POINT('Ctrl Pts',(-8.82496519553064,17.3802800566355,3.41544686134525));
#98357=CARTESIAN_POINT('Ctrl Pts',(-8.82726777203367,17.3821958057772,3.38795123295226));
#98358=CARTESIAN_POINT('Ctrl Pts',(-8.84231012943649,17.3911480601531,3.26178944834142));
#98359=CARTESIAN_POINT('Ctrl Pts',(-8.86655299930821,17.3985277403416,3.16491483118665));
#98360=CARTESIAN_POINT('Ctrl Pts',(-8.91069341185114,17.4073864251229,3.05167606897221));
#98361=CARTESIAN_POINT('Ctrl Pts',(-8.91929548709607,17.4089864046491,3.03131989624863));
#98362=CARTESIAN_POINT('Ctrl Pts',(-8.93754226602037,17.4121312993167,2.99131840811716));
#98363=CARTESIAN_POINT('Ctrl Pts',(-8.94717224803877,17.4136760340582,2.97167503094053));
#98364=CARTESIAN_POINT('Ctrl Pts',(-8.95991020370921,17.415573642148,2.94742537254336));
#98365=CARTESIAN_POINT('Ctrl Pts',(-8.96251028017742,17.4159539726808,2.9425588932285));
#98366=CARTESIAN_POINT('Ctrl Pts',(-8.96667556257935,17.4165521069417,2.93489297166834));
#98367=CARTESIAN_POINT('Ctrl Pts',(-8.96821812784317,17.4167712681556,2.9320814183766));
#98368=CARTESIAN_POINT('Ctrl Pts',(-8.97099457766154,17.4171615180117,2.92706957966829));
#98369=CARTESIAN_POINT('Ctrl Pts',(-8.97222404071616,17.4173328739448,2.92486696891829));
#98370=CARTESIAN_POINT('Ctrl Pts',(-8.97519169550874,17.4177430409711,2.91959025480199));
#98371=CARTESIAN_POINT('Ctrl Pts',(-8.97693664652385,17.4179814198171,2.91652000131271));
#98372=CARTESIAN_POINT('Ctrl Pts',(-8.98229116824021,17.418704606922,2.90719655335674));
#98373=CARTESIAN_POINT('Ctrl Pts',(-8.98594453688608,17.4191867321488,2.90096851770535));
#98374=CARTESIAN_POINT('Ctrl Pts',(-9.01937410399039,17.4235017868848,2.84516224096491));
#98375=CARTESIAN_POINT('Ctrl Pts',(-9.05271147142192,17.4271299352077,2.79779919344989));
#98376=CARTESIAN_POINT('Ctrl Pts',(-9.15391153174446,17.4370343584137,2.67442328908591));
#98377=CARTESIAN_POINT('Ctrl Pts',(-9.22833289443858,17.4432270880622,2.6044719750592));
#98378=CARTESIAN_POINT('Ctrl Pts',(-9.32174746321755,17.4507600878111,2.53706158439215));
#98379=CARTESIAN_POINT('Ctrl Pts',(-9.33281653587819,17.4516484883042,2.52935943999387));
#98380=CARTESIAN_POINT('Ctrl Pts',(-9.34936031547011,17.4529714636773,2.51826455415408));
#98381=CARTESIAN_POINT('Ctrl Pts',(-9.35473478414655,17.4534005116124,2.514723752873));
#98382=CARTESIAN_POINT('Ctrl Pts',(-9.36433928730087,17.4541660847305,2.50850841437812));
#98383=CARTESIAN_POINT('Ctrl Pts',(-9.36855788874728,17.4545019553831,2.50581643302681));
#98384=CARTESIAN_POINT('Ctrl Pts',(-9.3774772399631,17.4552113291997,2.50020447180118));
#98385=CARTESIAN_POINT('Ctrl Pts',(-9.38218165776093,17.4555850446643,2.49729058089947));
#98386=CARTESIAN_POINT('Ctrl Pts',(-9.39469879924941,17.4565783505446,2.48965906139158));
#98387=CARTESIAN_POINT('Ctrl Pts',(-9.40254599372701,17.4572000021982,2.48499898616939));
#98388=CARTESIAN_POINT('Ctrl Pts',(-9.44061947325637,17.4602117344973,2.4629834566206));
#98389=CARTESIAN_POINT('Ctrl Pts',(-9.47154917383984,17.4626457955063,2.44688596426713));
#98390=CARTESIAN_POINT('Ctrl Pts',(-9.56426336003494,17.4699110406619,2.40374595428708));
#98391=CARTESIAN_POINT('Ctrl Pts',(-9.62770498123338,17.4748515018915,2.38061004079575));
#98392=CARTESIAN_POINT('Ctrl Pts',(-9.73176023620944,17.4827656947702,2.35249233484872));
#98393=CARTESIAN_POINT('Ctrl Pts',(-9.77125785283919,17.4857257135124,2.34397156772625));
#98394=CARTESIAN_POINT('Ctrl Pts',(-9.81110409010019,17.488629053511,2.33749692571455));
#98395=CARTESIAN_POINT('Origin',(-10.,12.3756328852638,3.5));
#98396=CARTESIAN_POINT('',(-9.81110406180285,18.0875733665016,2.3374969303126));
#98397=CARTESIAN_POINT('',(-9.81110440024615,17.9879475328942,2.33749687531877));
#98398=CARTESIAN_POINT('',(-9.81110406371068,12.3756328852638,2.3374969300026));
#98399=CARTESIAN_POINT('Ctrl Pts',(-9.81110406180295,18.0875733665016,2.33749693031259));
#98400=CARTESIAN_POINT('Ctrl Pts',(-9.80411576776501,18.0871092595767,2.33863246310653));
#98401=CARTESIAN_POINT('Ctrl Pts',(-9.79714781030033,18.0866439604605,2.33982924799533));
#98402=CARTESIAN_POINT('Ctrl Pts',(-9.78457900609619,18.085799814295,2.34210480910901));
#98403=CARTESIAN_POINT('Ctrl Pts',(-9.77898416092229,18.0854223152074,2.34315970216565));
#98404=CARTESIAN_POINT('Ctrl Pts',(-9.76860887088543,18.0847189211277,2.34519394788202));
#98405=CARTESIAN_POINT('Ctrl Pts',(-9.76382641997234,18.0843933690987,2.34616252811452));
#98406=CARTESIAN_POINT('Ctrl Pts',(-9.7543469513773,18.0837453786588,2.34814378982686));
#98407=CARTESIAN_POINT('Ctrl Pts',(-9.74964983682037,18.083422974984,2.34915555185095));
#98408=CARTESIAN_POINT('Ctrl Pts',(-9.74029428288418,18.0827781235177,2.35123073065637));
#98409=CARTESIAN_POINT('Ctrl Pts',(-9.73563586249765,18.0824556919656,2.35229381140935));
#98410=CARTESIAN_POINT('Ctrl Pts',(-9.72311122132061,18.0815851196476,2.35523231143811));
#98411=CARTESIAN_POINT('Ctrl Pts',(-9.71525775263558,18.0810353104942,2.35716042096048));
#98412=CARTESIAN_POINT('Ctrl Pts',(-9.6857551707701,18.0789546778497,2.36472659120069));
#98413=CARTESIAN_POINT('Ctrl Pts',(-9.66424953609222,18.0774069270469,2.37089990130395));
#98414=CARTESIAN_POINT('Ctrl Pts',(-9.53566511287724,18.0679574477091,2.41180908384498));
#98415=CARTESIAN_POINT('Ctrl Pts',(-9.43385349669055,18.0595689109437,2.46113747362027));
#98416=CARTESIAN_POINT('Ctrl Pts',(-9.31081622845497,18.0487959780189,2.54427290530359));
#98417=CARTESIAN_POINT('Ctrl Pts',(-9.28195077056037,18.0462223388745,2.56576533165001));
#98418=CARTESIAN_POINT('Ctrl Pts',(-9.2493763596898,18.043301450093,2.59242264683703));
#98419=CARTESIAN_POINT('Ctrl Pts',(-9.24467125780358,18.0428791414985,2.59633468771121));
#98420=CARTESIAN_POINT('Ctrl Pts',(-9.23747131009495,18.042232548807,2.60241658430765));
#98421=CARTESIAN_POINT('Ctrl Pts',(-9.23495484127171,18.0420064886057,2.60456050073622));
#98422=CARTESIAN_POINT('Ctrl Pts',(-9.23032998835346,18.0415909543789,2.60853439258517));
#98423=CARTESIAN_POINT('Ctrl Pts',(-9.22821908935006,18.0414012716774,2.61036126304491));
#98424=CARTESIAN_POINT('Ctrl Pts',(-9.22344137210073,18.0409718815143,2.61452592568277));
#98425=CARTESIAN_POINT('Ctrl Pts',(-9.22077860474996,18.0407325124069,2.61686826754653));
#98426=CARTESIAN_POINT('Ctrl Pts',(-9.21388371865778,18.0401124230115,2.6229889168206));
#98427=CARTESIAN_POINT('Ctrl Pts',(-9.20966818703791,18.0397330291611,2.6267858931517));
#98428=CARTESIAN_POINT('Ctrl Pts',(-9.18113316722225,18.0371616909793,2.6528636315379));
#98429=CARTESIAN_POINT('Ctrl Pts',(-9.15772900839733,18.0350365285971,2.67612929158634));
#98430=CARTESIAN_POINT('Ctrl Pts',(-9.11432945725783,18.030988903081,2.72305762052059));
#98431=CARTESIAN_POINT('Ctrl Pts',(-9.09423036443751,18.0290636359274,2.74658556799021));
#98432=CARTESIAN_POINT('Ctrl Pts',(-9.04517756726749,18.024154224547,2.8088110062958));
#98433=CARTESIAN_POINT('Ctrl Pts',(-9.01763740792034,18.0211858772441,2.84854643952578));
#98434=CARTESIAN_POINT('Ctrl Pts',(-8.9740473722929,18.0159255826458,2.92051673623503));
#98435=CARTESIAN_POINT('Ctrl Pts',(-8.95689005064501,18.013660006794,2.95200276185415));
#98436=CARTESIAN_POINT('Ctrl Pts',(-8.9345101546078,18.0103647898004,2.99794471395833));
#98437=CARTESIAN_POINT('Ctrl Pts',(-8.92809223527411,18.0093726298812,3.01179734528906));
#98438=CARTESIAN_POINT('Ctrl Pts',(-8.91854321951504,18.0078176407391,3.03350488337976));
#98439=CARTESIAN_POINT('Ctrl Pts',(-8.91522424931074,18.0072609513128,3.04127565292638));
#98440=CARTESIAN_POINT('Ctrl Pts',(-8.90915996787377,18.0062122130788,3.05590800999441));
#98441=CARTESIAN_POINT('Ctrl Pts',(-8.90639505427279,18.0057208380292,3.06276106098184));
#98442=CARTESIAN_POINT('Ctrl Pts',(-8.90182819942725,18.0048861333767,3.07439471923412));
#98443=CARTESIAN_POINT('Ctrl Pts',(-8.89999251528954,18.0045439359986,3.07916191858856));
#98444=CARTESIAN_POINT('Ctrl Pts',(-8.89638616142106,18.0038580111336,3.08871230149107));
#98445=CARTESIAN_POINT('Ctrl Pts',(-8.89461543377078,18.00351429434,3.0934953444588));
#98446=CARTESIAN_POINT('Ctrl Pts',(-8.89077204816991,18.0027526120407,3.10408781551743));
#98447=CARTESIAN_POINT('Ctrl Pts',(-8.88871385948728,18.0023341803633,3.1099022964317));
#98448=CARTESIAN_POINT('Ctrl Pts',(-8.88188040603884,18.0009081886493,3.12970015931277));
#98449=CARTESIAN_POINT('Ctrl Pts',(-8.87732282605005,17.9998935823307,3.14375664644724));
#98450=CARTESIAN_POINT('Ctrl Pts',(-8.84947384722369,17.9932549225941,3.23549719002195));
#98451=CARTESIAN_POINT('Ctrl Pts',(-8.8339992366159,17.9873794006879,3.31531145062842));
#98452=CARTESIAN_POINT('Ctrl Pts',(-8.82201795511681,17.9774156360952,3.45055094926967));
#98453=CARTESIAN_POINT('Ctrl Pts',(-8.82099223672586,17.9733857360215,3.50530786869955));
#98454=CARTESIAN_POINT('Ctrl Pts',(-8.82459799146867,17.9683057693371,3.57606490475995));
#98455=CARTESIAN_POINT('Ctrl Pts',(-8.82575125828175,17.9671582550904,3.59217211647325));
#98456=CARTESIAN_POINT('Ctrl Pts',(-8.82822615749851,17.9652680938578,3.61898448011892));
#98457=CARTESIAN_POINT('Ctrl Pts',(-8.82936421732331,17.9645177737649,3.62970400731036));
#98458=CARTESIAN_POINT('Ctrl Pts',(-8.83114385746329,17.9634891274718,3.64452538643236));
#98459=CARTESIAN_POINT('Ctrl Pts',(-8.83166014318969,17.96320440937,3.64864134542963));
#98460=CARTESIAN_POINT('Ctrl Pts',(-8.83257149048436,17.9627241501477,3.65560855462035));
#98461=CARTESIAN_POINT('Ctrl Pts',(-8.83295527475605,17.9625279938959,3.65846121625734));
#98462=CARTESIAN_POINT('Ctrl Pts',(-8.83371180018087,17.9621527273921,3.66393258842002));
#98463=CARTESIAN_POINT('Ctrl Pts',(-8.83408290843956,17.9619735240023,3.66655147715855));
#98464=CARTESIAN_POINT('Ctrl Pts',(-8.83499435631392,17.9615447809174,3.672831147619));
#98465=CARTESIAN_POINT('Ctrl Pts',(-8.8355431363475,17.9612957070293,3.67649070520377));
#98466=CARTESIAN_POINT('Ctrl Pts',(-8.83760061054857,17.9603936228668,3.68978355142038));
#98467=CARTESIAN_POINT('Ctrl Pts',(-8.8392117224147,17.9597460167709,3.69940091986435));
#98468=CARTESIAN_POINT('Ctrl Pts',(-8.85179995574672,17.9550745952236,3.7692126977654));
#98469=CARTESIAN_POINT('Ctrl Pts',(-8.86733522570546,17.951264765726,3.82849857782535));
#98470=CARTESIAN_POINT('Ctrl Pts',(-8.90936975260595,17.9433310961337,3.94955829604754));
#98471=CARTESIAN_POINT('Ctrl Pts',(-8.93668015428111,17.9392222398299,4.01081041564168));
#98472=CARTESIAN_POINT('Ctrl Pts',(-8.98583327531172,17.9327590883663,4.09980554772121));
#98473=CARTESIAN_POINT('Ctrl Pts',(-9.00395612056176,17.9305170872061,4.12944187064315));
#98474=CARTESIAN_POINT('Ctrl Pts',(-9.02845617085175,17.9276261289549,4.1657933513373));
#98475=CARTESIAN_POINT('Ctrl Pts',(-9.03363958136156,17.9270216858615,4.17329468451222));
#98476=CARTESIAN_POINT('Ctrl Pts',(-9.04210754609234,17.9260451771105,4.18525011799301));
#98477=CARTESIAN_POINT('Ctrl Pts',(-9.04533737582244,17.9256751889192,4.18974266917796));
#98478=CARTESIAN_POINT('Ctrl Pts',(-9.05154982945142,17.9249680956219,4.19825668870298));
#98479=CARTESIAN_POINT('Ctrl Pts',(-9.05452668289495,17.9246312174058,4.20228223289569));
#98480=CARTESIAN_POINT('Ctrl Pts',(-9.06139298720138,17.923858519254,4.21144462343235));
#98481=CARTESIAN_POINT('Ctrl Pts',(-9.06529907761628,17.9234220592209,4.2165687402572));
#98482=CARTESIAN_POINT('Ctrl Pts',(-9.07752836170236,17.9220649333365,4.23234131485983));
#98483=CARTESIAN_POINT('Ctrl Pts',(-9.08599269692799,17.9211387494539,4.24287842098226));
#98484=CARTESIAN_POINT('Ctrl Pts',(-9.15955641909835,17.9131954505821,4.33129583125409));
#98485=CARTESIAN_POINT('Ctrl Pts',(-9.23427979769553,17.905760754493,4.40058992540698));
#98486=CARTESIAN_POINT('Ctrl Pts',(-9.3641878541863,17.8940621894593,4.49307736083118));
#98487=CARTESIAN_POINT('Ctrl Pts',(-9.41386803130244,17.8898326686735,4.52318651582399));
#98488=CARTESIAN_POINT('Ctrl Pts',(-9.47201008195407,17.8852906914201,4.55279339532869));
#98489=CARTESIAN_POINT('Ctrl Pts',(-9.4784801191875,17.8847907278865,4.55601340298587));
#98490=CARTESIAN_POINT('Ctrl Pts',(-9.48815724486811,17.8840514858372,4.56071887956098));
#98491=CARTESIAN_POINT('Ctrl Pts',(-9.49134189391957,17.883809574113,4.56224972552698));
#98492=CARTESIAN_POINT('Ctrl Pts',(-9.49681268654569,17.883396399321,4.56484926538973));
#98493=CARTESIAN_POINT('Ctrl Pts',(-9.49909542239117,17.8832247125377,4.56592496686999));
#98494=CARTESIAN_POINT('Ctrl Pts',(-9.50428753921127,17.8828358368276,4.56835130310064));
#98495=CARTESIAN_POINT('Ctrl Pts',(-9.50719899096266,17.8826189262557,4.5696973949353));
#98496=CARTESIAN_POINT('Ctrl Pts',(-9.51513328454796,17.8820308243359,4.57332649784314));
#98497=CARTESIAN_POINT('Ctrl Pts',(-9.52016680589226,17.8816610141385,4.57558617112916));
#98498=CARTESIAN_POINT('Ctrl Pts',(-9.54521779952762,17.8798358578718,4.58662132805739));
#98499=CARTESIAN_POINT('Ctrl Pts',(-9.56546241528391,17.8784091906423,4.5948744200728));
#98500=CARTESIAN_POINT('Ctrl Pts',(-9.60659485582774,17.875583885374,4.61032197373736));
#98501=CARTESIAN_POINT('Ctrl Pts',(-9.62747841984632,17.8741862407253,4.61750179535646));
#98502=CARTESIAN_POINT('Ctrl Pts',(-9.7435267706381,17.8665587824645,4.65378437489958));
#98503=CARTESIAN_POINT('Ctrl Pts',(-9.84187762461019,17.8605657183773,4.67132177802412));
#98504=CARTESIAN_POINT('Ctrl Pts',(-9.96880000747504,17.8524211489929,4.67765942916407));
#98505=CARTESIAN_POINT('Ctrl Pts',(-9.99637362433313,17.8506302551485,4.67806698838191));
#98506=CARTESIAN_POINT('Ctrl Pts',(-10.0323825152056,17.8482514033899,4.67733505562131));
#98507=CARTESIAN_POINT('Ctrl Pts',(-10.0408282216877,17.8476905967024,4.67707243218723));
#98508=CARTESIAN_POINT('Ctrl Pts',(-10.0546525339866,17.8467676380317,4.67649359684837));
#98509=CARTESIAN_POINT('Ctrl Pts',(-10.0600331889625,17.8464071646814,4.6762313112127));
#98510=CARTESIAN_POINT('Ctrl Pts',(-10.0704569982453,17.8457063348852,4.67565148189664));
#98511=CARTESIAN_POINT('Ctrl Pts',(-10.0755002890819,17.8453661239302,4.67533837700627));
#98512=CARTESIAN_POINT('Ctrl Pts',(-10.087176663426,17.8445757591754,4.67453800543552));
#98513=CARTESIAN_POINT('Ctrl Pts',(-10.0938078919757,17.8441248767153,4.67402698993955));
#98514=CARTESIAN_POINT('Ctrl Pts',(-10.1154214384111,17.8426484962089,4.67217712532677));
#98515=CARTESIAN_POINT('Ctrl Pts',(-10.1303819706907,17.8416158864112,4.6706074606143));
#98516=CARTESIAN_POINT('Ctrl Pts',(-10.2258570069655,17.8349544951473,4.65873730688055));
#98517=CARTESIAN_POINT('Ctrl Pts',(-10.3051407104166,17.829074017416,4.64042454488854));
#98518=CARTESIAN_POINT('Ctrl Pts',(-10.4336401811532,17.8191051179038,4.59637726004835));
#98519=CARTESIAN_POINT('Ctrl Pts',(-10.4840863978927,17.8150752203405,4.57505713107841));
#98520=CARTESIAN_POINT('Ctrl Pts',(-10.5472687349049,17.8099952564642,4.54300176558728));
#98521=CARTESIAN_POINT('Ctrl Pts',(-10.5615165047143,17.8088477426083,4.5354008988032));
#98522=CARTESIAN_POINT('Ctrl Pts',(-10.5850079534667,17.8069575819491,4.52224113535079));
#98523=CARTESIAN_POINT('Ctrl Pts',(-10.5943393840663,17.8062072620444,4.51684411867589));
#98524=CARTESIAN_POINT('Ctrl Pts',(-10.6071577347474,17.8051786159641,4.50919361591435));
#98525=CARTESIAN_POINT('Ctrl Pts',(-10.6107084729582,17.8048938978903,4.50704887251629));
#98526=CARTESIAN_POINT('Ctrl Pts',(-10.6167037077458,17.8044136387012,4.50338421551919));
#98527=CARTESIAN_POINT('Ctrl Pts',(-10.6191540778376,17.8042174824549,4.50187403183936));
#98528=CARTESIAN_POINT('Ctrl Pts',(-10.6238455546558,17.8038422159507,4.49895884926265));
#98529=CARTESIAN_POINT('Ctrl Pts',(-10.6260874879379,17.803663012555,4.49755526983949));
#98530=CARTESIAN_POINT('Ctrl Pts',(-10.631454504557,17.8032342694416,4.49416998751971));
#98531=CARTESIAN_POINT('Ctrl Pts',(-10.6345750386283,17.802985195531,4.49218107051237));
#98532=CARTESIAN_POINT('Ctrl Pts',(-10.6458838994318,17.8020831111688,4.48489802796709));
#98533=CARTESIAN_POINT('Ctrl Pts',(-10.654016050262,17.8014355048987,4.47951679836229));
#98534=CARTESIAN_POINT('Ctrl Pts',(-10.7126834119856,17.7967641004027,4.43963883518299));
#98535=CARTESIAN_POINT('Ctrl Pts',(-10.76053578613,17.792954286246,4.40134682148313));
#98536=CARTESIAN_POINT('Ctrl Pts',(-10.8540574977807,17.7850206203113,4.31373387201843));
#98537=CARTESIAN_POINT('Ctrl Pts',(-10.8989204011498,17.7809117527647,4.26388383497586));
#98538=CARTESIAN_POINT('Ctrl Pts',(-10.9602525442296,17.7744485858551,4.18280004077958));
#98539=CARTESIAN_POINT('Ctrl Pts',(-10.9799636855964,17.7722065812215,4.15419542725544));
#98540=CARTESIAN_POINT('Ctrl Pts',(-11.0032180383216,17.7693156190491,4.11703465567986));
#98541=CARTESIAN_POINT('Ctrl Pts',(-11.0079647995188,17.7687111756595,4.10924966468374));
#98542=CARTESIAN_POINT('Ctrl Pts',(-11.0154460157162,17.7677346665446,4.09665322142751));
#98543=CARTESIAN_POINT('Ctrl Pts',(-11.0182378460213,17.7673646782883,4.09187613959951));
#98544=CARTESIAN_POINT('Ctrl Pts',(-11.0234915783654,17.7666575849425,4.08273932280643));
#98545=CARTESIAN_POINT('Ctrl Pts',(-11.025959549915,17.7663207067433,4.07838320336483));
#98546=CARTESIAN_POINT('Ctrl Pts',(-11.031539899148,17.7655480087373,4.06838544415476));
#98547=CARTESIAN_POINT('Ctrl Pts',(-11.0346338828214,17.7651115488339,4.06273377569896));
#98548=CARTESIAN_POINT('Ctrl Pts',(-11.0440737868741,17.7637544237597,4.04514920178676));
#98549=CARTESIAN_POINT('Ctrl Pts',(-11.0502605992841,17.7628282405671,4.03313260241117));
#98550=CARTESIAN_POINT('Ctrl Pts',(-11.1011424803266,17.7548849371542,3.92998072691506));
#98551=CARTESIAN_POINT('Ctrl Pts',(-11.1340807275815,17.7474502350925,3.83354244262143));
#98552=CARTESIAN_POINT('Ctrl Pts',(-11.1657786386585,17.7357516688753,3.67725656013453));
#98553=CARTESIAN_POINT('Ctrl Pts',(-11.1730944875407,17.7315221526145,3.61962711772648));
#98554=CARTESIAN_POINT('Ctrl Pts',(-11.1765118980603,17.7269801796391,3.55447054712337));
#98555=CARTESIAN_POINT('Ctrl Pts',(-11.1768239908109,17.7264802162248,3.54725026979736));
#98556=CARTESIAN_POINT('Ctrl Pts',(-11.1771897000827,17.7257409743167,3.53649599231491));
#98557=CARTESIAN_POINT('Ctrl Pts',(-11.1772938969083,17.7254990626158,3.53296404956283));
#98558=CARTESIAN_POINT('Ctrl Pts',(-11.1774452594416,17.7250858878498,3.52690894722474));
#98559=CARTESIAN_POINT('Ctrl Pts',(-11.1775002128651,17.7249142010694,3.52438605274794));
#98560=CARTESIAN_POINT('Ctrl Pts',(-11.1776066004691,17.724525325347,3.51865596824399));
#98561=CARTESIAN_POINT('Ctrl Pts',(-11.1776530422394,17.72430841476,3.51544873280664));
#98562=CARTESIAN_POINT('Ctrl Pts',(-11.1777437268435,17.723720312759,3.50672433023728));
#98563=CARTESIAN_POINT('Ctrl Pts',(-11.1777623058643,17.7233505024961,3.50120689186058));
#98564=CARTESIAN_POINT('Ctrl Pts',(-11.1776621165944,17.7215253453811,3.47383322505357));
#98565=CARTESIAN_POINT('Ctrl Pts',(-11.1769737301889,17.7200986774005,3.45198180320903));
#98566=CARTESIAN_POINT('Ctrl Pts',(-11.1743682783242,17.7172733715659,3.4081216043102));
#98567=CARTESIAN_POINT('Ctrl Pts',(-11.1724395695005,17.7158757270746,3.3861226709214));
#98568=CARTESIAN_POINT('Ctrl Pts',(-11.1584188701966,17.7082482678743,3.26534573099039));
#98569=CARTESIAN_POINT('Ctrl Pts',(-11.1344649935851,17.7022552026835,3.16835776015286));
#98570=CARTESIAN_POINT('Ctrl Pts',(-11.0886647295067,17.6941106334478,3.04981750809907));
#98571=CARTESIAN_POINT('Ctrl Pts',(-11.0778291336374,17.6923197411514,3.02445890077501));
#98572=CARTESIAN_POINT('Ctrl Pts',(-11.0625237048422,17.6899408911618,2.99185647983035));
#98573=CARTESIAN_POINT('Ctrl Pts',(-11.0588507913954,17.6893800846437,2.98424671031694));
#98574=CARTESIAN_POINT('Ctrl Pts',(-11.0527027005779,17.6884571261806,2.97185124530459));
#98575=CARTESIAN_POINT('Ctrl Pts',(-11.0502759606193,17.6880966528669,2.96704175792726));
#98576=CARTESIAN_POINT('Ctrl Pts',(-11.0455091786332,17.6873958230908,2.95775360500639));
#98577=CARTESIAN_POINT('Ctrl Pts',(-11.0431731366546,17.687055612119,2.95327301047068));
#98578=CARTESIAN_POINT('Ctrl Pts',(-11.0376957167169,17.68626524725,2.94293007944702));
#98579=CARTESIAN_POINT('Ctrl Pts',(-11.0345333943406,17.6858143646916,2.93707909106465));
#98580=CARTESIAN_POINT('Ctrl Pts',(-11.024057880102,17.6843379835284,2.91808352830516));
#98581=CARTESIAN_POINT('Ctrl Pts',(-11.0165426558326,17.6833053731633,2.9050526794377));
#98582=CARTESIAN_POINT('Ctrl Pts',(-10.9668893240913,17.6766440032917,2.82264594396539));
#98583=CARTESIAN_POINT('Ctrl Pts',(-10.9179310513474,17.670763549706,2.75765134264615));
#98584=CARTESIAN_POINT('Ctrl Pts',(-10.8254550731689,17.6607946563338,2.65815033908663));
#98585=CARTESIAN_POINT('Ctrl Pts',(-10.7854704139677,17.6567647405241,2.62072545196242));
#98586=CARTESIAN_POINT('Ctrl Pts',(-10.7305004157303,17.6516847562364,2.57602765458157));
#98587=CARTESIAN_POINT('Ctrl Pts',(-10.7177644055167,17.6505372395401,2.56609954184605));
#98588=CARTESIAN_POINT('Ctrl Pts',(-10.6961921052441,17.6486470747133,2.54998536988366));
#98589=CARTESIAN_POINT('Ctrl Pts',(-10.6874680506366,17.6478967534409,2.54365333434536));
#98590=CARTESIAN_POINT('Ctrl Pts',(-10.6752677240596,17.6468681058139,2.53505141580833));
#98591=CARTESIAN_POINT('Ctrl Pts',(-10.6718648660031,17.6465833875367,2.53267902305687));
#98592=CARTESIAN_POINT('Ctrl Pts',(-10.6660796942342,17.6461031281056,2.52869099250927));
#98593=CARTESIAN_POINT('Ctrl Pts',(-10.6637038829593,17.6459069718193,2.52706603331727));
#98594=CARTESIAN_POINT('Ctrl Pts',(-10.6591334250081,17.6455317053185,2.52396455667966));
#98595=CARTESIAN_POINT('Ctrl Pts',(-10.6569397392817,17.6453525019657,2.5224867070541));
#98596=CARTESIAN_POINT('Ctrl Pts',(-10.651665181763,17.6449237590594,2.51895910061311));
#98597=CARTESIAN_POINT('Ctrl Pts',(-10.6485795678827,17.644674685312,2.51691643262635));
#98598=CARTESIAN_POINT('Ctrl Pts',(-10.6373285815162,17.6437726024014,2.50954433928428));
#98599=CARTESIAN_POINT('Ctrl Pts',(-10.6291064596758,17.6431249973965,2.5043016449291));
#98600=CARTESIAN_POINT('Ctrl Pts',(-10.5688230838811,17.6384534685661,2.46690788475853));
#98601=CARTESIAN_POINT('Ctrl Pts',(-10.5143845816141,17.6346435425509,2.43875096703978));
#98602=CARTESIAN_POINT('Ctrl Pts',(-10.3963210566087,17.6267098499502,2.38891653997269));
#98603=CARTESIAN_POINT('Ctrl Pts',(-10.3325406240363,17.6226010643856,2.36819041117671));
#98604=CARTESIAN_POINT('Ctrl Pts',(-10.2335292170158,17.6161380101065,2.34511259373766));
#98605=CARTESIAN_POINT('Ctrl Pts',(-10.1993825809055,17.6138960308008,2.33873041866766));
#98606=CARTESIAN_POINT('Ctrl Pts',(-10.1559783205597,17.6110050972218,2.33258877783548));
#98607=CARTESIAN_POINT('Ctrl Pts',(-10.1469360642581,17.6104006559921,2.3314162488708));
#98608=CARTESIAN_POINT('Ctrl Pts',(-10.1323862872003,17.6094241495307,2.32970108589526));
#98609=CARTESIAN_POINT('Ctrl Pts',(-10.1268868477128,17.6090541617477,2.32909206019663));
#98610=CARTESIAN_POINT('Ctrl Pts',(-10.1164033813455,17.6083470687559,2.32800580967398));
#98611=CARTESIAN_POINT('Ctrl Pts',(-10.1114201907177,17.6080101904338,2.32752156987279));
#98612=CARTESIAN_POINT('Ctrl Pts',(-10.1000173315549,17.6072374913649,2.32648685127655));
#98613=CARTESIAN_POINT('Ctrl Pts',(-10.093595976871,17.6068010305153,2.32595725500094));
#98614=CARTESIAN_POINT('Ctrl Pts',(-10.0736924512961,17.6054438995328,2.32448005154252));
#98615=CARTESIAN_POINT('Ctrl Pts',(-10.0601984856706,17.6045177113087,2.32371183698976));
#98616=CARTESIAN_POINT('Ctrl Pts',(-9.96781450314467,17.598132555985,2.32004616711968));
#98617=CARTESIAN_POINT('Ctrl Pts',(-9.88888725891994,17.5924370348984,2.32485788425224));
#98618=CARTESIAN_POINT('Ctrl Pts',(-9.81110406371068,17.5866589100326,2.3374969300026));
#98619=CARTESIAN_POINT('Ctrl Pts',(-9.81110409010019,17.488629053511,2.33749692571455));
#98620=CARTESIAN_POINT('Ctrl Pts',(-9.83100301365312,17.4900789605701,2.3342635361832));
#98621=CARTESIAN_POINT('Ctrl Pts',(-9.85098889505721,17.4915145218242,2.33154042954652));
#98622=CARTESIAN_POINT('Ctrl Pts',(-9.88075068876469,17.4936127359325,2.32826194785942));
#98623=CARTESIAN_POINT('Ctrl Pts',(-9.89047251007087,17.4942918938412,2.3273132534345));
#98624=CARTESIAN_POINT('Ctrl Pts',(-9.90389375181683,17.4952199036933,2.32617192319059));
#98625=CARTESIAN_POINT('Ctrl Pts',(-9.90758362860465,17.4954740422306,2.32587565391234));
#98626=CARTESIAN_POINT('Ctrl Pts',(-9.91391216649941,17.4959081385477,2.32539753862048));
#98627=CARTESIAN_POINT('Ctrl Pts',(-9.91655012696285,17.4960885559782,2.32520717724369));
#98628=CARTESIAN_POINT('Ctrl Pts',(-9.92205868388094,17.4964641654574,2.32482831497533));
#98629=CARTESIAN_POINT('Ctrl Pts',(-9.92492935769447,17.4966592594639,2.32464144324194));
#98630=CARTESIAN_POINT('Ctrl Pts',(-9.93193637675553,17.4971339443372,2.32421108445177));
#98631=CARTESIAN_POINT('Ctrl Pts',(-9.93607343056122,17.4974129151901,2.32397890080429));
#98632=CARTESIAN_POINT('Ctrl Pts',(-9.95095149768667,17.4984118161063,2.32322264291081));
#98633=CARTESIAN_POINT('Ctrl Pts',(-9.96169873869972,17.4991252105098,2.32282382908586));
#98634=CARTESIAN_POINT('Ctrl Pts',(-9.98854273719769,17.5008900864926,2.3221957298625));
#98635=CARTESIAN_POINT('Ctrl Pts',(-10.0046419522436,17.5019332897364,2.32214912920342));
#98636=CARTESIAN_POINT('Ctrl Pts',(-10.0751296890812,17.5064535852282,2.32339047285294));
#98637=CARTESIAN_POINT('Ctrl Pts',(-10.1293942273352,17.5098126276164,2.32811582350615));
#98638=CARTESIAN_POINT('Ctrl Pts',(-10.2637115757156,17.518217883783,2.34925949867592));
#98639=CARTESIAN_POINT('Ctrl Pts',(-10.3427361778212,17.5232598028131,2.37027556711188));
#98640=CARTESIAN_POINT('Ctrl Pts',(-10.4329982674911,17.5295589068715,2.40463090521283));
#98641=CARTESIAN_POINT('Ctrl Pts',(-10.4469406957582,17.5305472838744,2.41024547053482));
#98642=CARTESIAN_POINT('Ctrl Pts',(-10.4668889245423,17.5319855958489,2.41872575977277));
#98643=CARTESIAN_POINT('Ctrl Pts',(-10.4729842445534,17.5324283848964,2.42137812380982));
#98644=CARTESIAN_POINT('Ctrl Pts',(-10.48367102806,17.5332107086682,2.42613645535825));
#98645=CARTESIAN_POINT('Ctrl Pts',(-10.4882720471708,17.5335494984627,2.42822064654809));
#98646=CARTESIAN_POINT('Ctrl Pts',(-10.497750861408,17.5342516183721,2.43258810772595));
#98647=CARTESIAN_POINT('Ctrl Pts',(-10.5026266780322,17.5346150785005,2.43487536472795));
#98648=CARTESIAN_POINT('Ctrl Pts',(-10.51511086392,17.5355517035034,2.44083653568251));
#98649=CARTESIAN_POINT('Ctrl Pts',(-10.5226955873581,17.5361265263251,2.44455897239597));
#98650=CARTESIAN_POINT('Ctrl Pts',(-10.5548654137709,17.5385898402272,2.46077911703653));
#98651=CARTESIAN_POINT('Ctrl Pts',(-10.5790457141355,17.5405051338542,2.47405579497926));
#98652=CARTESIAN_POINT('Ctrl Pts',(-10.6882005363853,17.5494572057466,2.53907800328941));
#98653=CARTESIAN_POINT('Ctrl Pts',(-10.7668617734872,17.5568372297759,2.6006067872924));
#98654=CARTESIAN_POINT('Ctrl Pts',(-10.8523854214365,17.5656962387672,2.68696724661909));
#98655=CARTESIAN_POINT('Ctrl Pts',(-10.8674873018161,17.5672961810296,2.70310035784563));
#98656=CARTESIAN_POINT('Ctrl Pts',(-10.8966202717766,17.5704412699039,2.73603297017059));
#98657=CARTESIAN_POINT('Ctrl Pts',(-10.9106554197756,17.5719862294634,2.75281836830902));
#98658=CARTESIAN_POINT('Ctrl Pts',(-10.9276358720918,17.5738840726602,2.77431605024232));
#98659=CARTESIAN_POINT('Ctrl Pts',(-10.9310254881816,17.5742644213776,2.77866994414256));
#98660=CARTESIAN_POINT('Ctrl Pts',(-10.9363366669054,17.5748625778322,2.7855918582262));
#98661=CARTESIAN_POINT('Ctrl Pts',(-10.9382785002935,17.5750817432182,2.78814411336615));
#98662=CARTESIAN_POINT('Ctrl Pts',(-10.9417291026675,17.5754719965999,2.79271807397449));
#98663=CARTESIAN_POINT('Ctrl Pts',(-10.9432417938916,17.5756433519171,2.79473668454327));
#98664=CARTESIAN_POINT('Ctrl Pts',(-10.9468565946784,17.5760535124572,2.79959288855108));
#98665=CARTESIAN_POINT('Ctrl Pts',(-10.9489524398623,17.5762918854726,2.80243509237313));
#98666=CARTESIAN_POINT('Ctrl Pts',(-10.9552941345106,17.5770150370864,2.81111662617358));
#98667=CARTESIAN_POINT('Ctrl Pts',(-10.959499200563,17.5774971330373,2.8169857419205));
#98668=CARTESIAN_POINT('Ctrl Pts',(-10.9968899294645,17.5818111349828,2.8701997830073));
#98669=CARTESIAN_POINT('Ctrl Pts',(-11.0266060303766,17.5854383689854,2.91989673982626));
#98670=CARTESIAN_POINT('Ctrl Pts',(-11.0982026866433,17.5953431592931,3.06250989536388));
#98671=CARTESIAN_POINT('Ctrl Pts',(-11.1318724228655,17.6015370310837,3.15895819132559));
#98672=CARTESIAN_POINT('Ctrl Pts',(-11.1554945585162,17.6090712219406,3.27172571190887));
#98673=CARTESIAN_POINT('Ctrl Pts',(-11.1580318344068,17.609959452956,3.28496727807221));
#98674=CARTESIAN_POINT('Ctrl Pts',(-11.1614435802468,17.6112822237581,3.30458943678742));
#98675=CARTESIAN_POINT('Ctrl Pts',(-11.1624939908945,17.6117112391158,3.31093864309729));
#98676=CARTESIAN_POINT('Ctrl Pts',(-11.164268610167,17.6124767757069,3.32223974347204));
#98677=CARTESIAN_POINT('Ctrl Pts',(-11.1650133967928,17.6128126426386,3.3271882834147));
#98678=CARTESIAN_POINT('Ctrl Pts',(-11.1665153492769,17.6135220308798,3.33761888103181));
#98679=CARTESIAN_POINT('Ctrl Pts',(-11.1672654564537,17.6138957646291,3.3431018156406));
#98680=CARTESIAN_POINT('Ctrl Pts',(-11.1691503335468,17.614889171436,3.35764173560786));
#98681=CARTESIAN_POINT('Ctrl Pts',(-11.1702184834608,17.6155109064793,3.36670682437764));
#98682=CARTESIAN_POINT('Ctrl Pts',(-11.1748587628557,17.6185237424583,3.41045781029342));
#98683=CARTESIAN_POINT('Ctrl Pts',(-11.1769943377901,17.6209588630255,3.44527516423312));
#98684=CARTESIAN_POINT('Ctrl Pts',(-11.1787204378722,17.6282289792381,3.54758692397761));
#98685=CARTESIAN_POINT('Ctrl Pts',(-11.1740604166206,17.6331734412647,3.61500709026996));
#98686=CARTESIAN_POINT('Ctrl Pts',(-11.1543282571356,17.6425670100796,3.74141248401991));
#98687=CARTESIAN_POINT('Ctrl Pts',(-11.1404080268727,17.6469982779299,3.80037434751222));
#98688=CARTESIAN_POINT('Ctrl Pts',(-11.1190475394232,17.6519225596224,3.86731884001591));
#98689=CARTESIAN_POINT('Ctrl Pts',(-11.1159616712497,17.6526019510228,3.87659008164399));
#98690=CARTESIAN_POINT('Ctrl Pts',(-11.1115478807817,17.6535302197006,3.8893200183388));
#98691=CARTESIAN_POINT('Ctrl Pts',(-11.1103185980832,17.6537843874583,3.89281214292862));
#98692=CARTESIAN_POINT('Ctrl Pts',(-11.1081828754445,17.6542185206477,3.89878913289576));
#98693=CARTESIAN_POINT('Ctrl Pts',(-11.1072845034902,17.6543989458981,3.90127682044788));
#98694=CARTESIAN_POINT('Ctrl Pts',(-11.1053915689052,17.6547745568874,3.90646379529479));
#98695=CARTESIAN_POINT('Ctrl Pts',(-11.1043954877064,17.6549696446587,3.90916249151669));
#98696=CARTESIAN_POINT('Ctrl Pts',(-11.1019407322483,17.6554442902252,3.91573891956883));
#98697=CARTESIAN_POINT('Ctrl Pts',(-11.1004714467144,17.6557232282513,3.91961270583306));
#98698=CARTESIAN_POINT('Ctrl Pts',(-11.0951162488188,17.6567218789063,3.93351013249099));
#98699=CARTESIAN_POINT('Ctrl Pts',(-11.091113437866,17.6574350601812,3.94348857858813));
#98700=CARTESIAN_POINT('Ctrl Pts',(-11.0807799763132,17.6591993020098,3.96826125033395));
#98701=CARTESIAN_POINT('Ctrl Pts',(-11.0742815793299,17.6602420918645,3.98298353796955));
#98702=CARTESIAN_POINT('Ctrl Pts',(-11.0445176067774,17.6647594365688,4.04683911368431));
#98703=CARTESIAN_POINT('Ctrl Pts',(-11.0181665328738,17.6681160982642,4.09446437806296));
#98704=CARTESIAN_POINT('Ctrl Pts',(-10.9442595016032,17.6765221875922,4.20861150329932));
#98705=CARTESIAN_POINT('Ctrl Pts',(-10.8929064076063,17.681567221353,4.27231619189542));
#98706=CARTESIAN_POINT('Ctrl Pts',(-10.8247907581365,17.6878697503554,4.34085736850886));
#98707=CARTESIAN_POINT('Ctrl Pts',(-10.8139947267556,17.6888580315085,4.35131278638133));
#98708=CARTESIAN_POINT('Ctrl Pts',(-10.7981394080436,17.6902962289978,4.36609048736872));
#98709=CARTESIAN_POINT('Ctrl Pts',(-10.7932386358898,17.6907390010232,4.37058124863062));
#98710=CARTESIAN_POINT('Ctrl Pts',(-10.784547438861,17.6915213049355,4.37841100382307));
#98711=CARTESIAN_POINT('Ctrl Pts',(-10.7807730234685,17.6918600920117,4.38176757704264));
#98712=CARTESIAN_POINT('Ctrl Pts',(-10.772929690456,17.6925622162733,4.3886527795038));
#98713=CARTESIAN_POINT('Ctrl Pts',(-10.768857932976,17.692925683533,4.39217797895977));
#98714=CARTESIAN_POINT('Ctrl Pts',(-10.7583364824705,17.6938623481199,4.40116160239636));
#98715=CARTESIAN_POINT('Ctrl Pts',(-10.7518520618635,17.6944372036648,4.40657869204485));
#98716=CARTESIAN_POINT('Ctrl Pts',(-10.72395223163,17.6969008580603,4.42938102178373));
#98717=CARTESIAN_POINT('Ctrl Pts',(-10.7019894620115,17.6988164687031,4.44607953806297));
#98718=CARTESIAN_POINT('Ctrl Pts',(-10.5982105487315,17.7077686675846,4.51937948486913));
#98719=CARTESIAN_POINT('Ctrl Pts',(-10.5100227813261,17.7151484523054,4.56623694702003));
#98720=CARTESIAN_POINT('Ctrl Pts',(-10.3963578405525,17.724007235648,4.60927167305125));
#98721=CARTESIAN_POINT('Ctrl Pts',(-10.3754786773837,17.7256072038414,4.61651199678875));
#98722=CARTESIAN_POINT('Ctrl Pts',(-10.3335491836262,17.7287521575637,4.62974261753465));
#98723=CARTESIAN_POINT('Ctrl Pts',(-10.3125101311386,17.7302969606698,4.63574249173964));
#98724=CARTESIAN_POINT('Ctrl Pts',(-10.2859686582685,17.7321946402533,4.64251802201019));
#98725=CARTESIAN_POINT('Ctrl Pts',(-10.2806130525153,17.7325749763162,4.64384519139927));
#98726=CARTESIAN_POINT('Ctrl Pts',(-10.272130118479,17.7331731173264,4.64588417615998));
#98727=CARTESIAN_POINT('Ctrl Pts',(-10.2690089540329,17.733392279809,4.64662091810303));
#98728=CARTESIAN_POINT('Ctrl Pts',(-10.2634273508521,17.7337825307372,4.64791439426082));
#98729=CARTESIAN_POINT('Ctrl Pts',(-10.2609681454332,17.733953886483,4.64847596969939));
#98730=CARTESIAN_POINT('Ctrl Pts',(-10.2550618243977,17.7343640515367,4.64980476552377));
#98731=CARTESIAN_POINT('Ctrl Pts',(-10.2516130426483,17.7346024286095,4.65056438788727));
#98732=CARTESIAN_POINT('Ctrl Pts',(-10.2411029528239,17.7353256049204,4.65282980390785));
#98733=CARTESIAN_POINT('Ctrl Pts',(-10.2340310069864,17.7358077212436,4.65428622311128));
#98734=CARTESIAN_POINT('Ctrl Pts',(-10.1702020632865,17.7401224557555,4.66682061627781));
#98735=CARTESIAN_POINT('Ctrl Pts',(-10.1127061331978,17.7437503259744,4.67377097876649));
#98736=CARTESIAN_POINT('Ctrl Pts',(-9.9533067913942,17.7536548608026,4.68121276757545));
#98737=CARTESIAN_POINT('Ctrl Pts',(-9.85151409422792,17.7598479378296,4.67277182673046));
#98738=CARTESIAN_POINT('Ctrl Pts',(-9.7388927515219,17.7673812998558,4.64852073522732));
#98739=CARTESIAN_POINT('Ctrl Pts',(-9.72576130862969,17.7682696488174,4.64545623671794));
#98740=CARTESIAN_POINT('Ctrl Pts',(-9.70644438518839,17.7695925619886,4.6405970295336));
#98741=CARTESIAN_POINT('Ctrl Pts',(-9.70021605251052,17.7700216000187,4.63897588421517));
#98742=CARTESIAN_POINT('Ctrl Pts',(-9.68916894814907,17.7707871620305,4.63600359288551));
#98743=CARTESIAN_POINT('Ctrl Pts',(-9.6843448752707,17.7711230315515,4.63467261655085));
#98744=CARTESIAN_POINT('Ctrl Pts',(-9.67420446039413,17.7718324097526,4.63180517414995));
#98745=CARTESIAN_POINT('Ctrl Pts',(-9.66889018547529,17.7722061307756,4.63026190538948));
#98746=CARTESIAN_POINT('Ctrl Pts',(-9.654840429857,17.7731994673369,4.62607425762651));
#98747=CARTESIAN_POINT('Ctrl Pts',(-9.64612461963399,17.7738211443404,4.62336573276506));
#98748=CARTESIAN_POINT('Ctrl Pts',(-9.60427538744889,17.7768332120943,4.60982531482011));
#98749=CARTESIAN_POINT('Ctrl Pts',(-9.57160548376597,17.7792675951414,4.59762830670265));
#98750=CARTESIAN_POINT('Ctrl Pts',(-9.47746717023381,17.7865343204172,4.55763931968686));
#98751=CARTESIAN_POINT('Ctrl Pts',(-9.41779193248447,17.7914759972255,4.52599871519401));
#98752=CARTESIAN_POINT('Ctrl Pts',(-9.31029961705549,17.8008706988156,4.45659463956577));
#98753=CARTESIAN_POINT('Ctrl Pts',(-9.2620434936724,17.8053058647758,4.4198813094071));
#98754=CARTESIAN_POINT('Ctrl Pts',(-9.20952512712368,17.8102335552744,4.37312081382293));
#98755=CARTESIAN_POINT('Ctrl Pts',(-9.20231042653558,17.810912782223,4.36653438484952));
#98756=CARTESIAN_POINT('Ctrl Pts',(-9.19247559551547,17.8118408686077,4.35732905113829));
#98757=CARTESIAN_POINT('Ctrl Pts',(-9.189784864574,17.8120950157868,4.35478664064329));
#98758=CARTESIAN_POINT('Ctrl Pts',(-9.18519230823482,17.8125291230087,4.35040606945743));
#98759=CARTESIAN_POINT('Ctrl Pts',(-9.18328462643254,17.8127095427518,4.34857413138883));
#98760=CARTESIAN_POINT('Ctrl Pts',(-9.17931492594872,17.8130851526769,4.34473625890503));
#98761=CARTESIAN_POINT('Ctrl Pts',(-9.17725406525659,17.8132802448388,4.3427291765336));
#98762=CARTESIAN_POINT('Ctrl Pts',(-9.1722429370047,17.8137549180848,4.33781291120564));
#98763=CARTESIAN_POINT('Ctrl Pts',(-9.16930058981419,17.8140338792273,4.33489563463749));
#98764=CARTESIAN_POINT('Ctrl Pts',(-9.15877793866159,17.8150327061094,4.32435194331321));
#98765=CARTESIAN_POINT('Ctrl Pts',(-9.15128648566064,17.8157460374631,4.31663705141727));
#98766=CARTESIAN_POINT('Ctrl Pts',(-9.13284831473239,17.8175107258375,4.29712110728238));
#98767=CARTESIAN_POINT('Ctrl Pts',(-9.12203560278236,17.8185538067823,4.28519594756363));
#98768=CARTESIAN_POINT('Ctrl Pts',(-9.0757707842038,17.8230732291185,4.23202015213303));
#98769=CARTESIAN_POINT('Ctrl Pts',(-9.04295362409234,17.8264315670303,4.18856105035524));
#98770=CARTESIAN_POINT('Ctrl Pts',(-8.96871867297762,17.8348370694959,4.07463807381245));
#98771=CARTESIAN_POINT('Ctrl Pts',(-8.93140846709869,17.8398799100686,4.00185666486987));
#98772=CARTESIAN_POINT('Ctrl Pts',(-8.8964852328384,17.8461800275,3.91179618620671));
#98773=CARTESIAN_POINT('Ctrl Pts',(-8.89132043108675,17.8471683762383,3.89768143072672));
#98774=CARTESIAN_POINT('Ctrl Pts',(-8.88426296525698,17.8486066544528,3.8771871136755));
#98775=CARTESIAN_POINT('Ctrl Pts',(-8.88215190194974,17.8490494384809,3.87088391183506));
#98776=CARTESIAN_POINT('Ctrl Pts',(-8.87853082787826,17.8498317563965,3.85976029762559));
#98777=CARTESIAN_POINT('Ctrl Pts',(-8.87699824556304,17.8501705453894,3.85494736784152));
#98778=CARTESIAN_POINT('Ctrl Pts',(-8.87389561863522,17.850872666582,3.84498259434082));
#98779=CARTESIAN_POINT('Ctrl Pts',(-8.8723298606941,17.8512361288131,3.83982955047714));
#98780=CARTESIAN_POINT('Ctrl Pts',(-8.86839867114451,17.8521727654874,3.82656527856838));
#98781=CARTESIAN_POINT('Ctrl Pts',(-8.86608511506236,17.8527475979576,3.81843912427729));
#98782=CARTESIAN_POINT('Ctrl Pts',(-8.85659292161595,17.8552110122498,3.78368291579778));
#98783=CARTESIAN_POINT('Ctrl Pts',(-8.85026399791373,17.8571263993441,3.75683194695721));
#98784=CARTESIAN_POINT('Ctrl Pts',(-8.82547504892722,17.8660785086723,3.63221953184762));
#98785=CARTESIAN_POINT('Ctrl Pts',(-8.81850841326093,17.8734584621393,3.53259700562935));
#98786=CARTESIAN_POINT('Ctrl Pts',(-8.82539079220619,17.8823174045946,3.41125103427278));
#98787=CARTESIAN_POINT('Ctrl Pts',(-8.82726231850258,17.8839173545011,3.3892318002248));
#98788=CARTESIAN_POINT('Ctrl Pts',(-8.83221722202826,17.8870624035309,3.34554324231802));
#98789=CARTESIAN_POINT('Ctrl Pts',(-8.83528736489175,17.8886073169667,3.32388034180067));
#98790=CARTESIAN_POINT('Ctrl Pts',(-8.83988551679018,17.8905051119292,3.29687469043616));
#98791=CARTESIAN_POINT('Ctrl Pts',(-8.84084987028902,17.8908854569161,3.29144188980268));
#98792=CARTESIAN_POINT('Ctrl Pts',(-8.84243505093976,17.8914836088178,3.28286240433153));
#98793=CARTESIAN_POINT('Ctrl Pts',(-8.84303059665384,17.8917027733479,3.27971121887302));
#98794=CARTESIAN_POINT('Ctrl Pts',(-8.84411758018409,17.8920930260063,3.27408573027796));
#98795=CARTESIAN_POINT('Ctrl Pts',(-8.84460409318003,17.8922643814498,3.27161058608846));
#98796=CARTESIAN_POINT('Ctrl Pts',(-8.8457907818495,17.8926745433203,3.26567412964432));
#98797=CARTESIAN_POINT('Ctrl Pts',(-8.8464985764386,17.8929129175318,3.26221438344126));
#98798=CARTESIAN_POINT('Ctrl Pts',(-8.84859499979282,17.8936013404536,3.25219660451945));
#98799=CARTESIAN_POINT('Ctrl Pts',(-8.85002409727888,17.8940491928382,3.24564704510706));
#98800=CARTESIAN_POINT('Ctrl Pts',(-8.85350442342808,17.8950923553245,3.23032594889763));
#98801=CARTESIAN_POINT('Ctrl Pts',(-8.85560054263727,17.8956854080969,3.22156491954854));
#98802=CARTESIAN_POINT('Ctrl Pts',(-8.86307390784598,17.8976884382318,3.19184017313714));
#98803=CARTESIAN_POINT('Ctrl Pts',(-8.86892860749372,17.8990773229491,3.17099993999344));
#98804=CARTESIAN_POINT('Ctrl Pts',(-8.90182298871254,17.9061035945119,3.06520107757154));
#98805=CARTESIAN_POINT('Ctrl Pts',(-8.93787215315909,17.9114785743262,2.98334822380961));
#98806=CARTESIAN_POINT('Ctrl Pts',(-9.00576424095308,17.9199490216924,2.86702028851143));
#98807=CARTESIAN_POINT('Ctrl Pts',(-9.03097260801836,17.9228610952238,2.8290654022077));
#98808=CARTESIAN_POINT('Ctrl Pts',(-9.06439584052988,17.9265223527975,2.78456829284754));
#98809=CARTESIAN_POINT('Ctrl Pts',(-9.07058353047192,17.9271926022561,2.77654807592051));
#98810=CARTESIAN_POINT('Ctrl Pts',(-9.08048340227842,17.9282538131056,2.76405293998726));
#98811=CARTESIAN_POINT('Ctrl Pts',(-9.08412667999263,17.9286420576485,2.75952386380646));
#98812=CARTESIAN_POINT('Ctrl Pts',(-9.09091672521467,17.9293615443689,2.75120971618725));
#98813=CARTESIAN_POINT('Ctrl Pts',(-9.09405399762396,17.9296924013955,2.74741702840094));
#98814=CARTESIAN_POINT('Ctrl Pts',(-9.10107033368193,17.9304289446411,2.7390423411306));
#98815=CARTESIAN_POINT('Ctrl Pts',(-9.10496082191933,17.9308350889041,2.73447013711857));
#98816=CARTESIAN_POINT('Ctrl Pts',(-9.11578866546422,17.9319594032683,2.72194034514354));
#98817=CARTESIAN_POINT('Ctrl Pts',(-9.12279817762902,17.9326805223891,2.71404614586901));
#98818=CARTESIAN_POINT('Ctrl Pts',(-9.16898357371708,17.9373902989777,2.66341912299944));
#98819=CARTESIAN_POINT('Ctrl Pts',(-9.21115707305582,17.9415062888095,2.62354074563825));
#98820=CARTESIAN_POINT('Ctrl Pts',(-9.29204882337571,17.9490735359289,2.55763502943807));
#98821=CARTESIAN_POINT('Ctrl Pts',(-9.32970741111362,17.9524854535245,2.53048768757376));
#98822=CARTESIAN_POINT('Ctrl Pts',(-9.38108647417725,17.9569508411352,2.49787696078741));
#98823=CARTESIAN_POINT('Ctrl Pts',(-9.39344825642823,17.9580114744876,2.49034682639707));
#98824=CARTESIAN_POINT('Ctrl Pts',(-9.44544108949558,17.962408853302,2.45997517699205));
#98825=CARTESIAN_POINT('Ctrl Pts',(-9.4862517765319,17.9657108637688,2.43922152601819));
#98826=CARTESIAN_POINT('Ctrl Pts',(-9.53367794368512,17.9693085644532,2.41848489187108));
#98827=CARTESIAN_POINT('Ctrl Pts',(-9.53920358429843,17.9697241522026,2.41611907647317));
#98828=CARTESIAN_POINT('Ctrl Pts',(-9.54807424663757,17.9703853352421,2.41240118179785));
#98829=CARTESIAN_POINT('Ctrl Pts',(-9.55140770064966,17.9706324541602,2.41102202696952));
#98830=CARTESIAN_POINT('Ctrl Pts',(-9.55734108396712,17.9710698652058,2.40859906771301));
#98831=CARTESIAN_POINT('Ctrl Pts',(-9.55993846353534,17.9712605123008,2.40754919758599));
#98832=CARTESIAN_POINT('Ctrl Pts',(-9.56552813381234,17.9716689912033,2.40531300345106));
#98833=CARTESIAN_POINT('Ctrl Pts',(-9.56852155208188,17.9718866456502,2.40412967348693));
#98834=CARTESIAN_POINT('Ctrl Pts',(-9.57469601672108,17.9723334163409,2.40171806377634));
#98835=CARTESIAN_POINT('Ctrl Pts',(-9.57787762527539,17.97256244407,2.40049129557978));
#98836=CARTESIAN_POINT('Ctrl Pts',(-9.58600203777539,17.9731443690959,2.39739913848184));
#98837=CARTESIAN_POINT('Ctrl Pts',(-9.59095220804869,17.973496198362,2.39555313440607));
#98838=CARTESIAN_POINT('Ctrl Pts',(-9.60537548972847,17.9745138564587,2.3902847183569));
#98839=CARTESIAN_POINT('Ctrl Pts',(-9.61488053377607,17.975175189514,2.38695035048637));
#98840=CARTESIAN_POINT('Ctrl Pts',(-9.68538147067543,17.9800201456953,2.36322991948091));
#98841=CARTESIAN_POINT('Ctrl Pts',(-9.74786249841613,17.9839825748715,2.34776563038784));
#98842=CARTESIAN_POINT('Ctrl Pts',(-9.8111044001022,17.9879475322356,2.33749687418206));
#98843=CARTESIAN_POINT('Origin',(-10.,12.3756328852638,3.5));
#98844=CARTESIAN_POINT('',(-9.81110405347124,18.5858217457338,2.33749693166641));
#98845=CARTESIAN_POINT('',(-9.81110406374122,18.4867244625755,2.33749692999764));
#98846=CARTESIAN_POINT('',(-9.81110406371068,12.3756328852638,2.3374969300026));
#98847=CARTESIAN_POINT('Ctrl Pts',(-9.81110405343086,18.5858217463839,2.33749693167298));
#98848=CARTESIAN_POINT('Ctrl Pts',(-9.77349069906134,18.5834242261466,2.34360875225294));
#98849=CARTESIAN_POINT('Ctrl Pts',(-9.7361844295136,18.5810690906263,2.35154437023802));
#98850=CARTESIAN_POINT('Ctrl Pts',(-9.62087119967049,18.5736965981962,2.38199314469751));
#98851=CARTESIAN_POINT('Ctrl Pts',(-9.54478514597519,18.5686794602283,2.4107547070466));
#98852=CARTESIAN_POINT('Ctrl Pts',(-9.45881495506879,18.5624075265073,2.45384509380604));
#98853=CARTESIAN_POINT('Ctrl Pts',(-9.44549798619964,18.5614183188787,2.46084225270244));
#98854=CARTESIAN_POINT('Ctrl Pts',(-9.42649175251835,18.5599789256052,2.47129810515121));
#98855=CARTESIAN_POINT('Ctrl Pts',(-9.42069171163097,18.5595358991813,2.4745531694088));
#98856=CARTESIAN_POINT('Ctrl Pts',(-9.41053423289537,18.5587532066141,2.48036736758082));
#98857=CARTESIAN_POINT('Ctrl Pts',(-9.40616507516968,18.5584142865199,2.48290576819474));
#98858=CARTESIAN_POINT('Ctrl Pts',(-9.39717200900019,18.5577119450416,2.48820827456011));
#98859=CARTESIAN_POINT('Ctrl Pts',(-9.39255046766301,18.5573483938563,2.4909761418101));
#98860=CARTESIAN_POINT('Ctrl Pts',(-9.38072919374689,18.5564116345727,2.49816661790188));
#98861=CARTESIAN_POINT('Ctrl Pts',(-9.37355787603209,18.5558367686888,2.5026351140126));
#98862=CARTESIAN_POINT('Ctrl Pts',(-9.34319591591982,18.553374152951,2.52201049734209));
#98863=CARTESIAN_POINT('Ctrl Pts',(-9.32048612237669,18.5514596243354,2.53765092485362));
#98864=CARTESIAN_POINT('Ctrl Pts',(-9.21841478256243,18.5425053478852,2.61336351157382));
#98865=CARTESIAN_POINT('Ctrl Pts',(-9.14632789295126,18.5351219527637,2.68254192197185));
#98866=CARTESIAN_POINT('Ctrl Pts',(-9.06992351555006,18.5262594861745,2.77712990426883));
#98867=CARTESIAN_POINT('Ctrl Pts',(-9.0565229215821,18.5246591362309,2.79470960687341));
#98868=CARTESIAN_POINT('Ctrl Pts',(-9.03087925388811,18.5215162768187,2.83039044013339));
#98869=CARTESIAN_POINT('Ctrl Pts',(-9.01862882180434,18.5199738789571,2.84847659825261));
#98870=CARTESIAN_POINT('Ctrl Pts',(-9.00392254386255,18.5180786316875,2.87154539729453));
#98871=CARTESIAN_POINT('Ctrl Pts',(-9.00099014621973,18.517698408893,2.8762173444752));
#98872=CARTESIAN_POINT('Ctrl Pts',(-8.99640474476985,18.5171003607988,2.88363816463041));
#98873=CARTESIAN_POINT('Ctrl Pts',(-8.99473000714997,18.5168811792587,2.88637341116916));
#98874=CARTESIAN_POINT('Ctrl Pts',(-8.99175749543623,18.5164908404813,2.89127306378117));
#98875=CARTESIAN_POINT('Ctrl Pts',(-8.99045551103913,18.5163194161871,2.89343478843961));
#98876=CARTESIAN_POINT('Ctrl Pts',(-8.98734691054794,18.5159090125939,2.89863382916381));
#98877=CARTESIAN_POINT('Ctrl Pts',(-8.98554700613022,18.5156704664211,2.90167510911526));
#98878=CARTESIAN_POINT('Ctrl Pts',(-8.98010690339994,18.514946507767,2.9109623142101));
#98879=CARTESIAN_POINT('Ctrl Pts',(-8.97651041520775,18.5144637858156,2.91723383756804));
#98880=CARTESIAN_POINT('Ctrl Pts',(-8.9445371821246,18.5101308988543,2.97419757116948));
#98881=CARTESIAN_POINT('Ctrl Pts',(-8.91988556476199,18.5064873508038,3.02689887745853));
#98882=CARTESIAN_POINT('Ctrl Pts',(-8.86317525076844,18.4965894708289,3.17596077799349));
#98883=CARTESIAN_POINT('Ctrl Pts',(-8.8395151258666,18.4904163347123,3.27495614680011));
#98884=CARTESIAN_POINT('Ctrl Pts',(-8.82739449149161,18.4829037185242,3.38920989543255));
#98885=CARTESIAN_POINT('Ctrl Pts',(-8.82619916515082,18.4820123692791,3.40268760951448));
#98886=CARTESIAN_POINT('Ctrl Pts',(-8.82477758381623,18.4806857483324,3.42261211001609));
#98887=CARTESIAN_POINT('Ctrl Pts',(-8.82437164111217,18.4802560467876,3.42904528197074));
#98888=CARTESIAN_POINT('Ctrl Pts',(-8.82374424334731,18.4794896421377,3.4404808623872));
#98889=CARTESIAN_POINT('Ctrl Pts',(-8.82350184057688,18.4791535975777,3.44548199978562));
#98890=CARTESIAN_POINT('Ctrl Pts',(-8.82305877653664,18.4784442001713,3.45601116599528));
#98891=CARTESIAN_POINT('Ctrl Pts',(-8.8228651573261,18.4780706370321,3.46153935310707));
#98892=CARTESIAN_POINT('Ctrl Pts',(-8.82245573312975,18.4770785385819,3.47617617633316));
#98893=CARTESIAN_POINT('Ctrl Pts',(-8.82230667421296,18.4764579521033,3.48528615340469));
#98894=CARTESIAN_POINT('Ctrl Pts',(-8.82209851591881,18.4734619151482,3.52903835825502));
#98895=CARTESIAN_POINT('Ctrl Pts',(-8.82346218795207,18.4710430475044,3.56366694571281));
#98896=CARTESIAN_POINT('Ctrl Pts',(-8.83190686207788,18.4638476852932,3.66461288195093));
#98897=CARTESIAN_POINT('Ctrl Pts',(-8.84309368939802,18.4589646196837,3.73044504756727));
#98898=CARTESIAN_POINT('Ctrl Pts',(-8.87520753911197,18.4495493809486,3.8545820564606));
#98899=CARTESIAN_POINT('Ctrl Pts',(-8.89528188888828,18.4450352990063,3.91289945239814));
#98900=CARTESIAN_POINT('Ctrl Pts',(-8.92371248718268,18.4400364945684,3.978325511078));
#98901=CARTESIAN_POINT('Ctrl Pts',(-8.92770889949343,18.439358623463,3.98721855059252));
#98902=CARTESIAN_POINT('Ctrl Pts',(-8.93337393436904,18.4384319825849,3.99941725037453));
#98903=CARTESIAN_POINT('Ctrl Pts',(-8.93494826274736,18.4381779481164,4.00276590154947));
#98904=CARTESIAN_POINT('Ctrl Pts',(-8.93767497344222,18.4377439443733,4.00849542400908));
#98905=CARTESIAN_POINT('Ctrl Pts',(-8.93881963009903,18.4375635162429,4.01087990876534));
#98906=CARTESIAN_POINT('Ctrl Pts',(-8.94122671705154,18.4371877847573,4.01585122168124));
#98907=CARTESIAN_POINT('Ctrl Pts',(-8.94249060989853,18.436992580019,4.01843730352217));
#98908=CARTESIAN_POINT('Ctrl Pts',(-8.94559915049485,18.4365174570555,4.02473909697768));
#98909=CARTESIAN_POINT('Ctrl Pts',(-8.94745399709511,18.4362381609824,4.0284497936474));
#98910=CARTESIAN_POINT('Ctrl Pts',(-8.95419943843827,18.4352371573774,4.04176790742874));
#98911=CARTESIAN_POINT('Ctrl Pts',(-8.95920246102509,18.4345220202518,4.05131822329618));
#98912=CARTESIAN_POINT('Ctrl Pts',(-8.97202574889643,18.4327520512792,4.07499982415109));
#98913=CARTESIAN_POINT('Ctrl Pts',(-8.98000704092764,18.4317055576298,4.08904182919863));
#98914=CARTESIAN_POINT('Ctrl Pts',(-9.01628554696298,18.4271621727846,4.14991908915369));
#98915=CARTESIAN_POINT('Ctrl Pts',(-9.04753984874897,18.423784547491,4.19491694290226));
#98916=CARTESIAN_POINT('Ctrl Pts',(-9.13262463226795,18.4153861872425,4.30083586801072));
#98917=CARTESIAN_POINT('Ctrl Pts',(-9.18983058547563,18.4103689991484,4.35866264131626));
#98918=CARTESIAN_POINT('Ctrl Pts',(-9.26414599516599,18.404097010245,4.41969572333441));
#98919=CARTESIAN_POINT('Ctrl Pts',(-9.27595202709852,18.4031078040363,4.42901875080838));
#98920=CARTESIAN_POINT('Ctrl Pts',(-9.29323067446997,18.4016684124586,4.44213397074598));
#98921=CARTESIAN_POINT('Ctrl Pts',(-9.29856226968893,18.4012253862869,4.44611014463828));
#98922=CARTESIAN_POINT('Ctrl Pts',(-9.30800323592951,18.4004426940138,4.45302732080032));
#98923=CARTESIAN_POINT('Ctrl Pts',(-9.31209842758786,18.4001037739599,4.45598745859254));
#98924=CARTESIAN_POINT('Ctrl Pts',(-9.32059858058123,18.3994014324172,4.46204874809421));
#98925=CARTESIAN_POINT('Ctrl Pts',(-9.32500601650267,18.3990378811265,4.4651462080906));
#98926=CARTESIAN_POINT('Ctrl Pts',(-9.33638073686876,18.3981011212575,4.47302411618781));
#98927=CARTESIAN_POINT('Ctrl Pts',(-9.34337839692143,18.3975262548897,4.47775995058654));
#98928=CARTESIAN_POINT('Ctrl Pts',(-9.37342237787305,18.3950636341199,4.49762495922158));
#98929=CARTESIAN_POINT('Ctrl Pts',(-9.39694345623799,18.3931491008196,4.51201663078266));
#98930=CARTESIAN_POINT('Ctrl Pts',(-9.50760861202896,18.3841948224945,4.57450008185539));
#98931=CARTESIAN_POINT('Ctrl Pts',(-9.60011575229865,18.3768114309115,4.61224383759791));
#98932=CARTESIAN_POINT('Ctrl Pts',(-9.71759360527407,18.3679489676577,4.643603983339));
#98933=CARTESIAN_POINT('Ctrl Pts',(-9.73910252040602,18.3663486173295,4.64870189411356));
#98934=CARTESIAN_POINT('Ctrl Pts',(-9.78212622001024,18.3632057599128,4.65762817770039));
#98935=CARTESIAN_POINT('Ctrl Pts',(-9.80363031521089,18.3616633643626,4.66146936159186));
#98936=CARTESIAN_POINT('Ctrl Pts',(-9.83068509652546,18.3597681195106,4.66552904284654));
#98937=CARTESIAN_POINT('Ctrl Pts',(-9.83614562005127,18.3593878969035,4.66630923490543));
#98938=CARTESIAN_POINT('Ctrl Pts',(-9.8447895880421,18.358789849038,4.66748236664908));
#98939=CARTESIAN_POINT('Ctrl Pts',(-9.84796941679787,18.3585706675409,4.66790070246239));
#98940=CARTESIAN_POINT('Ctrl Pts',(-9.85365429363106,18.3581803287998,4.66862498908559));
#98941=CARTESIAN_POINT('Ctrl Pts',(-9.85615860318361,18.3580089044992,4.66893587661128));
#98942=CARTESIAN_POINT('Ctrl Pts',(-9.86217233772733,18.357598500839,4.66966280889915));
#98943=CARTESIAN_POINT('Ctrl Pts',(-9.86568265624522,18.3573599546059,4.67007111023077));
#98944=CARTESIAN_POINT('Ctrl Pts',(-9.87637929249081,18.3566359955851,4.67126651301685));
#98945=CARTESIAN_POINT('Ctrl Pts',(-9.88357123128922,18.3561532733312,4.67200327309138));
#98946=CARTESIAN_POINT('Ctrl Pts',(-9.9486133073264,18.3518203754249,4.67806170493588));
#98947=CARTESIAN_POINT('Ctrl Pts',(-10.0067849110766,18.3481768178725,4.67916319866799));
#98948=CARTESIAN_POINT('Ctrl Pts',(-10.1660283667076,18.3382789416503,4.67038731481509));
#98949=CARTESIAN_POINT('Ctrl Pts',(-10.2660937083242,18.332105817369,4.65176559017269));
#98950=CARTESIAN_POINT('Ctrl Pts',(-10.3754095839702,18.3245932135332,4.61639857167634));
#98951=CARTESIAN_POINT('Ctrl Pts',(-10.3882095555246,18.3237018625563,4.61201233939074));
#98952=CARTESIAN_POINT('Ctrl Pts',(-10.4069916827563,18.3223752395198,4.60521237020294));
#98953=CARTESIAN_POINT('Ctrl Pts',(-10.4130344381835,18.3219455376426,4.60296834187195));
#98954=CARTESIAN_POINT('Ctrl Pts',(-10.4237377209317,18.3211791326198,4.59889329630616));
#98955=CARTESIAN_POINT('Ctrl Pts',(-10.4284056016692,18.3208430880215,4.59708193492466));
#98956=CARTESIAN_POINT('Ctrl Pts',(-10.4382057939142,18.3201336907602,4.59320690775121));
#98957=CARTESIAN_POINT('Ctrl Pts',(-10.4433353876533,18.3197601278059,4.59113674359405));
#98958=CARTESIAN_POINT('Ctrl Pts',(-10.4568749047888,18.3187680303765,4.58556132768491));
#98959=CARTESIAN_POINT('Ctrl Pts',(-10.4652589228806,18.3181474447412,4.5819945477417));
#98960=CARTESIAN_POINT('Ctrl Pts',(-10.5053181178984,18.315151418866,4.56440063974568));
#98961=CARTESIAN_POINT('Ctrl Pts',(-10.5364025171527,18.3127325618501,4.54907913546556));
#98962=CARTESIAN_POINT('Ctrl Pts',(-10.6251998831324,18.3055372479804,4.50033195345198));
#98963=CARTESIAN_POINT('Ctrl Pts',(-10.6808006826714,18.3006542219303,4.46335221656612));
#98964=CARTESIAN_POINT('Ctrl Pts',(-10.7811667688113,18.2912389701846,4.383552533237));
#98965=CARTESIAN_POINT('Ctrl Pts',(-10.8262899906076,18.2867248357184,4.34150638684894));
#98966=CARTESIAN_POINT('Ctrl Pts',(-10.8745114468342,18.2817259830588,4.28893588721454));
#98967=CARTESIAN_POINT('Ctrl Pts',(-10.8810122389433,18.2810481120097,4.2816697225066));
#98968=CARTESIAN_POINT('Ctrl Pts',(-10.8898550346527,18.280121471194,4.27153533370644));
#98969=CARTESIAN_POINT('Ctrl Pts',(-10.8922746455954,18.2798674367325,4.26873578790931));
#98970=CARTESIAN_POINT('Ctrl Pts',(-10.8964011541252,18.2794334329983,4.2639155903449));
#98971=CARTESIAN_POINT('Ctrl Pts',(-10.8981144934879,18.2792530048699,4.26190052843531));
#98972=CARTESIAN_POINT('Ctrl Pts',(-10.901678173742,18.2788772733847,4.25768055181123));
#98973=CARTESIAN_POINT('Ctrl Pts',(-10.9035272382599,18.2786820686448,4.25547460417849));
#98974=CARTESIAN_POINT('Ctrl Pts',(-10.9080214050979,18.2782069456717,4.25007292926693));
#98975=CARTESIAN_POINT('Ctrl Pts',(-10.9106577798778,18.2779276495906,4.24686992213238));
#98976=CARTESIAN_POINT('Ctrl Pts',(-10.9200841850464,18.2769266459247,4.23529339214173));
#98977=CARTESIAN_POINT('Ctrl Pts',(-10.9267763451115,18.2762115087471,4.22684035842382));
#98978=CARTESIAN_POINT('Ctrl Pts',(-10.9432009857217,18.2744415396198,4.20549823478958));
#98979=CARTESIAN_POINT('Ctrl Pts',(-10.9527864412493,18.2733950458695,4.19249831084729));
#98980=CARTESIAN_POINT('Ctrl Pts',(-10.9936613983756,18.2688516603005,4.13460694451443));
#98981=CARTESIAN_POINT('Ctrl Pts',(-11.0220701539553,18.2654740344227,4.08776057943285));
#98982=CARTESIAN_POINT('Ctrl Pts',(-11.0842594467699,18.2570756743738,3.96696848501761));
#98983=CARTESIAN_POINT('Ctrl Pts',(-11.1138408013418,18.2520584870412,3.89119647104517));
#98984=CARTESIAN_POINT('Ctrl Pts',(-11.139397081249,18.2457864989762,3.79848891302892));
#98985=CARTESIAN_POINT('Ctrl Pts',(-11.1431163254308,18.2447972927459,3.78391261500665));
#98986=CARTESIAN_POINT('Ctrl Pts',(-11.148075872683,18.2433579011425,3.76279476575378));
#98987=CARTESIAN_POINT('Ctrl Pts',(-11.1495415937594,18.2429148749669,3.75630727556835));
#98988=CARTESIAN_POINT('Ctrl Pts',(-11.1520240419837,18.2421321826893,3.74486976613582));
#98989=CARTESIAN_POINT('Ctrl Pts',(-11.1530640160851,18.2417932626348,3.73992492393071));
#98990=CARTESIAN_POINT('Ctrl Pts',(-11.1551468898333,18.2410909210932,3.72969489616916));
#98991=CARTESIAN_POINT('Ctrl Pts',(-11.1561854106457,18.240727369804,3.72440895026488));
#98992=CARTESIAN_POINT('Ctrl Pts',(-11.1587596211645,18.239790609944,3.71081413007415));
#98993=CARTESIAN_POINT('Ctrl Pts',(-11.1602422021113,18.2392157435835,3.70249563708554));
#98994=CARTESIAN_POINT('Ctrl Pts',(-11.1661799907445,18.2367531228901,3.66697097036281));
#98995=CARTESIAN_POINT('Ctrl Pts',(-11.1697683934133,18.234838589661,3.63963080487817));
#98996=CARTESIAN_POINT('Ctrl Pts',(-11.1818745745313,18.2258843113643,3.51312231235816));
#98997=CARTESIAN_POINT('Ctrl Pts',(-11.1787578069356,18.2185009197276,3.41326016732601));
#98998=CARTESIAN_POINT('Ctrl Pts',(-11.1596586156403,18.2096384564231,3.29317800489739));
#98999=CARTESIAN_POINT('Ctrl Pts',(-11.1555735550435,18.2080381061008,3.2714539537016));
#99000=CARTESIAN_POINT('Ctrl Pts',(-11.1462411193192,18.2048952486538,3.22851652312526));
#99001=CARTESIAN_POINT('Ctrl Pts',(-11.1410097940751,18.2033528530685,3.20730770275499));
#99002=CARTESIAN_POINT('Ctrl Pts',(-11.1337218884577,18.2014576081798,3.18093861736378));
#99003=CARTESIAN_POINT('Ctrl Pts',(-11.1322151560517,18.2010773855698,3.17563241582836));
#99004=CARTESIAN_POINT('Ctrl Pts',(-11.1297734483135,18.2004793377008,3.16725790181794));
#99005=CARTESIAN_POINT('Ctrl Pts',(-11.128863146155,18.2002601562031,3.16418256999684));
#99006=CARTESIAN_POINT('Ctrl Pts',(-11.1272141411536,18.1998698174614,3.15869410952744));
#99007=CARTESIAN_POINT('Ctrl Pts',(-11.1264802489925,18.1996983931609,3.15627964899235));
#99008=CARTESIAN_POINT('Ctrl Pts',(-11.124699988925,18.1992879895017,3.15048964833436));
#99009=CARTESIAN_POINT('Ctrl Pts',(-11.1236461829439,18.1990494432695,3.14711643933805));
#99010=CARTESIAN_POINT('Ctrl Pts',(-11.1203904658806,18.1983254842543,3.13685742771944));
#99011=CARTESIAN_POINT('Ctrl Pts',(-11.1181402749674,18.1978427620049,3.12998695183104));
#99012=CARTESIAN_POINT('Ctrl Pts',(-11.0972376812962,18.1935098642643,3.06809787766158));
#99013=CARTESIAN_POINT('Ctrl Pts',(-11.0745987943013,18.1898663068556,3.01450096280877));
#99014=CARTESIAN_POINT('Ctrl Pts',(-11.0018524116027,18.1799684623845,2.87257388695619));
#99015=CARTESIAN_POINT('Ctrl Pts',(-10.9441647722163,18.1737953689029,2.7887176256973));
#99016=CARTESIAN_POINT('Ctrl Pts',(-10.8676030367396,18.1663009555454,2.70342253248312));
#99017=CARTESIAN_POINT('Ctrl Pts',(-10.8585850920111,18.1654280277789,2.69371077908075));
#99018=CARTESIAN_POINT('Ctrl Pts',(-10.844920008003,18.1641183259595,2.67948359509731));
#99019=CARTESIAN_POINT('Ctrl Pts',(-10.8403961773091,18.1636868101745,2.67485076926536));
#99020=CARTESIAN_POINT('Ctrl Pts',(-10.8323811372201,18.1629257230905,2.66677690183126));
#99021=CARTESIAN_POINT('Ctrl Pts',(-10.828906187939,18.1625968657817,2.66331988234828));
#99022=CARTESIAN_POINT('Ctrl Pts',(-10.8248741445703,18.1622165279818,2.65935841643118));
#99023=CARTESIAN_POINT('Ctrl Pts',(-10.824337982709,18.1621659775889,2.65883264645829));
#99024=CARTESIAN_POINT('Ctrl Pts',(-10.8236532523797,18.1621014517422,2.65816247097802));
#99025=CARTESIAN_POINT('Ctrl Pts',(-10.8235051471627,18.1620874968855,2.65801759043194));
#99026=CARTESIAN_POINT('Ctrl Pts',(-10.8232307964716,18.162061650367,2.65774935476712));
#99027=CARTESIAN_POINT('Ctrl Pts',(-10.8231045614585,18.1620497591706,2.65762598890958));
#99028=CARTESIAN_POINT('Ctrl Pts',(-10.8228696205998,18.162027630564,2.65739649118053));
#99029=CARTESIAN_POINT('Ctrl Pts',(-10.822760921931,18.1620173934736,2.65729035194553));
#99030=CARTESIAN_POINT('Ctrl Pts',(-10.8225578200812,18.1619982675225,2.65709210911373));
#99031=CARTESIAN_POINT('Ctrl Pts',(-10.8224634219369,18.1619893788856,2.65700000031386));
#99032=CARTESIAN_POINT('Ctrl Pts',(-10.8222864501071,18.161972716452,2.65682737842656));
#99033=CARTESIAN_POINT('Ctrl Pts',(-10.8222038800531,18.1619649428169,2.65674686159711));
#99034=CARTESIAN_POINT('Ctrl Pts',(-10.8220486389495,18.1619503285976,2.65659552526808));
#99035=CARTESIAN_POINT('Ctrl Pts',(-10.8219759705755,18.1619434881331,2.65652470303336));
#99036=CARTESIAN_POINT('Ctrl Pts',(-10.8218390072068,18.1619305962652,2.65639125372634));
#99037=CARTESIAN_POINT('Ctrl Pts',(-10.8217747141986,18.1619245449502,2.65632862460561));
#99038=CARTESIAN_POINT('Ctrl Pts',(-10.8216532749907,18.1619131156524,2.65621035526707));
#99039=CARTESIAN_POINT('Ctrl Pts',(-10.8215961303019,18.1619077377374,2.65615471350822));
#99040=CARTESIAN_POINT('Ctrl Pts',(-10.8214879890023,18.1618975610344,2.65604943776952));
#99041=CARTESIAN_POINT('Ctrl Pts',(-10.8214369935417,18.1618927622977,2.65599980260345));
#99042=CARTESIAN_POINT('Ctrl Pts',(-10.8213403283009,18.1618836663986,2.65590573294998));
#99043=CARTESIAN_POINT('Ctrl Pts',(-10.821294659397,18.1618793692745,2.65586129753099));
#99044=CARTESIAN_POINT('Ctrl Pts',(-10.8212079631434,18.1618712121021,2.65577695657751));
#99045=CARTESIAN_POINT('Ctrl Pts',(-10.8211669365161,18.1618673520873,2.65573705035193));
#99046=CARTESIAN_POINT('Ctrl Pts',(-10.8210434380328,18.1618557330906,2.65561694202383));
#99047=CARTESIAN_POINT('Ctrl Pts',(-10.8209609573237,18.1618479737121,2.65553674900314));
#99048=CARTESIAN_POINT('Ctrl Pts',(-10.8207975547961,18.1618326027557,2.6553779251808));
#99049=CARTESIAN_POINT('Ctrl Pts',(-10.8207166334206,18.1618249911975,2.65529929391654));
#99050=CARTESIAN_POINT('Ctrl Pts',(-10.8205562114074,18.1618099028211,2.65514345673258));
#99051=CARTESIAN_POINT('Ctrl Pts',(-10.8204767111811,18.1618024260221,2.65506625041332));
#99052=CARTESIAN_POINT('Ctrl Pts',(-10.8203190029885,18.1617875950225,2.65491313599457));
#99053=CARTESIAN_POINT('Ctrl Pts',(-10.8202407953796,18.161780240838,2.6548372275274));
#99054=CARTESIAN_POINT('Ctrl Pts',(-10.8200855525007,18.1617656437385,2.65468659031199));
#99055=CARTESIAN_POINT('Ctrl Pts',(-10.8200085175446,18.1617584008372,2.65461186122991));
#99056=CARTESIAN_POINT('Ctrl Pts',(-10.8153393870804,18.1613194351235,2.65008372970618));
#99057=CARTESIAN_POINT('Ctrl Pts',(-10.8107111758715,18.1608861007471,2.64566788123927));
#99058=CARTESIAN_POINT('Ctrl Pts',(-10.8009513909169,18.159975889463,2.63650664103468));
#99059=CARTESIAN_POINT('Ctrl Pts',(-10.7958131018888,18.1594987157767,2.63176880107858));
#99060=CARTESIAN_POINT('Ctrl Pts',(-10.7820523440761,18.15822599902,2.61930526121784));
#99061=CARTESIAN_POINT('Ctrl Pts',(-10.7733577941701,18.1574271648611,2.61166065185665));
#99062=CARTESIAN_POINT('Ctrl Pts',(-10.7000334764934,18.1507325484699,2.54908321115328));
#99063=CARTESIAN_POINT('Ctrl Pts',(-10.6297663587169,18.1445588070023,2.50116118129535));
#99064=CARTESIAN_POINT('Ctrl Pts',(-10.4970964304385,18.1335136388542,2.4302818706869));
#99065=CARTESIAN_POINT('Ctrl Pts',(-10.4367247341494,18.1286902129682,2.40424686192557));
#99066=CARTESIAN_POINT('Ctrl Pts',(-10.3652761292401,18.1234097713586,2.38028444595804));
#99067=CARTESIAN_POINT('Ctrl Pts',(-10.3560207567468,18.1227338289047,2.37730734006603));
#99068=CARTESIAN_POINT('Ctrl Pts',(-10.3431963543221,18.1218093283671,2.37335675993764));
#99069=CARTESIAN_POINT('Ctrl Pts',(-10.3396583306219,18.1215555375603,2.37228507708487));
#99070=CARTESIAN_POINT('Ctrl Pts',(-10.3335811907528,18.1211218412123,2.37047547943243));
#99071=CARTESIAN_POINT('Ctrl Pts',(-10.3310445555221,18.1209414782147,2.36972943239224));
#99072=CARTESIAN_POINT('Ctrl Pts',(-10.3257404762789,18.120565758728,2.36818884333892));
#99073=CARTESIAN_POINT('Ctrl Pts',(-10.3229726036237,18.1203705014787,2.36739589892121));
#99074=CARTESIAN_POINT('Ctrl Pts',(-10.3162057316406,18.1198950483606,2.36548413800484));
#99075=CARTESIAN_POINT('Ctrl Pts',(-10.312203618327,18.1196154767017,2.36437629126054));
#99076=CARTESIAN_POINT('Ctrl Pts',(-10.297764302382,18.1186123670068,2.36046136757202));
#99077=CARTESIAN_POINT('Ctrl Pts',(-10.287294053668,18.1178954357742,2.35777671979731));
#99078=CARTESIAN_POINT('Ctrl Pts',(-10.2610370337925,18.1161201219387,2.35142813809792));
#99079=CARTESIAN_POINT('Ctrl Pts',(-10.2452084354103,18.1150701423105,2.34794508244518));
#99080=CARTESIAN_POINT('Ctrl Pts',(-10.1753052305177,18.1105016912029,2.33406911861617));
#99081=CARTESIAN_POINT('Ctrl Pts',(-10.1206085605618,18.1071038267697,2.32714822764158));
#99082=CARTESIAN_POINT('Ctrl Pts',(-9.98053663495295,18.0984317542157,2.31933122154072));
#99083=CARTESIAN_POINT('Ctrl Pts',(-9.89520662422518,18.0931587899832,2.32383104602558));
#99084=CARTESIAN_POINT('Ctrl Pts',(-9.81110406180164,18.0875733665015,2.3374969303128));
#99085=CARTESIAN_POINT('Ctrl Pts',(-9.81110440024615,17.9879475328942,2.33749687531877));
#99086=CARTESIAN_POINT('Ctrl Pts',(-9.89624655459561,17.9932799162418,2.32366209245349));
#99087=CARTESIAN_POINT('Ctrl Pts',(-9.98262890818452,17.9986092040002,2.31922423813105));
#99088=CARTESIAN_POINT('Ctrl Pts',(-10.0775110639795,18.0048348360056,2.32477043396183));
#99089=CARTESIAN_POINT('Ctrl Pts',(-10.0862895802192,18.0054140870354,2.32538236028972));
#99090=CARTESIAN_POINT('Ctrl Pts',(-10.1008871800037,18.0063831519045,2.32656443916478));
#99091=CARTESIAN_POINT('Ctrl Pts',(-10.1067104492753,18.0067712805985,2.32707966319707));
#99092=CARTESIAN_POINT('Ctrl Pts',(-10.1181310954306,18.0075356525651,2.3281758779023));
#99093=CARTESIAN_POINT('Ctrl Pts',(-10.123728626005,18.0079117874567,2.32875367489248));
#99094=CARTESIAN_POINT('Ctrl Pts',(-10.1342783242733,18.0086236152886,2.32991912164577));
#99095=CARTESIAN_POINT('Ctrl Pts',(-10.1392313345299,18.0089590319524,2.3304981554405));
#99096=CARTESIAN_POINT('Ctrl Pts',(-10.1504082367705,18.009718753683,2.33187680435392));
#99097=CARTESIAN_POINT('Ctrl Pts',(-10.1566296744157,18.0101436225768,2.33269473558102));
#99098=CARTESIAN_POINT('Ctrl Pts',(-10.1726154039065,18.0112405480649,2.33492647329904));
#99099=CARTESIAN_POINT('Ctrl Pts',(-10.182368836859,18.0119148662445,2.33641330477323));
#99100=CARTESIAN_POINT('Ctrl Pts',(-10.2570175307998,18.0171158007603,2.34875448762267));
#99101=CARTESIAN_POINT('Ctrl Pts',(-10.3209080357674,18.0218095374206,2.36490547037418));
#99102=CARTESIAN_POINT('Ctrl Pts',(-10.427830953069,18.0300471456841,2.40168644266637));
#99103=CARTESIAN_POINT('Ctrl Pts',(-10.4715870104864,18.0335336224847,2.41975118561526));
#99104=CARTESIAN_POINT('Ctrl Pts',(-10.5592647438194,18.0406676563981,2.4622938759754));
#99105=CARTESIAN_POINT('Ctrl Pts',(-10.6029532176322,18.0443050612248,2.48705397359862));
#99106=CARTESIAN_POINT('Ctrl Pts',(-10.6510388957987,18.0483075126372,2.51852322725529));
#99107=CARTESIAN_POINT('Ctrl Pts',(-10.6571069916028,18.0488125319615,2.52257547217418));
#99108=CARTESIAN_POINT('Ctrl Pts',(-10.6661195342621,18.049562052046,2.5287158750594));
#99109=CARTESIAN_POINT('Ctrl Pts',(-10.6690925397554,18.0498092084123,2.5307615054033));
#99110=CARTESIAN_POINT('Ctrl Pts',(-10.6743311701619,18.0502444864554,2.53440163100622));
#99111=CARTESIAN_POINT('Ctrl Pts',(-10.6766006208901,18.0504329756944,2.53599048881924));
#99112=CARTESIAN_POINT('Ctrl Pts',(-10.6815185491109,18.0508412501147,2.53945948636753));
#99113=CARTESIAN_POINT('Ctrl Pts',(-10.6841648643626,18.0510608321134,2.54134257937088));
#99114=CARTESIAN_POINT('Ctrl Pts',(-10.6914308519375,18.0516635408586,2.54655839873518));
#99115=CARTESIAN_POINT('Ctrl Pts',(-10.6960342637986,18.0520451694833,2.54991378448837));
#99116=CARTESIAN_POINT('Ctrl Pts',(-10.7200556131997,18.0540364566971,2.567691032664));
#99117=CARTESIAN_POINT('Ctrl Pts',(-10.7390517520593,18.0556108103593,2.58267628412831));
#99118=CARTESIAN_POINT('Ctrl Pts',(-10.7700572192921,18.0582053337136,2.6087240954319));
#99119=CARTESIAN_POINT('Ctrl Pts',(-10.782321447387,18.0592385149888,2.61946944896289));
#99120=CARTESIAN_POINT('Ctrl Pts',(-10.8665400769098,18.0664141439465,2.69640704768386));
#99121=CARTESIAN_POINT('Ctrl Pts',(-10.9302287797529,18.072297639372,2.77107702809972));
#99122=CARTESIAN_POINT('Ctrl Pts',(-11.0012969513953,18.0805465736133,2.87911775893009));
#99123=CARTESIAN_POINT('Ctrl Pts',(-11.0175669802793,18.0825886942385,2.90615868717428));
#99124=CARTESIAN_POINT('Ctrl Pts',(-11.0368917332421,18.0852410942817,2.9414075683207));
#99125=CARTESIAN_POINT('Ctrl Pts',(-11.0409685778024,18.085815002005,2.94904230235077));
#99126=CARTESIAN_POINT('Ctrl Pts',(-11.0475137474967,18.0867607326882,2.96163150102086));
#99127=CARTESIAN_POINT('Ctrl Pts',(-11.050031996066,18.0871308034235,2.96655975278603));
#99128=CARTESIAN_POINT('Ctrl Pts',(-11.0547609299961,18.0878378101128,2.9759775909874));
#99129=CARTESIAN_POINT('Ctrl Pts',(-11.0569779239451,18.0881745176379,2.98046388811284));
#99130=CARTESIAN_POINT('Ctrl Pts',(-11.0619802149983,18.088946476539,2.9907510505271));
#99131=CARTESIAN_POINT('Ctrl Pts',(-11.064746675872,18.0893823647818,2.99656084483712));
#99132=CARTESIAN_POINT('Ctrl Pts',(-11.0731600540232,18.0907363857097,3.0146092005051));
#99133=CARTESIAN_POINT('Ctrl Pts',(-11.0786444231333,18.0916600018157,3.02692187541603));
#99134=CARTESIAN_POINT('Ctrl Pts',(-11.1237287054172,18.09961956489,3.13300020560193));
#99135=CARTESIAN_POINT('Ctrl Pts',(-11.1512224620096,18.1070757754673,3.23142357484736));
#99136=CARTESIAN_POINT('Ctrl Pts',(-11.1739626620484,18.1187789845062,3.38933301401143));
#99137=CARTESIAN_POINT('Ctrl Pts',(-11.1779796688525,18.122992580794,3.44707548108584));
#99138=CARTESIAN_POINT('Ctrl Pts',(-11.1777099224079,18.1275193761673,3.51210437389066));
#99139=CARTESIAN_POINT('Ctrl Pts',(-11.1776136034679,18.1280188069853,3.51932316421637));
#99140=CARTESIAN_POINT('Ctrl Pts',(-11.1773713344172,18.1287573690225,3.53007112707584));
#99141=CARTESIAN_POINT('Ctrl Pts',(-11.1772758804101,18.128999127416,3.53360110145967));
#99142=CARTESIAN_POINT('Ctrl Pts',(-11.1770850238677,18.1294120818648,3.53965188563967));
#99143=CARTESIAN_POINT('Ctrl Pts',(-11.1769973980032,18.1295837008919,3.54217287024685));
#99144=CARTESIAN_POINT('Ctrl Pts',(-11.1767799701779,18.1299724741011,3.54789832090751));
#99145=CARTESIAN_POINT('Ctrl Pts',(-11.176645179033,18.1301893498057,3.5511025502051));
#99146=CARTESIAN_POINT('Ctrl Pts',(-11.1762428663064,18.1307774616389,3.55981830479311));
#99147=CARTESIAN_POINT('Ctrl Pts',(-11.1759496930189,18.1311473159028,3.56532865053895));
#99148=CARTESIAN_POINT('Ctrl Pts',(-11.1743019023393,18.1329739809639,3.592675597958));
#99149=CARTESIAN_POINT('Ctrl Pts',(-11.1723776333173,18.1344020519729,3.61447513884007));
#99150=CARTESIAN_POINT('Ctrl Pts',(-11.1672940276228,18.1372284385312,3.65813595041488));
#99151=CARTESIAN_POINT('Ctrl Pts',(-11.1641250549916,18.1386258105676,3.67998688690251));
#99152=CARTESIAN_POINT('Ctrl Pts',(-11.1433098933133,18.1462488728141,3.79971086770836));
#99153=CARTESIAN_POINT('Ctrl Pts',(-11.113937697215,18.152238247045,3.89512961520169));
#99154=CARTESIAN_POINT('Ctrl Pts',(-11.0615380775325,18.1603808106143,4.01087592366385));
#99155=CARTESIAN_POINT('Ctrl Pts',(-11.0492717296893,18.1621741554056,4.03561734945052));
#99156=CARTESIAN_POINT('Ctrl Pts',(-11.0321300975534,18.1645556914776,4.06733937039312));
#99157=CARTESIAN_POINT('Ctrl Pts',(-11.0280321515678,18.1651166482754,4.07473157963259));
#99158=CARTESIAN_POINT('Ctrl Pts',(-11.0211929955393,18.1660397093128,4.08676140042664));
#99159=CARTESIAN_POINT('Ctrl Pts',(-11.0184988536213,18.1664001330915,4.09142553098409));
#99160=CARTESIAN_POINT('Ctrl Pts',(-11.0132165938155,18.1671007620256,4.10042710384001));
#99161=CARTESIAN_POINT('Ctrl Pts',(-11.0106323767912,18.1674408211155,4.10476670759857));
#99162=CARTESIAN_POINT('Ctrl Pts',(-11.0045834595305,18.168230677414,4.11477743966129));
#99163=CARTESIAN_POINT('Ctrl Pts',(-11.0010985400478,18.1686812014477,4.12043608651119));
#99164=CARTESIAN_POINT('Ctrl Pts',(-10.9895817743488,18.1701557052223,4.13878679549814));
#99165=CARTESIAN_POINT('Ctrl Pts',(-10.9813552755226,18.1711867736038,4.15135431612303));
#99166=CARTESIAN_POINT('Ctrl Pts',(-10.9267227928378,18.1778982903094,4.23143055451366));
#99167=CARTESIAN_POINT('Ctrl Pts',(-10.8736287694844,18.1838356198729,4.29408683982925));
#99168=CARTESIAN_POINT('Ctrl Pts',(-10.7753713026008,18.1938195071085,4.38815843873974));
#99169=CARTESIAN_POINT('Ctrl Pts',(-10.7337286537663,18.1978070430937,4.42285909312762));
#99170=CARTESIAN_POINT('Ctrl Pts',(-10.676832845844,18.2028394868716,4.46397618610012));
#99171=CARTESIAN_POINT('Ctrl Pts',(-10.6636295051111,18.2039802876305,4.4731129034171));
#99172=CARTESIAN_POINT('Ctrl Pts',(-10.6412944729006,18.2058605431677,4.48790264932902));
#99173=CARTESIAN_POINT('Ctrl Pts',(-10.6322651524079,18.206607576266,4.49370571249061));
#99174=CARTESIAN_POINT('Ctrl Pts',(-10.6196441671913,18.2076324459177,4.50157541405822));
#99175=CARTESIAN_POINT('Ctrl Pts',(-10.6161193657051,18.2079166159014,4.50374754420095));
#99176=CARTESIAN_POINT('Ctrl Pts',(-10.6101267082335,18.2083961748561,4.50739700919644));
#99177=CARTESIAN_POINT('Ctrl Pts',(-10.6076647823862,18.2085921754131,4.50888396119855));
#99178=CARTESIAN_POINT('Ctrl Pts',(-10.6029278669056,18.2089673181232,4.5117213294734));
#99179=CARTESIAN_POINT('Ctrl Pts',(-10.6006537516094,18.2091465523294,4.51307311297533));
#99180=CARTESIAN_POINT('Ctrl Pts',(-10.5951843999809,18.2095755934179,4.51629932359965));
#99181=CARTESIAN_POINT('Ctrl Pts',(-10.5919848121232,18.2098249326549,4.5181663755355));
#99182=CARTESIAN_POINT('Ctrl Pts',(-10.5802985309488,18.210729830924,4.52491194717597));
#99183=CARTESIAN_POINT('Ctrl Pts',(-10.5717596251167,18.211379938864,4.52969987422535));
#99184=CARTESIAN_POINT('Ctrl Pts',(-10.5103747872259,18.2159821661062,4.5631204312217));
#99185=CARTESIAN_POINT('Ctrl Pts',(-10.4554580488336,18.2197281853221,4.5877809253376));
#99186=CARTESIAN_POINT('Ctrl Pts',(-10.3351663407662,18.227645404358,4.63108167252156));
#99187=CARTESIAN_POINT('Ctrl Pts',(-10.2695844409577,18.2317996467166,4.64847979840075));
#99188=CARTESIAN_POINT('Ctrl Pts',(-10.1684502216729,18.2383249938015,4.66616496292897));
#99189=CARTESIAN_POINT('Ctrl Pts',(-10.1337799518953,18.24058082642,4.67064886017548));
#99190=CARTESIAN_POINT('Ctrl Pts',(-10.0898624353504,18.2434872683334,4.67435226128064));
#99191=CARTESIAN_POINT('Ctrl Pts',(-10.0807524246799,18.2440927560317,4.67501384204308));
#99192=CARTESIAN_POINT('Ctrl Pts',(-10.0661107185064,18.2450704674166,4.6759060658985));
#99193=CARTESIAN_POINT('Ctrl Pts',(-10.060583365428,18.2454406031612,4.67620379057935));
#99194=CARTESIAN_POINT('Ctrl Pts',(-10.0500556883709,18.2461476587458,4.67669644784738));
#99195=CARTESIAN_POINT('Ctrl Pts',(-10.0450558062762,18.2464843496313,4.67689849830154));
#99196=CARTESIAN_POINT('Ctrl Pts',(-10.0336256133754,18.2472561637289,4.6772874600654));
#99197=CARTESIAN_POINT('Ctrl Pts',(-10.0271948015114,18.2476919229504,4.67745355977199));
#99198=CARTESIAN_POINT('Ctrl Pts',(-10.0072965903409,18.2490451393374,4.67780440841259));
#99199=CARTESIAN_POINT('Ctrl Pts',(-9.99382754803064,18.2499680705262,4.67781082493407));
#99200=CARTESIAN_POINT('Ctrl Pts',(-9.87851607912541,18.2579320588304,4.67588781825329));
#99201=CARTESIAN_POINT('Ctrl Pts',(-9.7773397300021,18.2653941079817,4.6609841903134));
#99202=CARTESIAN_POINT('Ctrl Pts',(-9.62380994026725,18.2770984894761,4.61754636115816));
#99203=CARTESIAN_POINT('Ctrl Pts',(-9.56947619617376,18.2813076838934,4.59776120950571));
#99204=CARTESIAN_POINT('Ctrl Pts',(-9.51022586654913,18.2858303157477,4.57110618120037));
#99205=CARTESIAN_POINT('Ctrl Pts',(-9.50367100668084,18.2863296298738,4.5680845894087));
#99206=CARTESIAN_POINT('Ctrl Pts',(-9.49395128857164,18.2870680537542,4.56349528966235));
#99207=CARTESIAN_POINT('Ctrl Pts',(-9.49076518382856,18.2873097892858,4.56197336703647));
#99208=CARTESIAN_POINT('Ctrl Pts',(-9.48531472337242,18.2877227182769,4.55933964868881));
#99209=CARTESIAN_POINT('Ctrl Pts',(-9.48304704812351,18.2878943345572,4.55823488472557));
#99210=CARTESIAN_POINT('Ctrl Pts',(-9.47790413636035,18.288283119937,4.55570888883348));
#99211=CARTESIAN_POINT('Ctrl Pts',(-9.47503114506118,18.2885000104444,4.55428319286481));
#99212=CARTESIAN_POINT('Ctrl Pts',(-9.46723035984916,18.2890882019001,4.55037232988464));
#99213=CARTESIAN_POINT('Ctrl Pts',(-9.46231407576237,18.2894581203609,4.54786419477882));
#99214=CARTESIAN_POINT('Ctrl Pts',(-9.43798686714166,18.2912856192423,4.53523691572724));
#99215=CARTESIAN_POINT('Ctrl Pts',(-9.4188416518202,18.2927144285093,4.52461180745118));
#99216=CARTESIAN_POINT('Ctrl Pts',(-9.38100938219991,18.2955413722563,4.50221397226953));
#99217=CARTESIAN_POINT('Ctrl Pts',(-9.36233530163464,18.2969385898355,4.49043730791836));
#99218=CARTESIAN_POINT('Ctrl Pts',(-9.26139765913469,18.3045625736288,4.42274280095003));
#99219=CARTESIAN_POINT('Ctrl Pts',(-9.18614589061285,18.3105530304517,4.35710540261612));
#99220=CARTESIAN_POINT('Ctrl Pts',(-9.10170303908136,18.3186954464042,4.26218012688427));
#99221=CARTESIAN_POINT('Ctrl Pts',(-9.08409993934672,18.3204872710746,4.24093377808199));
#99222=CARTESIAN_POINT('Ctrl Pts',(-9.06210094078125,18.3228670699843,4.21239863223821));
#99223=CARTESIAN_POINT('Ctrl Pts',(-9.0570142691155,18.3234278606348,4.2056517283069));
#99224=CARTESIAN_POINT('Ctrl Pts',(-9.04880493339615,18.3243507181473,4.1945156690034));
#99225=CARTESIAN_POINT('Ctrl Pts',(-9.04563894558165,18.3247111060049,4.19015871029149));
#99226=CARTESIAN_POINT('Ctrl Pts',(-9.03956188737649,18.3254117151025,4.18167382754315));
#99227=CARTESIAN_POINT('Ctrl Pts',(-9.03664726509804,18.3257517906039,4.17754858285099));
#99228=CARTESIAN_POINT('Ctrl Pts',(-9.02995869865391,18.3265417587979,4.16795143513183));
#99229=CARTESIAN_POINT('Ctrl Pts',(-9.02620439401565,18.3269923789523,4.16246612036225));
#99230=CARTESIAN_POINT('Ctrl Pts',(-9.01411427830674,18.3284675252336,4.14447671868318));
#99231=CARTESIAN_POINT('Ctrl Pts',(-9.00597161324908,18.3294991485851,4.13184525569275));
#99232=CARTESIAN_POINT('Ctrl Pts',(-8.95516086036789,18.3361919565036,4.04961009884403));
#99233=CARTESIAN_POINT('Ctrl Pts',(-8.91959388633695,18.3421080836765,3.97589715996257));
#99234=CARTESIAN_POINT('Ctrl Pts',(-8.8735198630548,18.3520865123483,3.84798182249075));
#99235=CARTESIAN_POINT('Ctrl Pts',(-8.85866282121709,18.3560899583041,3.79563299143681));
#99236=CARTESIAN_POINT('Ctrl Pts',(-8.84416212533963,18.3611402196289,3.72669957180082));
#99237=CARTESIAN_POINT('Ctrl Pts',(-8.84117310622523,18.3622835156834,3.7108890068058));
#99238=CARTESIAN_POINT('Ctrl Pts',(-8.83672886962364,18.3641674345998,3.68442041156964));
#99239=CARTESIAN_POINT('Ctrl Pts',(-8.83509404162091,18.3649156713764,3.67379510826856));
#99240=CARTESIAN_POINT('Ctrl Pts',(-8.83303096585809,18.3659419026605,3.65904558680714));
#99241=CARTESIAN_POINT('Ctrl Pts',(-8.83247872274192,18.3662262521877,3.65493964562733));
#99242=CARTESIAN_POINT('Ctrl Pts',(-8.83157975420406,18.3667060246195,3.64797792508561));
#99243=CARTESIAN_POINT('Ctrl Pts',(-8.83122180818548,18.3669020603605,3.64512365801137));
#99244=CARTESIAN_POINT('Ctrl Pts',(-8.83055481796598,18.3672771996999,3.63964248761962));
#99245=CARTESIAN_POINT('Ctrl Pts',(-8.83024416166529,18.3674563957659,3.63701582815862));
#99246=CARTESIAN_POINT('Ctrl Pts',(-8.8295199078594,18.3678852529712,3.63071007167855));
#99247=CARTESIAN_POINT('Ctrl Pts',(-8.82911480095663,18.3681344473567,3.62702999850877));
#99248=CARTESIAN_POINT('Ctrl Pts',(-8.82770365067842,18.3690380497597,3.61363017070219));
#99249=CARTESIAN_POINT('Ctrl Pts',(-8.82680119339457,18.3696870276938,3.60389957572614));
#99250=CARTESIAN_POINT('Ctrl Pts',(-8.82118841703263,18.3743100207085,3.53391876247904));
#99251=CARTESIAN_POINT('Ctrl Pts',(-8.82100001393733,18.3780755183309,3.47338813801381));
#99252=CARTESIAN_POINT('Ctrl Pts',(-8.82930223483163,18.3850432005377,3.36117048309988));
#99253=CARTESIAN_POINT('Ctrl Pts',(-8.83658444193764,18.3882436265389,3.3095506956916));
#99254=CARTESIAN_POINT('Ctrl Pts',(-8.8538570894595,18.3935323922451,3.22707554986978));
#99255=CARTESIAN_POINT('Ctrl Pts',(-8.86174421446304,18.3955757670389,3.19585389264921));
#99256=CARTESIAN_POINT('Ctrl Pts',(-8.87493822674618,18.3985736378633,3.1513846675296));
#99257=CARTESIAN_POINT('Ctrl Pts',(-8.87922240176128,18.3994980844753,3.13784783269082));
#99258=CARTESIAN_POINT('Ctrl Pts',(-8.88735401788923,18.401172049723,3.11368189329267));
#99259=CARTESIAN_POINT('Ctrl Pts',(-8.89111178507049,18.401918680841,3.10302434163622));
#99260=CARTESIAN_POINT('Ctrl Pts',(-8.89709891113719,18.403069489924,3.08679271391117));
#99261=CARTESIAN_POINT('Ctrl Pts',(-8.89921856833119,18.4034700524006,3.08117866514559));
#99262=CARTESIAN_POINT('Ctrl Pts',(-8.90315471946913,18.4042017615654,3.07098983780693));
#99263=CARTESIAN_POINT('Ctrl Pts',(-8.90495717627639,18.4045324352286,3.06640975375854));
#99264=CARTESIAN_POINT('Ctrl Pts',(-8.9089515490497,18.4052558693646,3.05644374416888));
#99265=CARTESIAN_POINT('Ctrl Pts',(-8.91115474011382,18.4056490001597,3.05106250732625));
#99266=CARTESIAN_POINT('Ctrl Pts',(-8.91730879281347,18.4067313485794,3.03634320948005));
#99267=CARTESIAN_POINT('Ctrl Pts',(-8.92134045911533,18.4074232657645,3.02703969176047));
#99268=CARTESIAN_POINT('Ctrl Pts',(-8.94420991820909,18.4112574654107,2.97607972307845));
#99269=CARTESIAN_POINT('Ctrl Pts',(-8.96533847017534,18.4144770657886,2.9355004721414));
#99270=CARTESIAN_POINT('Ctrl Pts',(-9.03085482954009,18.4236590778649,2.82576497294438));
#99271=CARTESIAN_POINT('Ctrl Pts',(-9.08019497647052,18.4297550888367,2.75987024362528));
#99272=CARTESIAN_POINT('Ctrl Pts',(-9.16221862174384,18.4385294239397,2.67132123871332));
#99273=CARTESIAN_POINT('Ctrl Pts',(-9.18983972701976,18.4412990982674,2.64429728968606));
#99274=CARTESIAN_POINT('Ctrl Pts',(-9.22339103149082,18.4444113169594,2.61455538012551));
#99275=CARTESIAN_POINT('Ctrl Pts',(-9.22807301441973,18.4448402300817,2.61047068738269));
#99276=CARTESIAN_POINT('Ctrl Pts',(-9.23531010941911,18.4454947102431,2.60425701750173));
#99277=CARTESIAN_POINT('Ctrl Pts',(-9.2378421908074,18.4457221208378,2.60210156808752));
#99278=CARTESIAN_POINT('Ctrl Pts',(-9.24251491980092,18.4461388451465,2.5981578877948));
#99279=CARTESIAN_POINT('Ctrl Pts',(-9.24465278765459,18.4463283777685,2.5963665393551));
#99280=CARTESIAN_POINT('Ctrl Pts',(-9.24950251291036,18.4467558051354,2.5923321262458));
#99281=CARTESIAN_POINT('Ctrl Pts',(-9.25221807120943,18.4469933740409,2.59009361198067));
#99282=CARTESIAN_POINT('Ctrl Pts',(-9.25926933499607,18.4476058222775,2.58433393627761));
#99283=CARTESIAN_POINT('Ctrl Pts',(-9.26362018802743,18.447979427891,2.58083133545519));
#99284=CARTESIAN_POINT('Ctrl Pts',(-9.29249456489808,18.4504319288529,2.55792298962229));
#99285=CARTESIAN_POINT('Ctrl Pts',(-9.31776017914787,18.4524508247053,2.53946772444647));
#99286=CARTESIAN_POINT('Ctrl Pts',(-9.42384227091535,18.460557448076,2.46828068823577));
#99287=CARTESIAN_POINT('Ctrl Pts',(-9.51025497710065,18.4663519572449,2.42456781225349));
#99288=CARTESIAN_POINT('Ctrl Pts',(-9.63876069485742,18.4749879898778,2.37830091267319));
#99289=CARTESIAN_POINT('Ctrl Pts',(-9.67715047978829,18.4775655108535,2.36665524604034));
#99290=CARTESIAN_POINT('Ctrl Pts',(-9.7252929361676,18.4808340394498,2.35469581774253));
#99291=CARTESIAN_POINT('Ctrl Pts',(-9.73455670897024,18.4814645403141,2.35251340256812));
#99292=CARTESIAN_POINT('Ctrl Pts',(-9.74933048893811,18.4824729875636,2.34922137863148));
#99293=CARTESIAN_POINT('Ctrl Pts',(-9.75482387799382,18.4828486018293,2.34803849607988));
#99294=CARTESIAN_POINT('Ctrl Pts',(-9.76520904626305,18.4835599967895,2.34587992371218));
#99295=CARTESIAN_POINT('Ctrl Pts',(-9.77009898396429,18.4838955052308,2.34489590774025));
#99296=CARTESIAN_POINT('Ctrl Pts',(-9.78116678250418,18.4846561851731,2.34274176617434));
#99297=CARTESIAN_POINT('Ctrl Pts',(-9.78734801827866,18.4850819262733,2.341589999679));
#99298=CARTESIAN_POINT('Ctrl Pts',(-9.79938593191289,18.4859129265063,2.33944653728568));
#99299=CARTESIAN_POINT('Ctrl Pts',(-9.80524142726179,18.4863180005648,2.33844955389612));
#99300=CARTESIAN_POINT('Ctrl Pts',(-9.81110406377177,18.4867244625755,2.33749692999267));
#99301=CARTESIAN_POINT('Origin',(-10.,12.3756328852638,3.5));
#99302=CARTESIAN_POINT('',(-9.81110406371068,19.0863176770662,2.3374969300026));
#99303=CARTESIAN_POINT('',(-9.81110406413403,18.9883401336252,2.33749692993381));
#99304=CARTESIAN_POINT('',(-9.81110406371068,12.3756328852638,2.3374969300026));
#99305=CARTESIAN_POINT('Ctrl Pts',(-9.81110406371067,19.0863176770662,2.3374969300026));
#99306=CARTESIAN_POINT('Ctrl Pts',(-9.79998400258774,19.0854907841518,2.33930383650601));
#99307=CARTESIAN_POINT('Ctrl Pts',(-9.78888576509648,19.0846642194548,2.34127096453477));
#99308=CARTESIAN_POINT('Ctrl Pts',(-9.72816303969516,19.0801389074277,2.35293600888952));
#99309=CARTESIAN_POINT('Ctrl Pts',(-9.67917261129528,19.0764752257255,2.36566223870694));
#99310=CARTESIAN_POINT('Ctrl Pts',(-9.62482488272611,19.0724968665875,2.38358475133384));
#99311=CARTESIAN_POINT('Ctrl Pts',(-9.61852053254864,19.0720367550016,2.38572319545148));
#99312=CARTESIAN_POINT('Ctrl Pts',(-9.60896544392668,19.0713418497106,2.3890548959235));
#99313=CARTESIAN_POINT('Ctrl Pts',(-9.60570140454673,19.0711049067735,2.39020917884645));
#99314=CARTESIAN_POINT('Ctrl Pts',(-9.59981824651872,19.0706786892108,2.39231890929555));
#99315=CARTESIAN_POINT('Ctrl Pts',(-9.59719740566085,19.0704891283364,2.39326927169212));
#99316=CARTESIAN_POINT('Ctrl Pts',(-9.59140945740733,19.0700711831091,2.3953913662672));
#99317=CARTESIAN_POINT('Ctrl Pts',(-9.58824400559542,19.0698430556597,2.3965674161938));
#99318=CARTESIAN_POINT('Ctrl Pts',(-9.57904224954649,19.0691810904604,2.40003122565024));
#99319=CARTESIAN_POINT('Ctrl Pts',(-9.57301952247867,19.0687493122699,2.40235506255322));
#99320=CARTESIAN_POINT('Ctrl Pts',(-9.52303949310428,19.0651761876398,2.4221132215645));
#99321=CARTESIAN_POINT('Ctrl Pts',(-9.48014391937047,19.0621735933518,2.44213325427585));
#99322=CARTESIAN_POINT('Ctrl Pts',(-9.41448169321778,19.0575056016143,2.47774080300979));
#99323=CARTESIAN_POINT('Ctrl Pts',(-9.39086208190029,19.0558108590556,2.49163666484558));
#99324=CARTESIAN_POINT('Ctrl Pts',(-9.29702912408821,19.0489350406853,2.55134148710412));
#99325=CARTESIAN_POINT('Ctrl Pts',(-9.23132466535231,19.0437624975836,2.60375388754537));
#99326=CARTESIAN_POINT('Ctrl Pts',(-9.16110829012873,19.0373200254693,2.67321133735428));
#99327=CARTESIAN_POINT('Ctrl Pts',(-9.15067609718986,19.0363363046374,2.68393157842004));
#99328=CARTESIAN_POINT('Ctrl Pts',(-9.13591458038499,19.0349034661078,2.69969037993726));
#99329=CARTESIAN_POINT('Ctrl Pts',(-9.13141899381979,19.0344614154831,2.70457172980403));
#99330=CARTESIAN_POINT('Ctrl Pts',(-9.12357501119376,19.0336798607689,2.713234590327));
#99331=CARTESIAN_POINT('Ctrl Pts',(-9.12020921026243,19.0333410958976,2.71700016871379));
#99332=CARTESIAN_POINT('Ctrl Pts',(-9.11329974529456,19.0326385018901,2.72483111217792));
#99333=CARTESIAN_POINT('Ctrl Pts',(-9.10975958250047,19.0322745394522,2.72889939455472));
#99334=CARTESIAN_POINT('Ctrl Pts',(-9.1007270060145,19.031335497959,2.7394245589286));
#99335=CARTESIAN_POINT('Ctrl Pts',(-9.09527621637551,19.0307587455026,2.74591659077249));
#99336=CARTESIAN_POINT('Ctrl Pts',(-9.07223408091918,19.0282764271102,2.77396984100779));
#99337=CARTESIAN_POINT('Ctrl Pts',(-9.0553410949428,19.026343544825,2.79609040389123));
#99338=CARTESIAN_POINT('Ctrl Pts',(-8.98179620120832,19.0173818414405,2.89981473047593));
#99339=CARTESIAN_POINT('Ctrl Pts',(-8.93483146816138,19.0100122167057,2.98777791571953));
#99340=CARTESIAN_POINT('Ctrl Pts',(-8.89158921802332,19.0011627066966,3.10123939386179));
#99341=CARTESIAN_POINT('Ctrl Pts',(-8.88429422915025,18.9995608289268,3.12213069710084));
#99342=CARTESIAN_POINT('Ctrl Pts',(-8.87101429514304,18.996425836262,3.16390810003806));
#99343=CARTESIAN_POINT('Ctrl Pts',(-8.86500976498491,18.994892562184,3.18477975909209));
#99344=CARTESIAN_POINT('Ctrl Pts',(-8.85821020442655,18.9930068619418,3.211137693731));
#99345=CARTESIAN_POINT('Ctrl Pts',(-8.85687241657059,18.9926273814706,3.21647804275222));
#99346=CARTESIAN_POINT('Ctrl Pts',(-8.85481516921627,18.9920302394285,3.224941758712));
#99347=CARTESIAN_POINT('Ctrl Pts',(-8.85407094859939,18.9918112282617,3.22805893554562));
#99348=CARTESIAN_POINT('Ctrl Pts',(-8.85276335288098,18.9914210330536,3.23363651061897));
#99349=CARTESIAN_POINT('Ctrl Pts',(-8.85219516588755,18.9912495832095,3.23609566897549));
#99350=CARTESIAN_POINT('Ctrl Pts',(-8.85084959427549,18.9908389129372,3.24200596603605));
#99351=CARTESIAN_POINT('Ctrl Pts',(-8.85007984832411,18.9906001272704,3.24545880072074));
#99352=CARTESIAN_POINT('Ctrl Pts',(-8.84778056063179,18.989874709366,3.25599599922743));
#99353=CARTESIAN_POINT('Ctrl Pts',(-8.84630080768773,18.9893907835142,3.26309122211892));
#99354=CARTESIAN_POINT('Ctrl Pts',(-8.83342528632705,18.9850140235566,3.32781132193521));
#99355=CARTESIAN_POINT('Ctrl Pts',(-8.82628841603408,18.9813324031335,3.3862081527337));
#99356=CARTESIAN_POINT('Ctrl Pts',(-8.81883617117429,18.9714492689713,3.54532661765381));
#99357=CARTESIAN_POINT('Ctrl Pts',(-8.82701018842903,18.9653233945672,3.64592915043192));
#99358=CARTESIAN_POINT('Ctrl Pts',(-8.85040627704,18.957948760933,3.75628134001346));
#99359=CARTESIAN_POINT('Ctrl Pts',(-8.85314075385154,18.9571404936181,3.76825306017515));
#99360=CARTESIAN_POINT('Ctrl Pts',(-8.85755593364221,18.9559099267463,3.78627969302862));
#99361=CARTESIAN_POINT('Ctrl Pts',(-8.85909877664834,18.9554919885486,3.79236775367464));
#99362=CARTESIAN_POINT('Ctrl Pts',(-8.8618720366625,18.9547609796132,3.80295470449677));
#99363=CARTESIAN_POINT('Ctrl Pts',(-8.8630806322569,18.9544486118587,3.80745920719682));
#99364=CARTESIAN_POINT('Ctrl Pts',(-8.86566814277827,18.9537925125666,3.81687909683994));
#99365=CARTESIAN_POINT('Ctrl Pts',(-8.86705232373346,18.95344861751,3.82179292370729));
#99366=CARTESIAN_POINT('Ctrl Pts',(-8.87043021199245,18.9526258194779,3.83349239183901));
#99367=CARTESIAN_POINT('Ctrl Pts',(-8.87245316161597,18.9521459813136,3.84026931223404));
#99368=CARTESIAN_POINT('Ctrl Pts',(-8.87957439581595,18.9504994052089,3.86336456049646));
#99369=CARTESIAN_POINT('Ctrl Pts',(-8.8849666826012,18.9493232124068,3.87958923329227));
#99370=CARTESIAN_POINT('Ctrl Pts',(-8.91520067677335,18.943072253366,3.96434816573856));
#99371=CARTESIAN_POINT('Ctrl Pts',(-8.94600859246498,18.9378033393692,4.03057291809629));
#99372=CARTESIAN_POINT('Ctrl Pts',(-9.02206514510724,18.9267390668157,4.16093147815351));
#99373=CARTESIAN_POINT('Ctrl Pts',(-9.06800517295492,18.9209604702316,4.22427524741828));
#99374=CARTESIAN_POINT('Ctrl Pts',(-9.12600550551236,18.9148512896116,4.28950219229256));
#99375=CARTESIAN_POINT('Ctrl Pts',(-9.13221373951829,18.9142106830921,4.29632098260347));
#99376=CARTESIAN_POINT('Ctrl Pts',(-9.14097090452611,18.9133262088424,4.30571532787416));
#99377=CARTESIAN_POINT('Ctrl Pts',(-9.14345239949684,18.9130776712334,4.30835288419642));
#99378=CARTESIAN_POINT('Ctrl Pts',(-9.14775315307273,18.9126505816476,4.31288207119822));
#99379=CARTESIAN_POINT('Ctrl Pts',(-9.14956662319596,18.9124716021644,4.31477912450985));
#99380=CARTESIAN_POINT('Ctrl Pts',(-9.15339596494298,18.912096022413,4.31875824806223));
#99381=CARTESIAN_POINT('Ctrl Pts',(-9.15541320532642,18.9118995351367,4.32083896564153));
#99382=CARTESIAN_POINT('Ctrl Pts',(-9.16040591222934,18.911416508555,4.32595088924892));
#99383=CARTESIAN_POINT('Ctrl Pts',(-9.1633901732139,18.9111306409251,4.32897352357623));
#99384=CARTESIAN_POINT('Ctrl Pts',(-9.17448093381527,18.9100784027957,4.34008600254205));
#99385=CARTESIAN_POINT('Ctrl Pts',(-9.1826892674293,18.9093195185481,4.34807394191538));
#99386=CARTESIAN_POINT('Ctrl Pts',(-9.24234764927128,18.9039327368299,4.40445963977172));
#99387=CARTESIAN_POINT('Ctrl Pts',(-9.2979500151173,18.8995806610879,4.44826832722522));
#99388=CARTESIAN_POINT('Ctrl Pts',(-9.42457065689338,18.8902393084136,4.53075240296901));
#99389=CARTESIAN_POINT('Ctrl Pts',(-9.49630518013522,18.8852611271086,4.56764174058429));
#99390=CARTESIAN_POINT('Ctrl Pts',(-9.58526020020486,18.8790321186293,4.60241222742192));
#99391=CARTESIAN_POINT('Ctrl Pts',(-9.59938864416844,18.8780418803422,4.60762463345889));
#99392=CARTESIAN_POINT('Ctrl Pts',(-9.61989816254569,18.8766012561321,4.61474747307565));
#99393=CARTESIAN_POINT('Ctrl Pts',(-9.62620196734435,18.8761580468056,4.61687705827065));
#99394=CARTESIAN_POINT('Ctrl Pts',(-9.6373245850552,18.8753751407942,4.62052984955988));
#99395=CARTESIAN_POINT('Ctrl Pts',(-9.64213583194315,18.8750361914398,4.6220756820367));
#99396=CARTESIAN_POINT('Ctrl Pts',(-9.65209505100026,18.8743338964638,4.62520496665753));
#99397=CARTESIAN_POINT('Ctrl Pts',(-9.6572442259448,18.8739704216939,4.62678416221276));
#99398=CARTESIAN_POINT('Ctrl Pts',(-9.67049407031553,18.8730340866274,4.63074851911867));
#99399=CARTESIAN_POINT('Ctrl Pts',(-9.67860977203029,18.8724595714423,4.63308194146854));
#99400=CARTESIAN_POINT('Ctrl Pts',(-9.71327889665108,18.8700005993182,4.64264756109201));
#99401=CARTESIAN_POINT('Ctrl Pts',(-9.7400544190049,18.8680894623986,4.64903460181142));
#99402=CARTESIAN_POINT('Ctrl Pts',(-9.86461801156321,18.8591365406619,4.67417144747533));
#99403=CARTESIAN_POINT('Ctrl Pts',(-9.96430280832018,18.8517505804295,4.6814087477441));
#99404=CARTESIAN_POINT('Ctrl Pts',(-10.0857480728976,18.8428856952671,4.67483212468812));
#99405=CARTESIAN_POINT('Ctrl Pts',(-10.1077738939043,18.8412856229628,4.6730166813751));
#99406=CARTESIAN_POINT('Ctrl Pts',(-10.1514651602569,18.8381413205625,4.66817434421005));
#99407=CARTESIAN_POINT('Ctrl Pts',(-10.1731242356884,18.8365972515551,4.6651614231081));
#99408=CARTESIAN_POINT('Ctrl Pts',(-10.2001302772772,18.834700256385,4.66063490373656));
#99409=CARTESIAN_POINT('Ctrl Pts',(-10.2055657377183,18.8343198982049,4.65968454250745));
#99410=CARTESIAN_POINT('Ctrl Pts',(-10.2141501693984,18.8337216848738,4.65812134779758));
#99411=CARTESIAN_POINT('Ctrl Pts',(-10.2173035754431,18.8335024722693,4.65753380425885));
#99412=CARTESIAN_POINT('Ctrl Pts',(-10.2229334788012,18.8331121072638,4.65646102162653));
#99413=CARTESIAN_POINT('Ctrl Pts',(-10.2254108042875,18.8329406875773,4.65598070918241));
#99414=CARTESIAN_POINT('Ctrl Pts',(-10.2313531203559,18.8325303323802,4.65480876341944));
#99415=CARTESIAN_POINT('Ctrl Pts',(-10.2348165623519,18.8322918296986,4.65410949620656));
#99416=CARTESIAN_POINT('Ctrl Pts',(-10.2453533072506,18.8315681358634,4.65193273691118));
#99417=CARTESIAN_POINT('Ctrl Pts',(-10.2524163685677,18.8310856323672,4.65040569326551));
#99418=CARTESIAN_POINT('Ctrl Pts',(-10.3160182104771,18.8267606377487,4.63604090874528));
#99419=CARTESIAN_POINT('Ctrl Pts',(-10.3715593550871,18.823123942058,4.61910768173727));
#99420=CARTESIAN_POINT('Ctrl Pts',(-10.5202983234554,18.813223346089,4.56145766405397));
#99421=CARTESIAN_POINT('Ctrl Pts',(-10.6098106009705,18.8070416696428,4.51268539316257));
#99422=CARTESIAN_POINT('Ctrl Pts',(-10.7028913304139,18.7995201414882,4.44510389920806));
#99423=CARTESIAN_POINT('Ctrl Pts',(-10.7136865113828,18.7986300456772,4.4369787306138));
#99424=CARTESIAN_POINT('Ctrl Pts',(-10.7294190037176,18.7973049374349,4.42470778231506));
#99425=CARTESIAN_POINT('Ctrl Pts',(-10.7344661477864,18.7968754764958,4.42070410047622));
#99426=CARTESIAN_POINT('Ctrl Pts',(-10.7433767940649,18.7961093418461,4.41351577453718));
#99427=CARTESIAN_POINT('Ctrl Pts',(-10.7472533439593,18.7957733249903,4.41034749788038));
#99428=CARTESIAN_POINT('Ctrl Pts',(-10.7553716924883,18.795063822142,4.403625635235));
#99429=CARTESIAN_POINT('Ctrl Pts',(-10.7596088723576,18.7946901248327,4.40006668735827));
#99430=CARTESIAN_POINT('Ctrl Pts',(-10.7707626785591,18.7936972858277,4.39056337769105));
#99431=CARTESIAN_POINT('Ctrl Pts',(-10.7776354929931,18.7930760874858,4.38456840788581));
#99432=CARTESIAN_POINT('Ctrl Pts',(-10.8103581004241,18.7900719979608,4.35534926663345));
#99433=CARTESIAN_POINT('Ctrl Pts',(-10.835238742274,18.7876454046907,4.33107065226259));
#99434=CARTESIAN_POINT('Ctrl Pts',(-10.9048710026018,18.7804148113205,4.25683404185184));
#99435=CARTESIAN_POINT('Ctrl Pts',(-10.9464709948768,18.7755028892511,4.20411652783334));
#99436=CARTESIAN_POINT('Ctrl Pts',(-11.0169651658191,18.7660974286231,4.09716521431976));
#99437=CARTESIAN_POINT('Ctrl Pts',(-11.0465600502645,18.7616219072534,4.04363409649131));
#99438=CARTESIAN_POINT('Ctrl Pts',(-11.07591263311,18.7566582786299,3.97916821893319));
#99439=CARTESIAN_POINT('Ctrl Pts',(-11.079843753822,18.7559801494676,3.97024212799605));
#99440=CARTESIAN_POINT('Ctrl Pts',(-11.0851130618404,18.755053222373,3.9578628619176));
#99441=CARTESIAN_POINT('Ctrl Pts',(-11.0865463955926,18.754799155459,3.95445097475492));
#99442=CARTESIAN_POINT('Ctrl Pts',(-11.088976609975,18.7543651107791,3.94858890074289));
#99443=CARTESIAN_POINT('Ctrl Pts',(-11.0899813505894,18.7541846739709,3.94614203418176));
#99444=CARTESIAN_POINT('Ctrl Pts',(-11.0920621805362,18.753808940854,3.94102555574889));
#99445=CARTESIAN_POINT('Ctrl Pts',(-11.0931367377496,18.7536137430793,3.9383553579045));
#99446=CARTESIAN_POINT('Ctrl Pts',(-11.095735887596,18.7531386639463,3.9318276639923));
#99447=CARTESIAN_POINT('Ctrl Pts',(-11.0972499313141,18.7528594044669,3.92796595225371));
#99448=CARTESIAN_POINT('Ctrl Pts',(-11.1026241811366,18.7518586802466,3.91404240908337));
#99449=CARTESIAN_POINT('Ctrl Pts',(-11.1063667861951,18.7511437810916,3.90393533656195));
#99450=CARTESIAN_POINT('Ctrl Pts',(-11.1153672716648,18.7493745207204,3.87856501475415));
#99451=CARTESIAN_POINT('Ctrl Pts',(-11.1204512141427,18.748328489135,3.86324200218918));
#99452=CARTESIAN_POINT('Ctrl Pts',(-11.1413644571401,18.7437884174297,3.79558610926651));
#99453=CARTESIAN_POINT('Ctrl Pts',(-11.1538549141785,18.740413466457,3.74228858262037));
#99454=CARTESIAN_POINT('Ctrl Pts',(-11.1755803216177,18.7320141907098,3.60816092981128));
#99455=CARTESIAN_POINT('Ctrl Pts',(-11.1802383611547,18.7269935158248,3.52689208966883));
#99456=CARTESIAN_POINT('Ctrl Pts',(-11.1758097141291,18.7207176887387,3.43076987753496));
#99457=CARTESIAN_POINT('Ctrl Pts',(-11.1748297292917,18.7197285818846,3.41576006086347));
#99458=CARTESIAN_POINT('Ctrl Pts',(-11.1730022794265,18.7182893089736,3.39414657671874));
#99459=CARTESIAN_POINT('Ctrl Pts',(-11.1723858354497,18.7178463004401,3.38752447135021));
#99460=CARTESIAN_POINT('Ctrl Pts',(-11.171202399141,18.7170636287478,3.37588096249331));
#99461=CARTESIAN_POINT('Ctrl Pts',(-11.1706591098427,18.7167247115129,3.37085727893159));
#99462=CARTESIAN_POINT('Ctrl Pts',(-11.1694698460921,18.7160223654719,3.36048526011253));
#99463=CARTESIAN_POINT('Ctrl Pts',(-11.1688194706839,18.7156588068009,3.35513755888353));
#99464=CARTESIAN_POINT('Ctrl Pts',(-11.1670547579532,18.7147220059634,3.34141356518546));
#99465=CARTESIAN_POINT('Ctrl Pts',(-11.1658869361227,18.7141471057273,3.33304458360342));
#99466=CARTESIAN_POINT('Ctrl Pts',(-11.1605248860396,18.7116841327672,3.29742329998767));
#99467=CARTESIAN_POINT('Ctrl Pts',(-11.1554646833515,18.7097692715863,3.2703122204667));
#99468=CARTESIAN_POINT('Ctrl Pts',(-11.1277763200773,18.7008148620037,3.14627752970873));
#99469=CARTESIAN_POINT('Ctrl Pts',(-11.0938723854304,18.6934317180553,3.05229889351215));
#99470=CARTESIAN_POINT('Ctrl Pts',(-11.038508177659,18.684569488207,2.94404656152457));
#99471=CARTESIAN_POINT('Ctrl Pts',(-11.0278929506242,18.6829691109619,2.92465693991007));
#99472=CARTESIAN_POINT('Ctrl Pts',(-11.005716907244,18.6798263932201,2.88672568408536));
#99473=CARTESIAN_POINT('Ctrl Pts',(-10.9941728908451,18.6782841594691,2.86818333644014));
#99474=CARTESIAN_POINT('Ctrl Pts',(-10.9790748709384,18.6763890838603,2.84537195195708));
#99475=CARTESIAN_POINT('Ctrl Pts',(-10.975998338465,18.6760088743706,2.8407938634256));
#99476=CARTESIAN_POINT('Ctrl Pts',(-10.9710821949622,18.675410842515,2.83358817629996));
#99477=CARTESIAN_POINT('Ctrl Pts',(-10.9692638662058,18.6751916640279,2.83094626043057));
#99478=CARTESIAN_POINT('Ctrl Pts',(-10.9659955094781,18.6748013278273,2.82623883564534));
#99479=CARTESIAN_POINT('Ctrl Pts',(-10.9645496424637,18.6746299030794,2.8241705700943));
#99480=CARTESIAN_POINT('Ctrl Pts',(-10.9610630005252,18.6742194947261,2.81921702394936));
#99481=CARTESIAN_POINT('Ctrl Pts',(-10.9590158753862,18.6739809442761,2.81633626464712));
#99482=CARTESIAN_POINT('Ctrl Pts',(-10.9527415398683,18.6732569595755,2.8075905209288));
#99483=CARTESIAN_POINT('Ctrl Pts',(-10.9484731699149,18.6727742161372,2.80175507095913));
#99484=CARTESIAN_POINT('Ctrl Pts',(-10.9094167634968,18.6684405517692,2.74937863374166));
#99485=CARTESIAN_POINT('Ctrl Pts',(-10.8712775981772,18.6647963288094,2.70542555772147));
#99486=CARTESIAN_POINT('Ctrl Pts',(-10.7581357391074,18.654898715298,2.59302750797585));
#99487=CARTESIAN_POINT('Ctrl Pts',(-10.6773159606229,18.6487264197648,2.5311811623224));
#99488=CARTESIAN_POINT('Ctrl Pts',(-10.5778650907643,18.6412146809033,2.4736715369355));
#99489=CARTESIAN_POINT('Ctrl Pts',(-10.5660352579006,18.6403232086952,2.46710008258104));
#99490=CARTESIAN_POINT('Ctrl Pts',(-10.5484068660871,18.6389964393599,2.45770132548734));
#99491=CARTESIAN_POINT('Ctrl Pts',(-10.5426938133542,18.6385667142219,2.45471533072383));
#99492=CARTESIAN_POINT('Ctrl Pts',(-10.5325002272042,18.6378002830893,2.4494936262581));
#99493=CARTESIAN_POINT('Ctrl Pts',(-10.5280293723009,18.6374642358056,2.44723928934207));
#99494=CARTESIAN_POINT('Ctrl Pts',(-10.5185895044334,18.6367548487033,2.44255468945364));
#99495=CARTESIAN_POINT('Ctrl Pts',(-10.5136174858364,18.6363812986923,2.44013079328625));
#99496=CARTESIAN_POINT('Ctrl Pts',(-10.5004117612855,18.6353892727026,2.43380764943514));
#99497=CARTESIAN_POINT('Ctrl Pts',(-10.4921497068448,18.634768746092,2.42996882420994));
#99498=CARTESIAN_POINT('Ctrl Pts',(-10.4522700580434,18.6317734955339,2.41199899021114));
#99499=CARTESIAN_POINT('Ctrl Pts',(-10.4200869578729,18.629355382189,2.39917261952027));
#99500=CARTESIAN_POINT('Ctrl Pts',(-10.3244694947015,18.622163450117,2.36586877007432));
#99501=CARTESIAN_POINT('Ctrl Pts',(-10.2598109262317,18.617283191258,2.34933474197101));
#99502=CARTESIAN_POINT('Ctrl Pts',(-10.1333286962355,18.6078670296911,2.32819967738834));
#99503=CARTESIAN_POINT('Ctrl Pts',(-10.0718379974637,18.60334922107,2.32282822438742));
#99504=CARTESIAN_POINT('Ctrl Pts',(-10.0004555369352,18.5983469949769,2.32220974012492));
#99505=CARTESIAN_POINT('Ctrl Pts',(-9.99070591637658,18.5976691275771,2.32224631639192));
#99506=CARTESIAN_POINT('Ctrl Pts',(-9.97725779336423,18.5967424908091,2.32246378151545));
#99507=CARTESIAN_POINT('Ctrl Pts',(-9.9735583399493,18.5964884568067,2.32254104387882));
#99508=CARTESIAN_POINT('Ctrl Pts',(-9.96721516235065,18.5960544536518,2.32270343043901));
#99509=CARTESIAN_POINT('Ctrl Pts',(-9.96457127696026,18.5958740256461,2.32278002726015));
#99510=CARTESIAN_POINT('Ctrl Pts',(-9.95905075738442,18.5954982941839,2.32295857883695));
#99511=CARTESIAN_POINT('Ctrl Pts',(-9.95617421059215,18.5953030893455,2.32306217325309));
#99512=CARTESIAN_POINT('Ctrl Pts',(-9.94915294860697,18.594827965752,2.32334081027488));
#99513=CARTESIAN_POINT('Ctrl Pts',(-9.94500866980837,18.594548669153,2.3235272097041));
#99514=CARTESIAN_POINT('Ctrl Pts',(-9.93009850332987,18.5935476615325,2.3242767919371));
#99515=CARTESIAN_POINT('Ctrl Pts',(-9.91933908790185,18.5928325209864,2.32496590735998));
#99516=CARTESIAN_POINT('Ctrl Pts',(-9.8924896088628,18.5910625418283,2.32705610623543));
#99517=CARTESIAN_POINT('Ctrl Pts',(-9.87641566395351,18.590016041537,2.32864060664368));
#99518=CARTESIAN_POINT('Ctrl Pts',(-9.84390287006405,18.5879168049108,2.33252234842891));
#99519=CARTESIAN_POINT('Ctrl Pts',(-9.82747438054779,18.5868652106325,2.33483690563033));
#99520=CARTESIAN_POINT('Ctrl Pts',(-9.81110405343086,18.5858217463839,2.33749693167298));
#99521=CARTESIAN_POINT('Ctrl Pts',(-9.81110406377177,18.4867244625755,2.33749692999267));
#99522=CARTESIAN_POINT('Ctrl Pts',(-9.81502055737344,18.4869959966987,2.33686053621041));
#99523=CARTESIAN_POINT('Ctrl Pts',(-9.81894023795535,18.4872681500725,2.33624393924982));
#99524=CARTESIAN_POINT('Ctrl Pts',(-9.89385327067581,18.4924773252704,2.32484715925569));
#99525=CARTESIAN_POINT('Ctrl Pts',(-9.96566935042106,18.4976187432309,2.32056398740546));
#99526=CARTESIAN_POINT('Ctrl Pts',(-10.1040909410058,18.5077366739403,2.32496377705408));
#99527=CARTESIAN_POINT('Ctrl Pts',(-10.1704651577274,18.5126783721553,2.33274383280967));
#99528=CARTESIAN_POINT('Ctrl Pts',(-10.2627546373824,18.519458288938,2.35160521263381));
#99529=CARTESIAN_POINT('Ctrl Pts',(-10.2894864562524,18.5214096712654,2.35805058846731));
#99530=CARTESIAN_POINT('Ctrl Pts',(-10.3214770335043,18.5237112106892,2.36695973018287));
#99531=CARTESIAN_POINT('Ctrl Pts',(-10.3269724690046,18.5241053510851,2.36853336596239));
#99532=CARTESIAN_POINT('Ctrl Pts',(-10.3355438439853,18.52471795289,2.37105547119819));
#99533=CARTESIAN_POINT('Ctrl Pts',(-10.3386276304222,18.5249379162887,2.37197661864078));
#99534=CARTESIAN_POINT('Ctrl Pts',(-10.3443887632108,18.5253479840531,2.37372326163712));
#99535=CARTESIAN_POINT('Ctrl Pts',(-10.3470669189619,18.5255382524336,2.37454566259372));
#99536=CARTESIAN_POINT('Ctrl Pts',(-10.3531874757884,18.5259722942019,2.37644907221503));
#99537=CARTESIAN_POINT('Ctrl Pts',(-10.3566278654057,18.5262157022643,2.3775363494232));
#99538=CARTESIAN_POINT('Ctrl Pts',(-10.365788068929,18.5268624058227,2.38047764490603));
#99539=CARTESIAN_POINT('Ctrl Pts',(-10.3714988641808,18.5272641421922,2.38235971234764));
#99540=CARTESIAN_POINT('Ctrl Pts',(-10.4206598832273,18.5307120300276,2.39897982194325));
#99541=CARTESIAN_POINT('Ctrl Pts',(-10.4632345790552,18.5336280476373,2.41620344913844));
#99542=CARTESIAN_POINT('Ctrl Pts',(-10.5675707820091,18.5408501776574,2.46568848325332));
#99543=CARTESIAN_POINT('Ctrl Pts',(-10.6276750261111,18.5450886544862,2.50101988983706));
#99544=CARTESIAN_POINT('Ctrl Pts',(-10.7237486399299,18.5524872091298,2.56960697826571));
#99545=CARTESIAN_POINT('Ctrl Pts',(-10.7614083264604,18.5555747416005,2.60016680463221));
#99546=CARTESIAN_POINT('Ctrl Pts',(-10.8053616510598,18.5594948062132,2.64057325024989));
#99547=CARTESIAN_POINT('Ctrl Pts',(-10.8135372415315,18.5602384564028,2.64830823095255));
#99548=CARTESIAN_POINT('Ctrl Pts',(-10.825893209441,18.5613856238808,2.66033854129972));
#99549=CARTESIAN_POINT('Ctrl Pts',(-10.8301538932381,18.5617855617628,2.66455073767223));
#99550=CARTESIAN_POINT('Ctrl Pts',(-10.8378556874318,18.5625166274357,2.67228197291186));
#99551=CARTESIAN_POINT('Ctrl Pts',(-10.8413072514379,18.5628472865883,2.67579044367144));
#99552=CARTESIAN_POINT('Ctrl Pts',(-10.8487944014127,18.5635712820222,2.68349706901601));
#99553=CARTESIAN_POINT('Ctrl Pts',(-10.8528210271905,18.5639649926084,2.68770370821696));
#99554=CARTESIAN_POINT('Ctrl Pts',(-10.8637983875353,18.5650504682649,2.69934341338896));
#99555=CARTESIAN_POINT('Ctrl Pts',(-10.870684098414,18.5657449585784,2.70683683051033));
#99556=CARTESIAN_POINT('Ctrl Pts',(-10.9084484904098,18.5696316474158,2.74901854771153));
#99557=CARTESIAN_POINT('Ctrl Pts',(-10.9373476628373,18.5729037524011,2.78541609221565));
#99558=CARTESIAN_POINT('Ctrl Pts',(-11.0157691935003,18.5827173171535,2.89715449260702));
#99559=CARTESIAN_POINT('Ctrl Pts',(-11.0588828810836,18.589431328629,2.97657406568185));
#99560=CARTESIAN_POINT('Ctrl Pts',(-11.1038949888336,18.5981322731122,3.08837147933389));
#99561=CARTESIAN_POINT('Ctrl Pts',(-11.1141687062613,18.6003001263911,3.11705007426972));
#99562=CARTESIAN_POINT('Ctrl Pts',(-11.1250854278307,18.6028192841211,3.15170076397929));
#99563=CARTESIAN_POINT('Ctrl Pts',(-11.1268088936171,18.6032245361751,3.15731749592413));
#99564=CARTESIAN_POINT('Ctrl Pts',(-11.129421210619,18.6038505474558,3.16606381979828));
#99565=CARTESIAN_POINT('Ctrl Pts',(-11.130339217603,18.6040729146079,3.16918449667144));
#99566=CARTESIAN_POINT('Ctrl Pts',(-11.1320223298029,18.6044850443882,3.17499488202908));
#99567=CARTESIAN_POINT('Ctrl Pts',(-11.132790780747,18.6046749889997,3.17768349532472));
#99568=CARTESIAN_POINT('Ctrl Pts',(-11.1345310839594,18.6051093144321,3.18385547681247));
#99569=CARTESIAN_POINT('Ctrl Pts',(-11.1354964741756,18.6053533235141,3.1873406038143));
#99570=CARTESIAN_POINT('Ctrl Pts',(-11.1379970917406,18.6059937498227,3.19653236892446));
#99571=CARTESIAN_POINT('Ctrl Pts',(-11.1395054718017,18.60638869319,3.20224629772624));
#99572=CARTESIAN_POINT('Ctrl Pts',(-11.1508483744507,18.6094291367701,3.24656361659155));
#99573=CARTESIAN_POINT('Ctrl Pts',(-11.1587627493247,18.6119768778465,3.28563672548265));
#99574=CARTESIAN_POINT('Ctrl Pts',(-11.1745999321648,18.6186788460379,3.39106246825286));
#99575=CARTESIAN_POINT('Ctrl Pts',(-11.1788863393335,18.6227485357035,3.4578101689625));
#99576=CARTESIAN_POINT('Ctrl Pts',(-11.1763743507372,18.6302551840462,3.57822763442844));
#99577=CARTESIAN_POINT('Ctrl Pts',(-11.1715878064183,18.6336496524675,3.63174654587664));
#99578=CARTESIAN_POINT('Ctrl Pts',(-11.1610285414453,18.6380502199837,3.69822726476439));
#99579=CARTESIAN_POINT('Ctrl Pts',(-11.1586536362071,18.6389491892219,3.71166730640503));
#99580=CARTESIAN_POINT('Ctrl Pts',(-11.1548099979576,18.640284915843,3.73141035471224));
#99581=CARTESIAN_POINT('Ctrl Pts',(-11.1535219576905,18.6407159882934,3.73774771074581));
#99582=CARTESIAN_POINT('Ctrl Pts',(-11.1511439275649,18.6414838361605,3.74897349756806));
#99583=CARTESIAN_POINT('Ctrl Pts',(-11.1500748159385,18.6418199428225,3.75386622634108));
#99584=CARTESIAN_POINT('Ctrl Pts',(-11.1477623265163,18.6425284436076,3.76413471612076));
#99585=CARTESIAN_POINT('Ctrl Pts',(-11.1465123149345,18.6429010414789,3.76950884278542));
#99586=CARTESIAN_POINT('Ctrl Pts',(-11.1431117781274,18.6438881791984,3.78367671499674));
#99587=CARTESIAN_POINT('Ctrl Pts',(-11.1408975798915,18.6445047347936,3.79245464631184));
#99588=CARTESIAN_POINT('Ctrl Pts',(-11.1308347400008,18.6471987270005,3.8304929793025));
#99589=CARTESIAN_POINT('Ctrl Pts',(-11.1219605915897,18.6493086129913,3.85946760637358));
#99590=CARTESIAN_POINT('Ctrl Pts',(-11.1049243392197,18.6529656890843,3.90828400259256));
#99591=CARTESIAN_POINT('Ctrl Pts',(-11.097318730925,18.6544958026373,3.92830495938168));
#99592=CARTESIAN_POINT('Ctrl Pts',(-11.0590716621276,18.661738715238,4.02126864099925));
#99593=CARTESIAN_POINT('Ctrl Pts',(-11.0216765370403,18.6676118806604,4.09121010438067));
#99594=CARTESIAN_POINT('Ctrl Pts',(-10.9632796359642,18.675219229617,4.17811713285849));
#99595=CARTESIAN_POINT('Ctrl Pts',(-10.948310777399,18.6770625051985,4.19889723598452));
#99596=CARTESIAN_POINT('Ctrl Pts',(-10.9265126280757,18.6795884986067,4.227166606161));
#99597=CARTESIAN_POINT('Ctrl Pts',(-10.9202470233905,18.6802976610222,4.235079828692));
#99598=CARTESIAN_POINT('Ctrl Pts',(-10.9091273343962,18.6815258159335,4.24875852338272));
#99599=CARTESIAN_POINT('Ctrl Pts',(-10.9043182775691,18.6820474202172,4.25455967076355));
#99600=CARTESIAN_POINT('Ctrl Pts',(-10.8971343272435,18.6828121752383,4.26305830031935));
#99601=CARTESIAN_POINT('Ctrl Pts',(-10.8948023497106,18.6830582247048,4.26579156865528));
#99602=CARTESIAN_POINT('Ctrl Pts',(-10.8906345538917,18.6834940222957,4.27063153426628));
#99603=CARTESIAN_POINT('Ctrl Pts',(-10.888803710323,18.6836841202136,4.27274241198857));
#99604=CARTESIAN_POINT('Ctrl Pts',(-10.8848145076174,18.6840954153674,4.27730884279825));
#99605=CARTESIAN_POINT('Ctrl Pts',(-10.8826534308083,18.6843164090719,4.27976193272126));
#99606=CARTESIAN_POINT('Ctrl Pts',(-10.8766367905957,18.6849267677561,4.28653450160242));
#99607=CARTESIAN_POINT('Ctrl Pts',(-10.8727594828177,18.6853145720274,4.29083466881437));
#99608=CARTESIAN_POINT('Ctrl Pts',(-10.8516009129125,18.6874022835756,4.31395564946696));
#99609=CARTESIAN_POINT('Ctrl Pts',(-10.8337409417213,18.6890626938121,4.33224045987523));
#99610=CARTESIAN_POINT('Ctrl Pts',(-10.7417289868374,18.6972153842518,4.42050316569943));
#99611=CARTESIAN_POINT('Ctrl Pts',(-10.6593045206666,18.7033143794301,4.48122825725592));
#99612=CARTESIAN_POINT('Ctrl Pts',(-10.5343347039392,18.7123381733835,4.55035731373159));
#99613=CARTESIAN_POINT('Ctrl Pts',(-10.4975850708971,18.7149628484845,4.56825680352153));
#99614=CARTESIAN_POINT('Ctrl Pts',(-10.4511744412744,18.7182843198107,4.58794679838419));
#99615=CARTESIAN_POINT('Ctrl Pts',(-10.4423212024537,18.718918141663,4.59157618035455));
#99616=CARTESIAN_POINT('Ctrl Pts',(-10.4281896357665,18.7199306696061,4.59716926685864));
#99617=CARTESIAN_POINT('Ctrl Pts',(-10.4229396223855,18.7203070103151,4.5992037291893));
#99618=CARTESIAN_POINT('Ctrl Pts',(-10.4130131019117,18.7210190101658,4.60296876801733));
#99619=CARTESIAN_POINT('Ctrl Pts',(-10.4083397843936,18.7213543914444,4.60470744757937));
#99620=CARTESIAN_POINT('Ctrl Pts',(-10.3977653591543,18.7221137387072,4.60856533178555));
#99621=CARTESIAN_POINT('Ctrl Pts',(-10.3918581246791,18.7225382662599,4.61066717933961));
#99622=CARTESIAN_POINT('Ctrl Pts',(-10.3766287179769,18.723633722796,4.61594932053755));
#99623=CARTESIAN_POINT('Ctrl Pts',(-10.367283081658,18.7243069031887,4.61905996482451));
#99624=CARTESIAN_POINT('Ctrl Pts',(-10.2968215911285,18.7293906041109,4.64153497498529));
#99625=CARTESIAN_POINT('Ctrl Pts',(-10.2342651864853,18.7339593222223,4.6559941543712));
#99626=CARTESIAN_POINT('Ctrl Pts',(-10.0977616799265,18.7440012761968,4.67600800968173));
#99627=CARTESIAN_POINT('Ctrl Pts',(-10.0238263296714,18.7494865150083,4.67982389078537));
#99628=CARTESIAN_POINT('Ctrl Pts',(-9.92197565711148,18.7568285137915,4.67549786391979));
#99629=CARTESIAN_POINT('Ctrl Pts',(-9.89397906443406,18.7588224902347,4.67330425855927));
#99630=CARTESIAN_POINT('Ctrl Pts',(-9.86037324027178,18.7611670542721,4.6694582011128));
#99631=CARTESIAN_POINT('Ctrl Pts',(-9.85466600859611,18.7615635127172,4.66876265790381));
#99632=CARTESIAN_POINT('Ctrl Pts',(-9.84576501136729,18.762178913902,4.66761167993822));
#99633=CARTESIAN_POINT('Ctrl Pts',(-9.84256773184522,18.7623993804826,4.66718488185244));
#99634=CARTESIAN_POINT('Ctrl Pts',(-9.8365979672755,18.7628098721468,4.66636301400065));
#99635=CARTESIAN_POINT('Ctrl Pts',(-9.83382515877768,18.7630000650292,4.66597119479821));
#99636=CARTESIAN_POINT('Ctrl Pts',(-9.82749393809585,18.763433291044,4.66505350054097));
#99637=CARTESIAN_POINT('Ctrl Pts',(-9.82393651613221,18.7636759639573,4.66452121106781));
#99638=CARTESIAN_POINT('Ctrl Pts',(-9.81447676026642,18.7643194060786,4.66306142855582));
#99639=CARTESIAN_POINT('Ctrl Pts',(-9.80857885794919,18.7647186408972,4.66210529175673));
#99640=CARTESIAN_POINT('Ctrl Pts',(-9.76152998911399,18.7678898094255,4.65411006628227));
#99641=CARTESIAN_POINT('Ctrl Pts',(-9.7207675095226,18.7705543393162,4.64493145833517));
#99642=CARTESIAN_POINT('Ctrl Pts',(-9.58546529319722,18.7793755946881,4.6068062064459));
#99643=CARTESIAN_POINT('Ctrl Pts',(-9.49411002172692,18.7853269760098,4.56814553588639));
#99644=CARTESIAN_POINT('Ctrl Pts',(-9.38403353477632,18.7934757884722,4.50423644223821));
#99645=CARTESIAN_POINT('Ctrl Pts',(-9.35994180850256,18.7953236019816,4.48905551956549));
#99646=CARTESIAN_POINT('Ctrl Pts',(-9.32936823217239,18.7977673232605,4.46820506888624));
#99647=CARTESIAN_POINT('Ctrl Pts',(-9.32236407467754,18.7983341394577,4.46331592417238));
#99648=CARTESIAN_POINT('Ctrl Pts',(-9.31101506381247,18.7992643805696,4.45520890034256));
#99649=CARTESIAN_POINT('Ctrl Pts',(-9.30663800994663,18.7996260733591,4.45203646709418));
#99650=CARTESIAN_POINT('Ctrl Pts',(-9.29822023225099,18.8003274248761,4.44584652645403));
#99651=CARTESIAN_POINT('Ctrl Pts',(-9.29417673734981,18.8006669261074,4.44283297278198));
#99652=CARTESIAN_POINT('Ctrl Pts',(-9.28488814777285,18.8014529345546,4.43581709221581));
#99653=CARTESIAN_POINT('Ctrl Pts',(-9.27965712295027,18.8019001466999,4.43179650551133));
#99654=CARTESIAN_POINT('Ctrl Pts',(-9.262843366865,18.8033526300943,4.41864718527559));
#99655=CARTESIAN_POINT('Ctrl Pts',(-9.25139863752396,18.8043646990453,4.40934510419292));
#99656=CARTESIAN_POINT('Ctrl Pts',(-9.17259011493072,18.8115030777121,4.34279474460592));
#99657=CARTESIAN_POINT('Ctrl Pts',(-9.1116970333334,18.8179338696165,4.2783458041946));
#99658=CARTESIAN_POINT('Ctrl Pts',(-9.01698953687469,18.8295073344187,4.15236460862125));
#99659=CARTESIAN_POINT('Ctrl Pts',(-8.98034050004862,18.8345957388571,4.09345243026744));
#99660=CARTESIAN_POINT('Ctrl Pts',(-8.94582230754721,18.8399185740493,4.02522039534986));
#99661=CARTESIAN_POINT('Ctrl Pts',(-8.94262590536818,18.8404174881118,4.01875533874997));
#99662=CARTESIAN_POINT('Ctrl Pts',(-8.93795373797049,18.8411554383152,4.00908276226169));
#99663=CARTESIAN_POINT('Ctrl Pts',(-8.93643275453944,18.8413970954451,4.00589745673323));
#99664=CARTESIAN_POINT('Ctrl Pts',(-8.93384947230673,18.8418099371504,4.00042429689303));
#99665=CARTESIAN_POINT('Ctrl Pts',(-8.93278018035464,18.8419815440292,3.99813982135499));
#99666=CARTESIAN_POINT('Ctrl Pts',(-8.93036758694839,18.8423703712356,3.99294203986458));
#99667=CARTESIAN_POINT('Ctrl Pts',(-8.92902884404964,18.8425873125774,3.99002667015233));
#99668=CARTESIAN_POINT('Ctrl Pts',(-8.92541806257408,18.8431757774832,3.98207802010986));
#99669=CARTESIAN_POINT('Ctrl Pts',(-8.9231694495525,18.8435459164192,3.97703409344848));
#99670=CARTESIAN_POINT('Ctrl Pts',(-8.91216807814261,18.8453762827659,3.95188239101155));
#99671=CARTESIAN_POINT('Ctrl Pts',(-8.90394201365645,18.8468076310177,3.93154724570624));
#99672=CARTESIAN_POINT('Ctrl Pts',(-8.88858831600686,18.8496364922881,3.89031522561151));
#99673=CARTESIAN_POINT('Ctrl Pts',(-8.88147077724173,18.8510331798768,3.86942439229194));
#99674=CARTESIAN_POINT('Ctrl Pts',(-8.84550770964435,18.8586603570588,3.75327382426828));
#99675=CARTESIAN_POINT('Ctrl Pts',(-8.82824092380558,18.8646545588853,3.65485873449201));
#99676=CARTESIAN_POINT('Ctrl Pts',(-8.8222610540194,18.8727964767225,3.52797128486702));
#99677=CARTESIAN_POINT('Ctrl Pts',(-8.82192911420155,18.8745830559791,3.50046485942088));
#99678=CARTESIAN_POINT('Ctrl Pts',(-8.82275382667612,18.8769568598176,3.46453515242739));
#99679=CARTESIAN_POINT('Ctrl Pts',(-8.82303822485137,18.8775170760411,3.45609918345885));
#99680=CARTESIAN_POINT('Ctrl Pts',(-8.82365249826855,18.8784392299313,3.44228861600316));
#99681=CARTESIAN_POINT('Ctrl Pts',(-8.82392860320771,18.8787994936257,3.43691183407034));
#99682=CARTESIAN_POINT('Ctrl Pts',(-8.82453522350282,18.879500034427,3.42649392786755));
#99683=CARTESIAN_POINT('Ctrl Pts',(-8.82486132861812,18.8798401669265,3.42145265709528));
#99684=CARTESIAN_POINT('Ctrl Pts',(-8.82569194610124,18.8806305231952,3.40977857875488));
#99685=CARTESIAN_POINT('Ctrl Pts',(-8.82622023479299,18.8810814766345,3.40314769007917));
#99686=CARTESIAN_POINT('Ctrl Pts',(-8.82812743760418,18.8825588522177,3.38152458153715));
#99687=CARTESIAN_POINT('Ctrl Pts',(-8.82973760723348,18.8835924014127,3.36655479477446));
#99688=CARTESIAN_POINT('Ctrl Pts',(-8.84178115992368,18.8902113239789,3.27172173876614));
#99689=CARTESIAN_POINT('Ctrl Pts',(-8.86009520994865,18.8960441044976,3.19308881839438));
#99690=CARTESIAN_POINT('Ctrl Pts',(-8.90422769455571,18.9060013798844,3.06477244706115));
#99691=CARTESIAN_POINT('Ctrl Pts',(-8.92582023411268,18.9100678746802,3.01391526458323));
#99692=CARTESIAN_POINT('Ctrl Pts',(-8.95827258610392,18.9151886538216,2.95030715282623));
#99693=CARTESIAN_POINT('Ctrl Pts',(-8.9659432582124,18.9163417535588,2.9360098035996));
#99694=CARTESIAN_POINT('Ctrl Pts',(-8.97921656770736,18.9182400549069,2.91245150531441));
#99695=CARTESIAN_POINT('Ctrl Pts',(-8.98465566548599,18.9189930110098,2.90310138838998));
#99696=CARTESIAN_POINT('Ctrl Pts',(-8.9923604750014,18.9200245784108,2.89026653646036));
#99697=CARTESIAN_POINT('Ctrl Pts',(-8.99451676711371,18.9203096297034,2.88671721155589));
#99698=CARTESIAN_POINT('Ctrl Pts',(-8.99819938561159,18.9207902369444,2.88072713822424));
#99699=CARTESIAN_POINT('Ctrl Pts',(-8.99971595529528,18.92098641062,2.87828046604329));
#99700=CARTESIAN_POINT('Ctrl Pts',(-9.00264202663417,18.9213615385439,2.87359827650141));
#99701=CARTESIAN_POINT('Ctrl Pts',(-9.00405009653638,18.9215405868746,2.8713619193993));
#99702=CARTESIAN_POINT('Ctrl Pts',(-9.00744427543182,18.9219687309554,2.86601116742432));
#99703=CARTESIAN_POINT('Ctrl Pts',(-9.00943754722302,18.922217363406,2.86290131512426));
#99704=CARTESIAN_POINT('Ctrl Pts',(-9.0167209687425,18.9231159823095,2.85165472198858));
#99705=CARTESIAN_POINT('Ctrl Pts',(-9.02209718810573,18.9237606189912,2.84357379824361));
#99706=CARTESIAN_POINT('Ctrl Pts',(-9.0652349927705,18.9287964916085,2.78044038299123));
#99707=CARTESIAN_POINT('Ctrl Pts',(-9.10752085595098,18.9329318063801,2.72861481815714));
#99708=CARTESIAN_POINT('Ctrl Pts',(-9.19818303686321,18.9409909211741,2.63500154558711));
#99709=CARTESIAN_POINT('Ctrl Pts',(-9.24600791555207,18.9449037011179,2.59301157438885));
#99710=CARTESIAN_POINT('Ctrl Pts',(-9.31446399144532,18.9503384853983,2.54208032239438));
#99711=CARTESIAN_POINT('Ctrl Pts',(-9.33230027919226,18.9517401450621,2.52956364287481));
#99712=CARTESIAN_POINT('Ctrl Pts',(-9.36363722912782,18.9541873266529,2.5088458527334));
#99713=CARTESIAN_POINT('Ctrl Pts',(-9.37697488287497,18.9552242628136,2.50040819097376));
#99714=CARTESIAN_POINT('Ctrl Pts',(-9.39634012117295,18.9567254000042,2.48869551760604));
#99715=CARTESIAN_POINT('Ctrl Pts',(-9.40223341988969,18.9571816534026,2.48520094709104));
#99716=CARTESIAN_POINT('Ctrl Pts',(-9.41253599520039,18.9579784413068,2.47921267536463));
#99717=CARTESIAN_POINT('Ctrl Pts',(-9.41693153481843,18.9583181277069,2.4766956060828));
#99718=CARTESIAN_POINT('Ctrl Pts',(-9.42544709363859,18.9589757781765,2.47189192079601));
#99719=CARTESIAN_POINT('Ctrl Pts',(-9.42956487466947,18.9592935992385,2.46960151814644));
#99720=CARTESIAN_POINT('Ctrl Pts',(-9.43937487471307,18.9600503650681,2.46422180172666));
#99721=CARTESIAN_POINT('Ctrl Pts',(-9.44507900074691,18.960490081181,2.46115463672748));
#99722=CARTESIAN_POINT('Ctrl Pts',(-9.46549734818217,18.9620631627094,2.45039164019521));
#99723=CARTESIAN_POINT('Ctrl Pts',(-9.48034808147334,18.9632056552988,2.44296044141348));
#99724=CARTESIAN_POINT('Ctrl Pts',(-9.59547369030641,18.9720544317322,2.38836486407111));
#99725=CARTESIAN_POINT('Ctrl Pts',(-9.70177990851533,18.9802562432334,2.35526108830259));
#99726=CARTESIAN_POINT('Ctrl Pts',(-9.81110406455739,18.9883401336252,2.33749692986502));
#99727=CARTESIAN_POINT('Origin',(-10.,12.3756328852638,3.5));
#99728=CARTESIAN_POINT('',(-9.81110406371044,19.5876476368634,2.33749693000264));
#99729=CARTESIAN_POINT('',(-9.81110408816073,19.4882767440992,2.3374969260297));
#99730=CARTESIAN_POINT('',(-9.81110406371068,12.3756328852638,2.3374969300026));
#99731=CARTESIAN_POINT('Ctrl Pts',(-9.8111040637102,19.5876476368634,2.33749693000268));
#99732=CARTESIAN_POINT('Ctrl Pts',(-9.8106956841937,19.5876198932078,2.33756328787572));
#99733=CARTESIAN_POINT('Ctrl Pts',(-9.81028733975649,19.5875921427914,2.33762986092192));
#99734=CARTESIAN_POINT('Ctrl Pts',(-9.80493802576696,19.5872284921535,2.33850486206574));
#99735=CARTESIAN_POINT('Ctrl Pts',(-9.80000229175874,19.5868916146335,2.33934456249868));
#99736=CARTESIAN_POINT('Ctrl Pts',(-9.78872733839253,19.5861189224998,2.34133678830245));
#99737=CARTESIAN_POINT('Ctrl Pts',(-9.78239196873605,19.5856824678243,2.34250990606972));
#99738=CARTESIAN_POINT('Ctrl Pts',(-9.76279833730254,19.5843253753953,2.34630459606175));
#99739=CARTESIAN_POINT('Ctrl Pts',(-9.74957574175851,19.5833992200025,2.34910235978295));
#99740=CARTESIAN_POINT('Ctrl Pts',(-9.63747226563818,19.5754557336399,2.37484558205097));
#99741=CARTESIAN_POINT('Ctrl Pts',(-9.5419103071493,19.5680207909528,2.4102550182968));
#99742=CARTESIAN_POINT('Ctrl Pts',(-9.40074895210856,19.5563221770524,2.48444220930991));
#99743=CARTESIAN_POINT('Ctrl Pts',(-9.35146172340673,19.5520928430861,2.51518572825358));
#99744=CARTESIAN_POINT('Ctrl Pts',(-9.29880367410118,19.5475510424629,2.55370670596388));
#99745=CARTESIAN_POINT('Ctrl Pts',(-9.29301033178312,19.5470510838542,2.55802712279558));
#99746=CARTESIAN_POINT('Ctrl Pts',(-9.28444403644062,19.5463118476351,2.56453903857251));
#99747=CARTESIAN_POINT('Ctrl Pts',(-9.28164071803438,19.5460699368752,2.56669003531547));
#99748=CARTESIAN_POINT('Ctrl Pts',(-9.27685198211089,19.5456567631575,2.57039880882308));
#99749=CARTESIAN_POINT('Ctrl Pts',(-9.27486184923668,19.5454850764904,2.57195038216381));
#99750=CARTESIAN_POINT('Ctrl Pts',(-9.27035342446886,19.5450962002686,2.57548865583267));
#99751=CARTESIAN_POINT('Ctrl Pts',(-9.26783825203655,19.5448792890736,2.57747925436928));
#99752=CARTESIAN_POINT('Ctrl Pts',(-9.2610189228686,19.5442911838022,2.582921774973));
#99753=CARTESIAN_POINT('Ctrl Pts',(-9.25673077265675,19.5439213709027,2.58639375996656));
#99754=CARTESIAN_POINT('Ctrl Pts',(-9.23557728067456,19.542096179599,2.60376861916769));
#99755=CARTESIAN_POINT('Ctrl Pts',(-9.21907561138594,19.5406694813505,2.61810996780136));
#99756=CARTESIAN_POINT('Ctrl Pts',(-9.18672714268573,19.5378441526877,2.64784405864006));
#99757=CARTESIAN_POINT('Ctrl Pts',(-9.17089530889,19.5364465145444,2.66323958178222));
#99758=CARTESIAN_POINT('Ctrl Pts',(-9.08614423523973,19.5288190174745,2.75042365757527));
#99759=CARTESIAN_POINT('Ctrl Pts',(-9.02610783460518,19.5228259078037,2.83027498617237));
#99760=CARTESIAN_POINT('Ctrl Pts',(-8.96317202482156,19.5146813445591,2.94067642200042));
#99761=CARTESIAN_POINT('Ctrl Pts',(-8.95036472393774,19.5128905146499,2.96509747489161));
#99762=CARTESIAN_POINT('Ctrl Pts',(-8.93476737401636,19.5105117359612,2.99756004217785));
#99763=CARTESIAN_POINT('Ctrl Pts',(-8.9311901870933,19.5099509362705,3.005215161584));
#99764=CARTESIAN_POINT('Ctrl Pts',(-8.92546779331963,19.5090279861705,3.017812671825));
#99765=CARTESIAN_POINT('Ctrl Pts',(-8.92327354130888,19.5086675143326,3.02273255489377));
#99766=CARTESIAN_POINT('Ctrl Pts',(-8.91908664987462,19.5079666853692,3.03229611386409));
#99767=CARTESIAN_POINT('Ctrl Pts',(-8.91708998819997,19.5076264737208,3.03693790852968));
#99768=CARTESIAN_POINT('Ctrl Pts',(-8.91253458106892,19.5068361042433,3.04771882609351));
#99769=CARTESIAN_POINT('Ctrl Pts',(-8.90999786629261,19.5063852177268,3.05386701198037));
#99770=CARTESIAN_POINT('Ctrl Pts',(-8.9018941803872,19.5049088100926,3.07398950644592));
#99771=CARTESIAN_POINT('Ctrl Pts',(-8.89654302512441,19.5038761768603,3.08804854676251));
#99772=CARTESIAN_POINT('Ctrl Pts',(-8.86405164042408,19.4972156703019,3.17859259323325));
#99773=CARTESIAN_POINT('Ctrl Pts',(-8.84461417871865,19.4913361910959,3.25759442138906));
#99774=CARTESIAN_POINT('Ctrl Pts',(-8.82592424551814,19.481367545464,3.39213844431413));
#99775=CARTESIAN_POINT('Ctrl Pts',(-8.82218128266783,19.4773368932779,3.44678689843661));
#99776=CARTESIAN_POINT('Ctrl Pts',(-8.82227151734088,19.4722560852462,3.51764721967909));
#99777=CARTESIAN_POINT('Ctrl Pts',(-8.8226241623562,19.471108453926,3.53379342039898));
#99778=CARTESIAN_POINT('Ctrl Pts',(-8.82376574628731,19.4692181209239,3.56069795752622));
#99779=CARTESIAN_POINT('Ctrl Pts',(-8.82437058131702,19.4684677444576,3.57146154421775));
#99780=CARTESIAN_POINT('Ctrl Pts',(-8.82541272043861,19.4674390344187,3.58635388213993));
#99781=CARTESIAN_POINT('Ctrl Pts',(-8.82572416375481,19.46715430793,3.5904905077468));
#99782=CARTESIAN_POINT('Ctrl Pts',(-8.82628871929852,19.4666740387315,3.59749449619904));
#99783=CARTESIAN_POINT('Ctrl Pts',(-8.82653049699069,19.4664778808321,3.60036270930273));
#99784=CARTESIAN_POINT('Ctrl Pts',(-8.8270146263591,19.4661026144689,3.60586487455948));
#99785=CARTESIAN_POINT('Ctrl Pts',(-8.8272553379598,19.465923412848,3.60849892372828));
#99786=CARTESIAN_POINT('Ctrl Pts',(-8.82785408274519,19.4654946782989,3.61481595411492));
#99787=CARTESIAN_POINT('Ctrl Pts',(-8.8282206059166,19.4652456111362,3.61849813155037));
#99788=CARTESIAN_POINT('Ctrl Pts',(-8.82961591937848,19.4643435867982,3.63187579482989));
#99789=CARTESIAN_POINT('Ctrl Pts',(-8.83074777237364,19.4636960328355,3.64156046360809));
#99790=CARTESIAN_POINT('Ctrl Pts',(-8.83986891074685,19.4590182895021,3.71200592541082));
#99791=CARTESIAN_POINT('Ctrl Pts',(-8.85247072763083,19.4552027831496,3.77208311552354));
#99792=CARTESIAN_POINT('Ctrl Pts',(-8.88848401559368,19.4472677703029,3.8950944265588));
#99793=CARTESIAN_POINT('Ctrl Pts',(-8.91270515660466,19.4431630858671,3.95755512088264));
#99794=CARTESIAN_POINT('Ctrl Pts',(-8.95734718434812,19.4367056664832,4.0487936943912));
#99795=CARTESIAN_POINT('Ctrl Pts',(-8.97396849734466,19.4344649549755,4.07927403435532));
#99796=CARTESIAN_POINT('Ctrl Pts',(-8.99662360531662,19.4315754526703,4.11677708979781));
#99797=CARTESIAN_POINT('Ctrl Pts',(-9.00142761265321,19.4309711195921,4.12452489734398));
#99798=CARTESIAN_POINT('Ctrl Pts',(-9.00929092582271,19.4299947460041,4.13688397979329));
#99799=CARTESIAN_POINT('Ctrl Pts',(-9.01229369565801,19.4296247819132,4.14153092517949));
#99800=CARTESIAN_POINT('Ctrl Pts',(-9.01807594630742,19.4289177066454,4.15034243516118));
#99801=CARTESIAN_POINT('Ctrl Pts',(-9.0208494668279,19.428580822163,4.15451078084832));
#99802=CARTESIAN_POINT('Ctrl Pts',(-9.02725319283781,19.4278080698531,4.16400318888897));
#99803=CARTESIAN_POINT('Ctrl Pts',(-9.03090065749793,19.4273715616076,4.16931535705772));
#99804=CARTESIAN_POINT('Ctrl Pts',(-9.04233491616776,19.4260141346446,4.1856787962801));
#99805=CARTESIAN_POINT('Ctrl Pts',(-9.05026829596698,19.4250876943656,4.19662578785773));
#99806=CARTESIAN_POINT('Ctrl Pts',(-9.11934078999104,19.4171460840526,4.28856304071154));
#99807=CARTESIAN_POINT('Ctrl Pts',(-9.19051208496895,19.4097136085619,4.36145986912364));
#99808=CARTESIAN_POINT('Ctrl Pts',(-9.3156602931893,19.3980154833449,4.4602819690286));
#99809=CARTESIAN_POINT('Ctrl Pts',(-9.36380281102323,19.3937842799183,4.49283283272144));
#99810=CARTESIAN_POINT('Ctrl Pts',(-9.42042395604104,19.3892407118303,4.52529942222084));
#99811=CARTESIAN_POINT('Ctrl Pts',(-9.42672680911896,19.3887407039534,4.52883679518127));
#99812=CARTESIAN_POINT('Ctrl Pts',(-9.43615921276475,19.3880014094091,4.5340169800198));
#99813=CARTESIAN_POINT('Ctrl Pts',(-9.43926409502501,19.3877594890015,4.53570400888317));
#99814=CARTESIAN_POINT('Ctrl Pts',(-9.44459929430523,19.387346304537,4.53857184951618));
#99815=CARTESIAN_POINT('Ctrl Pts',(-9.44682585963015,19.3871746167073,4.53975949207676));
#99816=CARTESIAN_POINT('Ctrl Pts',(-9.4518911353612,19.386785745604,4.54244041680038));
#99817=CARTESIAN_POINT('Ctrl Pts',(-9.45473213902915,19.3865688406419,4.54392926507899));
#99818=CARTESIAN_POINT('Ctrl Pts',(-9.46247619763173,19.3859807688938,4.5479473558097));
#99819=CARTESIAN_POINT('Ctrl Pts',(-9.46739107478083,19.3856109830224,4.55045382307065));
#99820=CARTESIAN_POINT('Ctrl Pts',(-9.49185942519379,19.3837861421393,4.56271620129751));
#99821=CARTESIAN_POINT('Ctrl Pts',(-9.51166557592804,19.3823597541224,4.57196184925302));
#99822=CARTESIAN_POINT('Ctrl Pts',(-9.55197741244406,19.3795346594245,4.58943025924289));
#99823=CARTESIAN_POINT('Ctrl Pts',(-9.57247968743308,19.3781369562045,4.59763792233992));
#99824=CARTESIAN_POINT('Ctrl Pts',(-9.68657886661173,19.3705098470289,4.63963272065532));
#99825=CARTESIAN_POINT('Ctrl Pts',(-9.78393132078789,19.3645171930309,4.66202855537848));
#99826=CARTESIAN_POINT('Ctrl Pts',(-9.91038484356188,19.3563725682798,4.67465943783982));
#99827=CARTESIAN_POINT('Ctrl Pts',(-9.93791331513044,19.3545810991138,4.67643560114346));
#99828=CARTESIAN_POINT('Ctrl Pts',(-9.97392420066801,19.35220158984,4.6774916260664));
#99829=CARTESIAN_POINT('Ctrl Pts',(-9.98237349828021,19.3516407202029,4.6776484097632));
#99830=CARTESIAN_POINT('Ctrl Pts',(-9.9962106758143,19.3507176844233,4.67775622527403));
#99831=CARTESIAN_POINT('Ctrl Pts',(-10.0015979264835,19.3503571974653,4.67776123647286));
#99832=CARTESIAN_POINT('Ctrl Pts',(-10.0120377878676,19.3496563601732,4.67769931912421));
#99833=CARTESIAN_POINT('Ctrl Pts',(-10.0170903147317,19.3493161554538,4.67763683467039));
#99834=CARTESIAN_POINT('Ctrl Pts',(-10.0287914029237,19.348525833177,4.67741681019818));
#99835=CARTESIAN_POINT('Ctrl Pts',(-10.0354392901257,19.3480749872009,4.67723546641299));
#99836=CARTESIAN_POINT('Ctrl Pts',(-10.0571144547687,19.3465988506789,4.67646044123919));
#99837=CARTESIAN_POINT('Ctrl Pts',(-10.0721314311017,19.3455664516452,4.67563525421626));
#99838=CARTESIAN_POINT('Ctrl Pts',(-10.1681915179273,19.3388972049503,4.66850936938903));
#99839=CARTESIAN_POINT('Ctrl Pts',(-10.2484001980322,19.3330078572726,4.65412101550457));
#99840=CARTESIAN_POINT('Ctrl Pts',(-10.378943439907,19.3230366994419,4.61645828905838));
#99841=CARTESIAN_POINT('Ctrl Pts',(-10.4302987607397,19.3190135001058,4.59768884080807));
#99842=CARTESIAN_POINT('Ctrl Pts',(-10.4948981918747,19.3139410300771,4.56884567133155));
#99843=CARTESIAN_POINT('Ctrl Pts',(-10.509492291535,19.3127945597147,4.56196654809367));
#99844=CARTESIAN_POINT('Ctrl Pts',(-10.5335882617895,19.3109059301653,4.54999745630386));
#99845=CARTESIAN_POINT('Ctrl Pts',(-10.5431695788278,19.3101561128229,4.54507316522657));
#99846=CARTESIAN_POINT('Ctrl Pts',(-10.5563444570962,19.3091280350536,4.53807182093451));
#99847=CARTESIAN_POINT('Ctrl Pts',(-10.5599962784974,19.308843391771,4.53610637954867));
#99848=CARTESIAN_POINT('Ctrl Pts',(-10.5661648144221,19.3083632215399,4.53274428045651));
#99849=CARTESIAN_POINT('Ctrl Pts',(-10.5686869078735,19.3081670799818,4.53135762342437));
#99850=CARTESIAN_POINT('Ctrl Pts',(-10.5735172639854,19.3077918122062,4.52867876801562));
#99851=CARTESIAN_POINT('Ctrl Pts',(-10.5758262801741,19.3076125930233,4.5273880256599));
#99852=CARTESIAN_POINT('Ctrl Pts',(-10.581355634832,19.3071837737372,4.52427261408499));
#99853=CARTESIAN_POINT('Ctrl Pts',(-10.5845717841478,19.3069346398103,4.52244050791106));
#99854=CARTESIAN_POINT('Ctrl Pts',(-10.5962349840046,19.306032021093,4.51572344655203));
#99855=CARTESIAN_POINT('Ctrl Pts',(-10.6046301645907,19.305383949116,4.51074856188911));
#99856=CARTESIAN_POINT('Ctrl Pts',(-10.6661152699253,19.30064226317,4.47327295082016));
#99857=CARTESIAN_POINT('Ctrl Pts',(-10.716623094347,19.2967702573103,4.43670870784371));
#99858=CARTESIAN_POINT('Ctrl Pts',(-10.8143475464967,19.2888226885183,4.35340978179612));
#99859=CARTESIAN_POINT('Ctrl Pts',(-10.8609793736319,19.2847604850198,4.30633991809418));
#99860=CARTESIAN_POINT('Ctrl Pts',(-10.9180482090711,19.2791042454602,4.23810768157349));
#99861=CARTESIAN_POINT('Ctrl Pts',(-10.9321715940122,19.2776387399431,4.22018850604801));
#99862=CARTESIAN_POINT('Ctrl Pts',(-10.9555064872461,19.2750902707694,4.18874495398788));
#99863=CARTESIAN_POINT('Ctrl Pts',(-10.9649731051117,19.2740169116794,4.17541773927282));
#99864=CARTESIAN_POINT('Ctrl Pts',(-10.9780641416069,19.2724723249141,4.15615080749571));
#99865=CARTESIAN_POINT('Ctrl Pts',(-10.9819183274051,19.272009704083,4.15036892769035));
#99866=CARTESIAN_POINT('Ctrl Pts',(-10.988502919933,19.2712053595044,4.14029905347018));
#99867=CARTESIAN_POINT('Ctrl Pts',(-10.9912571751282,19.270864529619,4.1360268170144));
#99868=CARTESIAN_POINT('Ctrl Pts',(-10.9964996931501,19.2702072068537,4.12777816656594));
#99869=CARTESIAN_POINT('Ctrl Pts',(-10.9989920303147,19.2698908720284,4.12380444622677));
#99870=CARTESIAN_POINT('Ctrl Pts',(-11.0048226328033,19.2691416252343,4.11438371758833));
#99871=CARTESIAN_POINT('Ctrl Pts',(-11.0081404187772,19.2687079784874,4.10892427202413));
#99872=CARTESIAN_POINT('Ctrl Pts',(-11.0179275779915,19.2674064757458,4.09252016356392));
#99873=CARTESIAN_POINT('Ctrl Pts',(-11.0242641416544,19.2665339038608,4.08149775954924));
#99874=CARTESIAN_POINT('Ctrl Pts',(-11.0770612804849,19.2589972112251,3.98611622593119));
#99875=CARTESIAN_POINT('Ctrl Pts',(-11.11318201831,19.2519617598073,3.89646999741244));
#99876=CARTESIAN_POINT('Ctrl Pts',(-11.1539854625533,19.2403363299881,3.74345152269383));
#99877=CARTESIAN_POINT('Ctrl Pts',(-11.1652165621076,19.2357946717337,3.68227247097775));
#99878=CARTESIAN_POINT('Ctrl Pts',(-11.1723214424347,19.23095863704,3.61318722314911));
#99879=CARTESIAN_POINT('Ctrl Pts',(-11.1730039452346,19.2304508412068,3.60588041934202));
#99880=CARTESIAN_POINT('Ctrl Pts',(-11.1739156800366,19.2297023343447,3.59502462347152));
#99881=CARTESIAN_POINT('Ctrl Pts',(-11.1741971916666,19.2294588954618,3.59148037398434));
#99882=CARTESIAN_POINT('Ctrl Pts',(-11.1746711335742,19.2290258525456,3.58515037969062));
#99883=CARTESIAN_POINT('Ctrl Pts',(-11.1748697107118,19.2288359170841,3.58236517840755));
#99884=CARTESIAN_POINT('Ctrl Pts',(-11.1752812898076,19.2284227988759,3.57628784343758));
#99885=CARTESIAN_POINT('Ctrl Pts',(-11.1754903662571,19.2281998343281,3.57299551176822));
#99886=CARTESIAN_POINT('Ctrl Pts',(-11.1760358612897,19.2275789522069,3.56379451391262));
#99887=CARTESIAN_POINT('Ctrl Pts',(-11.1763415874712,19.2271826826438,3.55788402425024));
#99888=CARTESIAN_POINT('Ctrl Pts',(-11.177818798241,19.2249537298614,3.5244407718917));
#99889=CARTESIAN_POINT('Ctrl Pts',(-11.1780683239467,19.2231671307076,3.49687343688583));
#99890=CARTESIAN_POINT('Ctrl Pts',(-11.174745672095,19.21503415865,3.36936469083023));
#99891=CARTESIAN_POINT('Ctrl Pts',(-11.1594230897485,19.2090437502883,3.27014359740419));
#99892=CARTESIAN_POINT('Ctrl Pts',(-11.1205102474291,19.2001577518134,3.13503425940814));
#99893=CARTESIAN_POINT('Ctrl Pts',(-11.1072660814476,19.1975490029927,3.09663356699073));
#99894=CARTESIAN_POINT('Ctrl Pts',(-11.0884899344784,19.1942452733048,3.05013781052806));
#99895=CARTESIAN_POINT('Ctrl Pts',(-11.0848052020531,19.1936124253297,3.04132365256052));
#99896=CARTESIAN_POINT('Ctrl Pts',(-11.078779855658,19.1926010132917,3.02738941586182));
#99897=CARTESIAN_POINT('Ctrl Pts',(-11.0765090010053,19.1922248043069,3.02223948457464));
#99898=CARTESIAN_POINT('Ctrl Pts',(-11.0721559538404,19.1915127770178,3.01255609618663));
#99899=CARTESIAN_POINT('Ctrl Pts',(-11.0700816941445,19.1911772347577,3.00801919218443));
#99900=CARTESIAN_POINT('Ctrl Pts',(-11.0653318691927,19.1904171469972,2.99780233908241));
#99901=CARTESIAN_POINT('Ctrl Pts',(-11.0626395993961,19.1899920366627,2.9921303697872));
#99902=CARTESIAN_POINT('Ctrl Pts',(-11.0555969307692,19.1888943205306,2.97759433637464));
#99903=CARTESIAN_POINT('Ctrl Pts',(-11.0511802517357,19.1882194487497,2.96876311719355));
#99904=CARTESIAN_POINT('Ctrl Pts',(-11.0122489782288,19.1823828447992,2.89330628667435));
#99905=CARTESIAN_POINT('Ctrl Pts',(-10.9715577346623,19.1770001176065,2.83007690835861));
#99906=CARTESIAN_POINT('Ctrl Pts',(-10.8916610612483,19.1675561888095,2.72866209896345));
#99907=CARTESIAN_POINT('Ctrl Pts',(-10.8552950529299,19.1635605183903,2.68852475031126));
#99908=CARTESIAN_POINT('Ctrl Pts',(-10.7986896225448,19.1578623575284,2.63409775587127));
#99909=CARTESIAN_POINT('Ctrl Pts',(-10.7805569078029,19.1561059836174,2.61771723405829));
#99910=CARTESIAN_POINT('Ctrl Pts',(-10.7510466058762,19.1533698256869,2.59268107189906));
#99911=CARTESIAN_POINT('Ctrl Pts',(-10.7399990531984,19.1523711640608,2.58364849076324));
#99912=CARTESIAN_POINT('Ctrl Pts',(-10.725035338242,19.1510552117457,2.57186118516298));
#99913=CARTESIAN_POINT('Ctrl Pts',(-10.7212631507058,19.1507265161419,2.56892676403983));
#99914=CARTESIAN_POINT('Ctrl Pts',(-10.715321813714,19.1502136896766,2.56436271741215));
#99915=CARTESIAN_POINT('Ctrl Pts',(-10.7131647712895,19.1500285031694,2.56271752864176));
#99916=CARTESIAN_POINT('Ctrl Pts',(-10.7087431876435,19.1496509701811,2.55936926227273));
#99917=CARTESIAN_POINT('Ctrl Pts',(-10.7064781762765,19.1494586809308,2.55766689679374));
#99918=CARTESIAN_POINT('Ctrl Pts',(-10.7010840180038,19.1490033158699,2.55364306811529));
#99919=CARTESIAN_POINT('Ctrl Pts',(-10.6979494210103,19.1487407401611,2.55132890334686));
#99920=CARTESIAN_POINT('Ctrl Pts',(-10.6873697325875,19.1478611352126,2.54359910624135));
#99921=CARTESIAN_POINT('Ctrl Pts',(-10.679872411318,19.1472487570888,2.53825505659178));
#99922=CARTESIAN_POINT('Ctrl Pts',(-10.6615627362757,19.1457774943533,2.52552514797931));
#99923=CARTESIAN_POINT('Ctrl Pts',(-10.6506881834625,19.1449237666295,2.51823046994007));
#99924=CARTESIAN_POINT('Ctrl Pts',(-10.6075625500915,19.14160654792,2.4903330989449));
#99925=CARTESIAN_POINT('Ctrl Pts',(-10.574434766068,19.1392053375714,2.47112456541489));
#99926=CARTESIAN_POINT('Ctrl Pts',(-10.4591552371363,19.1311387053694,2.41158898337292));
#99927=CARTESIAN_POINT('Ctrl Pts',(-10.3732759380905,19.1255777229304,2.37922963955132));
#99928=CARTESIAN_POINT('Ctrl Pts',(-10.2622037901675,19.118203443365,2.35157801345508));
#99929=CARTESIAN_POINT('Ctrl Pts',(-10.2397321174924,19.1167044416958,2.3466777185466));
#99930=CARTESIAN_POINT('Ctrl Pts',(-10.2090874968363,19.1146437741221,2.34092947517724));
#99931=CARTESIAN_POINT('Ctrl Pts',(-10.2010270943222,19.1141002450309,2.33950434530639));
#99932=CARTESIAN_POINT('Ctrl Pts',(-10.188220260191,19.1132339742015,2.33737744326176));
#99933=CARTESIAN_POINT('Ctrl Pts',(-10.1834831654121,19.1129129720343,2.33662043913711));
#99934=CARTESIAN_POINT('Ctrl Pts',(-10.1737767020248,19.1122539802591,2.33513007075103));
#99935=CARTESIAN_POINT('Ctrl Pts',(-10.1688070082855,19.1119159098104,2.33439951662607));
#99936=CARTESIAN_POINT('Ctrl Pts',(-10.1573281499135,19.1111334316065,2.33278705375207));
#99937=CARTESIAN_POINT('Ctrl Pts',(-10.1508160280395,19.1106883260799,2.33192777137197));
#99938=CARTESIAN_POINT('Ctrl Pts',(-10.1302187937222,19.1092765389521,2.32938505497077));
#99939=CARTESIAN_POINT('Ctrl Pts',(-10.1161107285061,19.1083036794701,2.32790164581325));
#99940=CARTESIAN_POINT('Ctrl Pts',(-10.0048866778155,19.1005846743167,2.31823459263072));
#99941=CARTESIAN_POINT('Ctrl Pts',(-9.90717910965791,19.0934618621443,2.3218856286421));
#99942=CARTESIAN_POINT('Ctrl Pts',(-9.81110406371067,19.0863176770662,2.3374969300026));
#99943=CARTESIAN_POINT('Ctrl Pts',(-9.81110406455739,18.9883401336252,2.33749692986502));
#99944=CARTESIAN_POINT('Ctrl Pts',(-9.81189205314573,18.9883984008336,2.33736888904918));
#99945=CARTESIAN_POINT('Ctrl Pts',(-9.81268019879629,18.9884566579951,2.337241645059));
#99946=CARTESIAN_POINT('Ctrl Pts',(-9.81924205121837,18.9889415058973,2.33618909697252));
#99947=CARTESIAN_POINT('Ctrl Pts',(-9.82502247354454,18.9893674370338,2.33530599702566));
#99948=CARTESIAN_POINT('Ctrl Pts',(-9.84362289189887,18.99073382975,2.33260593164355));
#99949=CARTESIAN_POINT('Ctrl Pts',(-9.8564666697997,18.9916709747609,2.33095726650433));
#99950=CARTESIAN_POINT('Ctrl Pts',(-9.89543850473922,18.9944909464256,2.32660670646343));
#99951=CARTESIAN_POINT('Ctrl Pts',(-9.92163423104744,18.9963545400001,2.32456647167613));
#99952=CARTESIAN_POINT('Ctrl Pts',(-9.95371076337799,18.9985811855376,2.32314552655112));
#99953=CARTESIAN_POINT('Ctrl Pts',(-9.95954506704566,18.9989839461617,2.3229305258247));
#99954=CARTESIAN_POINT('Ctrl Pts',(-9.96865956607076,18.9996094102215,2.32266249580014));
#99955=CARTESIAN_POINT('Ctrl Pts',(-9.97193869398526,18.999833678247,2.32257977537113));
#99956=CARTESIAN_POINT('Ctrl Pts',(-9.97801059692306,19.0002475003697,2.32245198411027));
#99957=CARTESIAN_POINT('Ctrl Pts',(-9.98080317409126,19.00043725048,2.32240314804824));
#99958=CARTESIAN_POINT('Ctrl Pts',(-9.98717328333599,19.0008687997829,2.3223144149104));
#99959=CARTESIAN_POINT('Ctrl Pts',(-9.9907508414021,19.0011102454604,2.32228088412237));
#99960=CARTESIAN_POINT('Ctrl Pts',(-10.0017848540761,19.0018522371462,2.32222774932222));
#99961=CARTESIAN_POINT('Ctrl Pts',(-10.0092415629017,19.0023498924901,2.32226265204395));
#99962=CARTESIAN_POINT('Ctrl Pts',(-10.0266543470689,19.0035042382997,2.32250954841646));
#99963=CARTESIAN_POINT('Ctrl Pts',(-10.0366092002199,19.0041582419678,2.32277699695217));
#99964=CARTESIAN_POINT('Ctrl Pts',(-10.0716330933409,19.0064420711815,2.3241626748515));
#99965=CARTESIAN_POINT('Ctrl Pts',(-10.0966699822243,19.0080438064635,2.32595579348566));
#99966=CARTESIAN_POINT('Ctrl Pts',(-10.1747248343379,19.0129927559335,2.33406023796024));
#99967=CARTESIAN_POINT('Ctrl Pts',(-10.2273836816288,19.0162690350865,2.34317613279208));
#99968=CARTESIAN_POINT('Ctrl Pts',(-10.3519219515578,19.0242051509125,2.37357084010858));
#99969=CARTESIAN_POINT('Ctrl Pts',(-10.422733662362,19.0288827843279,2.39818979955342));
#99970=CARTESIAN_POINT('Ctrl Pts',(-10.4996716100713,19.0344432753646,2.43345410417092));
#99971=CARTESIAN_POINT('Ctrl Pts',(-10.5085637795759,19.0350932894676,2.43766543013439));
#99972=CARTESIAN_POINT('Ctrl Pts',(-10.5230315928306,19.0361635387493,2.44474065366962));
#99973=CARTESIAN_POINT('Ctrl Pts',(-10.528639100796,19.036581506668,2.44753858329002));
#99974=CARTESIAN_POINT('Ctrl Pts',(-10.5386674645924,19.0373348131293,2.45264271372318));
#99975=CARTESIAN_POINT('Ctrl Pts',(-10.543096540745,19.0376695747316,2.45493250521958));
#99976=CARTESIAN_POINT('Ctrl Pts',(-10.5524977666803,19.0383846159816,2.45986875564176));
#99977=CARTESIAN_POINT('Ctrl Pts',(-10.5574657228561,19.0387651586176,2.46252289008022));
#99978=CARTESIAN_POINT('Ctrl Pts',(-10.5708294608431,19.0397962109814,2.46978617697981));
#99979=CARTESIAN_POINT('Ctrl Pts',(-10.5791882178002,19.0404490692031,2.47446219307755));
#99980=CARTESIAN_POINT('Ctrl Pts',(-10.623021682264,19.0439157895418,2.49969011879592));
#99981=CARTESIAN_POINT('Ctrl Pts',(-10.6574583371417,19.0467914741873,2.52197969869417));
#99982=CARTESIAN_POINT('Ctrl Pts',(-10.7741743438869,19.0570929373783,2.60647913381633));
#99983=CARTESIAN_POINT('Ctrl Pts',(-10.8493761760381,19.0648120420495,2.67763645828133));
#99984=CARTESIAN_POINT('Ctrl Pts',(-10.9297271778065,19.0739596454404,2.77660689621544));
#99985=CARTESIAN_POINT('Ctrl Pts',(-10.9445128290272,19.0756872975698,2.79602136036394));
#99986=CARTESIAN_POINT('Ctrl Pts',(-10.9620032069501,19.0777745941901,2.82053145164619));
#99987=CARTESIAN_POINT('Ctrl Pts',(-10.9652867901641,19.0781684705743,2.82520440544327));
#99988=CARTESIAN_POINT('Ctrl Pts',(-10.9703861706662,19.0787831210101,2.83257486354273));
#99989=CARTESIAN_POINT('Ctrl Pts',(-10.972224956786,19.0790053761679,2.83525623955779));
#99990=CARTESIAN_POINT('Ctrl Pts',(-10.9756097071975,19.0794155940427,2.84023607698023));
#99991=CARTESIAN_POINT('Ctrl Pts',(-10.9771586579055,19.0796037487341,2.84253236397246));
#99992=CARTESIAN_POINT('Ctrl Pts',(-10.9807042762711,19.0800354588645,2.84782887810893));
#99993=CARTESIAN_POINT('Ctrl Pts',(-10.9826952859495,19.0802786385019,2.85083282155834));
#99994=CARTESIAN_POINT('Ctrl Pts',(-10.9888376573041,19.0810313860975,2.86019316497468));
#99995=CARTESIAN_POINT('Ctrl Pts',(-10.9929414709376,19.0815379411159,2.86658075384337));
#99996=CARTESIAN_POINT('Ctrl Pts',(-11.0024086577133,19.0827162764613,2.88163457344487));
#99997=CARTESIAN_POINT('Ctrl Pts',(-11.0077219599714,19.083385213998,2.8903317419825));
#99998=CARTESIAN_POINT('Ctrl Pts',(-11.0261747808898,19.0857400634209,2.92143704458738));
#99999=CARTESIAN_POINT('Ctrl Pts',(-11.0386859046591,19.0873959575151,2.94421087642474));
#100000=CARTESIAN_POINT('Ctrl Pts',(-11.0872208888072,19.0941554969275,
3.0399319193915));
#100001=CARTESIAN_POINT('Ctrl Pts',(-11.1163928819923,19.0990817094154,
3.11609928607263));
#100002=CARTESIAN_POINT('Ctrl Pts',(-11.1495653537033,19.1071215196411,
3.23967973298724));
#100003=CARTESIAN_POINT('Ctrl Pts',(-11.1589641652929,19.1100998799162,
3.28536444107205));
#100004=CARTESIAN_POINT('Ctrl Pts',(-11.1670888008747,19.1138350786317,
3.34156223592039));
#100005=CARTESIAN_POINT('Ctrl Pts',(-11.1684152444552,19.1145089297948,
3.35166052435051));
#100006=CARTESIAN_POINT('Ctrl Pts',(-11.1702941776619,19.1155745987537,
3.36755932671859));
#100007=CARTESIAN_POINT('Ctrl Pts',(-11.170934896874,19.1159636613248,3.37334906465146));
#100008=CARTESIAN_POINT('Ctrl Pts',(-11.1720376680692,19.1166839252601,
3.38403884597848));
#100009=CARTESIAN_POINT('Ctrl Pts',(-11.1725120074326,19.1170147355265,
3.3889375140874));
#100010=CARTESIAN_POINT('Ctrl Pts',(-11.1734954831971,19.1177502579421,
3.39980377255104));
#100011=CARTESIAN_POINT('Ctrl Pts',(-11.1739898273686,19.1181554216222,
3.4057725304668));
#100012=CARTESIAN_POINT('Ctrl Pts',(-11.1752812159359,19.1193253778963,
3.42295740986853));
#100013=CARTESIAN_POINT('Ctrl Pts',(-11.1759631689081,19.1200937140982,
3.43418125401113));
#100014=CARTESIAN_POINT('Ctrl Pts',(-11.180261697679,19.1264723334255,3.52682481585399));
#100015=CARTESIAN_POINT('Ctrl Pts',(-11.1755778781871,19.1323450055113,
3.60839299785585));
#100016=CARTESIAN_POINT('Ctrl Pts',(-11.1499528239173,19.1440623183262,
3.76616913206904));
#100017=CARTESIAN_POINT('Ctrl Pts',(-11.1296970892666,19.1498658833319,
3.84208768647109));
#100018=CARTESIAN_POINT('Ctrl Pts',(-11.0987993056824,19.1559965644812,
3.92405180790112));
#100019=CARTESIAN_POINT('Ctrl Pts',(-11.0954502411605,19.1566362585339,
3.93262990214132));
#100020=CARTESIAN_POINT('Ctrl Pts',(-11.0906453688245,19.1575196343418,
3.94452315474922));
#100021=CARTESIAN_POINT('Ctrl Pts',(-11.0892744744104,19.1577679723586,
3.94787194142619));
#100022=CARTESIAN_POINT('Ctrl Pts',(-11.0868832168156,19.1581947722519,
3.95363731753049));
#100023=CARTESIAN_POINT('Ctrl Pts',(-11.0858701841215,19.1583736607045,
3.95605688947068));
#100024=CARTESIAN_POINT('Ctrl Pts',(-11.083721164944,19.1587491081053,3.96114194573337));
#100025=CARTESIAN_POINT('Ctrl Pts',(-11.0825834118613,19.1589455538531,
3.96380665598274));
#100026=CARTESIAN_POINT('Ctrl Pts',(-11.0797533432997,19.1594285713811,
3.97036775556322));
#100027=CARTESIAN_POINT('Ctrl Pts',(-11.078049737449,19.1597144709575,3.9742592885987));
#100028=CARTESIAN_POINT('Ctrl Pts',(-11.0716717933705,19.1607673729671,
3.98861641891627));
#100029=CARTESIAN_POINT('Ctrl Pts',(-11.0668656263564,19.1615268752339,
3.99902324307275));
#100030=CARTESIAN_POINT('Ctrl Pts',(-11.0312913900265,19.1669245297216,
4.07318820303578));
#100031=CARTESIAN_POINT('Ctrl Pts',(-10.9949777285771,19.1712856660638,
4.13413615058105));
#100032=CARTESIAN_POINT('Ctrl Pts',(-10.9062645758237,19.1806261689906,
4.25645646733281));
#100033=CARTESIAN_POINT('Ctrl Pts',(-10.8526083893289,19.1855944090477,
4.31645497100776));
#100034=CARTESIAN_POINT('Ctrl Pts',(-10.7821386835598,19.1918123534832,
4.3806707465737));
#100035=CARTESIAN_POINT('Ctrl Pts',(-10.7708136174569,19.1928027293023,
4.39059992010049));
#100036=CARTESIAN_POINT('Ctrl Pts',(-10.754216055974,19.1942434285033,4.4045979567811));
#100037=CARTESIAN_POINT('Ctrl Pts',(-10.7490942725793,19.1946865722762,
4.40884382059606));
#100038=CARTESIAN_POINT('Ctrl Pts',(-10.740020354648,19.1954693100076,4.41623711978447));
#100039=CARTESIAN_POINT('Ctrl Pts',(-10.7360833913643,19.195808156552,4.41940297180304));
#100040=CARTESIAN_POINT('Ctrl Pts',(-10.727909268596,19.1965101862807,4.42588991865983));
#100041=CARTESIAN_POINT('Ctrl Pts',(-10.7236694693532,19.196873498213,4.42920748073001));
#100042=CARTESIAN_POINT('Ctrl Pts',(-10.7127254324685,19.1978093005164,
4.4376506481061));
#100043=CARTESIAN_POINT('Ctrl Pts',(-10.7059886753529,19.1983834432181,
4.4427334001706));
#100044=CARTESIAN_POINT('Ctrl Pts',(-10.6770794744032,19.2008396919502,
4.46406117779448));
#100045=CARTESIAN_POINT('Ctrl Pts',(-10.6543982050937,19.2027484090674,
4.47959856084791));
#100046=CARTESIAN_POINT('Ctrl Pts',(-10.5471510794701,19.2116978575062,
4.54767869105495));
#100047=CARTESIAN_POINT('Ctrl Pts',(-10.4566890148157,19.2190828585621,
4.59015326009959));
#100048=CARTESIAN_POINT('Ctrl Pts',(-10.340971990513,19.2279465635238,4.62752867021513));
#100049=CARTESIAN_POINT('Ctrl Pts',(-10.3197684044419,19.2295459706809,
4.63372442043447));
#100050=CARTESIAN_POINT('Ctrl Pts',(-10.2771986240006,19.2326938566424,
4.64487397446374));
#100051=CARTESIAN_POINT('Ctrl Pts',(-10.2558424465414,19.2342420526977,
4.64983489589336));
#100052=CARTESIAN_POINT('Ctrl Pts',(-10.2289477544548,19.2361432800371,
4.65529583793001));
#100053=CARTESIAN_POINT('Ctrl Pts',(-10.2235290632786,19.2365238901828,
4.65635647976024));
#100054=CARTESIAN_POINT('Ctrl Pts',(-10.2149506867973,19.2371223656953,
4.65797303707202));
#100055=CARTESIAN_POINT('Ctrl Pts',(-10.2117959303673,19.2373415910549,
4.65855420108203));
#100056=CARTESIAN_POINT('Ctrl Pts',(-10.2061562914261,19.2377318951477,
4.6595693202563));
#100057=CARTESIAN_POINT('Ctrl Pts',(-10.203672401958,19.2379032416432,4.66000818007255));
#100058=CARTESIAN_POINT('Ctrl Pts',(-10.1977088844212,19.2383133090819,
4.66104208397579));
#100059=CARTESIAN_POINT('Ctrl Pts',(-10.1942279711302,19.238551598389,4.66162946751131));
#100060=CARTESIAN_POINT('Ctrl Pts',(-10.1836263616881,19.2392742405756,
4.66336943969752));
#100061=CARTESIAN_POINT('Ctrl Pts',(-10.1764975080296,19.2397559163239,
4.6644722968057));
#100062=CARTESIAN_POINT('Ctrl Pts',(-10.1000787943225,19.24487822132,4.67557660500358));
#100063=CARTESIAN_POINT('Ctrl Pts',(-10.0300279354252,19.2492174251588,
4.67944794843017));
#100064=CARTESIAN_POINT('Ctrl Pts',(-9.87253636059848,19.2589635532404,
4.67410120691841));
#100065=CARTESIAN_POINT('Ctrl Pts',(-9.78564878657044,19.2643509490355,
4.6613836431938));
#100066=CARTESIAN_POINT('Ctrl Pts',(-9.68666921420075,19.2710279244627,
4.63540199575862));
#100067=CARTESIAN_POINT('Ctrl Pts',(-9.67243424658421,19.2720009560114,
4.63137726623645));
#100068=CARTESIAN_POINT('Ctrl Pts',(-9.65195794905035,19.2734209275381,
4.62516906585841));
#100069=CARTESIAN_POINT('Ctrl Pts',(-9.64565288833514,19.2738609775836,
4.62319936674547));
#100070=CARTESIAN_POINT('Ctrl Pts',(-9.63456289316034,19.2746401117231,
4.61963218417606));
#100071=CARTESIAN_POINT('Ctrl Pts',(-9.62977098717978,19.2749784700321,
4.61805678908035));
#100072=CARTESIAN_POINT('Ctrl Pts',(-9.61986804955209,19.2756813199378,
4.61473043841932));
#100073=CARTESIAN_POINT('Ctrl Pts',(-9.61475865923405,19.2760459514584,
4.6129750032105));
#100074=CARTESIAN_POINT('Ctrl Pts',(-9.60161688723282,19.2769890731157,
4.60835854370644));
#100075=CARTESIAN_POINT('Ctrl Pts',(-9.59360329032413,19.2775692657825,
4.60544537343507));
#100076=CARTESIAN_POINT('Ctrl Pts',(-9.55911100241798,19.2800891552865,
4.59248070731796));
#100077=CARTESIAN_POINT('Ctrl Pts',(-9.53297002011803,19.282057214737,4.58156366614755));
#100078=CARTESIAN_POINT('Ctrl Pts',(-9.41739377314355,19.291031086042,4.5283250180462));
#100079=CARTESIAN_POINT('Ctrl Pts',(-9.33311981038472,19.2983720385527,
4.47578042561953));
#100080=CARTESIAN_POINT('Ctrl Pts',(-9.22399339261876,19.3086266919065,
4.38693711660613));
#100081=CARTESIAN_POINT('Ctrl Pts',(-9.19298993233208,19.3116360642708,
4.35882434508971));
#100082=CARTESIAN_POINT('Ctrl Pts',(-9.15933723269075,19.3149582852632,
4.32487386684008));
#100083=CARTESIAN_POINT('Ctrl Pts',(-9.15516192169255,19.3153715039879,
4.32059698373091));
#100084=CARTESIAN_POINT('Ctrl Pts',(-9.14852579976048,19.3160296539579,
4.31369508497761));
#100085=CARTESIAN_POINT('Ctrl Pts',(-9.14604421024184,19.3162760874644,
4.3110903248079));
#100086=CARTESIAN_POINT('Ctrl Pts',(-9.14165218840433,19.3167127365933,
4.30643780861967));
#100087=CARTESIAN_POINT('Ctrl Pts',(-9.13973707864857,19.3169033025763,
4.30439456214863));
#100088=CARTESIAN_POINT('Ctrl Pts',(-9.13563206034962,19.3173121280907,
4.29998345552619));
#100089=CARTESIAN_POINT('Ctrl Pts',(-9.13344458219608,19.3175302068904,
4.29761342310487));
#100090=CARTESIAN_POINT('Ctrl Pts',(-9.12738613400547,19.3181349269486,
4.29099502872505));
#100091=CARTESIAN_POINT('Ctrl Pts',(-9.12353641936397,19.3185200185641,
4.28672720161164));
#100092=CARTESIAN_POINT('Ctrl Pts',(-9.10109168705945,19.3207713531377,
4.26147553435145));
#100093=CARTESIAN_POINT('Ctrl Pts',(-9.08321782752752,19.3225894053749,
4.23985936974546));
#100094=CARTESIAN_POINT('Ctrl Pts',(-9.02377539867595,19.3288093216091,
4.16250486355738));
#100095=CARTESIAN_POINT('Ctrl Pts',(-8.98637983303266,19.3330498770526,
4.10374059260751));
#100096=CARTESIAN_POINT('Ctrl Pts',(-8.92289268753821,19.3416065426909,
3.98126634574884));
#100097=CARTESIAN_POINT('Ctrl Pts',(-8.89675967625481,19.3459060019001,
3.91789513571142));
#100098=CARTESIAN_POINT('Ctrl Pts',(-8.87331662572205,19.3510497775196,
3.84318706946664));
#100099=CARTESIAN_POINT('Ctrl Pts',(-8.87047577616379,19.3517028384361,
3.83371815737684));
#100100=CARTESIAN_POINT('Ctrl Pts',(-8.86602549038059,19.3527770910535,
3.81817656162913));
#100101=CARTESIAN_POINT('Ctrl Pts',(-8.86434480985467,19.3531959862849,
3.81212465354827));
#100102=CARTESIAN_POINT('Ctrl Pts',(-8.86141659599306,19.3539503062828,
3.8012437021625));
#100103=CARTESIAN_POINT('Ctrl Pts',(-8.86015116890268,19.3542851476251,
3.79641959602214));
#100104=CARTESIAN_POINT('Ctrl Pts',(-8.8575241666918,19.3549996511248,3.78613922601779));
#100105=CARTESIAN_POINT('Ctrl Pts',(-8.8561709585977,19.3553795717486,3.78068097282013));
#100106=CARTESIAN_POINT('Ctrl Pts',(-8.85262845543941,19.356407177706,3.76594086858718));
#100107=CARTESIAN_POINT('Ctrl Pts',(-8.85051276119721,19.3570571846646,
3.75664193998796));
#100108=CARTESIAN_POINT('Ctrl Pts',(-8.84003089837772,19.3604783991102,
3.70783947056981));
#100109=CARTESIAN_POINT('Ctrl Pts',(-8.83358840206345,19.3633094933184,
3.66795498321577));
#100110=CARTESIAN_POINT('Ctrl Pts',(-8.81852289871263,19.373227556442,3.52996194804202));
#100111=CARTESIAN_POINT('Ctrl Pts',(-8.82015097849112,19.3805780282818,
3.43116287313408));
#100112=CARTESIAN_POINT('Ctrl Pts',(-8.83816885235124,19.3897844807032,
3.30481785220476));
#100113=CARTESIAN_POINT('Ctrl Pts',(-8.84336530088836,19.3918622349192,
3.27607102820146));
#100114=CARTESIAN_POINT('Ctrl Pts',(-8.85080117627748,19.3942692306733,
3.2421876559134));
#100115=CARTESIAN_POINT('Ctrl Pts',(-8.85201421312623,19.3946479314441,
3.23683887587118));
#100116=CARTESIAN_POINT('Ctrl Pts',(-8.85405992311323,19.395264236073,3.22810190695853));
#100117=CARTESIAN_POINT('Ctrl Pts',(-8.85487034871994,19.3955030285681,
3.22470867182289));
#100118=CARTESIAN_POINT('Ctrl Pts',(-8.85635549481777,19.3959310993064,
3.21861044826831));
#100119=CARTESIAN_POINT('Ctrl Pts',(-8.85702474919731,19.3961206771046,
3.21590422284104));
#100120=CARTESIAN_POINT('Ctrl Pts',(-8.85851961687754,19.3965369076787,
3.20995030462312));
#100121=CARTESIAN_POINT('Ctrl Pts',(-8.8593494833124,19.3967633158958,3.20670374989398));
#100122=CARTESIAN_POINT('Ctrl Pts',(-8.86178819406716,19.3974155310039,
3.1973300872187));
#100123=CARTESIAN_POINT('Ctrl Pts',(-8.86343266070185,19.3978393693575,
3.19121224289695));
#100124=CARTESIAN_POINT('Ctrl Pts',(-8.87650110290369,19.4010902412087,
3.14411349228073));
#100125=CARTESIAN_POINT('Ctrl Pts',(-8.89009007724601,19.4038051561101,
3.10376038917526));
#100126=CARTESIAN_POINT('Ctrl Pts',(-8.93993899352409,19.4122573436673,
2.97859678174298));
#100127=CARTESIAN_POINT('Ctrl Pts',(-8.98397580591143,19.4178218437441,
2.89726785762434));
#100128=CARTESIAN_POINT('Ctrl Pts',(-9.05616615819369,19.4258006561304,
2.79475139607661));
#100129=CARTESIAN_POINT('Ctrl Pts',(-9.07642483797551,19.4279459191167,
2.76842190042464));
#100130=CARTESIAN_POINT('Ctrl Pts',(-9.10377315968961,19.4307504735862,
2.73582736488738));
#100131=CARTESIAN_POINT('Ctrl Pts',(-9.10986371034737,19.4313696457649,
2.72874145510258));
#100132=CARTESIAN_POINT('Ctrl Pts',(-9.11972598759326,19.432364172045,2.71753985613129));
#100133=CARTESIAN_POINT('Ctrl Pts',(-9.12344386744931,19.4327373060001,
2.71337711810091));
#100134=CARTESIAN_POINT('Ctrl Pts',(-9.13020912907082,19.433413179582,2.70590988668082));
#100135=CARTESIAN_POINT('Ctrl Pts',(-9.13324612572637,19.4337154805079,
2.70259609501179));
#100136=CARTESIAN_POINT('Ctrl Pts',(-9.14045126032815,19.4344301393493,
2.6948240717936));
#100137=CARTESIAN_POINT('Ctrl Pts',(-9.14463519707527,19.4348431627808,
2.69038072977618));
#100138=CARTESIAN_POINT('Ctrl Pts',(-9.1570069699288,19.4360588763551,2.67744484957506));
#100139=CARTESIAN_POINT('Ctrl Pts',(-9.16528788553141,19.436865553463,2.66904278535773));
#100140=CARTESIAN_POINT('Ctrl Pts',(-9.23184320565395,19.4432961410119,
2.60351260582741));
#100141=CARTESIAN_POINT('Ctrl Pts',(-9.29577479141901,19.4491820735364,
2.55246819079272));
#100142=CARTESIAN_POINT('Ctrl Pts',(-9.42952397745353,19.4608305441315,
2.4667402010071));
#100143=CARTESIAN_POINT('Ctrl Pts',(-9.49854672400978,19.4665502601415,
2.43153600752212));
#100144=CARTESIAN_POINT('Ctrl Pts',(-9.57913666983085,19.4726083671997,
2.39997516681611));
#100145=CARTESIAN_POINT('Ctrl Pts',(-9.58778703949948,19.4732508394052,
2.39670445265449));
#100146=CARTESIAN_POINT('Ctrl Pts',(-9.5998811357328,19.474137421021,2.39229376684017));
#100147=CARTESIAN_POINT('Ctrl Pts',(-9.60329267978202,19.4743862293026,
2.39106740173889));
#100148=CARTESIAN_POINT('Ctrl Pts',(-9.60918399340608,19.4748136188465,
2.38898028778154));
#100149=CARTESIAN_POINT('Ctrl Pts',(-9.61166105268762,19.4749926293477,
2.38811204957746));
#100150=CARTESIAN_POINT('Ctrl Pts',(-9.61687680755017,19.4753680790314,
2.38630342265884));
#100151=CARTESIAN_POINT('Ctrl Pts',(-9.61961610212526,19.4755644062718,
2.38536484107397));
#100152=CARTESIAN_POINT('Ctrl Pts',(-9.62637404986326,19.4760467066566,
2.38307713733145));
#100153=CARTESIAN_POINT('Ctrl Pts',(-9.63039662931669,19.4763320121143,
2.38173957347419));
#100154=CARTESIAN_POINT('Ctrl Pts',(-9.64526308204525,19.4773801894911,
2.37688525269519));
#100155=CARTESIAN_POINT('Ctrl Pts',(-9.65615104800831,19.4781356484528,
2.37350413285198));
#100156=CARTESIAN_POINT('Ctrl Pts',(-9.71437430520808,19.4821192942717,
2.35634650847987));
#100157=CARTESIAN_POINT('Ctrl Pts',(-9.76247520181581,19.4852151258987,
2.34539866670362));
#100158=CARTESIAN_POINT('Ctrl Pts',(-9.81110408825476,19.4882767425658,
2.33749692601442));
#100159=CARTESIAN_POINT('Origin',(-10.,12.3756328852638,3.5));
#100160=CARTESIAN_POINT('',(-9.8111040599147,20.0861209582704,2.33749693061941));
#100161=CARTESIAN_POINT('',(-9.81110406371628,19.9867190062194,2.33749693000169));
#100162=CARTESIAN_POINT('',(-9.81110406371068,12.3756328852638,2.3374969300026));
#100163=CARTESIAN_POINT('Ctrl Pts',(-9.81110405611873,20.0861209582704,
2.33749693123622));
#100164=CARTESIAN_POINT('Ctrl Pts',(-9.80339163817242,20.0856358825423,
2.33875012747004));
#100165=CARTESIAN_POINT('Ctrl Pts',(-9.79569045090659,20.0851515754612,
2.34008027521026));
#100166=CARTESIAN_POINT('Ctrl Pts',(-9.72214789657499,20.0805229996855,
2.35353796094226));
#100167=CARTESIAN_POINT('Ctrl Pts',(-9.65744542390395,20.0764141432507,
2.37118082151058));
#100168=CARTESIAN_POINT('Ctrl Pts',(-9.56199150098702,20.0699509916069,
2.40617670742513));
#100169=CARTESIAN_POINT('Ctrl Pts',(-9.52993660473754,20.0677089904062,
2.41956449393576));
#100170=CARTESIAN_POINT('Ctrl Pts',(-9.49027198717962,20.0648180321093,
2.43822999119953));
#100171=CARTESIAN_POINT('Ctrl Pts',(-9.48206748339353,20.0642135890124,
2.4422079130821));
#100172=CARTESIAN_POINT('Ctrl Pts',(-9.46895979841029,20.0632370802572,
2.44875217871409));
#100173=CARTESIAN_POINT('Ctrl Pts',(-9.4640269681909,20.0628670920651,2.45125857101962));
#100174=CARTESIAN_POINT('Ctrl Pts',(-9.45466459853784,20.0621599987673,
2.45609893704234));
#100175=CARTESIAN_POINT('Ctrl Pts',(-9.45023191161884,20.0618231205514,
2.45842658588255));
#100176=CARTESIAN_POINT('Ctrl Pts',(-9.44012898191428,20.0610504224013,
2.46381419629831));
#100177=CARTESIAN_POINT('Ctrl Pts',(-9.43446878019102,20.0606139623696,
2.46689254516296));
#100178=CARTESIAN_POINT('Ctrl Pts',(-9.41701465362454,20.0592568364947,
2.4765715409358));
#100179=CARTESIAN_POINT('Ctrl Pts',(-9.4053092366131,20.0583306526201,2.48332866944659));
#100180=CARTESIAN_POINT('Ctrl Pts',(-9.30670098552378,20.0503873536954,
2.54253739057376));
#100181=CARTESIAN_POINT('Ctrl Pts',(-9.22681507711688,20.0429526575367,
2.60581058093292));
#100182=CARTESIAN_POINT('Ctrl Pts',(-9.11558580553999,20.0312540924891,
2.72008252877829));
#100183=CARTESIAN_POINT('Ctrl Pts',(-9.0782476741731,20.0270245717561,2.76458584413573));
#100184=CARTESIAN_POINT('Ctrl Pts',(-9.04011457419426,20.0224825945526,
2.81752856753465));
#100185=CARTESIAN_POINT('Ctrl Pts',(-9.03594489588116,20.0219826310204,
2.82343141545693));
#100186=CARTESIAN_POINT('Ctrl Pts',(-9.02981771699475,20.0212433889728,
2.8322770895193));
#100187=CARTESIAN_POINT('Ctrl Pts',(-9.02781879535383,20.0210014772488,
2.83519081414577));
#100188=CARTESIAN_POINT('Ctrl Pts',(-9.0244148110659,20.020588302457,2.84020081118961));
#100189=CARTESIAN_POINT('Ctrl Pts',(-9.02300334296982,20.0204166156738,
2.84229264637065));
#100190=CARTESIAN_POINT('Ctrl Pts',(-9.01981306202943,20.0200277399637,
2.84705366434144));
#100191=CARTESIAN_POINT('Ctrl Pts',(-9.01803842286806,20.0198108293916,
2.84972558694336));
#100192=CARTESIAN_POINT('Ctrl Pts',(-9.01324098203139,20.0192227274708,
2.85701310807822));
#100193=CARTESIAN_POINT('Ctrl Pts',(-9.01023961498612,20.0188529172726,
2.8616428225913));
#100194=CARTESIAN_POINT('Ctrl Pts',(-8.99551070237757,20.0170277609961,
2.88471631630304));
#100195=CARTESIAN_POINT('Ctrl Pts',(-8.98426476525646,20.0156010937578,
2.90346430017379));
#100196=CARTESIAN_POINT('Ctrl Pts',(-8.9627209616243,20.012775788483,2.94175749949464));
#100197=CARTESIAN_POINT('Ctrl Pts',(-8.9524382138839,20.011378143836,2.96130073828413));
#100198=CARTESIAN_POINT('Ctrl Pts',(-8.89887056809101,20.0037506855643,
3.07045270881068));
#100199=CARTESIAN_POINT('Ctrl Pts',(-8.86652933171974,19.9977576214643,
3.16497516888545));
#100200=CARTESIAN_POINT('Ctrl Pts',(-8.84089637897507,19.9896130520816,
3.28944367417763));
#100201=CARTESIAN_POINT('Ctrl Pts',(-8.83628560309965,19.9878221582552,
3.31663211255273));
#100202=CARTESIAN_POINT('Ctrl Pts',(-8.83151367051865,19.9854433065172,
3.35233091623306));
#100203=CARTESIAN_POINT('Ctrl Pts',(-8.83048432431036,19.9848824998316,
3.36071777350632));
#100204=CARTESIAN_POINT('Ctrl Pts',(-8.82894666077115,19.9839595411634,
3.37446849169533));
#100205=CARTESIAN_POINT('Ctrl Pts',(-8.82838473611101,19.9835990678135,
3.37982614811689));
#100206=CARTESIAN_POINT('Ctrl Pts',(-8.8273670033187,19.9828982380175,3.39021634647297));
#100207=CARTESIAN_POINT('Ctrl Pts',(-8.82690678755419,19.9825580270623,
3.3952483459377));
#100208=CARTESIAN_POINT('Ctrl Pts',(-8.82591586062558,19.9817676623063,
3.40691009438077));
#100209=CARTESIAN_POINT('Ctrl Pts',(-8.82540890318171,19.981316779845,3.4135416344194));
#100210=CARTESIAN_POINT('Ctrl Pts',(-8.8239386711868,19.979840399331,3.43518431935718));
#100211=CARTESIAN_POINT('Ctrl Pts',(-8.82320683328511,19.9788077895267,
3.45020915844231));
#100212=CARTESIAN_POINT('Ctrl Pts',(-8.82036756792613,19.9721463985116,
3.54637734953955));
#100213=CARTESIAN_POINT('Ctrl Pts',(-8.82636639331177,19.9662659210613,
3.62752706531917));
#100214=CARTESIAN_POINT('Ctrl Pts',(-8.8502875177255,19.9562970216206,3.76124339507507));
#100215=CARTESIAN_POINT('Ctrl Pts',(-8.86365935354226,19.9522671238449,
3.81435236792767));
#100216=CARTESIAN_POINT('Ctrl Pts',(-8.88569702970261,19.9471871597312,
3.88168657511586));
#100217=CARTESIAN_POINT('Ctrl Pts',(-8.89103452229348,19.9460396458423,
3.89692741852733));
#100218=CARTESIAN_POINT('Ctrl Pts',(-8.90045512658755,19.9441494851345,
3.92215200553805));
#100219=CARTESIAN_POINT('Ctrl Pts',(-8.90436486273141,19.9433991652139,
3.93219776853356));
#100220=CARTESIAN_POINT('Ctrl Pts',(-8.90996955252484,19.9423705191155,
3.94603351089719));
#100221=CARTESIAN_POINT('Ctrl Pts',(-8.91154729798638,19.9420858010394,
3.94986996572215));
#100222=CARTESIAN_POINT('Ctrl Pts',(-8.91425410075539,19.9416055418476,
3.95635423672192));
#100223=CARTESIAN_POINT('Ctrl Pts',(-8.91537264576085,19.9414093856008,
3.95900637273709));
#100224=CARTESIAN_POINT('Ctrl Pts',(-8.91753771859271,19.9410341190966,
3.96408778039762));
#100225=CARTESIAN_POINT('Ctrl Pts',(-8.91858271743203,19.9408549157014,
3.96651765229217));
#100226=CARTESIAN_POINT('Ctrl Pts',(-8.9211092898625,19.9404261725905,3.97233842844829));
#100227=CARTESIAN_POINT('Ctrl Pts',(-8.92259868732268,19.9401770986818,
3.97572593767233));
#100228=CARTESIAN_POINT('Ctrl Pts',(-8.92807058311616,19.9392750143365,
3.98801379309746));
#100229=CARTESIAN_POINT('Ctrl Pts',(-8.93214773819185,19.9386274080813,
3.99687191430081));
#100230=CARTESIAN_POINT('Ctrl Pts',(-8.96260541857004,19.9339560021355,
4.06093784989113));
#100231=CARTESIAN_POINT('Ctrl Pts',(-8.99314619730812,19.9301461866744,
4.11407344618222));
#100232=CARTESIAN_POINT('Ctrl Pts',(-9.06546062635027,19.9222125204287,
4.21987025281009));
#100233=CARTESIAN_POINT('Ctrl Pts',(-9.107880244488,19.918103653838,4.2718152243657));
#100234=CARTESIAN_POINT('Ctrl Pts',(-9.17865440184662,19.9116404882417,
4.34480308501752));
#100235=CARTESIAN_POINT('Ctrl Pts',(-9.20391585110715,19.9093984839035,
4.36864866872874));
#100236=CARTESIAN_POINT('Ctrl Pts',(-9.23709250909748,19.9065075220645,
4.3973017101519));
#100237=CARTESIAN_POINT('Ctrl Pts',(-9.24406191112564,19.9059030787001,
4.4031809324649));
#100238=CARTESIAN_POINT('Ctrl Pts',(-9.25536910357985,19.9049265696161,
4.4124968523613));
#100239=CARTESIAN_POINT('Ctrl Pts',(-9.25966417016777,19.9045565813654,
4.41598500793572));
#100240=CARTESIAN_POINT('Ctrl Pts',(-9.2678921952375,19.9038494880237,4.4225715644522));
#100241=CARTESIAN_POINT('Ctrl Pts',(-9.27182065428259,19.9035126098231,
4.42567541204627));
#100242=CARTESIAN_POINT('Ctrl Pts',(-9.28084969261911,19.9027399118046,
4.43271614763406));
#100243=CARTESIAN_POINT('Ctrl Pts',(-9.28596299022662,19.9023034518902,
4.43663638754346));
#100244=CARTESIAN_POINT('Ctrl Pts',(-9.30190097252241,19.9009463267472,
4.44864928846435));
#100245=CARTESIAN_POINT('Ctrl Pts',(-9.31283265216253,19.9000201434959,
4.45659747765247));
#100246=CARTESIAN_POINT('Ctrl Pts',(-9.4070112149981,19.892076840469,4.52262529160026));
#100247=CARTESIAN_POINT('Ctrl Pts',(-9.49729318952429,19.8846421389151,
4.56989509722444));
#100248=CARTESIAN_POINT('Ctrl Pts',(-9.64691103405417,19.8729435727985,
4.62507239997114));
#100249=CARTESIAN_POINT('Ctrl Pts',(-9.70274897772568,19.8687140561529,
4.64109734656486));
#100250=CARTESIAN_POINT('Ctrl Pts',(-9.76662081961227,19.8641720828138,
4.6544182279161));
#100251=CARTESIAN_POINT('Ctrl Pts',(-9.77370889480538,19.8636721193894,
4.65582854656554));
#100252=CARTESIAN_POINT('Ctrl Pts',(-9.78428139263669,19.8629328774693,
4.65783117503079));
#100253=CARTESIAN_POINT('Ctrl Pts',(-9.78775606294384,19.8626909657664,
4.65847315870684));
#100254=CARTESIAN_POINT('Ctrl Pts',(-9.79371714012995,19.8622777909982,
4.65954681326201));
#100255=CARTESIAN_POINT('Ctrl Pts',(-9.79620209652775,19.8621061042175,
4.65998614017859));
#100256=CARTESIAN_POINT('Ctrl Pts',(-9.80184882649107,19.8617172284962,
4.66096574585834));
#100257=CARTESIAN_POINT('Ctrl Pts',(-9.80501140682314,19.8615003179105,
4.66150109761973));
#100258=CARTESIAN_POINT('Ctrl Pts',(-9.81361977753592,19.8609122159163,
4.66292214503367));
#100259=CARTESIAN_POINT('Ctrl Pts',(-9.81906975252084,19.860542405659,4.6637825188793));
#100260=CARTESIAN_POINT('Ctrl Pts',(-9.84613806928921,19.8587172486159,
4.66786097940075));
#100261=CARTESIAN_POINT('Ctrl Pts',(-9.86783858980784,19.8572905806989,
4.67051538665244));
#100262=CARTESIAN_POINT('Ctrl Pts',(-9.91158265192551,19.8544652749122,
4.67463392820757));
#100263=CARTESIAN_POINT('Ctrl Pts',(-9.93361824205453,19.8530676304076,
4.67608505322905));
#100264=CARTESIAN_POINT('Ctrl Pts',(-10.0551201609284,19.8454401712868,
4.68066026965506));
#100265=CARTESIAN_POINT('Ctrl Pts',(-10.1546276556612,19.8394471061895,
4.67178824226758));
#100266=CARTESIAN_POINT('Ctrl Pts',(-10.2787689453709,19.8313025369412,
4.64461480179881));
#100267=CARTESIAN_POINT('Ctrl Pts',(-10.3054841319522,19.8295116445137,
4.63777608676271));
#100268=CARTESIAN_POINT('Ctrl Pts',(-10.3400404207402,19.8271327943743,
4.627625368954));
#100269=CARTESIAN_POINT('Ctrl Pts',(-10.3481215749565,19.8265719878419,
4.62515679943333));
#100270=CARTESIAN_POINT('Ctrl Pts',(-10.3613101030482,19.8256490293611,
4.62097238695968));
#100271=CARTESIAN_POINT('Ctrl Pts',(-10.3664335981194,19.8252885560443,
4.61930804491788));
#100272=CARTESIAN_POINT('Ctrl Pts',(-10.3763404105,19.8245877262665,4.61601455676634));
#100273=CARTESIAN_POINT('Ctrl Pts',(-10.381125023763,19.8242475152962,4.61438965823406));
#100274=CARTESIAN_POINT('Ctrl Pts',(-10.392182709015,19.8234571504368,4.61055482513273));
#100275=CARTESIAN_POINT('Ctrl Pts',(-10.3984477621367,19.8230062678867,
4.60832245965198));
#100276=CARTESIAN_POINT('Ctrl Pts',(-10.4188194824617,19.8215298867793,
4.60086854933664));
#100277=CARTESIAN_POINT('Ctrl Pts',(-10.4328445883031,19.8204972764622,
4.59542998303295));
#100278=CARTESIAN_POINT('Ctrl Pts',(-10.5218636455835,19.8138359047785,
4.55893428599914));
#100279=CARTESIAN_POINT('Ctrl Pts',(-10.593568449894,19.8079554491475,4.52046824730961));
#100280=CARTESIAN_POINT('Ctrl Pts',(-10.7060166537096,19.7979865552552,
4.44426024582946));
#100281=CARTESIAN_POINT('Ctrl Pts',(-10.7491051818362,19.7939566409911,
4.41045534012406));
#100282=CARTESIAN_POINT('Ctrl Pts',(-10.8016683311451,19.7888766584325,
4.36295054273845));
#100283=CARTESIAN_POINT('Ctrl Pts',(-10.8134237831107,19.7877291419767,
4.35187883911399));
#100284=CARTESIAN_POINT('Ctrl Pts',(-10.8326413335058,19.785838977503,4.33301839988183));
#100285=CARTESIAN_POINT('Ctrl Pts',(-10.840230570131,19.7850886563464,4.32536286234415));
#100286=CARTESIAN_POINT('Ctrl Pts',(-10.8505936130219,19.7840600088504,
4.31461817729191));
#100287=CARTESIAN_POINT('Ctrl Pts',(-10.8534575246255,19.7837752905904,
4.31161722767669));
#100288=CARTESIAN_POINT('Ctrl Pts',(-10.8582817126267,19.7832950311799,
4.306508430752));
#100289=CARTESIAN_POINT('Ctrl Pts',(-10.8602502089011,19.783098874897,4.30440843224425));
#100290=CARTESIAN_POINT('Ctrl Pts',(-10.8640128511282,19.7827236083958,
4.30036482410591));
#100291=CARTESIAN_POINT('Ctrl Pts',(-10.8658081670061,19.7825444050394,
4.29842236747187));
#100292=CARTESIAN_POINT('Ctrl Pts',(-10.8700993999265,19.7821156621156,
4.29374793835391));
#100293=CARTESIAN_POINT('Ctrl Pts',(-10.8725890348611,19.7818665883544,
4.29101019750494));
#100294=CARTESIAN_POINT('Ctrl Pts',(-10.8815917823888,19.7809645053208,
4.28101604715774));
#100295=CARTESIAN_POINT('Ctrl Pts',(-10.8880278403469,19.7803169002087,
4.27369031705033));
#100296=CARTESIAN_POINT('Ctrl Pts',(-10.9341832921174,19.7756453819506,
4.2198198220698));
#100297=CARTESIAN_POINT('Ctrl Pts',(-10.9703181327586,19.7718354654465,
4.17031612629714));
#100298=CARTESIAN_POINT('Ctrl Pts',(-11.0375864444072,19.7639017751128,
4.06124078745673));
#100299=CARTESIAN_POINT('Ctrl Pts',(-11.0678033570306,19.7597929825771,
4.00137034093373));
#100300=CARTESIAN_POINT('Ctrl Pts',(-11.1057209842605,19.7533299187207,
3.90704044478896));
#100301=CARTESIAN_POINT('Ctrl Pts',(-11.1172395101833,19.7510879372613,
3.87426772952716));
#100302=CARTESIAN_POINT('Ctrl Pts',(-11.1299331170329,19.7481970012508,
3.83230911694384));
#100303=CARTESIAN_POINT('Ctrl Pts',(-11.1324718450559,19.7475925598375,
3.82355171238884));
#100304=CARTESIAN_POINT('Ctrl Pts',(-11.1363873500754,19.7466160531505,
3.80943410928476));
#100305=CARTESIAN_POINT('Ctrl Pts',(-11.1378285078647,19.7462460653273,
3.80409202935022));
#100306=CARTESIAN_POINT('Ctrl Pts',(-11.1405019094315,19.7455389723053,
3.79389713154148));
#100307=CARTESIAN_POINT('Ctrl Pts',(-11.1417409584071,19.7452020939936,
3.78904621067819));
#100308=CARTESIAN_POINT('Ctrl Pts',(-11.1445037391334,19.7444293950151,
3.77793482677214));
#100309=CARTESIAN_POINT('Ctrl Pts',(-11.146007090309,19.743992934246,3.77166951046781));
#100310=CARTESIAN_POINT('Ctrl Pts',(-11.150504452496,19.7426358037659,3.752224565061));
#100311=CARTESIAN_POINT('Ctrl Pts',(-11.1533229723499,19.7417096159696,
3.73900590243519));
#100312=CARTESIAN_POINT('Ctrl Pts',(-11.1753687704391,19.7337663428555,
3.62612032282185));
#100313=CARTESIAN_POINT('Ctrl Pts',(-11.1818600735266,19.7263316806437,
3.52441964960938));
#100314=CARTESIAN_POINT('Ctrl Pts',(-11.1714577973445,19.7146331223228,
3.36529143487493));
#100315=CARTESIAN_POINT('Ctrl Pts',(-11.1634024523517,19.7104035758714,
3.30776029575101));
#100316=CARTESIAN_POINT('Ctrl Pts',(-11.1496108706964,19.7058615743522,
3.2439880219171));
#100317=CARTESIAN_POINT('Ctrl Pts',(-11.1480183003497,19.7053616101421,
3.23693864675703));
#100318=CARTESIAN_POINT('Ctrl Pts',(-11.1455505709564,19.7046223672919,
3.22646492577176));
#100319=CARTESIAN_POINT('Ctrl Pts',(-11.1447247612883,19.7043804554352,
3.22302929907591));
#100320=CARTESIAN_POINT('Ctrl Pts',(-11.1432826915567,19.7039672804955,
3.21714647322273));
#100321=CARTESIAN_POINT('Ctrl Pts',(-11.142674016126,19.7037955936963,3.21469748732636));
#100322=CARTESIAN_POINT('Ctrl Pts',(-11.1412737925602,19.7034067180566,
3.20914010069286));
#100323=CARTESIAN_POINT('Ctrl Pts',(-11.1404774148939,19.7031898075703,
3.2060329655415));
#100324=CARTESIAN_POINT('Ctrl Pts',(-11.1382766898464,19.702601706111,3.19759021177256));
#100325=CARTESIAN_POINT('Ctrl Pts',(-11.1368475060319,19.7022318962848,
3.19226106249127));
#100326=CARTESIAN_POINT('Ctrl Pts',(-11.1295712798933,19.7004067448321,
3.16587205869307));
#100327=CARTESIAN_POINT('Ctrl Pts',(-11.1231758255709,19.6989800818643,
3.14496624079025));
#100328=CARTESIAN_POINT('Ctrl Pts',(-11.1091579590717,19.6961547798103,
3.10332492490595));
#100329=CARTESIAN_POINT('Ctrl Pts',(-11.1015268879771,19.6947571342677,
3.08260198141742));
#100330=CARTESIAN_POINT('Ctrl Pts',(-11.0563197033247,19.6871296813386,
2.96973066768217));
#100331=CARTESIAN_POINT('Ctrl Pts',(-11.0077664858241,19.6811366235139,
2.88242078838443));
#100332=CARTESIAN_POINT('Ctrl Pts',(-10.9324788863872,19.6729920532858,
2.78004284522241));
#100333=CARTESIAN_POINT('Ctrl Pts',(-10.915371472707,19.6712011506575,2.75841382543352));
#100334=CARTESIAN_POINT('Ctrl Pts',(-10.8920507793595,19.6688222888599,
2.73096692673291));
#100335=CARTESIAN_POINT('Ctrl Pts',(-10.8865105460763,19.6682614812111,
2.72458688027257));
#100336=CARTESIAN_POINT('Ctrl Pts',(-10.8773265917048,19.667338521363,2.71423786397006));
#100337=CARTESIAN_POINT('Ctrl Pts',(-10.873723372428,19.6669780478048,2.71023323078161));
#100338=CARTESIAN_POINT('Ctrl Pts',(-10.8666873681529,19.6662772178942,
2.70252046963059));
#100339=CARTESIAN_POINT('Ctrl Pts',(-10.8632579372852,19.6659370070345,
2.6988094310242));
#100340=CARTESIAN_POINT('Ctrl Pts',(-10.8552595350308,19.6651466429285,
2.69026521348653));
#100341=CARTESIAN_POINT('Ctrl Pts',(-10.8506733289371,19.6646957610256,
2.68544847859021));
#100342=CARTESIAN_POINT('Ctrl Pts',(-10.8355824311164,19.6632193842461,
2.66986548017442));
#100343=CARTESIAN_POINT('Ctrl Pts',(-10.8249126090658,19.6621867776678,
2.65926194855719));
#100344=CARTESIAN_POINT('Ctrl Pts',(-10.7553824227598,19.6555252650437,
2.59276176086409));
#100345=CARTESIAN_POINT('Ctrl Pts',(-10.6910894853644,19.6496446503321,
2.54288213270714));
#100346=CARTESIAN_POINT('Ctrl Pts',(-10.5757529820029,19.6396757159865,
2.47111941540398));
#100347=CARTESIAN_POINT('Ctrl Pts',(-10.5273536555237,19.6356459219352,
2.445492793624));
#100348=CARTESIAN_POINT('Ctrl Pts',(-10.4625863905332,19.6305660738538,
2.41677815043175));
#100349=CARTESIAN_POINT('Ctrl Pts',(-10.4476925338677,19.6294185761121,
2.41053811709997));
#100350=CARTESIAN_POINT('Ctrl Pts',(-10.4226493720335,19.6275284390956,
2.40064621236914));
#100351=CARTESIAN_POINT('Ctrl Pts',(-10.412570083668,19.6267781269504,2.39682404448078));
#100352=CARTESIAN_POINT('Ctrl Pts',(-10.3985408956826,19.6257494896444,
2.39172321886773));
#100353=CARTESIAN_POINT('Ctrl Pts',(-10.3946349524379,19.6254647727251,
2.39032638818606));
#100354=CARTESIAN_POINT('Ctrl Pts',(-10.3880063499558,19.6249845149093,
2.38799531499366));
#100355=CARTESIAN_POINT('Ctrl Pts',(-10.3852875206404,19.6247883588897,
2.38705037212041));
#100356=CARTESIAN_POINT('Ctrl Pts',(-10.3800636100059,19.6244130923662,
2.38525621286648));
#100357=CARTESIAN_POINT('Ctrl Pts',(-10.3775591065739,19.6242338887269,
2.38440545895937));
#100358=CARTESIAN_POINT('Ctrl Pts',(-10.3715439610823,19.6238051444385,
2.38238475292391));
#100359=CARTESIAN_POINT('Ctrl Pts',(-10.3680306021654,19.6235560696021,
2.38122288533129));
#100360=CARTESIAN_POINT('Ctrl Pts',(-10.3552398004762,19.6226539770035,
2.37705974186617));
#100361=CARTESIAN_POINT('Ctrl Pts',(-10.3459303419297,19.6220063635559,
2.37415704783111));
#100362=CARTESIAN_POINT('Ctrl Pts',(-10.2779615202111,19.6173356462387,
2.35388705115075));
#100363=CARTESIAN_POINT('Ctrl Pts',(-10.2180562220649,19.6135264504694,
2.34099569901897));
#100364=CARTESIAN_POINT('Ctrl Pts',(-10.091059043873,19.6055929321073,2.32386806920044));
#100365=CARTESIAN_POINT('Ctrl Pts',(-10.0240662146888,19.601483611511,2.32059410611628));
#100366=CARTESIAN_POINT('Ctrl Pts',(-9.92245630101493,19.5950198221902,
2.32429256440615));
#100367=CARTESIAN_POINT('Ctrl Pts',(-9.88782851761291,19.5927776776006,
2.32708986039856));
#100368=CARTESIAN_POINT('Ctrl Pts',(-9.84433009853263,19.589886557428,2.33254760960661));
#100369=CARTESIAN_POINT('Ctrl Pts',(-9.83529664952736,19.5892821021039,
2.33378775488198));
#100370=CARTESIAN_POINT('Ctrl Pts',(-9.82121534134334,19.5883331559789,
2.33588775614029));
#100371=CARTESIAN_POINT('Ctrl Pts',(-9.81615701727274,19.5879909141281,
2.33667587204691));
#100372=CARTESIAN_POINT('Ctrl Pts',(-9.8111040637102,19.5876476368634,2.33749693000268));
#100373=CARTESIAN_POINT('Ctrl Pts',(-9.81110408825476,19.4882767425658,
2.33749692601442));
#100374=CARTESIAN_POINT('Ctrl Pts',(-9.8314222932125,19.4895559525066,2.33419540713123));
#100375=CARTESIAN_POINT('Ctrl Pts',(-9.85183268213264,19.4908290092334,
2.33142565391848));
#100376=CARTESIAN_POINT('Ctrl Pts',(-9.953143009874,19.4971287400356,2.32037699327464));
#100377=CARTESIAN_POINT('Ctrl Pts',(-10.0346566291727,19.5021558995863,
2.31995643091115));
#100378=CARTESIAN_POINT('Ctrl Pts',(-10.130523110947,19.508438767749,2.32940832202197));
#100379=CARTESIAN_POINT('Ctrl Pts',(-10.1454568499483,19.5094275866102,
2.33117005926822));
#100380=CARTESIAN_POINT('Ctrl Pts',(-10.1669389221768,19.5108664263385,
2.33412236378128));
#100381=CARTESIAN_POINT('Ctrl Pts',(-10.173517710403,19.511309293842,2.33508332164917));
#100382=CARTESIAN_POINT('Ctrl Pts',(-10.185079773689,19.5120917091539,2.33687229623325));
#100383=CARTESIAN_POINT('Ctrl Pts',(-10.1900665608985,19.5124305114833,
2.33767677517588));
#100384=CARTESIAN_POINT('Ctrl Pts',(-10.2003587733106,19.5131326113626,
2.33940514189671));
#100385=CARTESIAN_POINT('Ctrl Pts',(-10.2056633365375,19.5134960386458,
2.34033338711694));
#100386=CARTESIAN_POINT('Ctrl Pts',(-10.2192713714732,19.5144324813276,
2.34281095967114));
#100387=CARTESIAN_POINT('Ctrl Pts',(-10.2275647595564,19.5150071534281,
2.34441327320792));
#100388=CARTESIAN_POINT('Ctrl Pts',(-10.2628404000399,19.517468899703,2.3516231187118));
#100389=CARTESIAN_POINT('Ctrl Pts',(-10.2896366409912,19.5193827338782,
2.35808716009673));
#100390=CARTESIAN_POINT('Ctrl Pts',(-10.4120214363975,19.5283342217747,
2.3921947499258));
#100391=CARTESIAN_POINT('Ctrl Pts',(-10.5040827691871,19.5357153482304,
2.43094024442401));
#100392=CARTESIAN_POINT('Ctrl Pts',(-10.6092762727826,19.5445753968953,
2.49185045404422));
#100393=CARTESIAN_POINT('Ctrl Pts',(-10.6280796050488,19.5461752199412,
2.50345637978717));
#100394=CARTESIAN_POINT('Ctrl Pts',(-10.6648377401688,19.5493209306366,
2.52759846295841));
#100395=CARTESIAN_POINT('Ctrl Pts',(-10.6827923963382,19.5508666099407,
2.540120495292));
#100396=CARTESIAN_POINT('Ctrl Pts',(-10.7048255448218,19.5527652057932,
2.55641827768811));
#100397=CARTESIAN_POINT('Ctrl Pts',(-10.7092391114073,19.5531456127061,
2.55973120802322));
#100398=CARTESIAN_POINT('Ctrl Pts',(-10.7161806594788,19.5537438401859,
2.56501838999872));
#100399=CARTESIAN_POINT('Ctrl Pts',(-10.7187240732731,19.5539630189232,
2.56697210375359));
#100400=CARTESIAN_POINT('Ctrl Pts',(-10.723253665748,19.5543532835892,2.57048100583427));
#100401=CARTESIAN_POINT('Ctrl Pts',(-10.7252428187139,19.5545246369375,
2.57203217748863));
#100402=CARTESIAN_POINT('Ctrl Pts',(-10.730004516315,19.5549347767288,2.57577008443367));
#100403=CARTESIAN_POINT('Ctrl Pts',(-10.7327722265213,19.5551731310917,
2.57796290989698));
#100404=CARTESIAN_POINT('Ctrl Pts',(-10.7411675852092,19.5558961691738,
2.58467613587516));
#100405=CARTESIAN_POINT('Ctrl Pts',(-10.7467637051208,19.5563781714753,
2.58923595768833));
#100406=CARTESIAN_POINT('Ctrl Pts',(-10.7967634310582,19.5606888081975,
2.63074736166117));
#100407=CARTESIAN_POINT('Ctrl Pts',(-10.8384406400089,19.5643131194672,
2.67087317444984));
#100408=CARTESIAN_POINT('Ctrl Pts',(-10.9449613168303,19.5742190856175,
2.7897126931168));
#100409=CARTESIAN_POINT('Ctrl Pts',(-11.0027901641923,19.580416609729,2.8740049505218));
#100410=CARTESIAN_POINT('Ctrl Pts',(-11.055184346043,19.5879546091105,2.97668117235625));
#100411=CARTESIAN_POINT('Ctrl Pts',(-11.0611018464588,19.5888422972535,
2.98878630043618));
#100412=CARTESIAN_POINT('Ctrl Pts',(-11.069536221888,19.5901644127521,3.00681775390142));
#100413=CARTESIAN_POINT('Ctrl Pts',(-11.0722144109073,19.5905933237335,
3.01266776007505));
#100414=CARTESIAN_POINT('Ctrl Pts',(-11.0768901488104,19.5913587433108,
3.02310618490724));
#100415=CARTESIAN_POINT('Ctrl Pts',(-11.0789066540735,19.5916945983379,
3.02768597951232));
#100416=CARTESIAN_POINT('Ctrl Pts',(-11.0830919563164,19.5924040328762,
3.03735811749927));
#100417=CARTESIAN_POINT('Ctrl Pts',(-11.0852541584472,19.5927778252737,
3.04245316409917));
#100418=CARTESIAN_POINT('Ctrl Pts',(-11.0908882692075,19.593771555807,3.05599410745709));
#100419=CARTESIAN_POINT('Ctrl Pts',(-11.0942979429618,19.5943935583273,
3.06446532588785));
#100420=CARTESIAN_POINT('Ctrl Pts',(-11.1102686349562,19.5974099379914,
3.10551579292067));
#100421=CARTESIAN_POINT('Ctrl Pts',(-11.1214739789335,19.5998484609782,
3.13860007376705));
#100422=CARTESIAN_POINT('Ctrl Pts',(-11.150020170555,19.6071342427155,3.23708811206023));
#100423=CARTESIAN_POINT('Ctrl Pts',(-11.1632157029336,19.6120915781559,
3.30354038772696));
#100424=CARTESIAN_POINT('Ctrl Pts',(-11.1772481195622,19.6214797840134,
3.43063325644706));
#100425=CARTESIAN_POINT('Ctrl Pts',(-11.179255841517,19.6258929177163,3.49094275425309));
#100426=CARTESIAN_POINT('Ctrl Pts',(-11.1762140773131,19.6308014357199,
3.56091967566458));
#100427=CARTESIAN_POINT('Ctrl Pts',(-11.1756674744183,19.6314816817386,
3.57068781913781));
#100428=CARTESIAN_POINT('Ctrl Pts',(-11.174746215746,19.6324108976232,3.5841433769803));
#100429=CARTESIAN_POINT('Ctrl Pts',(-11.1744758010678,19.6326651722056,
3.58783719564363));
#100430=CARTESIAN_POINT('Ctrl Pts',(-11.1739823803604,19.6330994401997,
3.59416703616647));
#100431=CARTESIAN_POINT('Ctrl Pts',(-11.1737679117601,19.6332798940441,
3.59680366611608));
#100432=CARTESIAN_POINT('Ctrl Pts',(-11.1733017092714,19.6336555106059,
3.60230559372149));
#100433=CARTESIAN_POINT('Ctrl Pts',(-11.1730483602414,19.6338505756278,
3.60517071958557));
#100434=CARTESIAN_POINT('Ctrl Pts',(-11.1724046478051,19.6343250777062,
3.61215860850403));
#100435=CARTESIAN_POINT('Ctrl Pts',(-11.172003026203,19.6346038958872,3.61628034882937));
#100436=CARTESIAN_POINT('Ctrl Pts',(-11.1704818856396,19.6356016333146,
3.63108215866466));
#100437=CARTESIAN_POINT('Ctrl Pts',(-11.1692380126689,19.636314036907,3.6417493097949));
#100438=CARTESIAN_POINT('Ctrl Pts',(-11.1657694303742,19.6380759653208,
3.66832949514771));
#100439=CARTESIAN_POINT('Ctrl Pts',(-11.1633646282005,19.6391172472682,
3.68421720669907));
#100440=CARTESIAN_POINT('Ctrl Pts',(-11.1514269018134,19.6436238430998,
3.75347609685293));
#100441=CARTESIAN_POINT('Ctrl Pts',(-11.1385399351733,19.6469718338608,
3.8062054726742));
#100442=CARTESIAN_POINT('Ctrl Pts',(-11.0972058398895,19.6553809774893,
3.93580689827414));
#100443=CARTESIAN_POINT('Ctrl Pts',(-11.0642968278718,19.6604373674012,
4.01093879214562));
#100444=CARTESIAN_POINT('Ctrl Pts',(-11.0164468784094,19.6667523796445,
4.09511048235554));
#100445=CARTESIAN_POINT('Ctrl Pts',(-11.0087736910705,19.6677403037214,
4.10802660273766));
#100446=CARTESIAN_POINT('Ctrl Pts',(-10.9973526363589,19.6691780747029,
4.12643990362441));
#100447=CARTESIAN_POINT('Ctrl Pts',(-10.9938017561005,19.6696207833053,
4.13205798834511));
#100448=CARTESIAN_POINT('Ctrl Pts',(-10.9874689816378,19.6704030132263,
4.14189219043841));
#100449=CARTESIAN_POINT('Ctrl Pts',(-10.9847071350259,19.6707417901783,
4.14612106505734));
#100450=CARTESIAN_POINT('Ctrl Pts',(-10.9789440787966,19.6714439306755,
4.15482254361596));
#100451=CARTESIAN_POINT('Ctrl Pts',(-10.9759392230919,19.671807424522,4.15929257860341));
#100452=CARTESIAN_POINT('Ctrl Pts',(-10.9681410699812,19.6727442366819,
4.17072300746655));
#100453=CARTESIAN_POINT('Ctrl Pts',(-10.9633033927924,19.6733192142212,
4.17765260353574));
#100454=CARTESIAN_POINT('Ctrl Pts',(-10.9423499057712,19.6757841384546,
4.20698903212234));
#100455=CARTESIAN_POINT('Ctrl Pts',(-10.9255248777781,19.6777009314379,
4.22887606384999));
#100456=CARTESIAN_POINT('Ctrl Pts',(-10.8445964965762,19.6866536043635,
4.32682807504675));
#100457=CARTESIAN_POINT('Ctrl Pts',(-10.771792579397,19.6940324970517,4.39516378195481));
#100458=CARTESIAN_POINT('Ctrl Pts',(-10.6734014737404,19.7028904393982,
4.46649557861566));
#100459=CARTESIAN_POINT('Ctrl Pts',(-10.6551507405275,19.7044905044152,
4.47895906415409));
#100460=CARTESIAN_POINT('Ctrl Pts',(-10.6181642260564,19.7076349538169,
4.50271934070971));
#100461=CARTESIAN_POINT('Ctrl Pts',(-10.5994421264333,19.7091791730579,
4.51402286628597));
#100462=CARTESIAN_POINT('Ctrl Pts',(-10.575614483281,19.7110762420384,4.52751810850758));
#100463=CARTESIAN_POINT('Ctrl Pts',(-10.5707950419972,19.7114565308622,
4.53020314487165));
#100464=CARTESIAN_POINT('Ctrl Pts',(-10.5631445883315,19.7120546142186,
4.53439524273536));
#100465=CARTESIAN_POINT('Ctrl Pts',(-10.5603260577118,19.7122737658631,
4.53592473434785));
#100466=CARTESIAN_POINT('Ctrl Pts',(-10.5552792208171,19.7126640076338,
4.53863680504178));
#100467=CARTESIAN_POINT('Ctrl Pts',(-10.5530533737637,19.7128353649804,
4.53982373112309));
#100468=CARTESIAN_POINT('Ctrl Pts',(-10.5477021112782,19.7132455468889,
4.54265523160871));
#100469=CARTESIAN_POINT('Ctrl Pts',(-10.5445730943463,19.7134839391123,
4.54429290930887));
#100470=CARTESIAN_POINT('Ctrl Pts',(-10.5350238787731,19.7142072076487,
4.54923622530378));
#100471=CARTESIAN_POINT('Ctrl Pts',(-10.5285804560942,19.7146894000474,
4.55249699060958));
#100472=CARTESIAN_POINT('Ctrl Pts',(-10.4702362521768,19.7190068717558,
4.5813517585683));
#100473=CARTESIAN_POINT('Ctrl Pts',(-10.4165373495374,19.7226371190832,
4.60315107234167));
#100474=CARTESIAN_POINT('Ctrl Pts',(-10.2646766985676,19.7325407008603,
4.65211951200985));
#100475=CARTESIAN_POINT('Ctrl Pts',(-10.164285479955,19.7387308092398,4.67065851878124));
#100476=CARTESIAN_POINT('Ctrl Pts',(-10.0492923203816,19.7462610751277,
4.67679536232488));
#100477=CARTESIAN_POINT('Ctrl Pts',(-10.0358100500005,19.7471498640633,
4.67728275004208));
#100478=CARTESIAN_POINT('Ctrl Pts',(-10.0158868276254,19.7484733083011,
4.67766043836936));
#100479=CARTESIAN_POINT('Ctrl Pts',(-10.009450052787,19.7489024308902,4.6777296774391));
#100480=CARTESIAN_POINT('Ctrl Pts',(-9.99800866624269,19.7496680877224,
4.67775894902589));
#100481=CARTESIAN_POINT('Ctrl Pts',(-9.99300422924021,19.7500039669109,
4.67773985467367));
#100482=CARTESIAN_POINT('Ctrl Pts',(-9.98246726647646,19.750713307718,4.67763249001013));
#100483=CARTESIAN_POINT('Ctrl Pts',(-9.97693495101431,19.7510869813182,
4.67753712467072));
#100484=CARTESIAN_POINT('Ctrl Pts',(-9.96228252526964,19.7520800561195,
4.67718125093971));
#100485=CARTESIAN_POINT('Ctrl Pts',(-9.95316457014405,19.752701516847,4.67685374614358));
#100486=CARTESIAN_POINT('Ctrl Pts',(-9.90927040958652,19.7557107241877,
4.67476621863143));
#100487=CARTESIAN_POINT('Ctrl Pts',(-9.87458320834331,19.7581423614006,
4.67157062083553));
#100488=CARTESIAN_POINT('Ctrl Pts',(-9.77342230870075,19.7653964768915,
4.65770715480371));
#100489=CARTESIAN_POINT('Ctrl Pts',(-9.70766564010123,19.7703278005707,
4.64287446589006));
#100490=CARTESIAN_POINT('Ctrl Pts',(-9.58566361135629,19.7797266054412,
4.60413234679485));
#100491=CARTESIAN_POINT('Ctrl Pts',(-9.529286489425,19.7841761609002,4.5813016171111));
#100492=CARTESIAN_POINT('Ctrl Pts',(-9.46618039964194,19.789116514295,4.54986997633635));
#100493=CARTESIAN_POINT('Ctrl Pts',(-9.45749756252738,19.7897952092708,
4.54540970619246));
#100494=CARTESIAN_POINT('Ctrl Pts',(-9.44560020437287,19.790722705903,4.53911001597342));
#100495=CARTESIAN_POINT('Ctrl Pts',(-9.44233769905367,19.7909767864524,
4.53736277054947));
#100496=CARTESIAN_POINT('Ctrl Pts',(-9.43675805867344,19.7914108095985,
4.53434064587951));
#100497=CARTESIAN_POINT('Ctrl Pts',(-9.4344369077111,19.7915912115127,4.53307330097253));
#100498=CARTESIAN_POINT('Ctrl Pts',(-9.42959962153525,19.791966818013,4.53041096043378));
#100499=CARTESIAN_POINT('Ctrl Pts',(-9.42708430419931,19.7921619244093,
4.52901455037284));
#100500=CARTESIAN_POINT('Ctrl Pts',(-9.42095800466888,19.7926366873604,
4.52558403192004));
#100501=CARTESIAN_POINT('Ctrl Pts',(-9.41735254785636,19.7929157234149,
4.52354002691457));
#100502=CARTESIAN_POINT('Ctrl Pts',(-9.40442546891298,19.7939151215607,
4.51612096793535));
#100503=CARTESIAN_POINT('Ctrl Pts',(-9.39516647849559,19.7946289394325,
4.51063706398744));
#100504=CARTESIAN_POINT('Ctrl Pts',(-9.37223631340194,19.7963950756163,
4.49662798612296));
#100505=CARTESIAN_POINT('Ctrl Pts',(-9.35866212546349,19.7974391004056,
4.48794755613233));
#100506=CARTESIAN_POINT('Ctrl Pts',(-9.29998312044579,19.8019652652598,
4.44870416136977));
#100507=CARTESIAN_POINT('Ctrl Pts',(-9.25684901485212,19.8053290434821,
4.41530911333645));
#100508=CARTESIAN_POINT('Ctrl Pts',(-9.1553828257795,19.8137326492291,4.32483447172748));
#100509=CARTESIAN_POINT('Ctrl Pts',(-9.10038167563283,19.818768376362,4.26447029702423));
#100510=CARTESIAN_POINT('Ctrl Pts',(-9.04312986584215,19.8250606704396,
4.1868191808704));
#100511=CARTESIAN_POINT('Ctrl Pts',(-9.03444182074504,19.8260492352986,
4.17455052431923));
#100512=CARTESIAN_POINT('Ctrl Pts',(-9.02225389163279,19.82748777165,4.15662150801377));
#100513=CARTESIAN_POINT('Ctrl Pts',(-9.01856318507873,19.8279305940558,
4.15109218431998));
#100514=CARTESIAN_POINT('Ctrl Pts',(-9.012150976799,19.828712956748,4.14130716829582));
#100515=CARTESIAN_POINT('Ctrl Pts',(-9.00940964903017,19.829051751871,4.13706462148763));
#100516=CARTESIAN_POINT('Ctrl Pts',(-9.00380213034382,19.829753863258,4.12826258055273));
#100517=CARTESIAN_POINT('Ctrl Pts',(-9.00093975750705,19.8301173094164,
4.1237008063431));
#100518=CARTESIAN_POINT('Ctrl Pts',(-8.99366788701324,19.8310538568738,
4.11193309190051));
#100519=CARTESIAN_POINT('Ctrl Pts',(-8.98930451695686,19.8316286155903,
4.10469915219855));
#100520=CARTESIAN_POINT('Ctrl Pts',(-8.97103423981751,19.8340912626115,
4.07365900410973));
#100521=CARTESIAN_POINT('Ctrl Pts',(-8.95788876058976,19.8360059353588,
4.04941708511116));
#100522=CARTESIAN_POINT('Ctrl Pts',(-8.90128183863335,19.8449577586824,
3.93567278003121));
#100523=CARTESIAN_POINT('Ctrl Pts',(-8.86842553540125,19.8523382515614,
3.84135856033438));
#100524=CARTESIAN_POINT('Ctrl Pts',(-8.84323753409045,19.8611977026796,
3.72244938224359));
#100525=CARTESIAN_POINT('Ctrl Pts',(-8.8392682102299,19.8627975941922,3.70071107623423));
#100526=CARTESIAN_POINT('Ctrl Pts',(-8.83258978658459,19.8659429476777,
3.65724857194682));
#100527=CARTESIAN_POINT('Ctrl Pts',(-8.82986991932668,19.8674882135357,
3.63553399582588));
#100528=CARTESIAN_POINT('Ctrl Pts',(-8.8272234911941,19.8693863770422,3.6082625070403));
#100529=CARTESIAN_POINT('Ctrl Pts',(-8.82672912480367,19.8697667505298,
3.60276656291679));
#100530=CARTESIAN_POINT('Ctrl Pts',(-8.82600853391856,19.8703649372153,
3.59407116941341));
#100531=CARTESIAN_POINT('Ctrl Pts',(-8.82575672767739,19.8705841082841,
3.59087400825361));
#100532=CARTESIAN_POINT('Ctrl Pts',(-8.82533019478079,19.8709743664685,
3.58516028611495));
#100533=CARTESIAN_POINT('Ctrl Pts',(-8.82515049425902,19.8711457209473,
3.58264420527078));
#100534=CARTESIAN_POINT('Ctrl Pts',(-8.82473863113347,19.8715558726543,
3.57660448197468));
#100535=CARTESIAN_POINT('Ctrl Pts',(-8.82451423032849,19.8717942377292,
3.57308035253873));
#100536=CARTESIAN_POINT('Ctrl Pts',(-8.82387933802565,19.8725173410107,
3.56234874406912));
#100537=CARTESIAN_POINT('Ctrl Pts',(-8.82351925086111,19.8729993970934,
3.55513828769706));
#100538=CARTESIAN_POINT('Ctrl Pts',(-8.82087366611127,19.8773119659385,
3.49017693805894));
#100539=CARTESIAN_POINT('Ctrl Pts',(-8.82277551637046,19.8809379553014,
3.43232573194193));
#100540=CARTESIAN_POINT('Ctrl Pts',(-8.8397342467914,19.8908432126978,3.27364710826556));
#100541=CARTESIAN_POINT('Ctrl Pts',(-8.8636173534054,19.8970386072608,3.17429354386661));
#100542=CARTESIAN_POINT('Ctrl Pts',(-8.90468762747087,19.9045563031272,
3.06691783651471));
#100543=CARTESIAN_POINT('Ctrl Pts',(-8.90961085845438,19.9054259576994,
3.05466770734737));
#100544=CARTESIAN_POINT('Ctrl Pts',(-8.9172265018725,19.9067276320799,3.03660208529756));
#100545=CARTESIAN_POINT('Ctrl Pts',(-8.91976224021116,19.9071544107041,
3.03072134589832));
#100546=CARTESIAN_POINT('Ctrl Pts',(-8.92432829551426,19.9079115451808,
3.02036514318219));
#100547=CARTESIAN_POINT('Ctrl Pts',(-8.9263389163284,19.9082412280821,3.01588112218061));
#100548=CARTESIAN_POINT('Ctrl Pts',(-8.93030947881257,19.9088852132209,
3.00717250568848));
#100549=CARTESIAN_POINT('Ctrl Pts',(-8.93226653410931,19.9091994120708,
3.002946687963));
#100550=CARTESIAN_POINT('Ctrl Pts',(-8.93761240047505,19.9100491765944,
2.99158076800298));
#100551=CARTESIAN_POINT('Ctrl Pts',(-8.94104805609694,19.9105863410071,
2.98446309318307));
#100552=CARTESIAN_POINT('Ctrl Pts',(-8.95471086905163,19.912688732001,2.95687064307431));
#100553=CARTESIAN_POINT('Ctrl Pts',(-8.96546173993423,19.9142719213305,
2.93666233292482));
#100554=CARTESIAN_POINT('Ctrl Pts',(-8.99465638476766,19.9184010925096,
2.88544289330118));
#100555=CARTESIAN_POINT('Ctrl Pts',(-9.01394760968737,19.9209744989812,
2.85494459224756));
#100556=CARTESIAN_POINT('Ctrl Pts',(-9.0726024449445,19.9283784378158,2.77100819890187));
#100557=CARTESIAN_POINT('Ctrl Pts',(-9.11512363627019,19.9332845424425,
2.71994341536988));
#100558=CARTESIAN_POINT('Ctrl Pts',(-9.19328862141607,19.9414080419536,
2.64073719637236));
#100559=CARTESIAN_POINT('Ctrl Pts',(-9.22667392133962,19.9446511723571,
2.61057122740161));
#100560=CARTESIAN_POINT('Ctrl Pts',(-9.26638058771426,19.9481932641445,
2.57862406273584));
#100561=CARTESIAN_POINT('Ctrl Pts',(-9.27108396290685,19.9486080956115,
2.57489866798678));
#100562=CARTESIAN_POINT('Ctrl Pts',(-9.27865810334182,19.9492683105508,
2.56899306050476));
#100563=CARTESIAN_POINT('Ctrl Pts',(-9.28151068938987,19.9495152108158,
2.56678986038803));
#100564=CARTESIAN_POINT('Ctrl Pts',(-9.28659814469482,19.9499523785742,
2.56289771005367));
#100565=CARTESIAN_POINT('Ctrl Pts',(-9.28882897839037,19.950142999566,2.56120359628587));
#100566=CARTESIAN_POINT('Ctrl Pts',(-9.29363784592339,19.9505515880075,
2.5575786805811));
#100567=CARTESIAN_POINT('Ctrl Pts',(-9.29621776455562,19.9507693770259,
2.55565048752656));
#100568=CARTESIAN_POINT('Ctrl Pts',(-9.3034071771318,19.9513724662926,2.55032305334182));
#100569=CARTESIAN_POINT('Ctrl Pts',(-9.30803368176704,19.9517562304649,
2.54694675824155));
#100570=CARTESIAN_POINT('Ctrl Pts',(-9.33516370182266,19.9539826852576,
2.52744972804862));
#100571=CARTESIAN_POINT('Ctrl Pts',(-9.35820733967452,19.9557784206006,
2.51209119840029));
#100572=CARTESIAN_POINT('Ctrl Pts',(-9.43372348066762,19.9614378917222,
2.46551881474658));
#100573=CARTESIAN_POINT('Ctrl Pts',(-9.48808966504822,19.9651818522528,
2.43756445476573));
#100574=CARTESIAN_POINT('Ctrl Pts',(-9.61354454391748,19.9735993895092,
2.38493376537281));
#100575=CARTESIAN_POINT('Ctrl Pts',(-9.68531165407253,19.9782775217189,
2.3625952189228));
#100576=CARTESIAN_POINT('Ctrl Pts',(-9.76926308193124,19.9838973819999,
2.34502303630865));
#100577=CARTESIAN_POINT('Ctrl Pts',(-9.7798458273654,19.9846081061937,2.34295918836561));
#100578=CARTESIAN_POINT('Ctrl Pts',(-9.79415903839483,19.9855730677155,
2.34037129719402));
#100579=CARTESIAN_POINT('Ctrl Pts',(-9.79786609068529,19.985823321085,2.33971938221784));
#100580=CARTESIAN_POINT('Ctrl Pts',(-9.80475325438455,19.9862889044853,
2.33854222651863));
#100581=CARTESIAN_POINT('Ctrl Pts',(-9.80792268465862,19.9865034181986,
2.33801387450814));
#100582=CARTESIAN_POINT('Ctrl Pts',(-9.81110406371627,19.9867190062195,
2.33749693000169));
#100583=CARTESIAN_POINT('Origin',(-10.,12.3756328852638,3.5));
#100584=CARTESIAN_POINT('',(-9.81110406363821,20.5859883433483,2.33749693001438));
#100585=CARTESIAN_POINT('',(-9.81110406371067,20.4880078480432,2.3374969300026));
#100586=CARTESIAN_POINT('',(-9.81110406371068,12.3756328852638,2.3374969300026));
#100587=CARTESIAN_POINT('',(-11.1777499562264,20.2253931554249,3.50032110538681));
#100588=CARTESIAN_POINT('Ctrl Pts',(-9.81110406356574,20.5859883433483,
2.33749693002615));
#100589=CARTESIAN_POINT('Ctrl Pts',(-9.81073639201826,20.5859611875483,
2.33755667323291));
#100590=CARTESIAN_POINT('Ctrl Pts',(-9.81036874354825,20.5859340342295,
2.33761659172366));
#100591=CARTESIAN_POINT('Ctrl Pts',(-9.78819126391139,20.584296126581,2.34124182772966));
#100592=CARTESIAN_POINT('Ctrl Pts',(-9.76648498696821,20.5826957762589,
2.34542030371084));
#100593=CARTESIAN_POINT('Ctrl Pts',(-9.72358810022636,20.5795529188105,
2.35493736263092));
#100594=CARTESIAN_POINT('Ctrl Pts',(-9.70240198035234,20.5780105232236,
2.36025987622409));
#100595=CARTESIAN_POINT('Ctrl Pts',(-9.67606449026354,20.5761152783333,
2.36766114974818));
#100596=CARTESIAN_POINT('Ctrl Pts',(-9.67076481953176,20.5757350557232,
2.36919069459232));
#100597=CARTESIAN_POINT('Ctrl Pts',(-9.66240088682049,20.5751370078541,
2.37166840547774));
#100598=CARTESIAN_POINT('Ctrl Pts',(-9.65932949942044,20.5749178263563,
2.37259192876942));
#100599=CARTESIAN_POINT('Ctrl Pts',(-9.65384818347541,20.5745274876146,
2.37426452893913));
#100600=CARTESIAN_POINT('Ctrl Pts',(-9.65143690236066,20.5743560633141,
2.37500880090948));
#100601=CARTESIAN_POINT('Ctrl Pts',(-9.64565461365473,20.5739456596549,
2.37681395210539));
#100602=CARTESIAN_POINT('Ctrl Pts',(-9.64228596916589,20.5737071134228,
2.37788225930862));
#100603=CARTESIAN_POINT('Ctrl Pts',(-9.6320410580193,20.5729831544079,2.38118207877461));
#100604=CARTESIAN_POINT('Ctrl Pts',(-9.62518032564575,20.5725004321587,
2.38346180448838));
#100605=CARTESIAN_POINT('Ctrl Pts',(-9.56338174365886,20.568167534426,2.40463044101418));
#100606=CARTESIAN_POINT('Ctrl Pts',(-9.5098827134921,20.5645239770243,2.4274996833194));
#100607=CARTESIAN_POINT('Ctrl Pts',(-9.36826943834004,20.5546261007426,
2.50085617483137));
#100608=CARTESIAN_POINT('Ctrl Pts',(-9.28466172697889,20.5484529762735,
2.5589043661014));
#100609=CARTESIAN_POINT('Ctrl Pts',(-9.19949069819513,20.5409403722419,
2.63601910652487));
#100610=CARTESIAN_POINT('Ctrl Pts',(-9.18961845546957,20.5400490212924,
2.64527205835372));
#100611=CARTESIAN_POINT('Ctrl Pts',(-9.17528165568518,20.538722398289,2.65918119334069));
#100612=CARTESIAN_POINT('Ctrl Pts',(-9.17069218880232,20.5382926964171,
2.66370748862447));
#100613=CARTESIAN_POINT('Ctrl Pts',(-9.16260421545907,20.5375262914002,
2.67181618414751));
#100614=CARTESIAN_POINT('Ctrl Pts',(-9.15909093659463,20.5371902468025,
2.67538367796762));
#100615=CARTESIAN_POINT('Ctrl Pts',(-9.15174440813035,20.5364808495389,
2.68293934629228));
#100616=CARTESIAN_POINT('Ctrl Pts',(-9.14791630381486,20.5361072865817,
2.68693233131387));
#100617=CARTESIAN_POINT('Ctrl Pts',(-9.13785770776994,20.5351151891361,
2.69757321658443));
#100618=CARTESIAN_POINT('Ctrl Pts',(-9.13167609047031,20.5344946034875,
2.70426659313226));
#100619=CARTESIAN_POINT('Ctrl Pts',(-9.10236646992905,20.5314985774366,
2.73675091351327));
#100620=CARTESIAN_POINT('Ctrl Pts',(-9.0803084136442,20.5290797202521,2.76347974975143));
#100621=CARTESIAN_POINT('Ctrl Pts',(-9.01933954962103,20.521884405616,2.8443751124926));
#100622=CARTESIAN_POINT('Ctrl Pts',(-8.98381342920913,20.5170013789387,
2.900915767923));
#100623=CARTESIAN_POINT('Ctrl Pts',(-8.92503898786656,20.5075861273993,
3.01487587079966));
#100624=CARTESIAN_POINT('Ctrl Pts',(-8.90114669271512,20.5030719937658,
3.07173658175227));
#100625=CARTESIAN_POINT('Ctrl Pts',(-8.87874830853151,20.4980731418707,
3.13946602218613));
#100626=CARTESIAN_POINT('Ctrl Pts',(-8.87580224687535,20.4973952708207,
3.14876000779916));
#100627=CARTESIAN_POINT('Ctrl Pts',(-8.87189762322351,20.4964686300041,
3.16163070268488));
#100628=CARTESIAN_POINT('Ctrl Pts',(-8.87084010504099,20.4962145955425,
3.16517663402755));
#100629=CARTESIAN_POINT('Ctrl Pts',(-8.86905533645555,20.4957805918083,
3.17126572084837));
#100630=CARTESIAN_POINT('Ctrl Pts',(-8.86831991767989,20.4956001636798,
3.17380642262139));
#100631=CARTESIAN_POINT('Ctrl Pts',(-8.86680206358188,20.4952244321945,
3.17911717949799));
#100632=CARTESIAN_POINT('Ctrl Pts',(-8.86602121610177,20.4950292274547,
3.18188765269964));
#100633=CARTESIAN_POINT('Ctrl Pts',(-8.86413981711003,20.4945541044818,
3.18865787907789));
#100634=CARTESIAN_POINT('Ctrl Pts',(-8.86305021194824,20.4942748084008,
3.19266068899818));
#100635=CARTESIAN_POINT('Ctrl Pts',(-8.85920524850811,20.493273804736,3.20708599373197));
#100636=CARTESIAN_POINT('Ctrl Pts',(-8.85657177002975,20.4925586675594,
3.21754082879346));
#100637=CARTESIAN_POINT('Ctrl Pts',(-8.85035289272333,20.4907886984349,
3.24374351230246));
#100638=CARTESIAN_POINT('Ctrl Pts',(-8.84694705317454,20.4897422046864,
3.2595320915986));
#100639=CARTESIAN_POINT('Ctrl Pts',(-8.83343166562671,20.4851988191307,
3.32909865458305));
#100640=CARTESIAN_POINT('Ctrl Pts',(-8.82675138717847,20.4818211932636,
3.38347708022054));
#100641=CARTESIAN_POINT('Ctrl Pts',(-8.81961388951547,20.4734228332111,
3.51915056457533));
#100642=CARTESIAN_POINT('Ctrl Pts',(-8.8237354357337,20.4684056458646,3.60038767146555));
#100643=CARTESIAN_POINT('Ctrl Pts',(-8.83847783693928,20.4621336577842,
3.69541649029305));
#100644=CARTESIAN_POINT('Ctrl Pts',(-8.84106837096647,20.4611444515543,
3.71023507236384));
#100645=CARTESIAN_POINT('Ctrl Pts',(-8.8452125274448,20.4597050599514,3.73152794987668));
#100646=CARTESIAN_POINT('Ctrl Pts',(-8.84653840336031,20.4592620337759,
3.73804545861996));
#100647=CARTESIAN_POINT('Ctrl Pts',(-8.84896861495758,20.4584793414984,
3.74949418094076));
#100648=CARTESIAN_POINT('Ctrl Pts',(-8.85004962696088,20.4581404214439,
3.7544302141268));
#100649=CARTESIAN_POINT('Ctrl Pts',(-8.85234866049798,20.4574380799022,
3.76461384196006));
#100650=CARTESIAN_POINT('Ctrl Pts',(-8.85357098716073,20.457074528613,3.76986033289352));
#100651=CARTESIAN_POINT('Ctrl Pts',(-8.85680288337753,20.4561377687528,
3.78331397711061));
#100652=CARTESIAN_POINT('Ctrl Pts',(-8.85886483060423,20.4555629023922,
3.79150810583378));
#100653=CARTESIAN_POINT('Ctrl Pts',(-8.8680295003182,20.4531002816974,3.82634010419797));
#100654=CARTESIAN_POINT('Ctrl Pts',(-8.87597765704857,20.4511857484672,
3.85274442369307));
#100655=CARTESIAN_POINT('Ctrl Pts',(-8.9168572180483,20.44223147017,3.97307654656362));
#100656=CARTESIAN_POINT('Ctrl Pts',(-8.96068296716125,20.4348480785342,
4.06286221336357));
#100657=CARTESIAN_POINT('Ctrl Pts',(-9.02738149002707,20.4259856152306,
4.16452740842275));
#100658=CARTESIAN_POINT('Ctrl Pts',(-9.04002225594907,20.4243852649082,
4.18266116582207));
#100659=CARTESIAN_POINT('Ctrl Pts',(-9.0661541278816,20.4212424074616,4.21798598103389));
#100660=CARTESIAN_POINT('Ctrl Pts',(-9.07962872689841,20.419700011877,4.23517946835515));
#100661=CARTESIAN_POINT('Ctrl Pts',(-9.09709651131694,20.4178047669889,
4.25623460406264));
#100662=CARTESIAN_POINT('Ctrl Pts',(-9.10064818012581,20.417424544379,4.2604549910044));
#100663=CARTESIAN_POINT('Ctrl Pts',(-9.10631169703765,20.4168264965101,
4.26708967244059));
#100664=CARTESIAN_POINT('Ctrl Pts',(-9.10840392629794,20.4166073150124,
4.2695204938142));
#100665=CARTESIAN_POINT('Ctrl Pts',(-9.11216013350364,20.4162169762707,
4.27384869473795));
#100666=CARTESIAN_POINT('Ctrl Pts',(-9.11382027117275,20.4160455519702,
4.27574926315319));
#100667=CARTESIAN_POINT('Ctrl Pts',(-9.11781992301642,20.415635148311,4.28029857284411));
#100668=CARTESIAN_POINT('Ctrl Pts',(-9.12016526331128,20.4153966020788,
4.28294213575833));
#100669=CARTESIAN_POINT('Ctrl Pts',(-9.12734447967006,20.4146726430635,
4.29096122956591));
#100670=CARTESIAN_POINT('Ctrl Pts',(-9.13221609224328,20.4141899208141,
4.29630296982863));
#100671=CARTESIAN_POINT('Ctrl Pts',(-9.17667662839121,20.4098570230704,
4.34416147643956));
#100672=CARTESIAN_POINT('Ctrl Pts',(-9.21931738628219,20.4062134656592,
4.38374574424509));
#100673=CARTESIAN_POINT('Ctrl Pts',(-9.34390263378271,20.3963155893812,
4.48331486915842));
#100674=CARTESIAN_POINT('Ctrl Pts',(-9.43092347771074,20.390142464924,4.53610894636061));
#100675=CARTESIAN_POINT('Ctrl Pts',(-9.53600015323943,20.3826298609046,
4.58258129892083));
#100676=CARTESIAN_POINT('Ctrl Pts',(-9.54846704058526,20.3817385099534,
4.587840102455));
#100677=CARTESIAN_POINT('Ctrl Pts',(-9.567002835052,20.380411886948,4.59528538209383));
#100678=CARTESIAN_POINT('Ctrl Pts',(-9.57300384122338,20.3799821850758,
4.59763877969319));
#100679=CARTESIAN_POINT('Ctrl Pts',(-9.58370000472881,20.3792157800584,
4.60173247512458));
#100680=CARTESIAN_POINT('Ctrl Pts',(-9.58838754724043,20.3788797354607,
4.60349232902307));
#100681=CARTESIAN_POINT('Ctrl Pts',(-9.59827705223126,20.3781703381972,
4.60713338591671));
#100682=CARTESIAN_POINT('Ctrl Pts',(-9.60348131846986,20.3777967752402,
4.60900793250761));
#100683=CARTESIAN_POINT('Ctrl Pts',(-9.61729205581241,20.3768046777957,
4.61387284025146));
#100684=CARTESIAN_POINT('Ctrl Pts',(-9.62592021066983,20.3761840921479,
4.61680006173027));
#100685=CARTESIAN_POINT('Ctrl Pts',(-9.66751351904539,20.3731880661081,
4.6303750980549));
#100686=CARTESIAN_POINT('Ctrl Pts',(-9.70090068297981,20.3707692089342,
4.6396641134947));
#100687=CARTESIAN_POINT('Ctrl Pts',(-9.7995940032379,20.3635738943464,4.662487139047));
#100688=CARTESIAN_POINT('Ctrl Pts',(-9.86569352156252,20.3586908677085,
4.67196366563134));
#100689=CARTESIAN_POINT('Ctrl Pts',(-9.99370486433329,20.3492756161562,
4.67934175271247));
#100690=CARTESIAN_POINT('Ctrl Pts',(-10.0553679516324,20.3447614824703,
4.67805880004219));
#100691=CARTESIAN_POINT('Ctrl Pts',(-10.126354147867,20.3397626305271,4.67099305467454));
#100692=CARTESIAN_POINT('Ctrl Pts',(-10.1360432093052,20.3390847594772,
4.66990699008668));
#100693=CARTESIAN_POINT('Ctrl Pts',(-10.1493898054675,20.3381581186605,
4.66824288565207));
#100694=CARTESIAN_POINT('Ctrl Pts',(-10.1530594427439,20.337904084199,4.66776776876737));
#100695=CARTESIAN_POINT('Ctrl Pts',(-10.1593482735527,20.3374700804647,
4.66692338480501));
#100696=CARTESIAN_POINT('Ctrl Pts',(-10.161968545464,20.3372896523362,4.6665625782286));
#100697=CARTESIAN_POINT('Ctrl Pts',(-10.1674377517585,20.336913920851,4.66579069600065));
#100698=CARTESIAN_POINT('Ctrl Pts',(-10.1702864227244,20.3367187161112,
4.6653779996516));
#100699=CARTESIAN_POINT('Ctrl Pts',(-10.1772368627187,20.3362435931382,
4.66434503727578));
#100700=CARTESIAN_POINT('Ctrl Pts',(-10.1813369751643,20.3359642970572,
4.66371352749561));
#100701=CARTESIAN_POINT('Ctrl Pts',(-10.1960797090151,20.3349632933923,
4.6613630043238));
#100702=CARTESIAN_POINT('Ctrl Pts',(-10.2067023374316,20.3342481562155,
4.65951948849165));
#100703=CARTESIAN_POINT('Ctrl Pts',(-10.2331705512951,20.3324781870907,
4.6545507146789));
#100704=CARTESIAN_POINT('Ctrl Pts',(-10.2489803646816,20.331431693342,4.65124484413915));
#100705=CARTESIAN_POINT('Ctrl Pts',(-10.318034356667,20.3268883077846,4.63531629804634));
#100706=CARTESIAN_POINT('Ctrl Pts',(-10.3704332252228,20.3235106819161,
4.61931636456147));
#100707=CARTESIAN_POINT('Ctrl Pts',(-10.4972422789575,20.3151157560082,
4.57070967965573));
#100708=CARTESIAN_POINT('Ctrl Pts',(-10.5697429070831,20.3101020242223,
4.53395358826934));
#100709=CARTESIAN_POINT('Ctrl Pts',(-10.6503039417934,20.3038520009428,
4.48204781746084));
#100710=CARTESIAN_POINT('Ctrl Pts',(-10.6625656104499,20.3028811077379,
4.47381718645982));
#100711=CARTESIAN_POINT('Ctrl Pts',(-10.6797232635003,20.301492672393,4.46182606148965));
#100712=CARTESIAN_POINT('Ctrl Pts',(-10.6847497667246,20.301082197161,4.45825405923838));
#100713=CARTESIAN_POINT('Ctrl Pts',(-10.6938817081131,20.3003294969477,
4.45165605479284));
#100714=CARTESIAN_POINT('Ctrl Pts',(-10.6979960077748,20.2999877531958,
4.44864252656639));
#100715=CARTESIAN_POINT('Ctrl Pts',(-10.706111119976,20.2993083979176,4.44261722087401));
#100716=CARTESIAN_POINT('Ctrl Pts',(-10.7101125548101,20.2989708304174,
4.43960645857975));
#100717=CARTESIAN_POINT('Ctrl Pts',(-10.7195738353497,20.298166411297,4.43239263873652));
#100718=CARTESIAN_POINT('Ctrl Pts',(-10.7250161857706,20.2976986852138,
4.42816704539047));
#100719=CARTESIAN_POINT('Ctrl Pts',(-10.7367662851646,20.2966777604459,
4.41887753845133));
#100720=CARTESIAN_POINT('Ctrl Pts',(-10.74305953437,20.2961238765409,4.41379593582132));
#100721=CARTESIAN_POINT('Ctrl Pts',(-10.7603594095017,20.2945812436423,
4.39952994473833));
#100722=CARTESIAN_POINT('Ctrl Pts',(-10.77125114399,20.2935871237598,4.39020907371781));
#100723=CARTESIAN_POINT('Ctrl Pts',(-10.8063814603399,20.2903036980953,
4.35901674010213));
#100724=CARTESIAN_POINT('Ctrl Pts',(-10.8298794568478,20.2879831761069,
4.33633759967157));
#100725=CARTESIAN_POINT('Ctrl Pts',(-10.8880092789477,20.2819160964715,
4.27536892577747));
#100726=CARTESIAN_POINT('Ctrl Pts',(-10.9211203220358,20.2781283063199,
4.23572696446686));
#100727=CARTESIAN_POINT('Ctrl Pts',(-10.9869707754897,20.269923810293,4.14544713108034));
#100728=CARTESIAN_POINT('Ctrl Pts',(-11.0186466983019,20.2655179635429,
4.09420005360497));
#100729=CARTESIAN_POINT('Ctrl Pts',(-11.0507649879144,20.2606156713285,
4.03205622332839));
#100730=CARTESIAN_POINT('Ctrl Pts',(-11.0551510492866,20.2599349840516,
4.02330408316218));
#100731=CARTESIAN_POINT('Ctrl Pts',(-11.0610462800738,20.2590052211678,
4.01116492726664));
#100732=CARTESIAN_POINT('Ctrl Pts',(-11.0626491987577,20.2587508339966,
4.00782425369417));
#100733=CARTESIAN_POINT('Ctrl Pts',(-11.0653698643929,20.2583163851987,
4.00208477116824));
#100734=CARTESIAN_POINT('Ctrl Pts',(-11.0664953284914,20.2581358626886,
3.99968968375993));
#100735=CARTESIAN_POINT('Ctrl Pts',(-11.0688276000355,20.257760113066,3.99468262790467));
#100736=CARTESIAN_POINT('Ctrl Pts',(-11.0700329205486,20.2575649836713,
3.99207000531205));
#100737=CARTESIAN_POINT('Ctrl Pts',(-11.0729501651884,20.2570903355296,
3.98568525278006));
#100738=CARTESIAN_POINT('Ctrl Pts',(-11.074651807787,20.2568114359766,3.9819084094135));
#100739=CARTESIAN_POINT('Ctrl Pts',(-11.0806939252721,20.2558134563131,
3.96830659757076));
#100740=CARTESIAN_POINT('Ctrl Pts',(-11.0849200372567,20.255100894536,3.95843097886897));
#100741=CARTESIAN_POINT('Ctrl Pts',(-11.0951300998453,20.253338589886,3.93363966575459));
#100742=CARTESIAN_POINT('Ctrl Pts',(-11.1009451393259,20.2522970928123,
3.91865636169414));
#100743=CARTESIAN_POINT('Ctrl Pts',(-11.1250327618003,20.2477894196621,
3.8526143081343));
#100744=CARTESIAN_POINT('Ctrl Pts',(-11.1400745078617,20.2444406105812,
3.80044403117779));
#100745=CARTESIAN_POINT('Ctrl Pts',(-11.1689200755283,20.235952615356,3.66619924109002));
#100746=CARTESIAN_POINT('Ctrl Pts',(-11.1777273103824,20.2308183329953,
3.58338150555677));
#100747=CARTESIAN_POINT('Ctrl Pts',(-11.1777499562264,20.2253931554248,
3.50032110538561));
#100748=CARTESIAN_POINT('Ctrl Pts',(-11.1777499534635,20.2253938071954,
3.50033108412358));
#100749=CARTESIAN_POINT('Ctrl Pts',(-11.1777523518846,20.2248192267006,
3.49153415808618));
#100750=CARTESIAN_POINT('Ctrl Pts',(-11.1776563394807,20.2242418447553,
3.48273767565964));
#100751=CARTESIAN_POINT('Ctrl Pts',(-11.177311702439,20.2232141367527,3.46716407569449));
#100752=CARTESIAN_POINT('Ctrl Pts',(-11.1771031404095,20.2227650352233,
3.46038641281238));
#100753=CARTESIAN_POINT('Ctrl Pts',(-11.176641596819,20.2219858195418,3.44867756679113));
#100754=CARTESIAN_POINT('Ctrl Pts',(-11.1764161088448,20.2216565567637,
3.44374542585233));
#100755=CARTESIAN_POINT('Ctrl Pts',(-11.1759125429501,20.2210082332279,
3.43406538971739));
#100756=CARTESIAN_POINT('Ctrl Pts',(-11.1756367041683,20.2206892478258,
3.42931746908353));
#100757=CARTESIAN_POINT('Ctrl Pts',(-11.1749898935703,20.2200099539317,
3.41923883372543));
#100758=CARTESIAN_POINT('Ctrl Pts',(-11.1746113855777,20.2196494182659,
3.41390872742487));
#100759=CARTESIAN_POINT('Ctrl Pts',(-11.1735563648502,20.2187294442943,
3.40035784672447));
#100760=CARTESIAN_POINT('Ctrl Pts',(-11.1728297454345,20.2181684615175,
3.39214137779059));
#100761=CARTESIAN_POINT('Ctrl Pts',(-11.1696953433932,20.2159948809686,
3.36049082475049));
#100762=CARTESIAN_POINT('Ctrl Pts',(-11.1666711296417,20.2143633473612,
3.33712476093965));
#100763=CARTESIAN_POINT('Ctrl Pts',(-11.1453991290257,20.2049225232183,
3.20421887261046));
#100764=CARTESIAN_POINT('Ctrl Pts',(-11.1124310011361,20.1966476684144,
3.09761418234751));
#100765=CARTESIAN_POINT('Ctrl Pts',(-11.0496962918253,20.1859860650669,
2.96471931192452));
#100766=CARTESIAN_POINT('Ctrl Pts',(-11.0328656342338,20.1834132787226,
2.93292252538709));
#100767=CARTESIAN_POINT('Ctrl Pts',(-11.0114977457662,20.1804932262176,
2.89667189172198));
#100768=CARTESIAN_POINT('Ctrl Pts',(-11.0083497920221,20.1800709487296,
2.89142527417603));
#100769=CARTESIAN_POINT('Ctrl Pts',(-11.0034381886883,20.1794243934314,
2.88338197244157));
#100770=CARTESIAN_POINT('Ctrl Pts',(-11.0017034691587,20.1791983398307,
2.88056788024476));
#100771=CARTESIAN_POINT('Ctrl Pts',(-10.9984819636587,20.1787828117124,
2.87539082273478));
#100772=CARTESIAN_POINT('Ctrl Pts',(-10.9969986293577,20.1785931285669,
2.87302584627628));
#100773=CARTESIAN_POINT('Ctrl Pts',(-10.9936118006294,20.1781637298038,
2.86766841817856));
#100774=CARTESIAN_POINT('Ctrl Pts',(-10.9917031907188,20.1779243525982,
2.86467927621879));
#100775=CARTESIAN_POINT('Ctrl Pts',(-10.9867061658118,20.177304228134,2.85693064544739));
#100776=CARTESIAN_POINT('Ctrl Pts',(-10.9835967652343,20.17692480756,2.85218470301725));
#100777=CARTESIAN_POINT('Ctrl Pts',(-10.9621735290283,20.1743528001997,
2.81999584029923));
#100778=CARTESIAN_POINT('Ctrl Pts',(-10.9427459774541,20.1722270350799,
2.79330768335623));
#100779=CARTESIAN_POINT('Ctrl Pts',(-10.9029881733635,20.1681793530997,
2.74325458082259));
#100780=CARTESIAN_POINT('Ctrl Pts',(-10.8828080299801,20.166254594905,2.71980680567824));
#100781=CARTESIAN_POINT('Ctrl Pts',(-10.8287989665469,20.1613453636956,
2.66183481145911));
#100782=CARTESIAN_POINT('Ctrl Pts',(-10.7937276135609,20.1583766945129,
2.62855006666824));
#100783=CARTESIAN_POINT('Ctrl Pts',(-10.7292512219788,20.153116349402,2.5744882739032));
#100784=CARTESIAN_POINT('Ctrl Pts',(-10.7007559414711,20.150851067681,2.5527301848657));
#100785=CARTESIAN_POINT('Ctrl Pts',(-10.6587724170758,20.1475562426524,
2.52360511000773));
#100786=CARTESIAN_POINT('Ctrl Pts',(-10.6460625868608,20.1465641701671,
2.51514915858278));
#100787=CARTESIAN_POINT('Ctrl Pts',(-10.6260681542754,20.1450093039898,
2.50240032121892));
#100788=CARTESIAN_POINT('Ctrl Pts',(-10.6188953512204,20.1444526488642,
2.49793463729409));
#100789=CARTESIAN_POINT('Ctrl Pts',(-10.6053610733062,20.1434040053986,
2.4897091365988));
#100790=CARTESIAN_POINT('Ctrl Pts',(-10.5990110293552,20.1429126909859,
2.48593124478903));
#100791=CARTESIAN_POINT('Ctrl Pts',(-10.5882113704168,20.1420780469897,
2.47964293387874));
#100792=CARTESIAN_POINT('Ctrl Pts',(-10.5837801470256,20.1417358490932,
2.47710122827033));
#100793=CARTESIAN_POINT('Ctrl Pts',(-10.5748919949981,20.141049924237,2.47207963846551));
#100794=CARTESIAN_POINT('Ctrl Pts',(-10.5704352142344,20.140706207977,2.46959971830454));
#100795=CARTESIAN_POINT('Ctrl Pts',(-10.560553386624,20.1399445282237,2.46418485851698));
#100796=CARTESIAN_POINT('Ctrl Pts',(-10.5551211381641,20.1395260985697,
2.46126344724633));
#100797=CARTESIAN_POINT('Ctrl Pts',(-10.5365981999868,20.1381001203648,
2.45148878630345));
#100798=CARTESIAN_POINT('Ctrl Pts',(-10.5234020433121,20.1370855257098,
2.44483950984686));
#100799=CARTESIAN_POINT('Ctrl Pts',(-10.4369860569791,20.1304468619343,
2.40331618431191));
#100800=CARTESIAN_POINT('Ctrl Pts',(-10.3604680323456,20.1245713221996,
2.37584232468672));
#100801=CARTESIAN_POINT('Ctrl Pts',(-10.2286408593251,20.1146075391549,
2.34336251829231));
#100802=CARTESIAN_POINT('Ctrl Pts',(-10.174681864276,20.1105776391098,2.33399239900307));
#100803=CARTESIAN_POINT('Ctrl Pts',(-10.1042033625551,20.1054976724573,
2.32675773574855));
#100804=CARTESIAN_POINT('Ctrl Pts',(-10.0881088219053,20.1043501582151,
2.32543938343628));
#100805=CARTESIAN_POINT('Ctrl Pts',(-10.0612328296991,20.102459996989,2.3237934768731));
#100806=CARTESIAN_POINT('Ctrl Pts',(-10.0504651861512,20.1017096768983,
2.32328230650614));
#100807=CARTESIAN_POINT('Ctrl Pts',(-10.0355458261914,20.1006810306076,
2.32277922057519));
#100808=CARTESIAN_POINT('Ctrl Pts',(-10.0313992890752,20.1003963125062,
2.32266132517946));
#100809=CARTESIAN_POINT('Ctrl Pts',(-10.0243746095345,20.0999160532842,
2.32249873651406));
#100810=CARTESIAN_POINT('Ctrl Pts',(-10.0214967932199,20.0997198970324,
2.32244268264397));
#100811=CARTESIAN_POINT('Ctrl Pts',(-10.0159740566195,20.0993446305287,
2.32235536425518));
#100812=CARTESIAN_POINT('Ctrl Pts',(-10.0133292094032,20.0991654271388,
2.32232245877186));
#100813=CARTESIAN_POINT('Ctrl Pts',(-10.0069839998146,20.0987366840536,
2.32226489431862));
#100814=CARTESIAN_POINT('Ctrl Pts',(-10.0032835591551,20.0984876101652,
2.32224876371534));
#100815=CARTESIAN_POINT('Ctrl Pts',(-9.98983242764523,20.0975855260004,
2.32225352581305));
#100816=CARTESIAN_POINT('Ctrl Pts',(-9.98008184060888,20.0969379199024,
2.32237806612254));
#100817=CARTESIAN_POINT('Ctrl Pts',(-9.91697863991762,20.0927810965579,
2.32396808339277));
#100818=CARTESIAN_POINT('Ctrl Pts',(-9.86377934673636,20.0894339925388,
2.32893768609718));
#100819=CARTESIAN_POINT('Ctrl Pts',(-9.81110405611873,20.0861209582704,
2.33749693123622));
#100820=CARTESIAN_POINT('Ctrl Pts',(-9.81110406371629,19.9867190062195,
2.33749693000169));
#100821=CARTESIAN_POINT('Ctrl Pts',(-9.81408300875001,19.9869208761798,
2.33701287914126));
#100822=CARTESIAN_POINT('Ctrl Pts',(-9.81705392288393,19.9871224338232,
2.33654183422988));
#100823=CARTESIAN_POINT('Ctrl Pts',(-9.82309926517953,19.9875330584984,
2.33560711199982));
#100824=CARTESIAN_POINT('Ctrl Pts',(-9.82616391250262,19.9877414753334,
2.33514563915785));
#100825=CARTESIAN_POINT('Ctrl Pts',(-9.83479260505729,19.9883290187378,
2.33388114559629));
#100826=CARTESIAN_POINT('Ctrl Pts',(-9.84036056911844,19.9887090093696,
2.33310586763523));
#100827=CARTESIAN_POINT('Ctrl Pts',(-9.85546971521399,19.9897425786891,
2.33111224817086));
#100828=CARTESIAN_POINT('Ctrl Pts',(-9.86502044376763,19.9903985412879,
2.32997090231419));
#100829=CARTESIAN_POINT('Ctrl Pts',(-9.91336983910424,19.9937333288174,
2.32479283269449));
#100830=CARTESIAN_POINT('Ctrl Pts',(-9.95233393031936,19.9964676509658,
2.32256889282159));
#100831=CARTESIAN_POINT('Ctrl Pts',(-10.018655010393,20.0012028304539,2.32208082198291));
#100832=CARTESIAN_POINT('Ctrl Pts',(-10.0459743199467,20.0031764240022,
2.32283059498433));
#100833=CARTESIAN_POINT('Ctrl Pts',(-10.124754668176,20.0089225545093,2.32773925788832));
#100834=CARTESIAN_POINT('Ctrl Pts',(-10.176000535015,20.0127307415939,2.33433171477298));
#100835=CARTESIAN_POINT('Ctrl Pts',(-10.274516425143,20.0200715734531,2.35365126031592));
#100836=CARTESIAN_POINT('Ctrl Pts',(-10.3217628265244,20.0236003465914,
2.36600505292262));
#100837=CARTESIAN_POINT('Ctrl Pts',(-10.3742721558786,20.0274405126005,
2.38328272301918));
#100838=CARTESIAN_POINT('Ctrl Pts',(-10.3804159976824,20.0278885001588,
2.38536068754047));
#100839=CARTESIAN_POINT('Ctrl Pts',(-10.3897375670332,20.0285658396979,
2.38859947276409));
#100840=CARTESIAN_POINT('Ctrl Pts',(-10.3929278544304,20.028797235171,2.38972336553565));
#100841=CARTESIAN_POINT('Ctrl Pts',(-10.3987376679093,20.0292177997846,
2.39179825825361));
#100842=CARTESIAN_POINT('Ctrl Pts',(-10.4013586685951,20.0294072164162,
2.39274481362838));
#100843=CARTESIAN_POINT('Ctrl Pts',(-10.4072202674116,20.0298301334735,
2.39488523569953));
#100844=CARTESIAN_POINT('Ctrl Pts',(-10.4104589853413,20.0300633394703,
2.39608405637648));
#100845=CARTESIAN_POINT('Ctrl Pts',(-10.4198905754388,20.0307412275494,
2.39962243245576));
#100846=CARTESIAN_POINT('Ctrl Pts',(-10.4260691775891,20.0311837454883,
2.402000023942));
#100847=CARTESIAN_POINT('Ctrl Pts',(-10.4766953198986,20.0347993334587,
2.42197319592836));
#100848=CARTESIAN_POINT('Ctrl Pts',(-10.5200597499876,20.0378314754941,
2.44221019948332));
#100849=CARTESIAN_POINT('Ctrl Pts',(-10.5765731057789,20.041847787994,2.47290187046837));
#100850=CARTESIAN_POINT('Ctrl Pts',(-10.5909007814633,20.0428718525454,
2.48107733463048));
#100851=CARTESIAN_POINT('Ctrl Pts',(-10.6543390126385,20.0474517738232,
2.51906386232927));
#100852=CARTESIAN_POINT('Ctrl Pts',(-10.701398714838,20.0509786062734,2.55214198555983));
#100853=CARTESIAN_POINT('Ctrl Pts',(-10.768702724543,20.0564548063042,2.60721634288663));
#100854=CARTESIAN_POINT('Ctrl Pts',(-10.7908368869545,20.0583347070313,
2.62676271132575));
#100855=CARTESIAN_POINT('Ctrl Pts',(-10.8265638269669,20.06152904765,2.66078604611313));
#100856=CARTESIAN_POINT('Ctrl Pts',(-10.8405673593004,20.0628256887809,
2.67481259074185));
#100857=CARTESIAN_POINT('Ctrl Pts',(-10.859364479507,20.0646334520825,2.69461573330649));
#100858=CARTESIAN_POINT('Ctrl Pts',(-10.8644672203786,20.0651313392117,
2.7000952892779));
#100859=CARTESIAN_POINT('Ctrl Pts',(-10.8726631368383,20.0659429628049,
2.70906645928169));
#100860=CARTESIAN_POINT('Ctrl Pts',(-10.8757884822136,20.066255340196,2.71252850871705));
#100861=CARTESIAN_POINT('Ctrl Pts',(-10.8821691430148,20.0668991033908,
2.7196815486718));
#100862=CARTESIAN_POINT('Ctrl Pts',(-10.8854220477254,20.0672305803329,
2.72337455713588));
#100863=CARTESIAN_POINT('Ctrl Pts',(-10.8930565966765,20.0680164372405,
2.73215233893186));
#100864=CARTESIAN_POINT('Ctrl Pts',(-10.8974180674657,20.0684716303779,
2.73725435142679));
#100865=CARTESIAN_POINT('Ctrl Pts',(-10.9112304151462,20.0699335698288,
2.75369439265886));
#100866=CARTESIAN_POINT('Ctrl Pts',(-10.9205115355617,20.0709470651928,
2.765172532161));
#100867=CARTESIAN_POINT('Ctrl Pts',(-10.9796620141083,20.0776171570177,
2.8412046106869));
#100868=CARTESIAN_POINT('Ctrl Pts',(-11.0229166368048,20.0835284843486,
2.9106054093291));
#100869=CARTESIAN_POINT('Ctrl Pts',(-11.0824657962154,20.0935019930941,
3.03275624847548));
#100870=CARTESIAN_POINT('Ctrl Pts',(-11.1028729623652,20.0975054917523,
3.08320181648758));
#100871=CARTESIAN_POINT('Ctrl Pts',(-11.1247113915923,20.1025558120831,
3.1501740752645));
#100872=CARTESIAN_POINT('Ctrl Pts',(-11.1293853240724,20.103699116389,3.16557102945672));
#100873=CARTESIAN_POINT('Ctrl Pts',(-11.1366535284029,20.1055830474175,
3.19140743925264));
#100874=CARTESIAN_POINT('Ctrl Pts',(-11.1394228461299,20.1063312881727,
3.20179501940523));
#100875=CARTESIAN_POINT('Ctrl Pts',(-11.1430619584465,20.1073575239572,
3.21623674559256));
#100876=CARTESIAN_POINT('Ctrl Pts',(-11.1440530612351,20.1076418740774,
3.22025937051169));
#100877=CARTESIAN_POINT('Ctrl Pts',(-11.1456963428356,20.1081216472144,
3.22708384598744));
#100878=CARTESIAN_POINT('Ctrl Pts',(-11.1463595142758,20.1083176830717,
3.229882984959));
#100879=CARTESIAN_POINT('Ctrl Pts',(-11.1476127595621,20.1086928224003,
3.23526048233931));
#100880=CARTESIAN_POINT('Ctrl Pts',(-11.1482044099068,20.1088720183405,
3.23783842473664));
#100881=CARTESIAN_POINT('Ctrl Pts',(-11.1496033633604,20.1093008749394,
3.24402954109379));
#100882=CARTESIAN_POINT('Ctrl Pts',(-11.1504023303726,20.1095500688471,
3.24764459966185));
#100883=CARTESIAN_POINT('Ctrl Pts',(-11.1532479620208,20.1104536669804,
3.26081454202171));
#100884=CARTESIAN_POINT('Ctrl Pts',(-11.1551928111408,20.1111026411918,
3.27039135549404));
#100885=CARTESIAN_POINT('Ctrl Pts',(-11.1683076970161,20.1157257102722,
3.3393622053945));
#100886=CARTESIAN_POINT('Ctrl Pts',(-11.1750121087517,20.1194912788742,
3.39952190241154));
#100887=CARTESIAN_POINT('Ctrl Pts',(-11.1788398896702,20.1264591643744,
3.51198444674158));
#100888=CARTESIAN_POINT('Ctrl Pts',(-11.1771573165793,20.1296597207046,
3.56409033097425));
#100889=CARTESIAN_POINT('Ctrl Pts',(-11.1688640836789,20.1349485057596,
3.64794577320532));
#100890=CARTESIAN_POINT('Ctrl Pts',(-11.1643843926207,20.1369917582415,
3.67983310386289));
#100891=CARTESIAN_POINT('Ctrl Pts',(-11.1560551926117,20.1399894647762,
3.72546178889879));
#100892=CARTESIAN_POINT('Ctrl Pts',(-11.1532534539623,20.1409138732699,
3.73938059836828));
#100893=CARTESIAN_POINT('Ctrl Pts',(-11.1477711096285,20.1425877754625,
3.76428059411462));
#100894=CARTESIAN_POINT('Ctrl Pts',(-11.1451827087457,20.143334381969,3.7752804053697));
#100895=CARTESIAN_POINT('Ctrl Pts',(-11.1409780685346,20.1444851609889,
3.79206184151576));
#100896=CARTESIAN_POINT('Ctrl Pts',(-11.1394751874696,20.1448857183128,
3.79787139344392));
#100897=CARTESIAN_POINT('Ctrl Pts',(-11.1366589162444,20.1456174221612,
3.80842470196323));
#100898=CARTESIAN_POINT('Ctrl Pts',(-11.1353600517123,20.1459480956969,
3.81317222158315));
#100899=CARTESIAN_POINT('Ctrl Pts',(-11.132461868853,20.1466715344259,3.82351041838368));
#100900=CARTESIAN_POINT('Ctrl Pts',(-11.1308508351427,20.1470646699743,
3.82909764776214));
#100901=CARTESIAN_POINT('Ctrl Pts',(-11.1263171974171,20.1481470440211,
3.84439431831523));
#100902=CARTESIAN_POINT('Ctrl Pts',(-11.1233105327971,20.1488389822901,
3.8540781148118));
#100903=CARTESIAN_POINT('Ctrl Pts',(-11.1060586405339,20.1526736104553,
3.90720999113355));
#100904=CARTESIAN_POINT('Ctrl Pts',(-11.08941935221,20.155893639222,3.94983353891075));
#100905=CARTESIAN_POINT('Ctrl Pts',(-11.0360962360304,20.1650757658672,
4.06598498997737));
#100906=CARTESIAN_POINT('Ctrl Pts',(-10.9941393022134,20.1711714078078,
4.13680418674648));
#100907=CARTESIAN_POINT('Ctrl Pts',(-10.9295804304549,20.1790374335794,
4.22364202174625));
#100908=CARTESIAN_POINT('Ctrl Pts',(-10.9132995177798,20.1809194933138,
4.24408448819899));
#100909=CARTESIAN_POINT('Ctrl Pts',(-10.889715200559,20.1834931464585,4.27175551686923));
#100910=CARTESIAN_POINT('Ctrl Pts',(-10.8829778820513,20.1842121825738,
4.27945480422612));
#100911=CARTESIAN_POINT('Ctrl Pts',(-10.8710522641739,20.1854557171142,
4.29273008994474));
#100912=CARTESIAN_POINT('Ctrl Pts',(-10.8659087006168,20.185982913356,4.29834527132948));
#100913=CARTESIAN_POINT('Ctrl Pts',(-10.8582480389391,20.1867542555335,
4.30654719927686));
#100914=CARTESIAN_POINT('Ctrl Pts',(-10.8557730595638,20.1870013705768,
4.30917275807191));
#100915=CARTESIAN_POINT('Ctrl Pts',(-10.8513765439187,20.1874366033143,
4.31379402640196));
#100916=CARTESIAN_POINT('Ctrl Pts',(-10.8494599915744,20.1876250882883,
4.31579437374684));
#100917=CARTESIAN_POINT('Ctrl Pts',(-10.8452808539616,20.1880333853966,
4.32012553408611));
#100918=CARTESIAN_POINT('Ctrl Pts',(-10.8430156773208,20.1882529941397,
4.322453756858));
#100919=CARTESIAN_POINT('Ctrl Pts',(-10.8367505510495,20.1888558475691,
4.32884018092068));
#100920=CARTESIAN_POINT('Ctrl Pts',(-10.8327306730747,20.1892375929605,
4.33287883846769));
#100921=CARTESIAN_POINT('Ctrl Pts',(-10.8114767218962,20.191230638834,4.35392436846089));
#100922=CARTESIAN_POINT('Ctrl Pts',(-10.7937491855621,20.192806560208,4.37042732231724));
#100923=CARTESIAN_POINT('Ctrl Pts',(-10.6978053803539,20.2009741845307,
4.45437245742323));
#100924=CARTESIAN_POINT('Ctrl Pts',(-10.6114770902727,20.2071463496645,
4.51185899883369));
#100925=CARTESIAN_POINT('Ctrl Pts',(-10.4819244698483,20.2162628072759,
4.57541920215516));
#100926=CARTESIAN_POINT('Ctrl Pts',(-10.4441832936141,20.2188977988785,
4.59154857396462));
#100927=CARTESIAN_POINT('Ctrl Pts',(-10.3966876876106,20.2222308495901,
4.60897506787026));
#100928=CARTESIAN_POINT('Ctrl Pts',(-10.3876550550953,20.2228653870541,
4.61216472339869));
#100929=CARTESIAN_POINT('Ctrl Pts',(-10.3732508514827,20.2238787942883,
4.61705442713079));
#100930=CARTESIAN_POINT('Ctrl Pts',(-10.3679041268828,20.2242552914831,
4.61882677070917));
#100931=CARTESIAN_POINT('Ctrl Pts',(-10.3578011438012,20.2249674224564,
4.62209547880374));
#100932=CARTESIAN_POINT('Ctrl Pts',(-10.3530476810428,20.2253027771668,
4.62360013156433));
#100933=CARTESIAN_POINT('Ctrl Pts',(-10.342298847887,20.2260618413406,4.62692760528669));
#100934=CARTESIAN_POINT('Ctrl Pts',(-10.3362982351857,20.2264861106638,
4.62873283960243));
#100935=CARTESIAN_POINT('Ctrl Pts',(-10.3208411291097,20.2275804562918,
4.63324878254392));
#100936=CARTESIAN_POINT('Ctrl Pts',(-10.3113647224266,20.2282527763244,
4.63588900543347));
#100937=CARTESIAN_POINT('Ctrl Pts',(-10.2407967050034,20.2332708730553,
4.65460055847349));
#100938=CARTESIAN_POINT('Ctrl Pts',(-10.1785436077392,20.2377699938798,
4.665849600437));
#100939=CARTESIAN_POINT('Ctrl Pts',(-10.0413742919882,20.247797484014,4.67939013168238));
#100940=CARTESIAN_POINT('Ctrl Pts',(-9.96652313616605,20.2533444194973,
4.67964065471822));
#100941=CARTESIAN_POINT('Ctrl Pts',(-9.86406307194417,20.2607559088937,
4.67021874913391));
#100942=CARTESIAN_POINT('Ctrl Pts',(-9.83607242537982,20.2627599277497,
4.66662711229075));
#100943=CARTESIAN_POINT('Ctrl Pts',(-9.80255525819089,20.2651146206243,
4.66109593850998));
#100944=CARTESIAN_POINT('Ctrl Pts',(-9.79688197649627,20.2655116157713,
4.66011692359825));
#100945=CARTESIAN_POINT('Ctrl Pts',(-9.78803982648218,20.266127664956,4.65852421746741));
#100946=CARTESIAN_POINT('Ctrl Pts',(-9.78486601127488,20.2663482479126,
4.65793905070471));
#100947=CARTESIAN_POINT('Ctrl Pts',(-9.77894299369496,20.2667588382207,
4.65682181132248));
#100948=CARTESIAN_POINT('Ctrl Pts',(-9.77619330403156,20.2669490142444,
4.65629298460916));
#100949=CARTESIAN_POINT('Ctrl Pts',(-9.76991815316187,20.2673820542309,
4.65506290999898));
#100950=CARTESIAN_POINT('Ctrl Pts',(-9.76639399518316,20.2676245591421,
4.65435532557077));
#100951=CARTESIAN_POINT('Ctrl Pts',(-9.75702926421882,20.2682672567095,
4.65243042176241));
#100952=CARTESIAN_POINT('Ctrl Pts',(-9.75119451603392,20.268665920597,4.65118482020051));
#100953=CARTESIAN_POINT('Ctrl Pts',(-9.70483843885487,20.2718209449277,
4.64091981363938));
#100954=CARTESIAN_POINT('Ctrl Pts',(-9.66480537073408,20.2744711113973,
4.62980695412016));
#100955=CARTESIAN_POINT('Ctrl Pts',(-9.53209473436853,20.2832570607057,
4.58528947107605));
#100956=CARTESIAN_POINT('Ctrl Pts',(-9.44304826250539,20.2891869346684,
4.54239816186425));
#100957=CARTESIAN_POINT('Ctrl Pts',(-9.33604811866747,20.2973402573462,
4.47319182797513));
#100958=CARTESIAN_POINT('Ctrl Pts',(-9.31231178609172,20.2992199279908,
4.45656632586875));
#100959=CARTESIAN_POINT('Ctrl Pts',(-9.28236234030519,20.3016999669239,
4.43389779413292));
#100960=CARTESIAN_POINT('Ctrl Pts',(-9.27556786939737,20.3022701271856,
4.42863716388637));
#100961=CARTESIAN_POINT('Ctrl Pts',(-9.26458504300649,20.3032044681092,
4.41993980634557));
#100962=CARTESIAN_POINT('Ctrl Pts',(-9.26036168228592,20.3035668868986,
4.41654763300599));
#100963=CARTESIAN_POINT('Ctrl Pts',(-9.25225531093067,20.3042686700832,
4.40994413650025));
#100964=CARTESIAN_POINT('Ctrl Pts',(-9.24836920554888,20.3046078705389,
4.4067367859831));
#100965=CARTESIAN_POINT('Ctrl Pts',(-9.23946281579941,20.305391765671,4.39928940514371));
#100966=CARTESIAN_POINT('Ctrl Pts',(-9.23445723598799,20.3058371532488,
4.39503213136836));
#100967=CARTESIAN_POINT('Ctrl Pts',(-9.21844644696224,20.3072776016231,
4.3811822938852));
#100968=CARTESIAN_POINT('Ctrl Pts',(-9.20758425686547,20.3082793037851,
4.37142724768611));
#100969=CARTESIAN_POINT('Ctrl Pts',(-9.13049733805307,20.3155708501724,
4.29956430879739));
#100970=CARTESIAN_POINT('Ctrl Pts',(-9.07148163118422,20.3221840277917,
4.23019545948758));
#100971=CARTESIAN_POINT('Ctrl Pts',(-8.98373250859426,20.3337744633714,
4.0989955050327));
#100972=CARTESIAN_POINT('Ctrl Pts',(-8.95126630111046,20.3386971347639,
4.04014340697384));
#100973=CARTESIAN_POINT('Ctrl Pts',(-8.9210555250416,20.3438695204285,3.97225610637989));
#100974=CARTESIAN_POINT('Ctrl Pts',(-8.91818558161619,20.3443681380605,
3.96564426416064));
#100975=CARTESIAN_POINT('Ctrl Pts',(-8.91400110583827,20.3451057372637,
3.95575642344514));
#100976=CARTESIAN_POINT('Ctrl Pts',(-8.91264037301394,20.3453473362789,
3.9525003403922));
#100977=CARTESIAN_POINT('Ctrl Pts',(-8.91033219988537,20.3457601133023,
3.94690660046814));
#100978=CARTESIAN_POINT('Ctrl Pts',(-8.90937761380526,20.3459317132304,
3.94457196866307));
#100979=CARTESIAN_POINT('Ctrl Pts',(-8.90722572103314,20.3463205715296,
3.93926043824021));
#100980=CARTESIAN_POINT('Ctrl Pts',(-8.90603307456667,20.3465375506226,
3.93628170263555));
#100981=CARTESIAN_POINT('Ctrl Pts',(-8.90282003305195,20.3471262186187,
3.9281608403798));
#100982=CARTESIAN_POINT('Ctrl Pts',(-8.90082359108345,20.3474965213031,
3.92300923177427));
#100983=CARTESIAN_POINT('Ctrl Pts',(-8.89107253009644,20.349329021177,3.89731241876125));
#100984=CARTESIAN_POINT('Ctrl Pts',(-8.88385676699028,20.3507622587048,
3.87656569779962));
#100985=CARTESIAN_POINT('Ctrl Pts',(-8.87056402833909,20.3535925480839,
3.83459834429438));
#100986=CARTESIAN_POINT('Ctrl Pts',(-8.86449496176476,20.354988842516,3.81338486116286));
#100987=CARTESIAN_POINT('Ctrl Pts',(-8.83433743056372,20.3626184203353,
3.69555088010709));
#100988=CARTESIAN_POINT('Ctrl Pts',(-8.82198209778227,20.368615430995,3.59635181199653));
#100989=CARTESIAN_POINT('Ctrl Pts',(-8.82232944552952,20.3767569879161,
3.46933919565376));
#100990=CARTESIAN_POINT('Ctrl Pts',(-8.8233634238491,20.3785396462803,3.44191214365526));
#100991=CARTESIAN_POINT('Ctrl Pts',(-8.82596604229665,20.3809089681309,
3.40613593337647));
#100992=CARTESIAN_POINT('Ctrl Pts',(-8.82666831108206,20.3814687538488,
3.39773104833931));
#100993=CARTESIAN_POINT('Ctrl Pts',(-8.82796652857682,20.3823903804405,
3.38397597169515));
#100994=CARTESIAN_POINT('Ctrl Pts',(-8.82850900309326,20.3827505511097,
3.37862094163837));
#100995=CARTESIAN_POINT('Ctrl Pts',(-8.82963181697876,20.383451041018,3.368246800042));
#100996=CARTESIAN_POINT('Ctrl Pts',(-8.83020778602453,20.3837912164987,
3.36322732627408));
#100997=CARTESIAN_POINT('Ctrl Pts',(-8.83161728091387,20.384581864851,3.35160464816089));
#100998=CARTESIAN_POINT('Ctrl Pts',(-8.83247451198979,20.3850330690549,
3.34500454719157));
#100999=CARTESIAN_POINT('Ctrl Pts',(-8.83545608008461,20.3865121235132,
3.3234785788683));
#101000=CARTESIAN_POINT('Ctrl Pts',(-8.83781100190216,20.3875471233238,
3.30858670494187));
#101001=CARTESIAN_POINT('Ctrl Pts',(-8.85437118664686,20.3940947090039,
3.21548680961937));
#101002=CARTESIAN_POINT('Ctrl Pts',(-8.87617538606468,20.399847606979,3.13885309593576));
#101003=CARTESIAN_POINT('Ctrl Pts',(-8.92620128444489,20.4097850789373,
3.01298250203244));
#101004=CARTESIAN_POINT('Ctrl Pts',(-8.95056442064478,20.4139127774069,
2.96249162144857));
#101005=CARTESIAN_POINT('Ctrl Pts',(-8.98656465152177,20.4191018740922,
2.89974070847826));
#101006=CARTESIAN_POINT('Ctrl Pts',(-8.9949962953391,20.4202643623101,2.88572804625186));
#101007=CARTESIAN_POINT('Ctrl Pts',(-9.00951969146962,20.422176421368,2.86269144936422));
#101008=CARTESIAN_POINT('Ctrl Pts',(-9.01544944947884,20.4229338824131,
2.85356851481118));
#101009=CARTESIAN_POINT('Ctrl Pts',(-9.02382163013007,20.4239705398153,
2.84107042965553));
#101010=CARTESIAN_POINT('Ctrl Pts',(-9.02615658320928,20.4242562577699,
2.8376244347983));
#101011=CARTESIAN_POINT('Ctrl Pts',(-9.03013814158257,20.4247376586581,
2.83181489493639));
#101012=CARTESIAN_POINT('Ctrl Pts',(-9.03177522318189,20.4249339639694,
2.82944490064837));
#101013=CARTESIAN_POINT('Ctrl Pts',(-9.03492973482754,20.4253090837398,
2.82491376965978));
#101014=CARTESIAN_POINT('Ctrl Pts',(-9.03644575406605,20.4254879938058,
2.82275170682457));
#101015=CARTESIAN_POINT('Ctrl Pts',(-9.04009525359847,20.4259154687999,
2.81758405259375));
#101016=CARTESIAN_POINT('Ctrl Pts',(-9.04223561305342,20.4261635736663,
2.81458331837639));
#101017=CARTESIAN_POINT('Ctrl Pts',(-9.0500273488531,20.4270576235192,2.80376725143966));
#101018=CARTESIAN_POINT('Ctrl Pts',(-9.05576077101138,20.4276982915424,
2.7960111000178));
#101019=CARTESIAN_POINT('Ctrl Pts',(-9.1031808361541,20.4328674015646,2.73348316548014));
#101020=CARTESIAN_POINT('Ctrl Pts',(-9.14950639622086,20.4371231263793,
2.68238398189278));
#101021=CARTESIAN_POINT('Ctrl Pts',(-9.20411829190496,20.4417237355264,
2.63184201009508));
#101022=CARTESIAN_POINT('Ctrl Pts',(-9.20822645376329,20.4420674728578,
2.62809367461966));
#101023=CARTESIAN_POINT('Ctrl Pts',(-9.2753123662906,20.4476453646053,2.56774882981793));
#101024=CARTESIAN_POINT('Ctrl Pts',(-9.3441769549188,20.4528936258488,2.51808455820018));
#101025=CARTESIAN_POINT('Ctrl Pts',(-9.42762960266571,20.4591959935333,
2.47062350448235));
#101026=CARTESIAN_POINT('Ctrl Pts',(-9.43757425852956,20.4599457259568,
2.46515647951714));
#101027=CARTESIAN_POINT('Ctrl Pts',(-9.4529047014324,20.4611003228303,2.45701489633801));
#101028=CARTESIAN_POINT('Ctrl Pts',(-9.45823473956995,20.4615015340753,
2.45423635916133));
#101029=CARTESIAN_POINT('Ctrl Pts',(-9.46796793061911,20.4622339136259,
2.44925684888665));
#101030=CARTESIAN_POINT('Ctrl Pts',(-9.47236408450377,20.4625646043538,
2.44704243586168));
#101031=CARTESIAN_POINT('Ctrl Pts',(-9.48197568793369,20.4632874651336,
2.44227622395185));
#101032=CARTESIAN_POINT('Ctrl Pts',(-9.48719636264972,20.4636800014172,
2.43973531524629));
#101033=CARTESIAN_POINT('Ctrl Pts',(-9.50155067995783,20.4647591458223,
2.43287986859508));
#101034=CARTESIAN_POINT('Ctrl Pts',(-9.51072120002847,20.4654484273041,
2.42864415607073));
#101035=CARTESIAN_POINT('Ctrl Pts',(-9.56101938236463,20.4692291430415,
2.40619272905638));
#101036=CARTESIAN_POINT('Ctrl Pts',(-9.60310528787536,20.4723953026317,
2.39022885037411));
#101037=CARTESIAN_POINT('Ctrl Pts',(-9.70005177390833,20.4796933059368,
2.35967622004625));
#101038=CARTESIAN_POINT('Ctrl Pts',(-9.7552330849743,20.4838522304599,2.34657544438436));
#101039=CARTESIAN_POINT('Ctrl Pts',(-9.81110406371067,20.4880078480432,
2.3374969300026));
#101040=CARTESIAN_POINT('Origin',(-10.,12.3756328852638,3.5));
#101041=CARTESIAN_POINT('',(-9.81110406342901,21.0876323086995,2.33749693004837));
#101042=CARTESIAN_POINT('',(-9.81110406371115,20.988570409963,2.33749693000252));
#101043=CARTESIAN_POINT('',(-9.81110406371068,12.3756328852638,2.3374969300026));
#101044=CARTESIAN_POINT('Ctrl Pts',(-9.81110406314734,21.0876323086995,
2.33749693009414));
#101045=CARTESIAN_POINT('Ctrl Pts',(-9.78669199051518,21.0859356484233,
2.34146366484929));
#101046=CARTESIAN_POINT('Ctrl Pts',(-9.76241192458018,21.0842152344288,
2.34619821170569));
#101047=CARTESIAN_POINT('Ctrl Pts',(-9.64130261182356,21.0754627572677,
2.37379915618023));
#101048=CARTESIAN_POINT('Ctrl Pts',(-9.54750680248557,21.0680820720503,
2.40810433745266));
#101049=CARTESIAN_POINT('Ctrl Pts',(-9.43952359959329,21.0592221588631,
2.46392575164076));
#101050=CARTESIAN_POINT('Ctrl Pts',(-9.42017684661617,21.0576215132717,
2.47462745874384));
#101051=CARTESIAN_POINT('Ctrl Pts',(-9.3823584273696,21.0544801858814,2.49695972201989));
#101052=CARTESIAN_POINT('Ctrl Pts',(-9.3638852206975,21.0529395630909,2.50857221755907));
#101053=CARTESIAN_POINT('Ctrl Pts',(-9.34115921590794,21.0510461726802,
2.52375500780569));
#101054=CARTESIAN_POINT('Ctrl Pts',(-9.33659597150281,21.0506660938874,
2.52685018546233));
#101055=CARTESIAN_POINT('Ctrl Pts',(-9.3294134132817,21.0500682215491,2.5317960054331));
#101056=CARTESIAN_POINT('Ctrl Pts',(-9.3267797034674,21.0498490730532,2.533625446143));
#101057=CARTESIAN_POINT('Ctrl Pts',(-9.32208668480273,21.0494587621584,
2.53691383128695));
#101058=CARTESIAN_POINT('Ctrl Pts',(-9.32002460373643,21.0492873329456,
2.53836862990898));
#101059=CARTESIAN_POINT('Ctrl Pts',(-9.3150855375975,21.048876877795,2.54187697286218));
#101060=CARTESIAN_POINT('Ctrl Pts',(-9.31221310412364,21.0486382852997,
2.54393685217884));
#101061=CARTESIAN_POINT('Ctrl Pts',(-9.30349134601167,21.0479140445281,
2.55025104902241));
#101062=CARTESIAN_POINT('Ctrl Pts',(-9.29767176419438,21.0474310898435,
2.55454644183668));
#101063=CARTESIAN_POINT('Ctrl Pts',(-9.24537163718046,21.0430897716534,
2.59389821806427));
#101064=CARTESIAN_POINT('Ctrl Pts',(-9.20150380175031,21.0394389045419,
2.63230757303238));
#101065=CARTESIAN_POINT('Ctrl Pts',(-9.08965148198178,21.0295439043259,
2.74594117131653));
#101066=CARTESIAN_POINT('Ctrl Pts',(-9.02825244561503,21.0233798784461,
2.82691473257492));
#101067=CARTESIAN_POINT('Ctrl Pts',(-8.97122768240046,21.0158767722741,
2.92649655635056));
#101068=CARTESIAN_POINT('Ctrl Pts',(-8.96469762492873,21.0149840942198,
2.93837054138884));
#101069=CARTESIAN_POINT('Ctrl Pts',(-8.9553640054531,21.0136558697823,2.95605854900735));
#101070=CARTESIAN_POINT('Ctrl Pts',(-8.9524008723563,21.0132259133756,2.96178746931989));
#101071=CARTESIAN_POINT('Ctrl Pts',(-8.94722110563449,21.012459222582,2.97200687770881));
#101072=CARTESIAN_POINT('Ctrl Pts',(-8.94498575674969,21.0121231485311,
2.97648774339135));
#101073=CARTESIAN_POINT('Ctrl Pts',(-8.94034228998832,21.0114138621029,
2.98594632966647));
#101074=CARTESIAN_POINT('Ctrl Pts',(-8.93794052322276,21.0110404405146,
2.99092701471001));
#101075=CARTESIAN_POINT('Ctrl Pts',(-8.9316784008216,21.0100491233369,3.0041503597757));
#101076=CARTESIAN_POINT('Ctrl Pts',(-8.92787843399149,21.0094291823531,
3.01242103759702));
#101077=CARTESIAN_POINT('Ctrl Pts',(-8.91012395421612,21.0064416101893,
3.05227520173655));
#101078=CARTESIAN_POINT('Ctrl Pts',(-8.89746831222553,21.004030860246,3.08441518026381));
#101079=CARTESIAN_POINT('Ctrl Pts',(-8.86469628629428,20.996872323369,3.17973098606907));
#101080=CARTESIAN_POINT('Ctrl Pts',(-8.84847909249629,20.9920193651218,
3.24410053370179));
#101081=CARTESIAN_POINT('Ctrl Pts',(-8.8277159923457,20.9825942490547,3.37076540366857));
#101082=CARTESIAN_POINT('Ctrl Pts',(-8.82253212118833,20.9780401745215,
3.43275166958482));
#101083=CARTESIAN_POINT('Ctrl Pts',(-8.82221868157714,20.9730046328318,
3.50461158542088));
#101084=CARTESIAN_POINT('Ctrl Pts',(-8.8222972006709,20.9723267763767,3.51436080324933));
#101085=CARTESIAN_POINT('Ctrl Pts',(-8.82257251350386,20.9714001517486,
3.52780769143182));
#101086=CARTESIAN_POINT('Ctrl Pts',(-8.82266568946645,20.971146119123,3.53150675848965));
#101087=CARTESIAN_POINT('Ctrl Pts',(-8.82285536156098,20.9707121177052,
3.53784915383879));
#101088=CARTESIAN_POINT('Ctrl Pts',(-8.82294333124047,20.9705316900678,
3.54049268001567));
#101089=CARTESIAN_POINT('Ctrl Pts',(-8.8231456298481,20.9701559586746,3.54601237969055));
#101090=CARTESIAN_POINT('Ctrl Pts',(-8.82326159811414,20.9699607535405,
3.54888845874206));
#101091=CARTESIAN_POINT('Ctrl Pts',(-8.82357043861667,20.9694856280864,
3.55590848502478));
#101092=CARTESIAN_POINT('Ctrl Pts',(-8.82377466590847,20.969206329934,3.56005194700047));
#101093=CARTESIAN_POINT('Ctrl Pts',(-8.82458839400337,20.9682053104522,
3.57495892906291));
#101094=CARTESIAN_POINT('Ctrl Pts',(-8.82532380242086,20.967490159803,3.58571543497015));
#101095=CARTESIAN_POINT('Ctrl Pts',(-8.82752953646553,20.9657201505589,
3.6125561386714));
#101096=CARTESIAN_POINT('Ctrl Pts',(-8.8291832165579,20.9646736306487,3.62862342797687));
#101097=CARTESIAN_POINT('Ctrl Pts',(-8.83788757522245,20.9601300574398,
3.69895713798967));
#101098=CARTESIAN_POINT('Ctrl Pts',(-8.84838514535335,20.9567522800959,
3.75273188740912));
#101099=CARTESIAN_POINT('Ctrl Pts',(-8.88363617234454,20.9483539718096,
3.88393927337368));
#101100=CARTESIAN_POINT('Ctrl Pts',(-8.91272408536712,20.9433369819059,
3.959898404717));
#101101=CARTESIAN_POINT('Ctrl Pts',(-8.95618275692231,20.9370652111846,
4.04568022285635));
#101102=CARTESIAN_POINT('Ctrl Pts',(-8.96323716672006,20.9360759993633,
4.05896702636032));
#101103=CARTESIAN_POINT('Ctrl Pts',(-8.97377471958143,20.934636601082,4.07792817233288));
#101104=CARTESIAN_POINT('Ctrl Pts',(-8.97705470975434,20.9341935739138,
4.08371416691566));
#101105=CARTESIAN_POINT('Ctrl Pts',(-8.98291255601862,20.9334108804781,
4.09384655172591));
#101106=CARTESIAN_POINT('Ctrl Pts',(-8.98546972927173,20.933071960265,4.09820475099651));
#101107=CARTESIAN_POINT('Ctrl Pts',(-8.99081087149148,20.9323696189764,
4.10717492146276));
#101108=CARTESIAN_POINT('Ctrl Pts',(-8.9935985916655,20.9320060681025,4.11178450943681));
#101109=CARTESIAN_POINT('Ctrl Pts',(-9.00083984051157,20.9310693105475,
4.12357472070711));
#101110=CARTESIAN_POINT('Ctrl Pts',(-9.00533913346802,20.9304944460926,
4.13072673220846));
#101111=CARTESIAN_POINT('Ctrl Pts',(-9.02484482951817,20.9280318452134,
4.16100488266863));
#101112=CARTESIAN_POINT('Ctrl Pts',(-9.04058268662516,20.9261173304307,
4.18364702908351));
#101113=CARTESIAN_POINT('Ctrl Pts',(-9.11673357592585,20.9171630595168,
4.28539172899552));
#101114=CARTESIAN_POINT('Ctrl Pts',(-9.1862215247651,20.9097796539466,4.35718049325871));
#101115=CARTESIAN_POINT('Ctrl Pts',(-9.28113739330453,20.9009171775087,
4.43317736478721));
#101116=CARTESIAN_POINT('Ctrl Pts',(-9.29877456296343,20.8993168287003,
4.44650220380941));
#101117=CARTESIAN_POINT('Ctrl Pts',(-9.33456543634704,20.8961739633963,
4.47199219586792));
#101118=CARTESIAN_POINT('Ctrl Pts',(-9.35270420292256,20.8946315587097,
4.48416476650416));
#101119=CARTESIAN_POINT('Ctrl Pts',(-9.37583613841283,20.892736304301,4.49877172580266));
#101120=CARTESIAN_POINT('Ctrl Pts',(-9.38052066368577,20.8923560809533,
4.50168400269279));
#101121=CARTESIAN_POINT('Ctrl Pts',(-9.38796114902377,20.8917580321838,
4.50623744381136));
#101122=CARTESIAN_POINT('Ctrl Pts',(-9.39070357622337,20.8915388505167,
4.50790040035192));
#101123=CARTESIAN_POINT('Ctrl Pts',(-9.39561597200463,20.8911485116321,
4.51085180792733));
#101124=CARTESIAN_POINT('Ctrl Pts',(-9.39778327729904,20.8909770873568,
4.51214448077551));
#101125=CARTESIAN_POINT('Ctrl Pts',(-9.40299563997969,20.8905666839615,
4.51523068565759));
#101126=CARTESIAN_POINT('Ctrl Pts',(-9.40604463233112,20.8903281379665,
4.5170174890443));
#101127=CARTESIAN_POINT('Ctrl Pts',(-9.41535513971012,20.8896041803956,
4.52241758147703));
#101128=CARTESIAN_POINT('Ctrl Pts',(-9.42164206456965,20.8891214593377,
4.52598705088422));
#101129=CARTESIAN_POINT('Ctrl Pts',(-9.4787423845804,20.8847886046984,4.55771470497031));
#101130=CARTESIAN_POINT('Ctrl Pts',(-9.53154880003644,20.8811450847087,
4.58213921619906));
#101131=CARTESIAN_POINT('Ctrl Pts',(-9.68085334373629,20.8712471936509,
4.63820800628006));
#101132=CARTESIAN_POINT('Ctrl Pts',(-9.77995017932046,20.8650740225832,
4.66144224191181));
#101133=CARTESIAN_POINT('Ctrl Pts',(-9.8942555546854,20.8575613699168,4.67307128342787));
#101134=CARTESIAN_POINT('Ctrl Pts',(-9.90773820770885,20.856670025786,4.67420861041895));
#101135=CARTESIAN_POINT('Ctrl Pts',(-9.92766854568426,20.8553434110113,
4.67554445834274));
#101136=CARTESIAN_POINT('Ctrl Pts',(-9.93410338948209,20.8549137104477,
4.67592272142389));
#101137=CARTESIAN_POINT('Ctrl Pts',(-9.94554154627658,20.8541473068993,
4.67650091780684));
#101138=CARTESIAN_POINT('Ctrl Pts',(-9.95054367834808,20.8538112624526,
4.6767218038702));
#101139=CARTESIAN_POINT('Ctrl Pts',(-9.96107465919125,20.8531018646175,
4.67711956866531));
#101140=CARTESIAN_POINT('Ctrl Pts',(-9.96660363597277,20.8527283009321,
4.67728940458727));
#101141=CARTESIAN_POINT('Ctrl Pts',(-9.98124212897334,20.8517361994674,
4.67763585965445));
#101142=CARTESIAN_POINT('Ctrl Pts',(-9.99035269901281,20.8511156104981,
4.67774572685489));
#101143=CARTESIAN_POINT('Ctrl Pts',(-10.0341058688489,20.8481195408211,
4.6777656611274));
#101144=CARTESIAN_POINT('Ctrl Pts',(-10.0687287069652,20.8457006417903,
4.67625299079235));
#101145=CARTESIAN_POINT('Ctrl Pts',(-10.1696393247567,20.838505136811,4.66737384005766));
#101146=CARTESIAN_POINT('Ctrl Pts',(-10.2354242297465,20.8336219543693,
4.65590344173378));
#101147=CARTESIAN_POINT('Ctrl Pts',(-10.3594212786417,20.8242067540599,
4.62325536219842));
#101148=CARTESIAN_POINT('Ctrl Pts',(-10.4176497959986,20.8196928272384,
4.60293085007448));
#101149=CARTESIAN_POINT('Ctrl Pts',(-10.4829510851236,20.8146941652146,
4.57421988169029));
#101150=CARTESIAN_POINT('Ctrl Pts',(-10.4918268526413,20.8140162939421,
4.57018524907338));
#101151=CARTESIAN_POINT('Ctrl Pts',(-10.5040010719596,20.8130896528785,
4.56446778876622));
#101152=CARTESIAN_POINT('Ctrl Pts',(-10.5073429199312,20.8128356183889,
4.56287906950114));
#101153=CARTESIAN_POINT('Ctrl Pts',(-10.5130606598763,20.8124016146193,
4.56012773644353));
#101154=CARTESIAN_POINT('Ctrl Pts',(-10.5154401985236,20.8122211864834,
4.55897283269668));
#101155=CARTESIAN_POINT('Ctrl Pts',(-10.5204011105725,20.8118454549967,
4.55654438227177));
#101156=CARTESIAN_POINT('Ctrl Pts',(-10.5229817313711,20.8116502502629,
4.55526937626742));
#101157=CARTESIAN_POINT('Ctrl Pts',(-10.5292700937233,20.8111751273278,
4.55213375538536));
#101158=CARTESIAN_POINT('Ctrl Pts',(-10.532972776506,20.8108958312784,4.55026296332753));
#101159=CARTESIAN_POINT('Ctrl Pts',(-10.5462617468962,20.8098948278548,
4.54346029340332));
#101160=CARTESIAN_POINT('Ctrl Pts',(-10.5557904501707,20.8091796908837,
4.5384162344275));
#101161=CARTESIAN_POINT('Ctrl Pts',(-10.5794166621264,20.807409722371,4.52549119459981));
#101162=CARTESIAN_POINT('Ctrl Pts',(-10.5934241990498,20.8063632290216,
4.51744957267208));
#101163=CARTESIAN_POINT('Ctrl Pts',(-10.6541448030729,20.8018198463276,
4.48090953759299));
#101164=CARTESIAN_POINT('Ctrl Pts',(-10.6990077672982,20.7984422227704,
4.44946197147516));
#101165=CARTESIAN_POINT('Ctrl Pts',(-10.8045597075815,20.7900438619284,
4.36392233407427));
#101166=CARTESIAN_POINT('Ctrl Pts',(-10.8621398859975,20.7850266715709,
4.30646812406288));
#101167=CARTESIAN_POINT('Ctrl Pts',(-10.922852734733,20.7787546801758,4.23189081830266));
#101168=CARTESIAN_POINT('Ctrl Pts',(-10.9321248877533,20.7777654740312,
4.22004479028557));
#101169=CARTESIAN_POINT('Ctrl Pts',(-10.9451656558038,20.7763260825301,
4.20270988425559));
#101170=CARTESIAN_POINT('Ctrl Pts',(-10.9491188571776,20.7758830563697,
4.19736123367942));
#101171=CARTESIAN_POINT('Ctrl Pts',(-10.9559953557734,20.7751003641099,
4.18789059843499));
#101172=CARTESIAN_POINT('Ctrl Pts',(-10.9589378493359,20.7747614440578,
4.18378271067947));
#101173=CARTESIAN_POINT('Ctrl Pts',(-10.9649625165531,20.7740591025123,
4.1752565616609));
#101174=CARTESIAN_POINT('Ctrl Pts',(-10.9680409878828,20.7736955512168,
4.17083584171462));
#101175=CARTESIAN_POINT('Ctrl Pts',(-10.9758698911761,20.7727587913214,
4.15942733684858));
#101176=CARTESIAN_POINT('Ctrl Pts',(-10.9805755791749,20.7721839249317,
4.15240936851923));
#101177=CARTESIAN_POINT('Ctrl Pts',(-11.0003111616451,20.7697213039345,
4.12228020687205));
#101178=CARTESIAN_POINT('Ctrl Pts',(-11.0146015177673,20.7678067704228,
4.09869743298553));
#101179=CARTESIAN_POINT('Ctrl Pts',(-11.0766083272837,20.7588524920129,
3.98776450673754));
#101180=CARTESIAN_POINT('Ctrl Pts',(-11.113953782313,20.7514691005898,3.89509585705224));
#101181=CARTESIAN_POINT('Ctrl Pts',(-11.1448082671561,20.7426066374866,
3.77748418685354));
#101182=CARTESIAN_POINT('Ctrl Pts',(-11.1498136030304,20.741006287141,3.75595354011343));
#101183=CARTESIAN_POINT('Ctrl Pts',(-11.1585547229448,20.7378634298144,
3.71289184036065));
#101184=CARTESIAN_POINT('Ctrl Pts',(-11.1623033640226,20.7363210343686,
3.69137142142811));
#101185=CARTESIAN_POINT('Ctrl Pts',(-11.16624662239,20.7344257896258,3.66429942793547));
#101186=CARTESIAN_POINT('Ctrl Pts',(-11.1670033169644,20.7340455670272,
3.65883559880181));
#101187=CARTESIAN_POINT('Ctrl Pts',(-11.1681392529466,20.7334475191722,
3.65018666432755));
#101188=CARTESIAN_POINT('Ctrl Pts',(-11.1685439058007,20.733228337677,3.64700506541206));
#101189=CARTESIAN_POINT('Ctrl Pts',(-11.169243730342,20.7328379989375,3.64131712544456));
#101190=CARTESIAN_POINT('Ctrl Pts',(-11.169543841876,20.7326665746366,3.6388115016741));
#101191=CARTESIAN_POINT('Ctrl Pts',(-11.1702448973753,20.7322561709733,
3.63279469558978));
#101192=CARTESIAN_POINT('Ctrl Pts',(-11.1706380941375,20.7320176247375,
3.62928265306836));
#101193=CARTESIAN_POINT('Ctrl Pts',(-11.1717874707703,20.7312936657002,
3.61858097313007));
#101194=CARTESIAN_POINT('Ctrl Pts',(-11.1724932855425,20.7308109434326,
3.61138593125368));
#101195=CARTESIAN_POINT('Ctrl Pts',(-11.1782718619546,20.726478045031,3.54631838721667));
#101196=CARTESIAN_POINT('Ctrl Pts',(-11.1791231006365,20.7228344870486,
3.48814257594677));
#101197=CARTESIAN_POINT('Ctrl Pts',(-11.1696622566802,20.7129366109962,
3.32893834853862));
#101198=CARTESIAN_POINT('Ctrl Pts',(-11.1506102412773,20.7067634872503,
3.22895404992128));
#101199=CARTESIAN_POINT('Ctrl Pts',(-11.1147732947727,20.6992508839734,
3.11979133640583));
#101200=CARTESIAN_POINT('Ctrl Pts',(-11.1103320394087,20.6983595329181,
3.10701035095923));
#101201=CARTESIAN_POINT('Ctrl Pts',(-11.1034513351487,20.697032909787,3.08825764846938));
#101202=CARTESIAN_POINT('Ctrl Pts',(-11.1011813325995,20.6966032078948,
3.08222460216686));
#101203=CARTESIAN_POINT('Ctrl Pts',(-11.0970602809505,20.6958368028551,
3.07153894836502));
#101204=CARTESIAN_POINT('Ctrl Pts',(-11.0952288558923,20.695500758255,3.06687890296038));
#101205=CARTESIAN_POINT('Ctrl Pts',(-11.0913117058529,20.6947913610003,
3.05709547118812));
#101206=CARTESIAN_POINT('Ctrl Pts',(-11.0892194942599,20.6944177980544,
3.05197483051768));
#101207=CARTESIAN_POINT('Ctrl Pts',(-11.0835858855088,20.6934257006712,
3.0384594237697));
#101208=CARTESIAN_POINT('Ctrl Pts',(-11.0799830721792,20.6928051150741,
3.03009082743686));
#101209=CARTESIAN_POINT('Ctrl Pts',(-11.0622170021731,20.6898090897004,
2.99010769568831));
#101210=CARTESIAN_POINT('Ctrl Pts',(-11.046761923195,20.6873902331655,2.95908950041533));
#101211=CARTESIAN_POINT('Ctrl Pts',(-10.9976332173596,20.6801949214837,
2.87050268350627));
#101212=CARTESIAN_POINT('Ctrl Pts',(-10.9604146532626,20.675311897224,2.81506149664753));
#101213=CARTESIAN_POINT('Ctrl Pts',(-10.8801839534461,20.6658966448895,
2.71503961143204));
#101214=CARTESIAN_POINT('Ctrl Pts',(-10.8379440639796,20.6613825080462,
2.67009765805338));
#101215=CARTESIAN_POINT('Ctrl Pts',(-10.7851665871949,20.6563836532042,
2.62210277644192));
#101216=CARTESIAN_POINT('Ctrl Pts',(-10.777872524441,20.6557057821577,2.61563330231711));
#101217=CARTESIAN_POINT('Ctrl Pts',(-10.7677001892355,20.6547791413448,
2.6068341848783));
#101218=CARTESIAN_POINT('Ctrl Pts',(-10.7648902605897,20.6545251068836,
2.60442663949853));
#101219=CARTESIAN_POINT('Ctrl Pts',(-10.7600523560907,20.6540911031498,
2.60032090482777));
#101220=CARTESIAN_POINT('Ctrl Pts',(-10.7580299423317,20.6539106750215,
2.5986162497739));
#101221=CARTESIAN_POINT('Ctrl Pts',(-10.7537946744062,20.6535349435363,
2.59507075611822));
#101222=CARTESIAN_POINT('Ctrl Pts',(-10.7515807928218,20.6533397387963,
2.59323119832141));
#101223=CARTESIAN_POINT('Ctrl Pts',(-10.7461598347427,20.6528646158228,
2.58876031015327));
#101224=CARTESIAN_POINT('Ctrl Pts',(-10.7429455160034,20.6525853197413,
2.58613773855769));
#101225=CARTESIAN_POINT('Ctrl Pts',(-10.7313285422993,20.6515843160726,
2.57676122085405));
#101226=CARTESIAN_POINT('Ctrl Pts',(-10.722846798229,20.6508691788926,2.57010548620676));
#101227=CARTESIAN_POINT('Ctrl Pts',(-10.7014342159617,20.6490992097581,
2.55377280770514));
#101228=CARTESIAN_POINT('Ctrl Pts',(-10.6883931772399,20.6480527160031,
2.5442433642989));
#101229=CARTESIAN_POINT('Ctrl Pts',(-10.6303265089846,20.6435093304007,
2.50361782394039));
#101230=CARTESIAN_POINT('Ctrl Pts',(-10.5833583672972,20.6401317044958,
2.47541085614956));
#101231=CARTESIAN_POINT('Ctrl Pts',(-10.462299862807,20.6317333444562,2.41374176612588));
#101232=CARTESIAN_POINT('Ctrl Pts',(-10.3864012965253,20.6267161571588,
2.38448664390032));
#101233=CARTESIAN_POINT('Ctrl Pts',(-10.2935846581144,20.6204441691326,
2.35932941281007));
#101234=CARTESIAN_POINT('Ctrl Pts',(-10.2789924953926,20.6194549629014,
2.35567290780066));
#101235=CARTESIAN_POINT('Ctrl Pts',(-10.2578535063922,20.6180155712967,
2.3508042518414));
#101236=CARTESIAN_POINT('Ctrl Pts',(-10.2513597709488,20.6175725451209,
2.34936645240946));
#101237=CARTESIAN_POINT('Ctrl Pts',(-10.239911688272,20.6167898528432,2.34693322938069));
#101238=CARTESIAN_POINT('Ctrl Pts',(-10.2349624180284,20.6164509327887,
2.34591453677483));
#101239=CARTESIAN_POINT('Ctrl Pts',(-10.2247235247551,20.615748591247,2.34387569014433));
#101240=CARTESIAN_POINT('Ctrl Pts',(-10.2194331602217,20.6153850399579,
2.34285991818444));
#101241=CARTESIAN_POINT('Ctrl Pts',(-10.2058273920115,20.6144482800983,
2.34034421409722));
#101242=CARTESIAN_POINT('Ctrl Pts',(-10.1975025981861,20.6138734137381,
2.33889743161582));
#101243=CARTESIAN_POINT('Ctrl Pts',(-10.16195271686,20.6114107930482,2.33311251902508));
#101244=CARTESIAN_POINT('Ctrl Pts',(-10.1345973676973,20.6094962598224,
2.32964176231973));
#101245=CARTESIAN_POINT('Ctrl Pts',(-10.0084090380317,20.6005682353893,
2.3181138105309));
#101246=CARTESIAN_POINT('Ctrl Pts',(-9.90893778836096,20.5932142303674,
2.32159985969802));
#101247=CARTESIAN_POINT('Ctrl Pts',(-9.81110406356574,20.5859883433483,
2.33749693002615));
#101248=CARTESIAN_POINT('Ctrl Pts',(-9.81110406371067,20.4880078480432,
2.3374969300026));
#101249=CARTESIAN_POINT('Ctrl Pts',(-9.8367688653645,20.4899167657576,2.33332663844536));
#101250=CARTESIAN_POINT('Ctrl Pts',(-9.8625792519295,20.4918241056207,2.33000503893528));
#101251=CARTESIAN_POINT('Ctrl Pts',(-9.91463091193593,20.4956255539049,
2.32505466557443));
#101252=CARTESIAN_POINT('Ctrl Pts',(-9.94084622985053,20.4975173421905,
2.32344339867565));
#101253=CARTESIAN_POINT('Ctrl Pts',(-9.97735538488933,20.5001029330583,
2.32242297945779));
#101254=CARTESIAN_POINT('Ctrl Pts',(-9.98761936861823,20.500824430773,2.32227033911966));
#101255=CARTESIAN_POINT('Ctrl Pts',(-10.0055186560579,20.502071795745,2.32223818678792));
#101256=CARTESIAN_POINT('Ctrl Pts',(-10.0131530979203,20.5026003824754,
2.32229870173733));
#101257=CARTESIAN_POINT('Ctrl Pts',(-10.0243980035323,20.5033733614566,
2.32249719924083));
#101258=CARTESIAN_POINT('Ctrl Pts',(-10.0280090966784,20.5036207404338,
2.32257756104498));
#101259=CARTESIAN_POINT('Ctrl Pts',(-10.0344146930225,20.504057984682,2.32274959828643));
#101260=CARTESIAN_POINT('Ctrl Pts',(-10.0372092988945,20.5042482088913,
2.32283461310697));
#101261=CARTESIAN_POINT('Ctrl Pts',(-10.0432576214514,20.5046587396627,
2.32304017013204));
#101262=CARTESIAN_POINT('Ctrl Pts',(-10.0465111511223,20.5048788495448,
2.32316425257967));
#101263=CARTESIAN_POINT('Ctrl Pts',(-10.0554902725033,20.5054844157735,
2.32354399189579));
#101264=CARTESIAN_POINT('Ctrl Pts',(-10.0612146713599,20.5058683507546,
2.32382795617791));
#101265=CARTESIAN_POINT('Ctrl Pts',(-10.0915815731029,20.5078948468639,
2.32555664015501));
#101266=CARTESIAN_POINT('Ctrl Pts',(-10.1161781609322,20.5095006017224,
2.32773414647287));
#101267=CARTESIAN_POINT('Ctrl Pts',(-10.2427526680802,20.5176627460296,
2.34296336822354));
#101268=CARTESIAN_POINT('Ctrl Pts',(-10.3427737739851,20.523808994165,2.36855297663871));
#101269=CARTESIAN_POINT('Ctrl Pts',(-10.476228585395,20.5328926521535,2.42204859696507));
#101270=CARTESIAN_POINT('Ctrl Pts',(-10.5134243088481,20.5355240344521,
2.43926072632925));
#101271=CARTESIAN_POINT('Ctrl Pts',(-10.5581138524258,20.5388530341706,
2.46284250135655));
#101272=CARTESIAN_POINT('Ctrl Pts',(-10.5665274360215,20.5394873217159,
2.46741421443008));
#101273=CARTESIAN_POINT('Ctrl Pts',(-10.5797996117623,20.5405004218694,
2.47483699243526));
#101274=CARTESIAN_POINT('Ctrl Pts',(-10.5846952270175,20.5408768644156,
2.47762126806619));
#101275=CARTESIAN_POINT('Ctrl Pts',(-10.5938869645842,20.5415889495649,
2.482936483509));
#101276=CARTESIAN_POINT('Ctrl Pts',(-10.5981873644444,20.5419243135208,
2.48545980908448));
#101277=CARTESIAN_POINT('Ctrl Pts',(-10.6078570255081,20.5426834763975,
2.49121648420734));
#101278=CARTESIAN_POINT('Ctrl Pts',(-10.6132167239919,20.5431078357741,
2.49446551925175));
#101279=CARTESIAN_POINT('Ctrl Pts',(-10.6269251041777,20.5442025687766,
2.50292586431846));
#101280=CARTESIAN_POINT('Ctrl Pts',(-10.635234717728,20.5448751888077,2.50819923298898));
#101281=CARTESIAN_POINT('Ctrl Pts',(-10.6966403883498,20.5499145881241,
2.54825618553653));
#101282=CARTESIAN_POINT('Ctrl Pts',(-10.7469040976486,20.5544362763313,
2.5871714491312));
#101283=CARTESIAN_POINT('Ctrl Pts',(-10.8487600637358,20.5644684224261,
2.68009765299182));
#101284=CARTESIAN_POINT('Ctrl Pts',(-10.8988590583217,20.5699952926391,
2.73535251369354));
#101285=CARTESIAN_POINT('Ctrl Pts',(-10.9602686012246,20.5773841979994,
2.81752474544325));
#101286=CARTESIAN_POINT('Ctrl Pts',(-10.9763152413395,20.5793849670838,
2.84068436430025));
#101287=CARTESIAN_POINT('Ctrl Pts',(-10.9946228561666,20.581736382843,2.8692436683158));
#101288=CARTESIAN_POINT('Ctrl Pts',(-10.9976929049926,20.5821332047154,
2.87411099491157));
#101289=CARTESIAN_POINT('Ctrl Pts',(-11.0024285983117,20.5827490446988,
2.88174246512797));
#101290=CARTESIAN_POINT('Ctrl Pts',(-11.0041187149545,20.5829695900886,
2.88449120148253));
#101291=CARTESIAN_POINT('Ctrl Pts',(-11.0072544171624,20.5833801485293,
2.88963826890152));
#101292=CARTESIAN_POINT('Ctrl Pts',(-11.0087027355991,20.5835703299706,
2.89203479120434));
#101293=CARTESIAN_POINT('Ctrl Pts',(-11.0119910985509,20.584003429901,2.89752012098032));
#101294=CARTESIAN_POINT('Ctrl Pts',(-11.0138255580918,20.5842459889622,
2.90061220667193));
#101295=CARTESIAN_POINT('Ctrl Pts',(-11.0186678149814,20.5848889264806,
2.9088599391441));
#101296=CARTESIAN_POINT('Ctrl Pts',(-11.0216506750877,20.5852877743589,
2.91403021358801));
#101297=CARTESIAN_POINT('Ctrl Pts',(-11.0451027827353,20.5884480326347,
2.95540391806346));
#101298=CARTESIAN_POINT('Ctrl Pts',(-11.0636830910198,20.5911028574166,
2.9926501902343));
#101299=CARTESIAN_POINT('Ctrl Pts',(-11.1195236602504,20.5999001260097,
3.12121543004571));
#101300=CARTESIAN_POINT('Ctrl Pts',(-11.1472862253339,20.6058368508171,
3.2161939511381));
#101301=CARTESIAN_POINT('Ctrl Pts',(-11.1674551277628,20.6139886567099,
3.34196957809833));
#101302=CARTESIAN_POINT('Ctrl Pts',(-11.1709710869934,20.6158580953257,
3.37057207799114));
#101303=CARTESIAN_POINT('Ctrl Pts',(-11.1741682671452,20.6183264736807,
3.40781811257545));
#101304=CARTESIAN_POINT('Ctrl Pts',(-11.1748083983981,20.6188955664282,
3.41637081531469));
#101305=CARTESIAN_POINT('Ctrl Pts',(-11.1757001041675,20.6198285984352,
3.43033198180438));
#101306=CARTESIAN_POINT('Ctrl Pts',(-11.176007902314,20.620190785339,3.43573663774638));
#101307=CARTESIAN_POINT('Ctrl Pts',(-11.176530298103,20.6208924292544,3.44617693267445));
#101308=CARTESIAN_POINT('Ctrl Pts',(-11.1767498525556,20.6212317243772,
3.45121221382854));
#101309=CARTESIAN_POINT('Ctrl Pts',(-11.1771814960005,20.6220162878001,
3.46282368527109));
#101310=CARTESIAN_POINT('Ctrl Pts',(-11.1773708084431,20.6224622528056,
3.46940050205389));
#101311=CARTESIAN_POINT('Ctrl Pts',(-11.1778037200537,20.6239065026286,
3.49062125976624));
#101312=CARTESIAN_POINT('Ctrl Pts',(-11.1778292663653,20.6249114779892,
3.50526776684372));
#101313=CARTESIAN_POINT('Ctrl Pts',(-11.1760585623524,20.6321588531749,
3.60999444967978));
#101314=CARTESIAN_POINT('Ctrl Pts',(-11.164203775215,20.6387190329531,3.69958965366465));
#101315=CARTESIAN_POINT('Ctrl Pts',(-11.1257664630346,20.6503042282052,
3.85260280017017));
#101316=CARTESIAN_POINT('Ctrl Pts',(-11.1036382937098,20.655274555616,3.91672946722192));
#101317=CARTESIAN_POINT('Ctrl Pts',(-11.0731897566169,20.6604902367094,
3.98519148125711));
#101318=CARTESIAN_POINT('Ctrl Pts',(-11.0701998569949,20.6609889377655,
3.99175125805172));
#101319=CARTESIAN_POINT('Ctrl Pts',(-11.065656714068,20.6617266357524,4.0014810914199));
#101320=CARTESIAN_POINT('Ctrl Pts',(-11.0641492149745,20.6619682511247,
4.00467213751262));
#101321=CARTESIAN_POINT('Ctrl Pts',(-11.0615397501101,20.6623810463519,
4.01013212329531));
#101322=CARTESIAN_POINT('Ctrl Pts',(-11.060444817488,20.6625526482349,4.01240434598668));
#101323=CARTESIAN_POINT('Ctrl Pts',(-11.0579404988381,20.662941497775,4.01755894085841));
#101324=CARTESIAN_POINT('Ctrl Pts',(-11.056526629411,20.6631584662363,4.02043908222931));
#101325=CARTESIAN_POINT('Ctrl Pts',(-11.0526464772791,20.663747077036,4.028262218281));
#101326=CARTESIAN_POINT('Ctrl Pts',(-11.0501571214138,20.6641173336036,
4.03319377407471));
#101327=CARTESIAN_POINT('Ctrl Pts',(-11.0376036523578,20.6659492322764,
4.05763391574211));
#101328=CARTESIAN_POINT('Ctrl Pts',(-11.0270294717712,20.6673819374167,
4.07687740211616));
#101329=CARTESIAN_POINT('Ctrl Pts',(-11.004762407217,20.6702118242537,4.11484489007165));
#101330=CARTESIAN_POINT('Ctrl Pts',(-10.9930690558708,20.6716082293708,
4.13355795401394));
#101331=CARTESIAN_POINT('Ctrl Pts',(-10.9257473074405,20.6792371285798,
4.23484601747686));
#101332=CARTESIAN_POINT('Ctrl Pts',(-10.8603502715243,20.685233345798,4.31043484337156));
#101333=CARTESIAN_POINT('Ctrl Pts',(-10.7657791081188,20.6933750035747,
4.39522697423042));
#101334=CARTESIAN_POINT('Ctrl Pts',(-10.7447022177137,20.6951587683679,
4.41283481310521));
#101335=CARTESIAN_POINT('Ctrl Pts',(-10.7163714195351,20.6975293550459,
4.43486802143705));
#101336=CARTESIAN_POINT('Ctrl Pts',(-10.7096569472813,20.6980892623452,
4.4399751269331));
#101337=CARTESIAN_POINT('Ctrl Pts',(-10.6985692081646,20.6990110378513,
4.4482220726343));
#101338=CARTESIAN_POINT('Ctrl Pts',(-10.6942281723531,20.6993712347896,
4.4514048984));
#101339=CARTESIAN_POINT('Ctrl Pts',(-10.6857707134083,20.7000717390455,
4.45751716247405));
#101340=CARTESIAN_POINT('Ctrl Pts',(-10.6816569519441,20.7004119023647,
4.46045009568194));
#101341=CARTESIAN_POINT('Ctrl Pts',(-10.6720813548095,20.70120246812,4.46718457263074));
#101342=CARTESIAN_POINT('Ctrl Pts',(-10.666605960808,20.7016536014184,4.47096644374171));
#101343=CARTESIAN_POINT('Ctrl Pts',(-10.6486267859144,20.7031321810286,
4.4831609577789));
#101344=CARTESIAN_POINT('Ctrl Pts',(-10.6359939781741,20.7041667705274,
4.49137974528929));
#101345=CARTESIAN_POINT('Ctrl Pts',(-10.5554821045012,20.7107366545475,
4.54158780089417));
#101346=CARTESIAN_POINT('Ctrl Pts',(-10.4836511126367,20.7165144601256,
4.57682068307146));
#101347=CARTESIAN_POINT('Ctrl Pts',(-10.3420275033499,20.7275946246151,
4.62924105330901));
#101348=CARTESIAN_POINT('Ctrl Pts',(-10.2731202322393,20.7328535035932,
4.647856772218));
#101349=CARTESIAN_POINT('Ctrl Pts',(-10.191628991443,20.7386693490162,4.66211249168484));
#101350=CARTESIAN_POINT('Ctrl Pts',(-10.1802806184288,20.7394701285077,
4.66392698962636));
#101351=CARTESIAN_POINT('Ctrl Pts',(-10.1646987256062,20.7405555494079,
4.6661850083173));
#101352=CARTESIAN_POINT('Ctrl Pts',(-10.1604871120029,20.7408475213601,
4.66677205663001));
#101353=CARTESIAN_POINT('Ctrl Pts',(-10.1533997190042,20.7413363935927,
4.66772085212518));
#101354=CARTESIAN_POINT('Ctrl Pts',(-10.1505256469116,20.7415339601047,
4.66809481315633));
#101355=CARTESIAN_POINT('Ctrl Pts',(-10.1450486253927,20.7419091240841,
4.66878690738286));
#101356=CARTESIAN_POINT('Ctrl Pts',(-10.142445958736,20.74208683103,4.66910696165161));
#101357=CARTESIAN_POINT('Ctrl Pts',(-10.1362525066815,20.7425084036835,
4.66984759143203));
#101358=CARTESIAN_POINT('Ctrl Pts',(-10.1326607842979,20.7427518377742,
4.67026033425424));
#101359=CARTESIAN_POINT('Ctrl Pts',(-10.1199335018557,20.7436109287352,
4.6716635418858));
#101360=CARTESIAN_POINT('Ctrl Pts',(-10.1107880236469,20.7442218336206,
4.67256365580787));
#101361=CARTESIAN_POINT('Ctrl Pts',(-10.0230935293739,20.7500263970944,
4.68015948742423));
#101362=CARTESIAN_POINT('Ctrl Pts',(-9.94405766944615,20.7548575072673,
4.67906060174838));
#101363=CARTESIAN_POINT('Ctrl Pts',(-9.7854191155167,20.7647309284812,4.66085420586738));
#101364=CARTESIAN_POINT('Ctrl Pts',(-9.7062965599428,20.7697563286272,4.64339986845356));
#101365=CARTESIAN_POINT('Ctrl Pts',(-9.6187844980767,20.7758078957804,4.6144053852409));
#101366=CARTESIAN_POINT('Ctrl Pts',(-9.60803248210983,20.7765598602351,
4.6106691999123));
#101367=CARTESIAN_POINT('Ctrl Pts',(-9.59168132916687,20.7777171826537,
4.60472039038266));
#101368=CARTESIAN_POINT('Ctrl Pts',(-9.586041995808,20.7781188601552,4.6026196290512));
#101369=CARTESIAN_POINT('Ctrl Pts',(-9.57622719731688,20.778822487287,4.5988775184938));
#101370=CARTESIAN_POINT('Ctrl Pts',(-9.57204451424204,20.7791237953439,
4.59725534411934));
#101371=CARTESIAN_POINT('Ctrl Pts',(-9.56262378810786,20.7798057694444,
4.5935396340685));
#101372=CARTESIAN_POINT('Ctrl Pts',(-9.55739134348373,20.7801868902638,
4.59143229623557));
#101373=CARTESIAN_POINT('Ctrl Pts',(-9.54328057766385,20.7812211479528,
4.58563110652246));
#101374=CARTESIAN_POINT('Ctrl Pts',(-9.53443218967265,20.781876658423,4.5818660428249));
#101375=CARTESIAN_POINT('Ctrl Pts',(-9.49238672129402,20.7850256794751,
4.56336401268124));
#101376=CARTESIAN_POINT('Ctrl Pts',(-9.45984029088913,20.787566807976,4.54720640821779));
#101377=CARTESIAN_POINT('Ctrl Pts',(-9.35910668954076,20.7957715993893,
4.491251108654));
#101378=CARTESIAN_POINT('Ctrl Pts',(-9.29415054255041,20.8015963585646,
4.44609562928631));
#101379=CARTESIAN_POINT('Ctrl Pts',(-9.19828206009965,20.8108344645681,
4.36404812852664));
#101380=CARTESIAN_POINT('Ctrl Pts',(-9.16423835392765,20.8142659561741,
4.33116439182139));
#101381=CARTESIAN_POINT('Ctrl Pts',(-9.12581283732179,20.8182446058098,
4.28929260992186));
#101382=CARTESIAN_POINT('Ctrl Pts',(-9.11944976186729,20.8189071842837,
4.28218751727656));
#101383=CARTESIAN_POINT('Ctrl Pts',(-9.11057362648706,20.8198358394714,
4.27203069752461));
#101384=CARTESIAN_POINT('Ctrl Pts',(-9.10798874194613,20.8201068203273,
4.26904264411427));
#101385=CARTESIAN_POINT('Ctrl Pts',(-9.10357062155876,20.8205708345567,
4.26388317615764));
#101386=CARTESIAN_POINT('Ctrl Pts',(-9.10173013264509,20.8207643883875,
4.26171804722446));
#101387=CARTESIAN_POINT('Ctrl Pts',(-9.09791276827517,20.8211663444236,
4.25719426800012));
#101388=CARTESIAN_POINT('Ctrl Pts',(-9.09593728488424,20.8213746483992,
4.25483451220988));
#101389=CARTESIAN_POINT('Ctrl Pts',(-9.09072759071522,20.8219248436071,
4.24856163416063));
#101390=CARTESIAN_POINT('Ctrl Pts',(-9.087509347654,20.8222656106025,4.24463524368693));
#101391=CARTESIAN_POINT('Ctrl Pts',(-9.07379722871105,20.8237219905988,
4.22768349145525));
#101392=CARTESIAN_POINT('Ctrl Pts',(-9.06355550127781,20.824821138523,4.21445546284441));
#101393=CARTESIAN_POINT('Ctrl Pts',(-8.98746808428698,20.8331147779856,
4.11173374650378));
#101394=CARTESIAN_POINT('Ctrl Pts',(-8.93429645710424,20.8397177421073,
4.01353798502857));
#101395=CARTESIAN_POINT('Ctrl Pts',(-8.88111974510063,20.8493760551488,
3.87007450989365));
#101396=CARTESIAN_POINT('Ctrl Pts',(-8.86867289843669,20.8520638670126,
3.83007053489452));
#101397=CARTESIAN_POINT('Ctrl Pts',(-8.85601480671824,20.8554561853596,
3.78015310424117));
#101398=CARTESIAN_POINT('Ctrl Pts',(-8.85376140333662,20.8560943262768,
3.77078580960637));
#101399=CARTESIAN_POINT('Ctrl Pts',(-8.85037039066297,20.8571121610184,
3.75588803929416));
#101400=CARTESIAN_POINT('Ctrl Pts',(-8.84915715843412,20.8574894459042,
3.75037507753535));
#101401=CARTESIAN_POINT('Ctrl Pts',(-8.84694740443567,20.8582022412135,
3.73997836747467));
#101402=CARTESIAN_POINT('Ctrl Pts',(-8.84594215928674,20.8585374665223,
3.73509658433723));
#101403=CARTESIAN_POINT('Ctrl Pts',(-8.84374674489691,20.8592951266807,
3.72408147173955));
#101404=CARTESIAN_POINT('Ctrl Pts',(-8.84257433982359,20.8597181129003,
3.71794479683222));
#101405=CARTESIAN_POINT('Ctrl Pts',(-8.83969283270423,20.8608069433553,
3.7021828492199));
#101406=CARTESIAN_POINT('Ctrl Pts',(-8.83805467422681,20.8614749933599,
3.69254525928092));
#101407=CARTESIAN_POINT('Ctrl Pts',(-8.82719874844838,20.8662795359316,
3.62348426713597));
#101408=CARTESIAN_POINT('Ctrl Pts',(-8.82242551438339,20.8705542842563,
3.56346170745649));
#101409=CARTESIAN_POINT('Ctrl Pts',(-8.82203501085231,20.8805375701437,
3.42598683872903));
#101410=CARTESIAN_POINT('Ctrl Pts',(-8.82943731780189,20.8862874589667,
3.34879781870742));
#101411=CARTESIAN_POINT('Ctrl Pts',(-8.84987800239737,20.8939265285851,
3.24478425553931));
#101412=CARTESIAN_POINT('Ctrl Pts',(-8.85642619911104,20.8959625499864,
3.21688348762403));
#101413=CARTESIAN_POINT('Ctrl Pts',(-8.86551145253675,20.8983494830781,
3.18367071219165));
#101414=CARTESIAN_POINT('Ctrl Pts',(-8.86707786727827,20.8987481641312,
3.1781057203367));
#101415=CARTESIAN_POINT('Ctrl Pts',(-8.86958395688524,20.8993662484761,
3.1694473099146));
#101416=CARTESIAN_POINT('Ctrl Pts',(-8.87049547170255,20.8995871966833,
3.16634593866105));
#101417=CARTESIAN_POINT('Ctrl Pts',(-8.87222015067925,20.8999980980351,
3.16056589749218));
#101418=CARTESIAN_POINT('Ctrl Pts',(-8.87303008972077,20.9001882225889,
3.15788639308306));
#101419=CARTESIAN_POINT('Ctrl Pts',(-8.87489957134157,20.9006206850331,
3.15178031192174));
#101420=CARTESIAN_POINT('Ctrl Pts',(-8.87596521854471,20.9008626675028,
3.14835566737631));
#101421=CARTESIAN_POINT('Ctrl Pts',(-8.87883698777103,20.9015030515399,
3.13927318576526));
#101422=CARTESIAN_POINT('Ctrl Pts',(-8.880670317713,20.9018999417412,3.13362396303219));
#101423=CARTESIAN_POINT('Ctrl Pts',(-8.89541671779103,20.9050025287569,
3.08932848361827));
#101424=CARTESIAN_POINT('Ctrl Pts',(-8.91028628324103,20.9076059251985,
3.05135746611207));
#101425=CARTESIAN_POINT('Ctrl Pts',(-8.96727488464075,20.9162844605701,
2.92548874689851));
#101426=CARTESIAN_POINT('Ctrl Pts',(-9.01830618231569,20.9221514653709,
2.84207728254627));
#101427=CARTESIAN_POINT('Ctrl Pts',(-9.09805110011913,20.9303225203821,
2.74203243946404));
#101428=CARTESIAN_POINT('Ctrl Pts',(-9.1179946762363,20.9323001187201,2.71891550015676));
#101429=CARTESIAN_POINT('Ctrl Pts',(-9.14477734480224,20.9348915715385,
2.69020635858557));
#101430=CARTESIAN_POINT('Ctrl Pts',(-9.15081338828464,20.9354716447545,
2.68387891628739));
#101431=CARTESIAN_POINT('Ctrl Pts',(-9.16072482523161,20.936418146161,2.67371799768141));
#101432=CARTESIAN_POINT('Ctrl Pts',(-9.16455743023023,20.9367827231718,
2.66984310082046));
#101433=CARTESIAN_POINT('Ctrl Pts',(-9.17197673779533,20.9374858618342,
2.66244533703686));
#101434=CARTESIAN_POINT('Ctrl Pts',(-9.17555938063965,20.9378242407662,
2.65891855328911));
#101435=CARTESIAN_POINT('Ctrl Pts',(-9.18382319967626,20.9386022005231,
2.65088711138032));
#101436=CARTESIAN_POINT('Ctrl Pts',(-9.18851925316926,20.9390424404358,
2.646398066081));
#101437=CARTESIAN_POINT('Ctrl Pts',(-9.20358649965861,20.9404492939567,
2.63223170829749));
#101438=CARTESIAN_POINT('Ctrl Pts',(-9.21409515549528,20.9414221224794,
2.62270311958018));
#101439=CARTESIAN_POINT('Ctrl Pts',(-9.29675864365264,20.9490140239718,
2.55042634696519));
#101440=CARTESIAN_POINT('Ctrl Pts',(-9.376128382834,20.955996950912,2.49649835125264));
#101441=CARTESIAN_POINT('Ctrl Pts',(-9.51683441024283,20.9676140339523,
2.42409476199778));
#101442=CARTESIAN_POINT('Ctrl Pts',(-9.57475449239545,20.9721985892043,
2.3999140255961));
#101443=CARTESIAN_POINT('Ctrl Pts',(-9.64131736904383,20.9770747493859,
2.3781729762258));
#101444=CARTESIAN_POINT('Ctrl Pts',(-9.64832660261297,20.9775834490114,
2.37595599308374));
#101445=CARTESIAN_POINT('Ctrl Pts',(-9.65875777723135,20.9783329743605,
2.37276379534378));
#101446=CARTESIAN_POINT('Ctrl Pts',(-9.66216395478507,20.9785765393113,
2.37173827367811));
#101447=CARTESIAN_POINT('Ctrl Pts',(-9.66825137869082,20.9790096576048,
2.36993552961538));
#101448=CARTESIAN_POINT('Ctrl Pts',(-9.67093078760381,20.9791995436096,
2.36915239356958));
#101449=CARTESIAN_POINT('Ctrl Pts',(-9.67677934710888,20.9796123760741,
2.36746552745444));
#101450=CARTESIAN_POINT('Ctrl Pts',(-9.67994951510487,20.9798351056841,
2.36656556883547));
#101451=CARTESIAN_POINT('Ctrl Pts',(-9.68881119841782,20.9804549091218,
2.36409002684421));
#101452=CARTESIAN_POINT('Ctrl Pts',(-9.69451094658588,20.9808503433781,
2.36254390010009));
#101453=CARTESIAN_POINT('Ctrl Pts',(-9.72669115817815,20.9830660952592,
2.35407396458365));
#101454=CARTESIAN_POINT('Ctrl Pts',(-9.75339736526943,20.984840961702,2.34803141727121));
#101455=CARTESIAN_POINT('Ctrl Pts',(-9.79053812481558,20.9872520692737,
2.34097905577803));
#101456=CARTESIAN_POINT('Ctrl Pts',(-9.8008096501287,20.9879128975803,2.33916967646004));
#101457=CARTESIAN_POINT('Ctrl Pts',(-9.81110406371161,20.988570409963,2.33749693000245));
#101458=CARTESIAN_POINT('Origin',(-10.,12.3756328852638,3.5));
#101459=CARTESIAN_POINT('',(-9.81110406371042,21.5864520766487,2.33749693000264));
#101460=CARTESIAN_POINT('',(-9.8111040680739,21.4868028556135,2.33749692929362));
#101461=CARTESIAN_POINT('',(-9.81110406371068,12.3756328852638,2.3374969300026));
#101462=CARTESIAN_POINT('Ctrl Pts',(-9.81110406371016,21.5864520766487,
2.33749693000268));
#101463=CARTESIAN_POINT('Ctrl Pts',(-9.81060766089596,21.5864209889335,
2.33757759084289));
#101464=CARTESIAN_POINT('Ctrl Pts',(-9.81011130921745,21.5863899011916,
2.33765856972403));
#101465=CARTESIAN_POINT('Ctrl Pts',(-9.72529092088347,21.5810768181492,
2.35155264421486));
#101466=CARTESIAN_POINT('Ctrl Pts',(-9.64273262524373,21.5757844251671,
2.37449841993186));
#101467=CARTESIAN_POINT('Ctrl Pts',(-9.55279108763647,21.5694278398515,
2.41039941934661));
#101468=CARTESIAN_POINT('Ctrl Pts',(-9.54225700543766,21.5686741209824,
2.41478270717911));
#101469=CARTESIAN_POINT('Ctrl Pts',(-9.52626035112546,21.567514573904,2.42171334733196));
#101470=CARTESIAN_POINT('Ctrl Pts',(-9.52075069016363,21.567112447069,2.424150820525));
#101471=CARTESIAN_POINT('Ctrl Pts',(-9.51116959311343,21.5664082378757,
2.4284776996498));
#101472=CARTESIAN_POINT('Ctrl Pts',(-9.50708976996682,21.5661067996405,
2.43034832257606));
#101473=CARTESIAN_POINT('Ctrl Pts',(-9.49790811575377,21.5654248026092,
2.4346218490978));
#101474=CARTESIAN_POINT('Ctrl Pts',(-9.49281268076681,21.5650437904338,
2.4370381540536));
#101475=CARTESIAN_POINT('Ctrl Pts',(-9.47908744396125,21.5640105046256,
2.44366795134327));
#101476=CARTESIAN_POINT('Ctrl Pts',(-9.47049166045894,21.5633558662003,
2.4479504779268));
#101477=CARTESIAN_POINT('Ctrl Pts',(-9.42981017407345,21.560220877665,2.46884336836683));
#101478=CARTESIAN_POINT('Ctrl Pts',(-9.39845078724527,21.557693438203,2.48681763870582));
#101479=CARTESIAN_POINT('Ctrl Pts',(-9.29254781678088,21.5487588127927,
2.55416930938222));
#101480=CARTESIAN_POINT('Ctrl Pts',(-9.22283677679343,21.5421268174682,
2.6105630143172));
#101481=CARTESIAN_POINT('Ctrl Pts',(-9.13077231293729,21.5325595642172,
2.7041996059016));
#101482=CARTESIAN_POINT('Ctrl Pts',(-9.1029756882655,21.5295418364413,2.73566810806177));
#101483=CARTESIAN_POINT('Ctrl Pts',(-9.07299056895803,21.5261894181262,
2.77350945504996));
#101484=CARTESIAN_POINT('Ctrl Pts',(-9.06910572105483,21.5257530613272,
2.77849404505435));
#101485=CARTESIAN_POINT('Ctrl Pts',(-9.06322409983174,21.5250896032388,
2.78616725579008));
#101486=CARTESIAN_POINT('Ctrl Pts',(-9.06119843339019,21.5248605817397,
2.78883342803537));
#101487=CARTESIAN_POINT('Ctrl Pts',(-9.05750642348659,21.5244422556921,
2.79373609835053));
#101488=CARTESIAN_POINT('Ctrl Pts',(-9.0558366527482,21.524252721047,2.79596987664177));
#101489=CARTESIAN_POINT('Ctrl Pts',(-9.05209267020263,21.5238269598399,
2.80101576120915));
#101490=CARTESIAN_POINT('Ctrl Pts',(-9.05002303005636,21.5235910468645,
2.80383117756344));
#101491=CARTESIAN_POINT('Ctrl Pts',(-9.04472757167543,21.5229858717687,
2.81110239570888));
#101492=CARTESIAN_POINT('Ctrl Pts',(-9.04152034091558,21.5226178329765,
2.81557172213832));
#101493=CARTESIAN_POINT('Ctrl Pts',(-9.021313262602,21.5202881579029,2.84415122569372));
#101494=CARTESIAN_POINT('Ctrl Pts',(-9.0051914315643,21.5183798443153,2.86887276120704));
#101495=CARTESIAN_POINT('Ctrl Pts',(-8.9395345757537,21.5102622948452,2.97833115784914));
#101496=CARTESIAN_POINT('Ctrl Pts',(-8.89976923487954,21.5043752016211,
3.0684678189506));
#101497=CARTESIAN_POINT('Ctrl Pts',(-8.86008415261758,21.4956207998367,
3.20114524339427));
#101498=CARTESIAN_POINT('Ctrl Pts',(-8.85051866639125,21.4930281097516,
3.24035711906565));
#101499=CARTESIAN_POINT('Ctrl Pts',(-8.84120256186922,21.4897424105239,
3.28934745860847));
#101500=CARTESIAN_POINT('Ctrl Pts',(-8.83953500549171,21.4891106940761,
3.29873653211263));
#101501=CARTESIAN_POINT('Ctrl Pts',(-8.8370654379355,21.4881006724145,3.31369406097109));
#101502=CARTESIAN_POINT('Ctrl Pts',(-8.83618897134081,21.4877247109436,
3.31924993424982));
#101503=CARTESIAN_POINT('Ctrl Pts',(-8.83461021506429,21.4870128896893,
3.32974547392619));
#101504=CARTESIAN_POINT('Ctrl Pts',(-8.8338994501011,21.4866773040379,3.33468375552347));
#101505=CARTESIAN_POINT('Ctrl Pts',(-8.83236433442107,21.4859167618943,
3.34585231103746));
#101506=CARTESIAN_POINT('Ctrl Pts',(-8.83155843726905,21.4854912378293,
3.35208492514912));
#101507=CARTESIAN_POINT('Ctrl Pts',(-8.82961230260852,21.484391740244,3.36814557904493));
#101508=CARTESIAN_POINT('Ctrl Pts',(-8.82854597816542,21.4837154883602,
3.37798190768718));
#101509=CARTESIAN_POINT('Ctrl Pts',(-8.82043654673883,21.4778622293617,
3.46274154140933));
#101510=CARTESIAN_POINT('Ctrl Pts',(-8.82046679861231,21.4724628834874,
3.53815303662331));
#101511=CARTESIAN_POINT('Ctrl Pts',(-8.83290441303645,21.4629824137846,
3.66714860287829));
#101512=CARTESIAN_POINT('Ctrl Pts',(-8.84186292123912,21.4589667569451,
3.72083792206369));
#101513=CARTESIAN_POINT('Ctrl Pts',(-8.86279869579375,21.4524326404411,
3.80845393113823));
#101514=CARTESIAN_POINT('Ctrl Pts',(-8.87267588599687,21.4498774591765,
3.84279954364262));
#101515=CARTESIAN_POINT('Ctrl Pts',(-8.88605380159144,21.4469746775545,
3.88243463509204));
#101516=CARTESIAN_POINT('Ctrl Pts',(-8.8880525474143,21.4465530461188,3.88820774050974));
#101517=CARTESIAN_POINT('Ctrl Pts',(-8.89120131201368,21.445907267494,3.89707864075277));
#101518=CARTESIAN_POINT('Ctrl Pts',(-8.89231955928833,21.4456813510246,
3.9001874802726));
#101519=CARTESIAN_POINT('Ctrl Pts',(-8.89440689617213,21.4452659496934,
3.90591470257956));
#101520=CARTESIAN_POINT('Ctrl Pts',(-8.89537221088707,21.4450762572026,
3.90853433738499));
#101521=CARTESIAN_POINT('Ctrl Pts',(-8.89758580801163,21.4446466792264,
3.91447630458804));
#101522=CARTESIAN_POINT('Ctrl Pts',(-8.89883979767756,21.4444071333578,
3.91779644255815));
#101523=CARTESIAN_POINT('Ctrl Pts',(-8.9021404518251,21.4437862783744,3.92641735530025));
#101524=CARTESIAN_POINT('Ctrl Pts',(-8.90421053184145,21.4434063010936,
3.93170915333724));
#101525=CARTESIAN_POINT('Ctrl Pts',(-8.91863544540237,21.4408203143358,
3.96781159030337));
#101526=CARTESIAN_POINT('Ctrl Pts',(-8.93225107484958,21.4386819589838,
3.99810608855455));
#101527=CARTESIAN_POINT('Ctrl Pts',(-8.9817222821857,21.4316931874244,4.09679491866861));
#101528=CARTESIAN_POINT('Ctrl Pts',(-9.02301624192878,21.427010037129,4.16223686438359));
#101529=CARTESIAN_POINT('Ctrl Pts',(-9.10165924243954,21.4190121596264,
4.26332656869609));
#101530=CARTESIAN_POINT('Ctrl Pts',(-9.13546501107661,21.4157866785003,
4.30141244229991));
#101531=CARTESIAN_POINT('Ctrl Pts',(-9.18106887098913,21.4115900099408,
4.3465361201954));
#101532=CARTESIAN_POINT('Ctrl Pts',(-9.19067065934757,21.4107144363865,
4.35572051037113));
#101533=CARTESIAN_POINT('Ctrl Pts',(-9.20512417298615,21.4094068662907,
4.36908482657173));
#101534=CARTESIAN_POINT('Ctrl Pts',(-9.20985813780862,21.4089802072176,
4.37339100695769));
#101535=CARTESIAN_POINT('Ctrl Pts',(-9.21835397157798,21.4082172066396,
4.38099350928657));
#101536=CARTESIAN_POINT('Ctrl Pts',(-9.22210221612152,21.4078815023235,
4.38430487597133));
#101537=CARTESIAN_POINT('Ctrl Pts',(-9.23005910452318,21.4071707219209,
4.39124461112308));
#101538=CARTESIAN_POINT('Ctrl Pts',(-9.2342725519246,21.4067954223185,4.39486725963459));
#101539=CARTESIAN_POINT('Ctrl Pts',(-9.24554928228974,21.4057937413676,
4.40442483890571));
#101540=CARTESIAN_POINT('Ctrl Pts',(-9.2526568288875,21.4051652361289,4.41030673472405));
#101541=CARTESIAN_POINT('Ctrl Pts',(-9.28788994388713,21.402062738911,4.43877336380849));
#101542=CARTESIAN_POINT('Ctrl Pts',(-9.31697099058934,21.3995414810387,
4.46013907845837));
#101543=CARTESIAN_POINT('Ctrl Pts',(-9.40679276896362,21.3918633201409,
4.51998293881145));
#101544=CARTESIAN_POINT('Ctrl Pts',(-9.47011789267306,21.3865802960843,
4.55426885899629));
#101545=CARTESIAN_POINT('Ctrl Pts',(-9.53861643345747,21.3811126577436,
4.58361773137528));
#101546=CARTESIAN_POINT('Ctrl Pts',(-9.54107281093733,21.3809169202154,
4.58466032397677));
#101547=CARTESIAN_POINT('Ctrl Pts',(-9.59590647481775,21.3765551259045,
4.60771448176959));
#101548=CARTESIAN_POINT('Ctrl Pts',(-9.6498116723613,21.3724186632665,4.62591858503384));
#101549=CARTESIAN_POINT('Ctrl Pts',(-9.71128686315043,21.3680038433719,
4.64183375466668));
#101550=CARTESIAN_POINT('Ctrl Pts',(-9.71776170521399,21.3675425608669,
4.64345141953894));
#101551=CARTESIAN_POINT('Ctrl Pts',(-9.72761945962613,21.3668462466509,
4.64582542932428));
#101552=CARTESIAN_POINT('Ctrl Pts',(-9.73099240499729,21.3666090529338,
4.64662198996523));
#101553=CARTESIAN_POINT('Ctrl Pts',(-9.73708496443484,21.3661825770929,
4.64803245560088));
#101554=CARTESIAN_POINT('Ctrl Pts',(-9.7398032683243,21.3659930069641,4.64865159919433));
#101555=CARTESIAN_POINT('Ctrl Pts',(-9.74581574850585,21.3655752714533,
4.64999861277007));
#101556=CARTESIAN_POINT('Ctrl Pts',(-9.74911086286419,21.3653473613673,
4.65072198408916));
#101557=CARTESIAN_POINT('Ctrl Pts',(-9.75870468653502,21.3646866608307,
4.65278493280844));
#101558=CARTESIAN_POINT('Ctrl Pts',(-9.76501145436277,21.3642559179237,
4.65408704943447));
#101559=CARTESIAN_POINT('Ctrl Pts',(-9.81703417466507,21.3607299443617,
4.66438369511787));
#101560=CARTESIAN_POINT('Ctrl Pts',(-9.86324229880007,21.3577693813007,
4.67071103809498));
#101561=CARTESIAN_POINT('Ctrl Pts',(-9.98333399929278,21.3502382887052,
4.67994489720296));
#101562=CARTESIAN_POINT('Ctrl Pts',(-10.0573273847919,21.3457466972263,
4.67866939681464));
#101563=CARTESIAN_POINT('Ctrl Pts',(-10.1760339882518,21.3382354977675,
4.66541259719002));
#101564=CARTESIAN_POINT('Ctrl Pts',(-10.2210159069323,21.3353190849814,
4.65772436870066));
#101565=CARTESIAN_POINT('Ctrl Pts',(-10.2753100425379,21.3316528537621,
4.64516469027391));
#101566=CARTESIAN_POINT('Ctrl Pts',(-10.2851544486379,21.3309822295945,
4.64275313048984));
#101567=CARTESIAN_POINT('Ctrl Pts',(-10.3005960155963,21.3299204749674,
4.63875849640265));
#101568=CARTESIAN_POINT('Ctrl Pts',(-10.3062148225051,21.3295320647968,
4.63726046187481));
#101569=CARTESIAN_POINT('Ctrl Pts',(-10.3165702959627,21.3288122995571,
4.63441727502301));
#101570=CARTESIAN_POINT('Ctrl Pts',(-10.3213100860692,21.328481330143,4.63308390398976));
#101571=CARTESIAN_POINT('Ctrl Pts',(-10.3318115787902,21.3277445709373,
4.63005849322923));
#101572=CARTESIAN_POINT('Ctrl Pts',(-10.3375689498991,21.3273383230373,
4.62835203889783));
#101573=CARTESIAN_POINT('Ctrl Pts',(-10.3541355561356,21.326162502829,4.62330364396763));
#101574=CARTESIAN_POINT('Ctrl Pts',(-10.3649097564031,21.3253893328993,
4.61984995548207));
#101575=CARTESIAN_POINT('Ctrl Pts',(-10.4607946775943,21.3184303199654,
4.58758322931835));
#101576=CARTESIAN_POINT('Ctrl Pts',(-10.5423805778352,21.3119203202055,
4.54927878819919));
#101577=CARTESIAN_POINT('Ctrl Pts',(-10.677781617431,21.3002375554488,4.46566658218919));
#101578=CARTESIAN_POINT('Ctrl Pts',(-10.7334347878888,21.295131361341,4.42410772875779));
#101579=CARTESIAN_POINT('Ctrl Pts',(-10.7922887529663,21.2896000151356,
4.37147361930295));
#101580=CARTESIAN_POINT('Ctrl Pts',(-10.7993858571999,21.2889307652949,
4.36496820950128));
#101581=CARTESIAN_POINT('Ctrl Pts',(-10.8090878294552,21.2880137168224,
4.35585367917322));
#101582=CARTESIAN_POINT('Ctrl Pts',(-10.8117611785812,21.287760795513,4.35331847852627));
#101583=CARTESIAN_POINT('Ctrl Pts',(-10.8163302160157,21.2873281954461,
4.34894464741933));
#101584=CARTESIAN_POINT('Ctrl Pts',(-10.8182316770991,21.2871480642184,
4.34711212888631));
#101585=CARTESIAN_POINT('Ctrl Pts',(-10.8221954761754,21.2867723837437,
4.34326624977039));
#101586=CARTESIAN_POINT('Ctrl Pts',(-10.8242566087649,21.2865769359695,
4.34125169373057));
#101587=CARTESIAN_POINT('Ctrl Pts',(-10.8292799916466,21.2861002901267,
4.33630564158192));
#101588=CARTESIAN_POINT('Ctrl Pts',(-10.832234155061,21.2858197237098,4.33336591192429));
#101589=CARTESIAN_POINT('Ctrl Pts',(-10.8428636179949,21.2848089815148,
4.3226754916312));
#101590=CARTESIAN_POINT('Ctrl Pts',(-10.8504470414974,21.2840855453392,
4.31483366018202));
#101591=CARTESIAN_POINT('Ctrl Pts',(-10.8691610897656,21.2822908142297,
4.29493599764574));
#101592=CARTESIAN_POINT('Ctrl Pts',(-10.8801510704906,21.2812281599641,
4.28275052868337));
#101593=CARTESIAN_POINT('Ctrl Pts',(-10.9277274622911,21.2765674968214,
4.22772925870101));
#101594=CARTESIAN_POINT('Ctrl Pts',(-10.9614701114316,21.2730950872831,
4.18252790778383));
#101595=CARTESIAN_POINT('Ctrl Pts',(-11.034464058166,21.2647272749209,4.06852837226142));
#101596=CARTESIAN_POINT('Ctrl Pts',(-11.0702664090662,21.2598325230113,
3.99786359865141));
#101597=CARTESIAN_POINT('Ctrl Pts',(-11.1041550809007,21.2536957138836,
3.91007825678255));
#101598=CARTESIAN_POINT('Ctrl Pts',(-11.1093166522239,21.2527037635114,
3.89590295610612));
#101599=CARTESIAN_POINT('Ctrl Pts',(-11.1163619332114,21.251261094752,3.87533375995834));
#101600=CARTESIAN_POINT('Ctrl Pts',(-11.1184660082218,21.2508175818711,
3.8690165073243));
#101601=CARTESIAN_POINT('Ctrl Pts',(-11.1220728033281,21.2500343215023,
3.85787320683798));
#101602=CARTESIAN_POINT('Ctrl Pts',(-11.1235982473083,21.2496953234722,
3.85305464934382));
#101603=CARTESIAN_POINT('Ctrl Pts',(-11.1266845267381,21.2489931051004,
3.84308312128736));
#101604=CARTESIAN_POINT('Ctrl Pts',(-11.1282411338635,21.2486297566912,
3.83792897640752));
#101605=CARTESIAN_POINT('Ctrl Pts',(-11.1321458661258,21.2476941232236,
3.82467209187733));
#101606=CARTESIAN_POINT('Ctrl Pts',(-11.1344423379403,21.2471201880642,
3.81655458434204));
#101607=CARTESIAN_POINT('Ctrl Pts',(-11.1438374067516,21.2446672292287,
3.78192923535056));
#101608=CARTESIAN_POINT('Ctrl Pts',(-11.1500950833864,21.2427616881632,
3.75520421058968));
#101609=CARTESIAN_POINT('Ctrl Pts',(-11.1747225928471,21.2338109893741,
3.63055861103171));
#101610=CARTESIAN_POINT('Ctrl Pts',(-11.1815519657687,21.2264207830843,
3.53078472805198));
#101611=CARTESIAN_POINT('Ctrl Pts',(-11.1744612972435,21.2175518910583,
3.40931590665271));
#101612=CARTESIAN_POINT('Ctrl Pts',(-11.1725539858955,21.2159522736708,
3.38730489248347));
#101613=CARTESIAN_POINT('Ctrl Pts',(-11.1675250740633,21.2128055979059,
3.34360352561482));
#101614=CARTESIAN_POINT('Ctrl Pts',(-11.1644149784763,21.2112587818767,
3.32191978207275));
#101615=CARTESIAN_POINT('Ctrl Pts',(-11.1597657451936,21.2093589140312,
3.29489281092851));
#101616=CARTESIAN_POINT('Ctrl Pts',(-11.1587915082088,21.2089783336941,
3.2894583503408));
#101617=CARTESIAN_POINT('Ctrl Pts',(-11.1571907403435,21.2083798492295,
3.28087686924934));
#101618=CARTESIAN_POINT('Ctrl Pts',(-11.1565895182251,21.2081605856563,
3.27772529850798));
#101619=CARTESIAN_POINT('Ctrl Pts',(-11.1554924375407,21.2077701775835,
3.27209945878811));
#101620=CARTESIAN_POINT('Ctrl Pts',(-11.1550015086394,21.2075987654235,
3.26962433913444));
#101621=CARTESIAN_POINT('Ctrl Pts',(-11.1538042781537,21.2071884894799,
3.2636882853228));
#101622=CARTESIAN_POINT('Ctrl Pts',(-11.1530903581196,21.206950058039,3.26022893083061));
#101623=CARTESIAN_POINT('Ctrl Pts',(-11.1508697206862,21.2062267978725,
3.24970800420805));
#101624=CARTESIAN_POINT('Ctrl Pts',(-11.1493135846269,21.2057446521037,
3.2426568675873));
#101625=CARTESIAN_POINT('Ctrl Pts',(-11.1347205305769,21.2014325364851,
3.17930730219187));
#101626=CARTESIAN_POINT('Ctrl Pts',(-11.1176194348603,21.1978070249937,
3.1240170554102));
#101627=CARTESIAN_POINT('Ctrl Pts',(-11.0593837445126,21.1879019542428,
2.97544375652879));
#101628=CARTESIAN_POINT('Ctrl Pts',(-11.0101226965424,21.1817063151812,
2.88591264915616));
#101629=CARTESIAN_POINT('Ctrl Pts',(-10.9420019277671,21.1741702234808,
2.79295749048992));
#101630=CARTESIAN_POINT('Ctrl Pts',(-10.9338487750669,21.1732821932321,
2.78222344484587));
#101631=CARTESIAN_POINT('Ctrl Pts',(-10.9215330394064,21.1719595781677,
2.76657424038097));
#101632=CARTESIAN_POINT('Ctrl Pts',(-10.9175112892476,21.1715305141533,
2.76154924407858));
#101633=CARTESIAN_POINT('Ctrl Pts',(-10.9102887396569,21.1707648246262,
2.75267508316271));
#101634=CARTESIAN_POINT('Ctrl Pts',(-10.9071041811297,21.1704288531802,
2.74881285679101));
#101635=CARTESIAN_POINT('Ctrl Pts',(-10.9003456555051,21.169719174951,2.74072177781364));
#101636=CARTESIAN_POINT('Ctrl Pts',(-10.896766304651,21.1693452551555,2.73649760242505));
#101637=CARTESIAN_POINT('Ctrl Pts',(-10.8872030542396,21.1683511880839,
2.72537154404571));
#101638=CARTESIAN_POINT('Ctrl Pts',(-10.881168514265,21.1677289750639,2.71851388655775));
#101639=CARTESIAN_POINT('Ctrl Pts',(-10.8516763584051,21.1647114692983,
2.68577489064124));
#101640=CARTESIAN_POINT('Ctrl Pts',(-10.827157148463,21.1622719974959,2.66087798256142));
#101641=CARTESIAN_POINT('Ctrl Pts',(-10.7519895419738,21.1549822660332,
2.59105209623496));
#101642=CARTESIAN_POINT('Ctrl Pts',(-10.6985365808187,21.1500217906373,
2.54935847792475));
#101643=CARTESIAN_POINT('Ctrl Pts',(-10.5913465241177,21.1406355005657,
2.47969309061722));
#101644=CARTESIAN_POINT('Ctrl Pts',(-10.5384409198096,21.1362273893005,
2.45080994710929));
#101645=CARTESIAN_POINT('Ctrl Pts',(-10.4746300737837,21.1313231392644,
2.42207739369234));
#101646=CARTESIAN_POINT('Ctrl Pts',(-10.4656557121155,21.1306425690593,
2.41817024188138));
#101647=CARTESIAN_POINT('Ctrl Pts',(-10.4532181071734,21.1297129359121,
2.41293876110759));
#101648=CARTESIAN_POINT('Ctrl Pts',(-10.4497960688404,21.1294585633578,
2.41151835699353));
#101649=CARTESIAN_POINT('Ctrl Pts',(-10.443918502564,21.1290241330062,2.40911117515022));
#101650=CARTESIAN_POINT('Ctrl Pts',(-10.4414662740918,21.1288436144095,
2.40811649234232));
#101651=CARTESIAN_POINT('Ctrl Pts',(-10.4363407705603,21.1284678655562,
2.40605755491009));
#101652=CARTESIAN_POINT('Ctrl Pts',(-10.4336669221798,21.1282727330546,
2.40499482098623));
#101653=CARTESIAN_POINT('Ctrl Pts',(-10.4271339065682,21.1277980653066,
2.40242592520942));
#101654=CARTESIAN_POINT('Ctrl Pts',(-10.4232705862356,21.1275191493763,
2.40093028614284));
#101655=CARTESIAN_POINT('Ctrl Pts',(-10.4093610559541,21.1265210449645,
2.39562959549805));
#101656=CARTESIAN_POINT('Ctrl Pts',(-10.3992704201818,21.1258083769603,
2.3919415104663));
#101657=CARTESIAN_POINT('Ctrl Pts',(-10.3739600414459,21.1240457563599,
2.38308134222335));
#101658=CARTESIAN_POINT('Ctrl Pts',(-10.3586818657378,21.1230040533606,
2.37808165466593));
#101659=CARTESIAN_POINT('Ctrl Pts',(-10.2914146014787,21.118494913406,2.35758357973594));
#101660=CARTESIAN_POINT('Ctrl Pts',(-10.2384891239259,21.1151449211672,
2.34537381825059));
#101661=CARTESIAN_POINT('Ctrl Pts',(-10.1041615685227,21.106736958698,2.32401955978369));
#101662=CARTESIAN_POINT('Ctrl Pts',(-10.0223096222156,21.1016836574985,
2.3196272665717));
#101663=CARTESIAN_POINT('Ctrl Pts',(-9.92566052898394,21.0953719452171,
2.32450245495432));
#101664=CARTESIAN_POINT('Ctrl Pts',(-9.91067031644554,21.0943838234684,
2.3255465059992));
#101665=CARTESIAN_POINT('Ctrl Pts',(-9.88908277236535,21.0929457271959,
2.32746572423783));
#101666=CARTESIAN_POINT('Ctrl Pts',(-9.88246604931636,21.0925028936094,
2.32811048873557));
#101667=CARTESIAN_POINT('Ctrl Pts',(-9.8708308498433,21.0917204260234,2.32934380734268));
#101668=CARTESIAN_POINT('Ctrl Pts',(-9.86580999521794,21.0913815367225,
2.32990870782936));
#101669=CARTESIAN_POINT('Ctrl Pts',(-9.85544259007978,21.0906791459331,
2.33114275884775));
#101670=CARTESIAN_POINT('Ctrl Pts',(-9.85009669501997,21.0903155139542,
2.33181632760801));
#101671=CARTESIAN_POINT('Ctrl Pts',(-9.83637456789667,21.089378306202,2.33364102195471));
#101672=CARTESIAN_POINT('Ctrl Pts',(-9.82800588999497,21.0888030695785,
2.33484568947816));
#101673=CARTESIAN_POINT('Ctrl Pts',(-9.81680032626574,21.088027758761,2.33658207678296));
#101674=CARTESIAN_POINT('Ctrl Pts',(-9.81395129694457,21.0878301939243,
2.33703428108315));
#101675=CARTESIAN_POINT('Ctrl Pts',(-9.81110406314734,21.0876323086995,
2.33749693009414));
#101676=CARTESIAN_POINT('Ctrl Pts',(-9.81110406371161,20.988570409963,2.33749693000245));
#101677=CARTESIAN_POINT('Ctrl Pts',(-9.81154564090745,20.9885986138497,
2.33742517781529));
#101678=CARTESIAN_POINT('Ctrl Pts',(-9.81198726021747,20.9886268116318,
2.33735367703001));
#101679=CARTESIAN_POINT('Ctrl Pts',(-9.89061252215599,20.9936455543156,
2.32466974970649));
#101680=CARTESIAN_POINT('Ctrl Pts',(-9.96987033142047,20.9984459045583,
2.31997459421931));
#101681=CARTESIAN_POINT('Ctrl Pts',(-10.0714622469342,21.0048223705121,
2.32420514394297));
#101682=CARTESIAN_POINT('Ctrl Pts',(-10.0938901091305,21.0062429994486,
2.32578325338818));
#101683=CARTESIAN_POINT('Ctrl Pts',(-10.1454347139656,21.0095536917515,
2.33089630592362));
#101684=CARTESIAN_POINT('Ctrl Pts',(-10.1744907577607,21.0114539862627,
2.33487878170737));
#101685=CARTESIAN_POINT('Ctrl Pts',(-10.2121854611868,21.0139787103814,
2.34148691748549));
#101686=CARTESIAN_POINT('Ctrl Pts',(-10.2209866004524,21.0145724376907,
2.34313347901222));
#101687=CARTESIAN_POINT('Ctrl Pts',(-10.2351582057523,21.0155357024768,
2.34595239022433));
#101688=CARTESIAN_POINT('Ctrl Pts',(-10.2405408480495,21.0159032629769,
2.3470622887425));
#101689=CARTESIAN_POINT('Ctrl Pts',(-10.2508187068302,21.0166084346186,
2.34925668513458));
#101690=CARTESIAN_POINT('Ctrl Pts',(-10.2557151638454,21.0169458378856,
2.35033485133998));
#101691=CARTESIAN_POINT('Ctrl Pts',(-10.2669532748006,21.0177236479194,
2.35288475151277));
#101692=CARTESIAN_POINT('Ctrl Pts',(-10.2732898602838,21.0181647261048,
2.35437785742977));
#101693=CARTESIAN_POINT('Ctrl Pts',(-10.2930945040031,21.0195513562585,
2.35921813503534));
#101694=CARTESIAN_POINT('Ctrl Pts',(-10.3065155617127,21.0205027794733,
2.36275076017877));
#101695=CARTESIAN_POINT('Ctrl Pts',(-10.3732860600221,21.025297086593,2.38159353656787));
#101696=CARTESIAN_POINT('Ctrl Pts',(-10.4255613565746,21.0292513415884,
2.40042215953935));
#101697=CARTESIAN_POINT('Ctrl Pts',(-10.5327527806387,21.037763712179,2.44782202949778));
#101698=CARTESIAN_POINT('Ctrl Pts',(-10.587147324562,21.0423279138933,2.4771795833104));
#101699=CARTESIAN_POINT('Ctrl Pts',(-10.6574821338285,21.0484322724202,
2.52260702654373));
#101700=CARTESIAN_POINT('Ctrl Pts',(-10.6756386939345,21.0500272416079,
2.53506879640161));
#101701=CARTESIAN_POINT('Ctrl Pts',(-10.7114594161842,21.0531989351113,
2.56116147982816));
#101702=CARTESIAN_POINT('Ctrl Pts',(-10.7291078168543,21.0547745707211,
2.57480044467821));
#101703=CARTESIAN_POINT('Ctrl Pts',(-10.7506549218015,21.0567044539238,
2.59245215959245));
#101704=CARTESIAN_POINT('Ctrl Pts',(-10.7549254166935,21.0570872537584,
2.59600137580944));
#101705=CARTESIAN_POINT('Ctrl Pts',(-10.7616286837894,21.0576884012062,
2.6016531034189));
#101706=CARTESIAN_POINT('Ctrl Pts',(-10.7640781544275,21.0579081285107,
2.60373554509684));
#101707=CARTESIAN_POINT('Ctrl Pts',(-10.7684332777394,21.0582988592766,
2.60746892670866));
#101708=CARTESIAN_POINT('Ctrl Pts',(-10.7703421477392,21.0584701341852,
2.60911594765053));
#101709=CARTESIAN_POINT('Ctrl Pts',(-10.7749031601599,21.0588794325035,
2.61307692414931));
#101710=CARTESIAN_POINT('Ctrl Pts',(-10.7775502337982,21.0591170290067,
2.61539665112905));
#101711=CARTESIAN_POINT('Ctrl Pts',(-10.7855509635379,21.0598354626007,
2.62247164203893));
#101712=CARTESIAN_POINT('Ctrl Pts',(-10.7908718103145,21.0603136679155,
2.62726400252087));
#101713=CARTESIAN_POINT('Ctrl Pts',(-10.8401253760307,21.0647479041644,
2.67244591334805));
#101714=CARTESIAN_POINT('Ctrl Pts',(-10.8809788604181,21.0684853233663,
2.71607735761498));
#101715=CARTESIAN_POINT('Ctrl Pts',(-10.9806828145175,21.078362541328,2.8402520021803));
#101716=CARTESIAN_POINT('Ctrl Pts',(-11.0329121469552,21.0844331029509,
2.92545966933217));
#101717=CARTESIAN_POINT('Ctrl Pts',(-11.0794508365027,21.0918383931154,
3.02875686773288));
#101718=CARTESIAN_POINT('Ctrl Pts',(-11.0848797272695,21.0927441592198,
3.04139325160445));
#101719=CARTESIAN_POINT('Ctrl Pts',(-11.0925153469007,21.094083459204,3.0600608466953));
#101720=CARTESIAN_POINT('Ctrl Pts',(-11.0948961450542,21.0945111708585,
3.06601996517926));
#101721=CARTESIAN_POINT('Ctrl Pts',(-11.0990508773686,21.0952761030237,
3.07667106149437));
#101722=CARTESIAN_POINT('Ctrl Pts',(-11.1008437731231,21.095612683287,3.08135551232209));
#101723=CARTESIAN_POINT('Ctrl Pts',(-11.1045356614451,21.0963196453872,
3.09118933909534));
#101724=CARTESIAN_POINT('Ctrl Pts',(-11.1064286877198,21.0966902152309,
3.09634081070988));
#101725=CARTESIAN_POINT('Ctrl Pts',(-11.1113034018002,21.0976661609161,
3.10989826783242));
#101726=CARTESIAN_POINT('Ctrl Pts',(-11.1142256797146,21.0982734709802,
3.11832508684376));
#101727=CARTESIAN_POINT('Ctrl Pts',(-11.1273248236092,21.1011028537429,
3.15753140946153));
#101728=CARTESIAN_POINT('Ctrl Pts',(-11.136322926937,21.1033626812468,3.18868690122713));
#101729=CARTESIAN_POINT('Ctrl Pts',(-11.1587195841948,21.110042016487,3.28025119861834));
#101730=CARTESIAN_POINT('Ctrl Pts',(-11.1686579903668,21.1145542407696,
3.34138883224352));
#101731=CARTESIAN_POINT('Ctrl Pts',(-11.1794438209105,21.1241702078613,
3.47192558831706));
#101732=CARTESIAN_POINT('Ctrl Pts',(-11.1790587667774,21.1292631194004,
3.54120840115635));
#101733=CARTESIAN_POINT('Ctrl Pts',(-11.1716958218964,21.1347827839524,
3.61965260157989));
#101734=CARTESIAN_POINT('Ctrl Pts',(-11.1706780137146,21.1354524242924,
3.62923175796202));
#101735=CARTESIAN_POINT('Ctrl Pts',(-11.1691085773061,21.1363698526213,
3.6424562035722));
#101736=CARTESIAN_POINT('Ctrl Pts',(-11.1686572292205,21.1366227701528,
3.64611268588511));
#101737=CARTESIAN_POINT('Ctrl Pts',(-11.16785299283,21.1370553265834,3.65238576045523));
#101738=CARTESIAN_POINT('Ctrl Pts',(-11.1675084537776,21.1372354181284,
3.65500336629065));
#101739=CARTESIAN_POINT('Ctrl Pts',(-11.1667695710616,21.1376109702939,
3.6604747005108));
#101740=CARTESIAN_POINT('Ctrl Pts',(-11.1663735553362,21.1378063297447,
3.6633281700207));
#101741=CARTESIAN_POINT('Ctrl Pts',(-11.1653794727514,21.1382826797727,
3.67030293401405));
#101742=CARTESIAN_POINT('Ctrl Pts',(-11.1647700016236,21.1385630399553,
3.67442261745356));
#101743=CARTESIAN_POINT('Ctrl Pts',(-11.162487402374,21.1395725799719,3.68930598295207));
#101744=CARTESIAN_POINT('Ctrl Pts',(-11.1606867584251,21.1402950397002,
3.70004995796409));
#101745=CARTESIAN_POINT('Ctrl Pts',(-11.1558063064342,21.1420869486675,
3.72688118864197));
#101746=CARTESIAN_POINT('Ctrl Pts',(-11.1525394399606,21.1431477903619,
3.74293247528852));
#101747=CARTESIAN_POINT('Ctrl Pts',(-11.1365940327204,21.1477956352903,
3.81369146068927));
#101748=CARTESIAN_POINT('Ctrl Pts',(-11.1203464074761,21.1512577245616,
3.86752313020131));
#101749=CARTESIAN_POINT('Ctrl Pts',(-11.0720527831591,21.1596291581774,
3.9940449992541));
#101750=CARTESIAN_POINT('Ctrl Pts',(-11.0363880347072,21.1645376023556,
4.06504461538111));
#101751=CARTESIAN_POINT('Ctrl Pts',(-10.9857756510308,21.170689469143,4.14464628008067));
#101752=CARTESIAN_POINT('Ctrl Pts',(-10.9774413006887,21.1716810807169,
4.15721452397165));
#101753=CARTESIAN_POINT('Ctrl Pts',(-10.9650838299278,21.1731232556094,
4.1750944883846));
#101754=CARTESIAN_POINT('Ctrl Pts',(-10.9612531316651,21.1735666184544,
4.18053786143023));
#101755=CARTESIAN_POINT('Ctrl Pts',(-10.9544338540055,21.1743496119374,
4.19005551146871));
#101756=CARTESIAN_POINT('Ctrl Pts',(-10.9514647856071,21.1746884936265,
4.19414360975794));
#101757=CARTESIAN_POINT('Ctrl Pts',(-10.9452787790403,21.1753904681497,
4.20254683867452));
#101758=CARTESIAN_POINT('Ctrl Pts',(-10.9420583871401,21.1757536889523,
4.20685926759882));
#101759=CARTESIAN_POINT('Ctrl Pts',(-10.9337165852982,21.17668898526,4.21787151784638));
#101760=CARTESIAN_POINT('Ctrl Pts',(-10.9285526431293,21.1772627096449,
4.22453858440401));
#101761=CARTESIAN_POINT('Ctrl Pts',(-10.9062892814536,21.1797146238594,
4.2526534307638));
#101762=CARTESIAN_POINT('Ctrl Pts',(-10.8885162073047,21.1816193076829,
4.27355425230225));
#101763=CARTESIAN_POINT('Ctrl Pts',(-10.8029055706081,21.1905671575275,
4.36738465427131));
#101764=CARTESIAN_POINT('Ctrl Pts',(-10.7267254541968,21.1979552228097,
4.43213606072194));
#101765=CARTESIAN_POINT('Ctrl Pts',(-10.6248350759737,21.2068218217987,
4.49858084636574));
#101766=CARTESIAN_POINT('Ctrl Pts',(-10.6060039454294,21.2084209034416,
4.51011974061249));
#101767=CARTESIAN_POINT('Ctrl Pts',(-10.5678311798878,21.2115704985386,
4.53205835324206));
#101768=CARTESIAN_POINT('Ctrl Pts',(-10.5485001835475,21.2131206708753,
4.54246073941665));
#101769=CARTESIAN_POINT('Ctrl Pts',(-10.5239529926709,21.2150239642162,
4.55479800627797));
#101770=CARTESIAN_POINT('Ctrl Pts',(-10.5190001609658,21.2154047336667,
4.55724377912728));
#101771=CARTESIAN_POINT('Ctrl Pts',(-10.5111435854824,21.2160034035956,
4.56105494236738));
#101772=CARTESIAN_POINT('Ctrl Pts',(-10.5082512326133,21.2162226654962,
4.56244342949355));
#101773=CARTESIAN_POINT('Ctrl Pts',(-10.5030748862707,21.2166130005149,
4.5649023820717));
#101774=CARTESIAN_POINT('Ctrl Pts',(-10.5007931395268,21.2167843416638,
4.56597732439389));
#101775=CARTESIAN_POINT('Ctrl Pts',(-10.4953103495957,21.2171943525046,
4.56853880411862));
#101776=CARTESIAN_POINT('Ctrl Pts',(-10.4921060596624,21.217432590908,4.57001829198612));
#101777=CARTESIAN_POINT('Ctrl Pts',(-10.4823362115003,21.2181549234049,
4.57447606626499));
#101778=CARTESIAN_POINT('Ctrl Pts',(-10.4757497641976,21.218636343718,4.57740856048036));
#101779=CARTESIAN_POINT('Ctrl Pts',(-10.406689354833,21.223630695253,4.60739962892105));
#101780=CARTESIAN_POINT('Ctrl Pts',(-10.3419981526692,21.2278586349213,
4.62905724252357));
#101781=CARTESIAN_POINT('Ctrl Pts',(-10.1886170451612,21.2376195215725,
4.66600108341388));
#101782=CARTESIAN_POINT('Ctrl Pts',(-10.0993433749463,21.2431279394555,
4.67697221023942));
#101783=CARTESIAN_POINT('Ctrl Pts',(-9.9950210428757,21.2499363005898,4.67783087533478));
#101784=CARTESIAN_POINT('Ctrl Pts',(-9.98034807543187,21.2509016250325,
4.67767743103788));
#101785=CARTESIAN_POINT('Ctrl Pts',(-9.95910072027127,21.2523123764753,
4.67705805534586));
#101786=CARTESIAN_POINT('Ctrl Pts',(-9.95252096252726,21.2527510403674,
4.67681101064465));
#101787=CARTESIAN_POINT('Ctrl Pts',(-9.94090819259789,21.2535285650007,
4.67627744643598));
#101788=CARTESIAN_POINT('Ctrl Pts',(-9.93587425784356,21.2538667096216,
4.67601375865072));
#101789=CARTESIAN_POINT('Ctrl Pts',(-9.92544019535183,21.2545699523815,
4.67540000895739));
#101790=CARTESIAN_POINT('Ctrl Pts',(-9.92004048721214,21.2549351955567,
4.67504502898794));
#101791=CARTESIAN_POINT('Ctrl Pts',(-9.90609885812247,21.2558817055601,
4.6740319562832));
#101792=CARTESIAN_POINT('Ctrl Pts',(-9.89756145409032,21.256464698335,4.67331785820197));
#101793=CARTESIAN_POINT('Ctrl Pts',(-9.86044273670116,21.2590146620994,
4.66980491764224));
#101794=CARTESIAN_POINT('Ctrl Pts',(-9.83196356980939,21.2610108445436,
4.66605458075093));
#101795=CARTESIAN_POINT('Ctrl Pts',(-9.70638529070889,21.2699968738891,
4.64482170220833));
#101796=CARTESIAN_POINT('Ctrl Pts',(-9.61157926070604,21.2773176200586,
4.61622131678748));
#101797=CARTESIAN_POINT('Ctrl Pts',(-9.48342597116334,21.2875371123037,
4.55923542330977));
#101798=CARTESIAN_POINT('Ctrl Pts',(-9.44630315176044,21.2905328236377,
4.54031197377109));
#101799=CARTESIAN_POINT('Ctrl Pts',(-9.4050893413494,21.2938417619775,4.51647036939357));
#101800=CARTESIAN_POINT('Ctrl Pts',(-9.39994436455622,21.2942545056208,
4.51344163212387));
#101801=CARTESIAN_POINT('Ctrl Pts',(-9.39173790569342,21.2949120471539,
4.5085262591544));
#101802=CARTESIAN_POINT('Ctrl Pts',(-9.3886617278601,21.2951583430357,4.50666454624072));
#101803=CARTESIAN_POINT('Ctrl Pts',(-9.38320510005982,21.2955948394334,
4.50332793993167));
#101804=CARTESIAN_POINT('Ctrl Pts',(-9.38082132794078,21.2957853893846,
4.5018586109474));
#101805=CARTESIAN_POINT('Ctrl Pts',(-9.37570217889202,21.2961942856514,
4.49867797770765));
#101806=CARTESIAN_POINT('Ctrl Pts',(-9.37296858404418,21.2964124505531,
4.49696392945528));
#101807=CARTESIAN_POINT('Ctrl Pts',(-9.36538026488416,21.2970176554021,
4.49216226250676));
#101808=CARTESIAN_POINT('Ctrl Pts',(-9.36054098793095,21.297403141663,4.48905022045298));
#101809=CARTESIAN_POINT('Ctrl Pts',(-9.33216500349244,21.2996619525451,
4.47050686126541));
#101810=CARTESIAN_POINT('Ctrl Pts',(-9.30916259113074,21.301486711869,4.45426994197139));
#101811=CARTESIAN_POINT('Ctrl Pts',(-9.22763760337343,21.3080175628248,
4.39222844277644));
#101812=CARTESIAN_POINT('Ctrl Pts',(-9.17289961975558,21.312536437468,4.34173737174336));
#101813=CARTESIAN_POINT('Ctrl Pts',(-9.08080888038258,21.3211081214306,
4.23907279221526));
#101814=CARTESIAN_POINT('Ctrl Pts',(-9.04224760145529,21.3251195339991,
4.18836735335184));
#101815=CARTESIAN_POINT('Ctrl Pts',(-9.00266521871272,21.3299443197606,
4.12651040437049));
#101816=CARTESIAN_POINT('Ctrl Pts',(-8.99746402292412,21.3305946209163,
4.11815334490128));
#101817=CARTESIAN_POINT('Ctrl Pts',(-8.98912324854826,21.3316652474119,
4.10436954359671));
#101818=CARTESIAN_POINT('Ctrl Pts',(-8.98592110023948,21.3320833027469,
4.09898108012593));
#101819=CARTESIAN_POINT('Ctrl Pts',(-8.98024924889666,21.3328367046411,
4.08926083308064));
#101820=CARTESIAN_POINT('Ctrl Pts',(-8.97776373635961,21.3331714736486,
4.08493841023257));
#101821=CARTESIAN_POINT('Ctrl Pts',(-8.97252951700681,21.3338864636661,
4.07570060328802));
#101822=CARTESIAN_POINT('Ctrl Pts',(-8.96978847818066,21.3342669472355,
4.07078104072404));
#101823=CARTESIAN_POINT('Ctrl Pts',(-8.96248321550514,21.3352976722442,
4.05744563989258));
#101824=CARTESIAN_POINT('Ctrl Pts',(-8.95798623633236,21.3359502596197,
4.0489936488159));
#101825=CARTESIAN_POINT('Ctrl Pts',(-8.93480562539564,21.339412618335,4.00411502754312));
#101826=CARTESIAN_POINT('Ctrl Pts',(-8.91792976471142,21.3422840251816,
3.9667915223606));
#101827=CARTESIAN_POINT('Ctrl Pts',(-8.86567853363002,21.3525466616692,
3.83308018475613));
#101828=CARTESIAN_POINT('Ctrl Pts',(-8.84098351146032,21.3602280785029,
3.7330335261323));
#101829=CARTESIAN_POINT('Ctrl Pts',(-8.82679678713881,21.3693812433472,
3.60633953495458));
#101830=CARTESIAN_POINT('Ctrl Pts',(-8.82481225723331,21.3711437800464,
3.58153439140686));
#101831=CARTESIAN_POINT('Ctrl Pts',(-8.82333834893399,21.3732669246141,
3.55094526049342));
#101832=CARTESIAN_POINT('Ctrl Pts',(-8.82310385595059,21.3736631351421,
3.54520542167043));
#101833=CARTESIAN_POINT('Ctrl Pts',(-8.82280216638695,21.3742806281274,
3.53620694740019));
#101834=CARTESIAN_POINT('Ctrl Pts',(-8.82270648660259,21.3745034134395,
3.53294945324659));
#101835=CARTESIAN_POINT('Ctrl Pts',(-8.82255385112819,21.3749159110755,
3.52689691407597));
#101836=CARTESIAN_POINT('Ctrl Pts',(-8.82249332592416,21.3751058084816,
3.52410207966527));
#101837=CARTESIAN_POINT('Ctrl Pts',(-8.82237748541622,21.3755395033274,
3.51770000197227));
#101838=CARTESIAN_POINT('Ctrl Pts',(-8.82232879223608,21.3757829331426,
3.51409270020506));
#101839=CARTESIAN_POINT('Ctrl Pts',(-8.82222891109429,21.3765372402006,
3.50287396588964));
#101840=CARTESIAN_POINT('Ctrl Pts',(-8.82223493142859,21.3770450865625,
3.49526203499083));
#101841=CARTESIAN_POINT('Ctrl Pts',(-8.8224219643369,21.3782269110615,3.4774260861938));
#101842=CARTESIAN_POINT('Ctrl Pts',(-8.822662327604,21.378898023308,3.46720316192881));
#101843=CARTESIAN_POINT('Ctrl Pts',(-8.82398925523013,21.3812632906469,
3.43089674910637));
#101844=CARTESIAN_POINT('Ctrl Pts',(-8.82580985829891,21.3829271398711,
3.40484628954157));
#101845=CARTESIAN_POINT('Ctrl Pts',(-8.8369296966279,21.3897358894272,3.2972956070754));
#101846=CARTESIAN_POINT('Ctrl Pts',(-8.85386275014144,21.3947014451756,
3.21681821422124));
#101847=CARTESIAN_POINT('Ctrl Pts',(-8.89307350196077,21.4027389105031,
3.09514477982906));
#101848=CARTESIAN_POINT('Ctrl Pts',(-8.90965692252478,21.4056685141406,
3.05240057632517));
#101849=CARTESIAN_POINT('Ctrl Pts',(-8.93290010578409,21.409349318696,3.00150648525169));
#101850=CARTESIAN_POINT('Ctrl Pts',(-8.93723320736266,21.4100205244395,
2.99233406420002));
#101851=CARTESIAN_POINT('Ctrl Pts',(-8.94423608637796,21.4110829190323,
2.97799286790172));
#101852=CARTESIAN_POINT('Ctrl Pts',(-8.94682666505395,21.4114713808675,
2.97278580086486));
#101853=CARTESIAN_POINT('Ctrl Pts',(-8.9516806384427,21.4121910735635,2.96320785734931));
#101854=CARTESIAN_POINT('Ctrl Pts',(-8.95393308207187,21.4125219176924,
2.95883155101292));
#101855=CARTESIAN_POINT('Ctrl Pts',(-8.95899186883728,21.4132581874936,
2.9491523542884));
#101856=CARTESIAN_POINT('Ctrl Pts',(-8.96181141905327,21.4136640694684,
2.94385655985796));
#101857=CARTESIAN_POINT('Ctrl Pts',(-8.97005511184859,21.4148381740305,
2.92865408769705));
#101858=CARTESIAN_POINT('Ctrl Pts',(-8.97558132892231,21.415609979382,2.91880382399427));
#101859=CARTESIAN_POINT('Ctrl Pts',(-9.0229852836873,21.4221081608214,2.83708519005339));
#101860=CARTESIAN_POINT('Ctrl Pts',(-9.07221869555927,21.4281086586544,
2.76977365273283));
#101861=CARTESIAN_POINT('Ctrl Pts',(-9.17954640257612,21.4398163832943,
2.65158794907028));
#101862=CARTESIAN_POINT('Ctrl Pts',(-9.2363744279862,21.4454750502884,2.60009718495586));
#101863=CARTESIAN_POINT('Ctrl Pts',(-9.30525363052713,21.4514809814556,
2.54894334776844));
#101864=CARTESIAN_POINT('Ctrl Pts',(-9.31277330588414,21.4521261099288,
2.54349555254843));
#101865=CARTESIAN_POINT('Ctrl Pts',(-9.32332281259553,21.4530157526779,
2.53604137278203));
#101866=CARTESIAN_POINT('Ctrl Pts',(-9.32629844172185,21.4532650067609,
2.5339593889506));
#101867=CARTESIAN_POINT('Ctrl Pts',(-9.33144261961252,21.4536929556091,
2.53039544672466));
#101868=CARTESIAN_POINT('Ctrl Pts',(-9.33360656086063,21.4538720821405,
2.52890693277009));
#101869=CARTESIAN_POINT('Ctrl Pts',(-9.338165246464,21.4542475358484,2.52579355566578));
#101870=CARTESIAN_POINT('Ctrl Pts',(-9.34056102896826,21.4544437522708,
2.5241702602653));
#101871=CARTESIAN_POINT('Ctrl Pts',(-9.34647387744535,21.4549253799471,
2.52019564828033));
#101872=CARTESIAN_POINT('Ctrl Pts',(-9.34999772057944,21.455210127747,2.51785439030807));
#101873=CARTESIAN_POINT('Ctrl Pts',(-9.36301452579025,21.4562538868665,
2.50930670683235));
#101874=CARTESIAN_POINT('Ctrl Pts',(-9.37258474779524,21.4570055662909,
2.50321826845062));
#101875=CARTESIAN_POINT('Ctrl Pts',(-9.39696813417252,21.4588854081707,
2.48819626184515));
#101876=CARTESIAN_POINT('Ctrl Pts',(-9.41189329411615,21.4600038422507,
2.47944877470532));
#101877=CARTESIAN_POINT('Ctrl Pts',(-9.48141641054314,21.4650927957274,
2.44073394308111));
#101878=CARTESIAN_POINT('Ctrl Pts',(-9.5381479879789,21.4689133235716,2.41479613307216));
#101879=CARTESIAN_POINT('Ctrl Pts',(-9.66624522916771,21.4773478406234,
2.36810473132451));
#101880=CARTESIAN_POINT('Ctrl Pts',(-9.73804036721294,21.4819622223032,
2.34936910054604));
#101881=CARTESIAN_POINT('Ctrl Pts',(-9.81110407243713,21.4868028556135,
2.33749692858463));
#101882=CARTESIAN_POINT('Origin',(-10.,12.3756328852638,3.5));
#101883=CARTESIAN_POINT('',(-9.8111040636317,22.0857064764352,2.33749693001543));
#101884=CARTESIAN_POINT('',(-9.81110406961625,21.9876672748128,2.337496929043));
#101885=CARTESIAN_POINT('',(-9.81110406371068,12.3756328852638,2.3374969300026));
#101886=CARTESIAN_POINT('Ctrl Pts',(-9.81110406355273,22.0857064764352,
2.33749693002826));
#101887=CARTESIAN_POINT('Ctrl Pts',(-9.8103247751117,22.0856498195303,2.33762355715178));
#101888=CARTESIAN_POINT('Ctrl Pts',(-9.80954560011318,22.0855931853744,
2.33775097013001));
#101889=CARTESIAN_POINT('Ctrl Pts',(-9.79283541045386,22.0843789276208,
2.34050072497862));
#101890=CARTESIAN_POINT('Ctrl Pts',(-9.77695900832715,22.0832314482922,
2.34344973863966));
#101891=CARTESIAN_POINT('Ctrl Pts',(-9.75059291391459,22.0813413382915,
2.34891036631903));
#101892=CARTESIAN_POINT('Ctrl Pts',(-9.74006838971411,22.0805910350128,
2.35124118369179));
#101893=CARTESIAN_POINT('Ctrl Pts',(-9.72553964738539,22.0795624077329,
2.35466870128597));
#101894=CARTESIAN_POINT('Ctrl Pts',(-9.72150738656724,22.0792776921328,
2.35564247957726));
#101895=CARTESIAN_POINT('Ctrl Pts',(-9.71468602652686,22.0787974358861,
2.35732800699329));
#101896=CARTESIAN_POINT('Ctrl Pts',(-9.71189426241367,22.0786012801257,
2.35802870801962));
#101897=CARTESIAN_POINT('Ctrl Pts',(-9.70654196415059,22.0782260135799,
2.35939295117848));
#101898=CARTESIAN_POINT('Ctrl Pts',(-9.70398107014798,22.0780468096624,
2.36005489073016));
#101899=CARTESIAN_POINT('Ctrl Pts',(-9.69784286012353,22.0776180640313,
2.36166357413394));
#101900=CARTESIAN_POINT('Ctrl Pts',(-9.69426770543513,22.0773689881369,
2.3626185685466));
#101901=CARTESIAN_POINT('Ctrl Pts',(-9.68128846490411,22.0764668861262,
2.3661512009867));
#101902=CARTESIAN_POINT('Ctrl Pts',(-9.67191166545329,22.0758192644764,
2.3688288362949));
#101903=CARTESIAN_POINT('Ctrl Pts',(-9.60396894989899,22.0711492975925,
2.38914649991693));
#101904=CARTESIAN_POINT('Ctrl Pts',(-9.54681501114852,22.0673407774482,
2.41121101967124));
#101905=CARTESIAN_POINT('Ctrl Pts',(-9.43122370003349,22.0594074206221,
2.46652395825332));
#101906=CARTESIAN_POINT('Ctrl Pts',(-9.37339822592928,22.0552976053787,
2.50052573707119));
#101907=CARTESIAN_POINT('Ctrl Pts',(-9.29044656281656,22.048833136515,2.55934326753237));
#101908=CARTESIAN_POINT('Ctrl Pts',(-9.26302129996159,22.0465908391404,
2.58067241863764));
#101909=CARTESIAN_POINT('Ctrl Pts',(-9.22963691461689,22.0436995464849,
2.60909095729312));
#101910=CARTESIAN_POINT('Ctrl Pts',(-9.22276266541128,22.0430950781334,
2.61508174180841));
#101911=CARTESIAN_POINT('Ctrl Pts',(-9.21182992672751,22.0421185383506,
2.62483509325445));
#101912=CARTESIAN_POINT('Ctrl Pts',(-9.20772709699707,22.0417485446261,
2.62854757801004));
#101913=CARTESIAN_POINT('Ctrl Pts',(-9.19996196585082,22.0410414471881,
2.63567409326709));
#101914=CARTESIAN_POINT('Ctrl Pts',(-9.19629496727374,22.0407045704094,
2.63908284476846));
#101915=CARTESIAN_POINT('Ctrl Pts',(-9.18795891131913,22.0399318846853,
2.64693151218014));
#101916=CARTESIAN_POINT('Ctrl Pts',(-9.18330436444943,22.039495435716,2.65138653638812));
#101917=CARTESIAN_POINT('Ctrl Pts',(-9.16900058793069,22.0381383789181,
2.66530384018087));
#101918=CARTESIAN_POINT('Ctrl Pts',(-9.15947779084611,22.0372122538678,
2.67489389075329));
#101919=CARTESIAN_POINT('Ctrl Pts',(-9.07984663606967,22.0292685678515,
2.75789670383281));
#101920=CARTESIAN_POINT('Ctrl Pts',(-9.01934912951955,22.0218333625618,
2.83991299501524));
#101921=CARTESIAN_POINT('Ctrl Pts',(-8.94198618195627,22.0101346966179,
2.97936010306964));
#101922=CARTESIAN_POINT('Ctrl Pts',(-8.91763002963586,22.0059055615872,
3.03209403724379));
#101923=CARTESIAN_POINT('Ctrl Pts',(-8.89471958978426,22.0013639490506,
3.09318001584837));
#101924=CARTESIAN_POINT('Ctrl Pts',(-8.89224413626641,22.0008639956864,
3.09996970409996));
#101925=CARTESIAN_POINT('Ctrl Pts',(-8.88865156322865,22.000124765676,3.11011258122135));
#101926=CARTESIAN_POINT('Ctrl Pts',(-8.88748684223309,21.9998828559432,
3.11344855212162));
#101927=CARTESIAN_POINT('Ctrl Pts',(-8.88551605898633,21.9994696833693,
3.11917592561827));
#101928=CARTESIAN_POINT('Ctrl Pts',(-8.88470265195474,21.999297996826,3.12156472641531));
#101929=CARTESIAN_POINT('Ctrl Pts',(-8.88287277281675,21.9989091200592,
3.12699583242468));
#101930=CARTESIAN_POINT('Ctrl Pts',(-8.88186104704888,21.9986922082007,
3.13003968691543));
#101931=CARTESIAN_POINT('Ctrl Pts',(-8.87914289687149,21.9981040993601,
3.1383304574281));
#101932=CARTESIAN_POINT('Ctrl Pts',(-8.8774608600233,21.9977342835829,3.14358537369414));
#101933=CARTESIAN_POINT('Ctrl Pts',(-8.86929898277906,21.9959090549653,
3.16971525283914));
#101934=CARTESIAN_POINT('Ctrl Pts',(-8.8633637300722,21.9944823236821,3.19075747016308));
#101935=CARTESIAN_POINT('Ctrl Pts',(-8.85261760544848,21.991656970104,3.23336143327061));
#101936=CARTESIAN_POINT('Ctrl Pts',(-8.84782074009101,21.9902593388887,
3.25491728925781));
#101937=CARTESIAN_POINT('Ctrl Pts',(-8.82475682652325,21.9826318004815,
3.37429918182883));
#101938=CARTESIAN_POINT('Ctrl Pts',(-8.81833950296988,21.9766386422591,
3.47399664970996));
#101939=CARTESIAN_POINT('Ctrl Pts',(-8.82625031172498,21.9684940855511,
3.60083017933001));
#101940=CARTESIAN_POINT('Ctrl Pts',(-8.82893183874177,21.9667033237362,
3.62827402932933));
#101941=CARTESIAN_POINT('Ctrl Pts',(-8.83368978543899,21.9643246228715,
3.66397237620907));
#101942=CARTESIAN_POINT('Ctrl Pts',(-8.83489615623078,21.9637638306331,
3.67233538173899));
#101943=CARTESIAN_POINT('Ctrl Pts',(-8.83701882998091,21.9628408896615,
3.68600774328032));
#101944=CARTESIAN_POINT('Ctrl Pts',(-8.83788177904923,21.9624804194345,
3.69132517155686));
#101945=CARTESIAN_POINT('Ctrl Pts',(-8.83962481761764,21.9617795913581,
3.70161853040299));
#101946=CARTESIAN_POINT('Ctrl Pts',(-8.84050051241438,21.9614393789712,
3.70659509337616));
#101947=CARTESIAN_POINT('Ctrl Pts',(-8.84260295194821,21.9606490044631,
3.71810862347875));
#101948=CARTESIAN_POINT('Ctrl Pts',(-8.84385309035559,21.9601981136261,
3.72464108849274));
#101949=CARTESIAN_POINT('Ctrl Pts',(-8.84811095153056,21.958721677096,3.74591250977103));
#101950=CARTESIAN_POINT('Ctrl Pts',(-8.85134562441883,21.9576890189019,
3.76060397433992));
#101951=CARTESIAN_POINT('Ctrl Pts',(-8.87382280160247,21.9510294572635,
3.85412431780265));
#101952=CARTESIAN_POINT('Ctrl Pts',(-8.90088399175274,21.9451510444456,
3.93083474910885));
#101953=CARTESIAN_POINT('Ctrl Pts',(-8.95902781007525,21.9351826698706,
4.05359376450294));
#101954=CARTESIAN_POINT('Ctrl Pts',(-8.98586914502017,21.931151211646,4.10135541725436));
#101955=CARTESIAN_POINT('Ctrl Pts',(-9.02480804608973,21.9260695019658,
4.16057286638449));
#101956=CARTESIAN_POINT('Ctrl Pts',(-9.03395780744671,21.9249217451991,
4.17388307301617));
#101957=CARTESIAN_POINT('Ctrl Pts',(-9.04966730272038,21.9230312281458,
4.19575789218673));
#101958=CARTESIAN_POINT('Ctrl Pts',(-9.05607592125321,21.9222807912769,
4.20442787731998));
#101959=CARTESIAN_POINT('Ctrl Pts',(-9.06511437510329,21.9212520129367,
4.21631078429671));
#101960=CARTESIAN_POINT('Ctrl Pts',(-9.06764326070904,21.9209672774621,
4.21959932139397));
#101961=CARTESIAN_POINT('Ctrl Pts',(-9.07195617667646,21.920486997575,4.22514688813352));
#101962=CARTESIAN_POINT('Ctrl Pts',(-9.07373119394163,21.9202908379102,
4.2274128449363));
#101963=CARTESIAN_POINT('Ctrl Pts',(-9.07715321574078,21.9199155716973,
4.23174850260919));
#101964=CARTESIAN_POINT('Ctrl Pts',(-9.07879890168456,21.9197363719713,
4.23381918420263));
#101965=CARTESIAN_POINT('Ctrl Pts',(-9.08276352632826,21.9193076465659,
4.23877331111639));
#101966=CARTESIAN_POINT('Ctrl Pts',(-9.08508912329468,21.9190585866078,
4.2416514292178));
#101967=CARTESIAN_POINT('Ctrl Pts',(-9.09359112434942,21.9181566263438,
4.25207250642525));
#101968=CARTESIAN_POINT('Ctrl Pts',(-9.09984776648703,21.9175091282161,
4.25954991706177));
#101969=CARTESIAN_POINT('Ctrl Pts',(-9.14630040786892,21.9128115822555,
4.31368587186263));
#101970=CARTESIAN_POINT('Ctrl Pts',(-9.19001369223749,21.9089783890553,
4.35721169676561));
#101971=CARTESIAN_POINT('Ctrl Pts',(-9.28770567613959,21.9010392725421,
4.44030531977779));
#101972=CARTESIAN_POINT('Ctrl Pts',(-9.34204561852476,21.8969476846134,
4.47909790200215));
#101973=CARTESIAN_POINT('Ctrl Pts',(-9.42916919979026,21.8905082673321,
4.53075075722707));
#101974=CARTESIAN_POINT('Ctrl Pts',(-9.45972751884151,21.8882716146272,
4.54709131037607));
#101975=CARTESIAN_POINT('Ctrl Pts',(-9.49917526252393,21.8853866947294,
4.56599843030483));
#101976=CARTESIAN_POINT('Ctrl Pts',(-9.50743643005745,21.8847827083907,
4.56984073250448));
#101977=CARTESIAN_POINT('Ctrl Pts',(-9.52078347699878,21.8838067607989,
4.57586113628776));
#101978=CARTESIAN_POINT('Ctrl Pts',(-9.52584168407093,21.8834368726653,
4.57809997224384));
#101979=CARTESIAN_POINT('Ctrl Pts',(-9.53550815665088,21.8827298541608,
4.58229730682978));
#101980=CARTESIAN_POINT('Ctrl Pts',(-9.54011351929205,21.8823929498681,
4.58426221756415));
#101981=CARTESIAN_POINT('Ctrl Pts',(-9.55067618437587,21.8816200265718,
4.58868945198816));
#101982=CARTESIAN_POINT('Ctrl Pts',(-9.55664140962897,21.8811833661382,
4.59113233460971));
#101983=CARTESIAN_POINT('Ctrl Pts',(-9.57518925560504,21.8798249885159,
4.59855085017303));
#101984=CARTESIAN_POINT('Ctrl Pts',(-9.58783740389136,21.8788977386115,
4.6033585576613));
#101985=CARTESIAN_POINT('Ctrl Pts',(-9.6959403248465,21.8709614747477,4.64233160564095));
#101986=CARTESIAN_POINT('Ctrl Pts',(-9.79533868790776,21.8635360269073,
4.66425041570765));
#101987=CARTESIAN_POINT('Ctrl Pts',(-9.95415924840633,21.8518392909558,
4.67829073224624));
#101988=CARTESIAN_POINT('Ctrl Pts',(-10.0123378697796,21.8476027582929,
4.67911823295361));
#101989=CARTESIAN_POINT('Ctrl Pts',(-10.0775621651369,21.8430541521517,
4.67521548465421));
#101990=CARTESIAN_POINT('Ctrl Pts',(-10.0847746276831,21.8425540039893,
4.6747172399784));
#101991=CARTESIAN_POINT('Ctrl Pts',(-10.0955053962565,21.8418145433738,
4.67387659930378));
#101992=CARTESIAN_POINT('Ctrl Pts',(-10.0990273227439,21.8415725954983,
4.67358473971121));
#101993=CARTESIAN_POINT('Ctrl Pts',(-10.1050618889919,21.8411593804347,
4.67305730047634));
#101994=CARTESIAN_POINT('Ctrl Pts',(-10.1075751374841,21.8409876892926,
4.67282949355771));
#101995=CARTESIAN_POINT('Ctrl Pts',(-10.1132808253094,21.8405988327509,
4.67229382109334));
#101996=CARTESIAN_POINT('Ctrl Pts',(-10.1164727512392,21.8403819455252,
4.67198099267715));
#101997=CARTESIAN_POINT('Ctrl Pts',(-10.1251505967325,21.8397939691701,
4.67109470750654));
#101998=CARTESIAN_POINT('Ctrl Pts',(-10.1306339149798,21.8394242602091,
4.67049573644395));
#101999=CARTESIAN_POINT('Ctrl Pts',(-10.1578046359435,21.8376004159884,
4.66733442426051));
#102000=CARTESIAN_POINT('Ctrl Pts',(-10.1794236259989,21.8361749103093,
4.66420757216516));
#102001=CARTESIAN_POINT('Ctrl Pts',(-10.222702197749,21.8333504808757,4.65671360904641));
#102002=CARTESIAN_POINT('Ctrl Pts',(-10.2443505002342,21.831952592415,4.65233483538477));
#102003=CARTESIAN_POINT('Ctrl Pts',(-10.3627757890489,21.8243265834302,
4.62489332615178));
#102004=CARTESIAN_POINT('Ctrl Pts',(-10.4564486897553,21.8183352226786,
4.59025059363022));
#102005=CARTESIAN_POINT('Ctrl Pts',(-10.5691322067729,21.8101904217924,
4.53147747594666));
#102006=CARTESIAN_POINT('Ctrl Pts',(-10.5931522809165,21.808397136702,4.51785432757466));
#102007=CARTESIAN_POINT('Ctrl Pts',(-10.6238724416345,21.8060155521596,
4.49897432634854));
#102008=CARTESIAN_POINT('Ctrl Pts',(-10.6310266925503,21.8054544839664,
4.49447063065251));
#102009=CARTESIAN_POINT('Ctrl Pts',(-10.64266020199,21.8045312049652,4.48697110243191));
#102010=CARTESIAN_POINT('Ctrl Pts',(-10.6471685645495,21.8041706750826,
4.48402080245969));
#102011=CARTESIAN_POINT('Ctrl Pts',(-10.6558652109445,21.8034698141119,
4.47824404771403));
#102012=CARTESIAN_POINT('Ctrl Pts',(-10.6600558685892,21.8031296290296,
4.47542136576162));
#102013=CARTESIAN_POINT('Ctrl Pts',(-10.6697185904393,21.8023394405889,
4.46882210816201));
#102014=CARTESIAN_POINT('Ctrl Pts',(-10.6751770520304,21.8018887095739,
4.46502601669752));
#102015=CARTESIAN_POINT('Ctrl Pts',(-10.6928687426397,21.8004133416613,
4.45249874025107));
#102016=CARTESIAN_POINT('Ctrl Pts',(-10.7049666077899,21.7993816065526,
4.44357988015936));
#102017=CARTESIAN_POINT('Ctrl Pts',(-10.7816628972542,21.7926886960074,
4.38473901599613));
#102018=CARTESIAN_POINT('Ctrl Pts',(-10.8410816839392,21.7867725861585,
4.32845458620045));
#102019=CARTESIAN_POINT('Ctrl Pts',(-10.9295621806644,21.7767945812469,
4.22523266426164));
#102020=CARTESIAN_POINT('Ctrl Pts',(-10.9620329983566,21.7727915361459,
4.18157270232591));
#102021=CARTESIAN_POINT('Ctrl Pts',(-11.0000593999272,21.7677416241228,
4.1222821666571));
#102022=CARTESIAN_POINT('Ctrl Pts',(-11.0084669995646,21.766598302739,4.10856245668405));
#102023=CARTESIAN_POINT('Ctrl Pts',(-11.0220193037739,21.7647142948109,
4.08539488592011));
#102024=CARTESIAN_POINT('Ctrl Pts',(-11.0273202899451,21.7639659951333,
4.0760413806091));
#102025=CARTESIAN_POINT('Ctrl Pts',(-11.0344862644481,21.7629396338561,
4.06298348298946));
#102026=CARTESIAN_POINT('Ctrl Pts',(-11.0364606939359,21.7626552166709,
4.05934020478251));
#102027=CARTESIAN_POINT('Ctrl Pts',(-11.0397735368128,21.7621753153193,
4.05314946844439));
#102028=CARTESIAN_POINT('Ctrl Pts',(-11.0411219062584,21.7619792181189,
4.0506074093977));
#102029=CARTESIAN_POINT('Ctrl Pts',(-11.0436922694824,21.7616039463091,
4.04571834340991));
#102030=CARTESIAN_POINT('Ctrl Pts',(-11.0449156833096,21.7614246792558,
4.04337213660475));
#102031=CARTESIAN_POINT('Ctrl Pts',(-11.0478327183914,21.7609956290836,
4.03773169584484));
#102032=CARTESIAN_POINT('Ctrl Pts',(-11.0495187396879,21.7607463132603,
4.03443353040128));
#102033=CARTESIAN_POINT('Ctrl Pts',(-11.055599397633,21.7598420704948,4.02239890020367));
#102034=CARTESIAN_POINT('Ctrl Pts',(-11.0599008853495,21.7591925826536,
4.01361544740916));
#102035=CARTESIAN_POINT('Ctrl Pts',(-11.0899349554065,21.7545782477769,
3.95030253735665));
#102036=CARTESIAN_POINT('Ctrl Pts',(-11.1115592611839,21.7508208994187,
3.8939143403414));
#102037=CARTESIAN_POINT('Ctrl Pts',(-11.1480598909885,21.7429008557308,
3.77133335846606));
#102038=CARTESIAN_POINT('Ctrl Pts',(-11.1617357242476,21.738754741515,3.70501902657362));
#102039=CARTESIAN_POINT('Ctrl Pts',(-11.1737361384073,21.7322404507094,
3.60323288527593));
#102040=CARTESIAN_POINT('Ctrl Pts',(-11.1762797282096,21.7299870019384,
3.56840456654972));
#102041=CARTESIAN_POINT('Ctrl Pts',(-11.1775328855013,21.7270831215993,
3.52438799562588));
#102042=CARTESIAN_POINT('Ctrl Pts',(-11.1776865905774,21.7264777052935,
3.51525638774523));
#102043=CARTESIAN_POINT('Ctrl Pts',(-11.1777628658049,21.7255000008533,
3.50058785196672));
#102044=CARTESIAN_POINT('Ctrl Pts',(-11.1777526159938,21.7251297994593,
3.49505152759654));
#102045=CARTESIAN_POINT('Ctrl Pts',(-11.1776587691406,21.7244225462642,
3.4845098335991));
#102046=CARTESIAN_POINT('Ctrl Pts',(-11.1775822923772,21.7240857230801,
3.47950450938479));
#102047=CARTESIAN_POINT('Ctrl Pts',(-11.1773345385335,21.7233135020717,
3.46806441387532));
#102048=CARTESIAN_POINT('Ctrl Pts',(-11.1771424130771,21.7228774669752,
3.46163030151686));
#102049=CARTESIAN_POINT('Ctrl Pts',(-11.1763846681915,21.7215229929797,
3.44172511825552));
#102050=CARTESIAN_POINT('Ctrl Pts',(-11.1756404777487,21.7205990670929,
3.4282623517072));
#102051=CARTESIAN_POINT('Ctrl Pts',(-11.1673054868669,21.712640992128,3.31332524974692));
#102052=CARTESIAN_POINT('Ctrl Pts',(-11.1468247047791,21.7051868421417,
3.21323517264621));
#102053=CARTESIAN_POINT('Ctrl Pts',(-11.0949534582972,21.6934844066775,
3.06237657518924));
#102054=CARTESIAN_POINT('Ctrl Pts',(-11.0721530844793,21.6892696002597,
3.00915716045355));
#102055=CARTESIAN_POINT('Ctrl Pts',(-11.0422085638946,21.684741537234,2.95141225303632));
#102056=CARTESIAN_POINT('Ctrl Pts',(-11.0388253390069,21.6842419624985,
2.94503231773434));
#102057=CARTESIAN_POINT('Ctrl Pts',(-11.0337000424018,21.6835031807407,
2.93557838272303));
#102058=CARTESIAN_POINT('Ctrl Pts',(-11.032002552061,21.6832613451691,2.93248059674107));
#102059=CARTESIAN_POINT('Ctrl Pts',(-11.0290685811872,21.6828482551897,
2.92718302660301));
#102060=CARTESIAN_POINT('Ctrl Pts',(-11.0278389432434,21.6826765775692,
2.92497953341313));
#102061=CARTESIAN_POINT('Ctrl Pts',(-11.0250298177703,21.6822876613856,
2.91998342431266));
#102062=CARTESIAN_POINT('Ctrl Pts',(-11.0234459957428,21.6820707015592,
2.91719329978942));
#102063=CARTESIAN_POINT('Ctrl Pts',(-11.0191059142591,21.6814823347117,
2.90961989028381));
#102064=CARTESIAN_POINT('Ctrl Pts',(-11.01632735048,21.6811123109142,2.90484938203497));
#102065=CARTESIAN_POINT('Ctrl Pts',(-11.0023628099584,21.6792843822694,
2.88125671805755));
#102066=CARTESIAN_POINT('Ctrl Pts',(-10.990686216488,21.6778552604976,2.86272814221592));
#102067=CARTESIAN_POINT('Ctrl Pts',(-10.96621566679,21.6750281030935,2.82619775654785));
#102068=CARTESIAN_POINT('Ctrl Pts',(-10.9534187904661,21.6736309723582,
2.80820892944009));
#102069=CARTESIAN_POINT('Ctrl Pts',(-10.8801490287803,21.6660004258613,
2.71111054368101));
#102070=CARTESIAN_POINT('Ctrl Pts',(-10.8103410218032,21.6600037390744,
2.63956011151695));
#102071=CARTESIAN_POINT('Ctrl Pts',(-10.710833322145,21.6518596486799,2.560549759865));
#102072=CARTESIAN_POINT('Ctrl Pts',(-10.6887140681461,21.6500738265903,
2.54421576256108));
#102073=CARTESIAN_POINT('Ctrl Pts',(-10.6590832186332,21.6477007717478,
2.52389773705692));
#102074=CARTESIAN_POINT('Ctrl Pts',(-10.6520705008869,21.6471405208899,
2.519199116786));
#102075=CARTESIAN_POINT('Ctrl Pts',(-10.6405022230419,21.6462182430471,
2.5116271122258));
#102076=CARTESIAN_POINT('Ctrl Pts',(-10.635976305133,21.6458578898257,2.50870882144673));
#102077=CARTESIAN_POINT('Ctrl Pts',(-10.6271645184658,21.6451571259854,
2.50311220786298));
#102078=CARTESIAN_POINT('Ctrl Pts',(-10.6228811040013,21.6448168597622,
2.5004302264277));
#102079=CARTESIAN_POINT('Ctrl Pts',(-10.6129169555056,21.6440261189539,
2.49428027520603));
#102080=CARTESIAN_POINT('Ctrl Pts',(-10.6072238673351,21.6435749135678,
2.49083275372079));
#102081=CARTESIAN_POINT('Ctrl Pts',(-10.588546741144,21.6420963723018,2.47973784719996));
#102082=CARTESIAN_POINT('Ctrl Pts',(-10.5754455657394,21.6410618957317,
2.4722916312653));
#102083=CARTESIAN_POINT('Ctrl Pts',(-10.4919220581323,21.6344803743921,
2.42691782964652));
#102084=CARTESIAN_POINT('Ctrl Pts',(-10.417944416415,21.6286896827707,2.39600237227468));
#102085=CARTESIAN_POINT('Ctrl Pts',(-10.2882084112286,21.6187433255133,
2.35670553029678));
#102086=CARTESIAN_POINT('Ctrl Pts',(-10.2339198405707,21.614645101014,2.34437531602081));
#102087=CARTESIAN_POINT('Ctrl Pts',(-10.1628597976156,21.6094887866822,
2.33345075892763));
#102088=CARTESIAN_POINT('Ctrl Pts',(-10.1467078797446,21.6083307151759,
2.33130957908645));
#102089=CARTESIAN_POINT('Ctrl Pts',(-10.1197322636978,21.606425073981,2.32830166828272));
#102090=CARTESIAN_POINT('Ctrl Pts',(-10.1089320173734,21.6056696792347,
2.32724826488207));
#102091=CARTESIAN_POINT('Ctrl Pts',(-10.0939738268989,21.6046352969177,
2.32599775173931));
#102092=CARTESIAN_POINT('Ctrl Pts',(-10.0898274850354,21.6043498258082,
2.32567322123748));
#102093=CARTESIAN_POINT('Ctrl Pts',(-10.0828066694807,21.6038686705337,
2.32516111118792));
#102094=CARTESIAN_POINT('Ctrl Pts',(-10.0799330934752,21.6036723659857,
2.32496210256212));
#102095=CARTESIAN_POINT('Ctrl Pts',(-10.0744218041311,21.6032971104566,
2.32460073125346));
#102096=CARTESIAN_POINT('Ctrl Pts',(-10.0717842465693,21.6031180646089,
2.3244367017482));
#102097=CARTESIAN_POINT('Ctrl Pts',(-10.0654611566832,21.6026900827338,
2.32406482940919));
#102098=CARTESIAN_POINT('Ctrl Pts',(-10.0617751268381,21.6024416088264,
2.32386543155666));
#102099=CARTESIAN_POINT('Ctrl Pts',(-10.0484195788042,21.60154480173,2.32320591593911));
#102100=CARTESIAN_POINT('Ctrl Pts',(-10.0387450939451,21.6009017880161,
2.32284767149286));
#102101=CARTESIAN_POINT('Ctrl Pts',(-9.96163517026617,21.595821520519,2.32094401604707));
#102102=CARTESIAN_POINT('Ctrl Pts',(-9.89417523585574,21.5916457831624,
2.32507510158336));
#102103=CARTESIAN_POINT('Ctrl Pts',(-9.82198378129026,21.5871330419721,
2.33576822427561));
#102104=CARTESIAN_POINT('Ctrl Pts',(-9.81654085550856,21.5867925610894,
2.33661350190372));
#102105=CARTESIAN_POINT('Ctrl Pts',(-9.81110406371016,21.5864520766487,
2.33749693000268));
#102106=CARTESIAN_POINT('Ctrl Pts',(-9.81110407243713,21.4868028556135,
2.33749692858463));
#102107=CARTESIAN_POINT('Ctrl Pts',(-9.81517067467535,21.4870722770751,
2.33683614357623));
#102108=CARTESIAN_POINT('Ctrl Pts',(-9.81924120982507,21.4873423546502,
2.33619662123157));
#102109=CARTESIAN_POINT('Ctrl Pts',(-9.83303428352159,21.4882589494198,
2.33410371765976));
#102110=CARTESIAN_POINT('Ctrl Pts',(-9.84277088387619,21.4889083879988,
2.33275080332901));
#102111=CARTESIAN_POINT('Ctrl Pts',(-9.8587378479823,21.4899778809616,2.33073557055172));
#102112=CARTESIAN_POINT('Ctrl Pts',(-9.86495870835362,21.4903956735842,
2.33000079121547));
#102113=CARTESIAN_POINT('Ctrl Pts',(-9.87614085585395,21.4911487887447,
2.32877037586977));
#102114=CARTESIAN_POINT('Ctrl Pts',(-9.88110002354407,21.4914835355677,
2.32825654927539));
#102115=CARTESIAN_POINT('Ctrl Pts',(-9.89167004103714,21.4921986798962,
2.32722916687655));
#102116=CARTESIAN_POINT('Ctrl Pts',(-9.8972815953929,21.4925793412509,2.32672435699143));
#102117=CARTESIAN_POINT('Ctrl Pts',(-9.91244938790626,21.4936110516241,
2.32546952546572));
#102118=CARTESIAN_POINT('Ctrl Pts',(-9.92201134098397,21.4942644542814,
2.32479588798927));
#102119=CARTESIAN_POINT('Ctrl Pts',(-9.97262803496219,21.4977399671803,
2.32185040525782));
#102120=CARTESIAN_POINT('Ctrl Pts',(-10.0137679521485,21.5006242779217,
2.32161320888497));
#102121=CARTESIAN_POINT('Ctrl Pts',(-10.1588035758424,21.511005580528,2.32837290664097));
#102122=CARTESIAN_POINT('Ctrl Pts',(-10.2616586579371,21.518802440347,2.34697807224981));
#102123=CARTESIAN_POINT('Ctrl Pts',(-10.3830147408723,21.5279392074216,
2.38602373832498));
#102124=CARTESIAN_POINT('Ctrl Pts',(-10.4050890730134,21.5295958415547,
2.3938596713672));
#102125=CARTESIAN_POINT('Ctrl Pts',(-10.4321713656941,21.5316097259848,
2.4043929715578));
#102126=CARTESIAN_POINT('Ctrl Pts',(-10.4374113586635,21.5319984981899,
2.40647443715146));
#102127=CARTESIAN_POINT('Ctrl Pts',(-10.4456337560816,21.5326069290953,
2.40980915418591));
#102128=CARTESIAN_POINT('Ctrl Pts',(-10.4486262053365,21.5328280218014,
2.41103716620755));
#102129=CARTESIAN_POINT('Ctrl Pts',(-10.4539394730286,21.533219932796,2.41324319208894));
#102130=CARTESIAN_POINT('Ctrl Pts',(-10.4562622058674,21.53339103251,2.41421631785437));
#102131=CARTESIAN_POINT('Ctrl Pts',(-10.4617984758005,21.5337983263239,
2.41655668087407));
#102132=CARTESIAN_POINT('Ctrl Pts',(-10.4650090696985,21.5340341059273,
2.41793076751005));
#102133=CARTESIAN_POINT('Ctrl Pts',(-10.4746577872373,21.5347415660773,
2.42211115092003));
#102134=CARTESIAN_POINT('Ctrl Pts',(-10.4810771105898,21.5352107312872,
2.42496083532509));
#102135=CARTESIAN_POINT('Ctrl Pts',(-10.4958657975622,21.5362889463584,
2.43168486873679));
#102136=CARTESIAN_POINT('Ctrl Pts',(-10.504216016322,21.5368957720601,2.43560048402255));
#102137=CARTESIAN_POINT('Ctrl Pts',(-10.610265072029,21.544588056823,2.48685750011809));
#102138=CARTESIAN_POINT('Ctrl Pts',(-10.7010211253718,21.5510541319297,
2.54739445712384));
#102139=CARTESIAN_POINT('Ctrl Pts',(-10.8175293886042,21.5608412143302,
2.65089858870542));
#102140=CARTESIAN_POINT('Ctrl Pts',(-10.8509281605442,21.5638591628275,
2.68437265775023));
#102141=CARTESIAN_POINT('Ctrl Pts',(-10.8889929303099,21.5676385469017,
2.72741276953132));
#102142=CARTESIAN_POINT('Ctrl Pts',(-10.895661765706,21.5683145195203,2.73515397008703));
#102143=CARTESIAN_POINT('Ctrl Pts',(-10.9059777810372,21.5693828140017,
2.74744877896466));
#102144=CARTESIAN_POINT('Ctrl Pts',(-10.9096933918586,21.569772357924,2.75194451358904));
#102145=CARTESIAN_POINT('Ctrl Pts',(-10.9161986784941,21.5704629701072,
2.75993578435973));
#102146=CARTESIAN_POINT('Ctrl Pts',(-10.91900214559,21.5707634784891,2.76341998588178));
#102147=CARTESIAN_POINT('Ctrl Pts',(-10.9253936401151,21.5714553237191,
2.77145674623781));
#102148=CARTESIAN_POINT('Ctrl Pts',(-10.928968013463,21.5718471905044,2.77601996598856));
#102149=CARTESIAN_POINT('Ctrl Pts',(-10.938820813771,21.5729414296021,2.7887916354707));
#102150=CARTESIAN_POINT('Ctrl Pts',(-10.9450249768115,21.5736466665227,
2.7970564464425));
#102151=CARTESIAN_POINT('Ctrl Pts',(-10.9839092432363,21.5781731378335,
2.85030099869168));
#102152=CARTESIAN_POINT('Ctrl Pts',(-11.0134735994954,21.5821113117776,
2.89745889831677));
#102153=CARTESIAN_POINT('Ctrl Pts',(-11.0782934478732,21.59209333158,3.01920956130157));
#102154=CARTESIAN_POINT('Ctrl Pts',(-11.1092601515494,21.5982219388943,
3.09575101075284));
#102155=CARTESIAN_POINT('Ctrl Pts',(-11.1398953365033,21.6062232699944,
3.20241999968618));
#102156=CARTESIAN_POINT('Ctrl Pts',(-11.1467948879311,21.6082599998995,
3.23022782064838));
#102157=CARTESIAN_POINT('Ctrl Pts',(-11.1537939556788,21.610625814954,3.2636013268679));
#102158=CARTESIAN_POINT('Ctrl Pts',(-11.1548766312647,21.6110024898336,
3.26894850305121));
#102159=CARTESIAN_POINT('Ctrl Pts',(-11.1565889857464,21.6116161724631,
3.2777184452769));
#102160=CARTESIAN_POINT('Ctrl Pts',(-11.1572407050726,21.6118543523878,
3.2811367485556));
#102161=CARTESIAN_POINT('Ctrl Pts',(-11.1583871701761,21.6122817857458,
3.28729833986086));
#102162=CARTESIAN_POINT('Ctrl Pts',(-11.1588873335337,21.6124713344613,
3.29004052555067));
#102163=CARTESIAN_POINT('Ctrl Pts',(-11.159968681859,21.6128880482592,3.29609070786868));
#102164=CARTESIAN_POINT('Ctrl Pts',(-11.1605454544756,21.6131149649992,
3.29939942393878));
#102165=CARTESIAN_POINT('Ctrl Pts',(-11.162175349159,21.6137701242357,3.30899185014391));
#102166=CARTESIAN_POINT('Ctrl Pts',(-11.163191666558,21.6141963706911,3.31528181774291));
#102167=CARTESIAN_POINT('Ctrl Pts',(-11.1708052012482,21.6175385550112,
3.36495866976929));
#102168=CARTESIAN_POINT('Ctrl Pts',(-11.1750245704109,21.6203351253198,
3.40868077583424));
#102169=CARTESIAN_POINT('Ctrl Pts',(-11.1810212841267,21.6296605105556,
3.5573764098261));
#102170=CARTESIAN_POINT('Ctrl Pts',(-11.1712224620157,21.6359739337432,
3.66230061828851));
#102171=CARTESIAN_POINT('Ctrl Pts',(-11.1427639967321,21.6441500726106,
3.78576171668288));
#102172=CARTESIAN_POINT('Ctrl Pts',(-11.1372851304337,21.6455712800106,
3.80684156451089));
#102173=CARTESIAN_POINT('Ctrl Pts',(-11.1289953473737,21.6475408609851,
3.83545309690688));
#102174=CARTESIAN_POINT('Ctrl Pts',(-11.1266868932461,21.6480731358535,
3.84312667327583));
#102175=CARTESIAN_POINT('Ctrl Pts',(-11.1228817617851,21.648925834145,3.85532280813239));
#102176=CARTESIAN_POINT('Ctrl Pts',(-11.1214356110884,21.6492446147442,
3.85986097034221));
#102177=CARTESIAN_POINT('Ctrl Pts',(-11.11840386614,21.6499023019012,3.86917911144047));
#102178=CARTESIAN_POINT('Ctrl Pts',(-11.1168150632454,21.6502413073615,
3.87395793516264));
#102179=CARTESIAN_POINT('Ctrl Pts',(-11.1130516254508,21.6510314954133,
3.88503973466421));
#102180=CARTESIAN_POINT('Ctrl Pts',(-11.1108540353886,21.6514834221491,
3.89133467399603));
#102181=CARTESIAN_POINT('Ctrl Pts',(-11.1036283972482,21.6529398350791,
3.91148093559938));
#102182=CARTESIAN_POINT('Ctrl Pts',(-11.0983939751393,21.6539510682763,
3.92525620591153));
#102183=CARTESIAN_POINT('Ctrl Pts',(-11.0854761480399,21.656349756588,3.95742068839113));
#102184=CARTESIAN_POINT('Ctrl Pts',(-11.0775819024816,21.6577438510636,
3.97571978771312));
#102185=CARTESIAN_POINT('Ctrl Pts',(-11.0282503144281,21.6660583343638,
4.08253579514326));
#102186=CARTESIAN_POINT('Ctrl Pts',(-10.9763910342186,21.6733139826275,
4.16580921944011));
#102187=CARTESIAN_POINT('Ctrl Pts',(-10.8890482099523,21.6834155845373,
4.27354262799605));
#102188=CARTESIAN_POINT('Ctrl Pts',(-10.8615892249823,21.686363070088,4.30401473160558));
#102189=CARTESIAN_POINT('Ctrl Pts',(-10.8283880077875,21.689625156212,4.33719993858729));
#102190=CARTESIAN_POINT('Ctrl Pts',(-10.8241499786093,21.690036280962,4.34137223929261));
#102191=CARTESIAN_POINT('Ctrl Pts',(-10.8173039659384,21.6906917487054,
4.34801071314387));
#102192=CARTESIAN_POINT('Ctrl Pts',(-10.8147160638966,21.6909375751822,
4.35049731242162));
#102193=CARTESIAN_POINT('Ctrl Pts',(-10.8100893005367,21.691373551303,4.35490246505053));
#102194=CARTESIAN_POINT('Ctrl Pts',(-10.8080549189143,21.6915640472247,
4.35682562300048));
#102195=CARTESIAN_POINT('Ctrl Pts',(-10.8036578351873,21.6919731877646,
4.36095271960525));
#102196=CARTESIAN_POINT('Ctrl Pts',(-10.8012929136054,21.6921916486279,
4.36315419751851));
#102197=CARTESIAN_POINT('Ctrl Pts',(-10.7946765873179,21.6927985207113,
4.36926263114877));
#102198=CARTESIAN_POINT('Ctrl Pts',(-10.790405395359,21.6931853643033,4.37314816309634));
#102199=CARTESIAN_POINT('Ctrl Pts',(-10.7648714480178,21.6954701744423,
4.39603565506007));
#102200=CARTESIAN_POINT('Ctrl Pts',(-10.7429508840491,21.6973182610938,
4.41429345348561));
#102201=CARTESIAN_POINT('Ctrl Pts',(-10.6598333726941,21.7040125223968,
4.47855692282397));
#102202=CARTESIAN_POINT('Ctrl Pts',(-10.5948562291706,21.7086610917834,
4.519363253048));
#102203=CARTESIAN_POINT('Ctrl Pts',(-10.4717687882584,21.7172236408201,
4.58085861958815));
#102204=CARTESIAN_POINT('Ctrl Pts',(-10.4151318874035,21.7210809082755,
4.60385015494241));
#102205=CARTESIAN_POINT('Ctrl Pts',(-10.3476362889929,21.7257346768253,
4.62531776545494));
#102206=CARTESIAN_POINT('Ctrl Pts',(-10.3382627663802,21.7263820325624,
4.62817080004644));
#102207=CARTESIAN_POINT('Ctrl Pts',(-10.3228493119951,21.7274487880799,
4.63265286029768));
#102208=CARTESIAN_POINT('Ctrl Pts',(-10.3168299435071,21.7278659459502,
4.63435134087523));
#102209=CARTESIAN_POINT('Ctrl Pts',(-10.3059892919184,21.7286183692001,
4.63731722238255));
#102210=CARTESIAN_POINT('Ctrl Pts',(-10.3011729165265,21.7289530633027,
4.63860211844908));
#102211=CARTESIAN_POINT('Ctrl Pts',(-10.2908895782006,21.7296685847242,
4.64127565950245));
#102212=CARTESIAN_POINT('Ctrl Pts',(-10.2854205228723,21.7300496790276,
4.64265567905805));
#102213=CARTESIAN_POINT('Ctrl Pts',(-10.270603132418,21.7310837896781,4.64628157147354));
#102214=CARTESIAN_POINT('Ctrl Pts',(-10.2612370354732,21.7317391784714,
4.64845230554885));
#102215=CARTESIAN_POINT('Ctrl Pts',(-10.2112493153471,21.7352470558314,
4.65939459278967));
#102216=CARTESIAN_POINT('Ctrl Pts',(-10.1702159203195,21.7381631471894,
4.66612516795698));
#102217=CARTESIAN_POINT('Ctrl Pts',(-10.0215775472286,21.748859530898,4.68249350971822));
#102218=CARTESIAN_POINT('Ctrl Pts',(-9.91313845917287,21.7569666946326,
4.67949465745268));
#102219=CARTESIAN_POINT('Ctrl Pts',(-9.78727160619767,21.7660655985922,
4.65854519447687));
#102220=CARTESIAN_POINT('Ctrl Pts',(-9.76799169907782,21.7674484957347,
4.65483877525444));
#102221=CARTESIAN_POINT('Ctrl Pts',(-9.74355635270306,21.7691800072668,
4.6495045271145));
#102222=CARTESIAN_POINT('Ctrl Pts',(-9.73830836911851,21.769550627205,4.6483211637927));
#102223=CARTESIAN_POINT('Ctrl Pts',(-9.73000585443508,21.7701347720265,
4.64638916250692));
#102224=CARTESIAN_POINT('Ctrl Pts',(-9.72694597658911,21.7703495845633,
4.64566419663078));
#102225=CARTESIAN_POINT('Ctrl Pts',(-9.72114922999216,21.770755588289,4.64426625110816));
#102226=CARTESIAN_POINT('Ctrl Pts',(-9.71841189973956,21.7709469039492,
4.64359570973499));
#102227=CARTESIAN_POINT('Ctrl Pts',(-9.71198796305757,21.7713949657094,
4.64199762681728));
#102228=CARTESIAN_POINT('Ctrl Pts',(-9.70830340620653,21.7716512529751,
4.64106205408025));
#102229=CARTESIAN_POINT('Ctrl Pts',(-9.69623647694154,21.7724884717113,
4.63793578290126));
#102230=CARTESIAN_POINT('Ctrl Pts',(-9.68787350053225,21.7730653395749,
4.63567036730967));
#102231=CARTESIAN_POINT('Ctrl Pts',(-9.64216108551712,21.7762038879674,
4.62274438232728));
#102232=CARTESIAN_POINT('Ctrl Pts',(-9.60532767950584,21.7786793262564,
4.61033240357154));
#102233=CARTESIAN_POINT('Ctrl Pts',(-9.48377213901692,21.7868737948191,
4.56255521807392));
#102234=CARTESIAN_POINT('Ctrl Pts',(-9.40258964468741,21.7924140098975,
4.51912522269836));
#102235=CARTESIAN_POINT('Ctrl Pts',(-9.29970956773928,21.8003863660617,
4.44753142954271));
#102236=CARTESIAN_POINT('Ctrl Pts',(-9.27298399161936,21.8025545923064,
4.42718385170613));
#102237=CARTESIAN_POINT('Ctrl Pts',(-9.23992868811659,21.805387415021,4.39970841119374));
#102238=CARTESIAN_POINT('Ctrl Pts',(-9.23276410357852,21.8060109662452,
4.39360656615301));
#102239=CARTESIAN_POINT('Ctrl Pts',(-9.22145705306379,21.8070108736661,
4.38374049225568));
#102240=CARTESIAN_POINT('Ctrl Pts',(-9.21726686606795,21.8073849667075,
4.38003137278449));
#102241=CARTESIAN_POINT('Ctrl Pts',(-9.20976067198723,21.8080616300315,
4.37329093106037));
#102242=CARTESIAN_POINT('Ctrl Pts',(-9.20643525465463,21.8083637542896,
4.37027021079243));
#102243=CARTESIAN_POINT('Ctrl Pts',(-9.1986493395123,21.8090767345027,4.3631159615435));
#102244=CARTESIAN_POINT('Ctrl Pts',(-9.19420344822566,21.8094882463053,
4.358966797307));
#102245=CARTESIAN_POINT('Ctrl Pts',(-9.18130597622644,21.810695095343,4.34674187503279));
#102246=CARTESIAN_POINT('Ctrl Pts',(-9.17294246221775,21.8114943316774,
4.33857469526382));
#102247=CARTESIAN_POINT('Ctrl Pts',(-9.1095662534862,21.817682511737,4.27481582433907));
#102248=CARTESIAN_POINT('Ctrl Pts',(-9.06010306459542,21.8233106859232,
4.21400368632121));
#102249=CARTESIAN_POINT('Ctrl Pts',(-8.97226763976339,21.8349916141909,
4.0809190027683));
#102250=CARTESIAN_POINT('Ctrl Pts',(-8.93463676396819,21.8410194355429,
4.00862942113423));
#102251=CARTESIAN_POINT('Ctrl Pts',(-8.90144387380693,21.8473341975225,
3.92467670187064));
#102252=CARTESIAN_POINT('Ctrl Pts',(-8.89823449662909,21.8479583939721,
3.91627953511174));
#102253=CARTESIAN_POINT('Ctrl Pts',(-8.8938860077113,21.8488229573773,3.90449922950167));
#102254=CARTESIAN_POINT('Ctrl Pts',(-8.89266575158476,21.8490677552318,
3.90114667358498));
#102255=CARTESIAN_POINT('Ctrl Pts',(-8.89057913328366,21.8494901282862,
3.89533177967653));
#102256=CARTESIAN_POINT('Ctrl Pts',(-8.88970569660362,21.8496681101149,
3.89287203478302));
#102257=CARTESIAN_POINT('Ctrl Pts',(-8.88787518624191,21.8500436081635,
3.88766214684093));
#102258=CARTESIAN_POINT('Ctrl Pts',(-8.88692012020401,21.8502410015256,
3.88491131839937));
#102259=CARTESIAN_POINT('Ctrl Pts',(-8.88457397826253,21.8507296778961,
3.87807208596694));
#102260=CARTESIAN_POINT('Ctrl Pts',(-8.88319515144265,21.8510202528708,
3.87397946983578));
#102261=CARTESIAN_POINT('Ctrl Pts',(-8.87808248896295,21.8521109793721,
3.85852366875419));
#102262=CARTESIAN_POINT('Ctrl Pts',(-8.87449915973305,21.8529029129152,
3.84711094567244));
#102263=CARTESIAN_POINT('Ctrl Pts',(-8.86579037159797,21.8549059325265,
3.81781977636356));
#102264=CARTESIAN_POINT('Ctrl Pts',(-8.86091321640439,21.8561055901371,
3.79987042147051));
#102265=CARTESIAN_POINT('Ctrl Pts',(-8.84014576814355,21.8616411204594,
3.71560027741768));
#102266=CARTESIAN_POINT('Ctrl Pts',(-8.82960884258752,21.8658049433229,
3.64809185660545));
#102267=CARTESIAN_POINT('Ctrl Pts',(-8.82021655868084,21.8743716551814,
3.5102204745359));
#102268=CARTESIAN_POINT('Ctrl Pts',(-8.82169371835029,21.8787637077503,
3.44011888749817));
#102269=CARTESIAN_POINT('Ctrl Pts',(-8.83047251192312,21.8840111599051,
3.36072085320286));
#102270=CARTESIAN_POINT('Ctrl Pts',(-8.83168553988959,21.8846656509144,
3.35088749681665));
#102271=CARTESIAN_POINT('Ctrl Pts',(-8.83387092222589,21.8857417822387,
3.3348407729421));
#102272=CARTESIAN_POINT('Ctrl Pts',(-8.83476925136269,21.8861611123166,
3.32861769007663));
#102273=CARTESIAN_POINT('Ctrl Pts',(-8.83646950996575,21.8869159084852,
3.31747125933727));
#102274=CARTESIAN_POINT('Ctrl Pts',(-8.83725297494085,21.8872507881111,
3.31254521395774));
#102275=CARTESIAN_POINT('Ctrl Pts',(-8.83898556986418,21.8879650437512,
3.30208048989017));
#102276=CARTESIAN_POINT('Ctrl Pts',(-8.83994309288268,21.8883446761303,
3.29654334658551));
#102277=CARTESIAN_POINT('Ctrl Pts',(-8.84254252260718,21.8893376479344,
3.28212666247222));
#102278=CARTESIAN_POINT('Ctrl Pts',(-8.84424696501407,21.8899529416023,
3.27325891994445));
#102279=CARTESIAN_POINT('Ctrl Pts',(-8.85269301864736,21.8928452054921,
3.23188885348993));
#102280=CARTESIAN_POINT('Ctrl Pts',(-8.86070420168162,21.8951617938466,
3.19966418467643));
#102281=CARTESIAN_POINT('Ctrl Pts',(-8.88870130724449,21.9022050723872,
3.10442895038725));
#102282=CARTESIAN_POINT('Ctrl Pts',(-8.91263795038509,21.9070402854017,
3.04272201003186));
#102283=CARTESIAN_POINT('Ctrl Pts',(-8.96938470451807,21.9165394902133,
2.92647254558138));
#102284=CARTESIAN_POINT('Ctrl Pts',(-9.00169479759932,21.9211851039395,
2.87191564100453));
#102285=CARTESIAN_POINT('Ctrl Pts',(-9.0438761486563,21.9263063678553,2.812237172837));
#102286=CARTESIAN_POINT('Ctrl Pts',(-9.04961488367065,21.9269857585909,
2.80432861797643));
#102287=CARTESIAN_POINT('Ctrl Pts',(-9.05766297932109,21.9279140265319,
2.79352303123261));
#102288=CARTESIAN_POINT('Ctrl Pts',(-9.05988837889258,21.9281681942064,
2.79056437308831));
#102289=CARTESIAN_POINT('Ctrl Pts',(-9.06372754037962,21.9286023272908,
2.78551001455653));
#102290=CARTESIAN_POINT('Ctrl Pts',(-9.06533446140725,21.928782752519,2.78340918979952));
#102291=CARTESIAN_POINT('Ctrl Pts',(-9.06870384169119,21.929158363504,2.77903481151096));
#102292=CARTESIAN_POINT('Ctrl Pts',(-9.07046757049206,21.929353451293,2.77676227958919));
#102293=CARTESIAN_POINT('Ctrl Pts',(-9.07479172303867,21.9298280969713,
2.77123263596257));
#102294=CARTESIAN_POINT('Ctrl Pts',(-9.07736107365033,21.9301070350908,
2.76798248687196));
#102295=CARTESIAN_POINT('Ctrl Pts',(-9.08644150371859,21.9310823360061,
2.75661978685024));
#102296=CARTESIAN_POINT('Ctrl Pts',(-9.09304308694545,21.9317726568497,
2.74857971568812));
#102297=CARTESIAN_POINT('Ctrl Pts',(-9.13127426651407,21.9356723478917,
2.70325596330276));
#102298=CARTESIAN_POINT('Ctrl Pts',(-9.16509833814906,21.9387493355969,
2.66787873877219));
#102299=CARTESIAN_POINT('Ctrl Pts',(-9.23675336229815,21.9448151996094,
2.60171600829347));
#102300=CARTESIAN_POINT('Ctrl Pts',(-9.27448774359679,21.9477991712231,
2.57097277677265));
#102301=CARTESIAN_POINT('Ctrl Pts',(-9.36390976967964,21.9546438464068,
2.5068977748864));
#102302=CARTESIAN_POINT('Ctrl Pts',(-9.41651685434449,21.9585215953546,
2.47510551062792));
#102303=CARTESIAN_POINT('Ctrl Pts',(-9.48011907270479,21.9631981330904,
2.44315799207569));
#102304=CARTESIAN_POINT('Ctrl Pts',(-9.48893559984864,21.9638459716114,
2.43886646567031));
#102305=CARTESIAN_POINT('Ctrl Pts',(-9.5034638314767,21.9649133616857,2.43201777090185));
#102306=CARTESIAN_POINT('Ctrl Pts',(-9.50914426702402,21.9653306667345,
2.42939509847233));
#102307=CARTESIAN_POINT('Ctrl Pts',(-9.51938767883757,21.9660832503043,
2.42476434680652));
#102308=CARTESIAN_POINT('Ctrl Pts',(-9.52394304996281,21.9664179565195,
2.42273972868125));
#102309=CARTESIAN_POINT('Ctrl Pts',(-9.53367852607802,21.967133389966,2.41848664170061));
#102310=CARTESIAN_POINT('Ctrl Pts',(-9.53886204128283,21.9675143834526,
2.41626634160683));
#102311=CARTESIAN_POINT('Ctrl Pts',(-9.54946689300735,21.9682940791329,
2.41181373166932));
#102312=CARTESIAN_POINT('Ctrl Pts',(-9.55488934683647,21.968692872576,2.40958451067744));
#102313=CARTESIAN_POINT('Ctrl Pts',(-9.56852944595827,21.9696964304524,
2.40409563520672));
#102314=CARTESIAN_POINT('Ctrl Pts',(-9.57676745552589,21.9703028971545,
2.4008878939507));
#102315=CARTESIAN_POINT('Ctrl Pts',(-9.65822383938616,21.9763040950047,
2.37022170619078));
#102316=CARTESIAN_POINT('Ctrl Pts',(-9.73394555776837,21.9819386115451,
2.350034469155));
#102317=CARTESIAN_POINT('Ctrl Pts',(-9.81110406961726,21.9876672748128,
2.33749692904284));
#102318=CARTESIAN_POINT('Origin',(-10.,12.3756328852638,3.5));
#102319=CARTESIAN_POINT('',(-9.81110404738689,22.5875279348072,2.33749693265506));
#102320=CARTESIAN_POINT('',(-9.81110406371112,22.4887934941609,2.33749693000253));
#102321=CARTESIAN_POINT('',(-9.81110406371068,12.3756328852638,2.3374969300026));
#102322=CARTESIAN_POINT('Ctrl Pts',(-9.81111389378217,22.5875286339524,
2.33749533275007));
#102323=CARTESIAN_POINT('Ctrl Pts',(-9.72555949551518,22.5814538128317,
2.35139712794946));
#102324=CARTESIAN_POINT('Ctrl Pts',(-9.64181293403421,22.5750945898088,
2.37469770477806));
#102325=CARTESIAN_POINT('Ctrl Pts',(-9.50651574673404,22.5643975402355,
2.42898871694999));
#102326=CARTESIAN_POINT('Ctrl Pts',(-9.45336513184311,22.5600820943743,
2.45511538686148));
#102327=CARTESIAN_POINT('Ctrl Pts',(-9.39614249259326,22.5554589601237,
2.4888106712376));
#102328=CARTESIAN_POINT('Ctrl Pts',(-9.38992182114609,22.5549567624739,
2.49255155457603));
#102329=CARTESIAN_POINT('Ctrl Pts',(-9.38071951120628,22.5542148761943,
2.49820198242319));
#102330=CARTESIAN_POINT('Ctrl Pts',(-9.37771139781822,22.5539725275117,
2.50006775817275));
#102331=CARTESIAN_POINT('Ctrl Pts',(-9.37257263360514,22.5535588655669,
2.50328723598973));
#102332=CARTESIAN_POINT('Ctrl Pts',(-9.37043787747973,22.5533871257053,
2.50463425396613));
#102333=CARTESIAN_POINT('Ctrl Pts',(-9.36560386870875,22.5529984797386,
2.50770625717497));
#102334=CARTESIAN_POINT('Ctrl Pts',(-9.36290731249977,22.5527818498101,
2.50943539756362));
#102335=CARTESIAN_POINT('Ctrl Pts',(-9.35560104202677,22.5521952569375,
2.51416264893798));
#102336=CARTESIAN_POINT('Ctrl Pts',(-9.35100514436171,22.551826663362,2.51718212262959));
#102337=CARTESIAN_POINT('Ctrl Pts',(-9.32843011714878,22.5500171932951,
2.5322411740018));
#102338=CARTESIAN_POINT('Ctrl Pts',(-9.31076270077627,22.5486044097237,
2.54474331094942));
#102339=CARTESIAN_POINT('Ctrl Pts',(-9.27575220616946,22.5457895456707,
2.57099546250814));
#102340=CARTESIAN_POINT('Ctrl Pts',(-9.25843229426695,22.5443889605833,
2.58476137869081));
#102341=CARTESIAN_POINT('Ctrl Pts',(-9.16563788696809,22.5367783291289,
2.66287931892294));
#102342=CARTESIAN_POINT('Ctrl Pts',(-9.09813992032658,22.5308051759434,
2.73607585946128));
#102343=CARTESIAN_POINT('Ctrl Pts',(-9.02981576249249,22.5232598586663,
2.8320298762372));
#102344=CARTESIAN_POINT('Ctrl Pts',(-9.0193805387261,22.5220566774688,2.84744582122026));
#102345=CARTESIAN_POINT('Ctrl Pts',(-9.00406702162296,22.5202064943524,
2.87126574924087));
#102346=CARTESIAN_POINT('Ctrl Pts',(-8.99891987268374,22.5195689635595,
2.87949389590779));
#102347=CARTESIAN_POINT('Ctrl Pts',(-8.98970894085492,22.5183983150926,
2.89463129119739));
#102348=CARTESIAN_POINT('Ctrl Pts',(-8.98561284684558,22.5178663823735,
2.90152026264539));
#102349=CARTESIAN_POINT('Ctrl Pts',(-8.97893653358354,22.5169799564346,
2.91301421125764));
#102350=CARTESIAN_POINT('Ctrl Pts',(-8.97631634759026,22.5166269036711,
2.91759576162104));
#102351=CARTESIAN_POINT('Ctrl Pts',(-8.9713586158957,22.5159487952961,2.92640147148972));
#102352=CARTESIAN_POINT('Ctrl Pts',(-8.96901607009313,22.5156239262654,
2.93062270498448));
#102353=CARTESIAN_POINT('Ctrl Pts',(-8.96360778275862,22.5148632997845,
2.94051117066737));
#102354=CARTESIAN_POINT('Ctrl Pts',(-8.96056248896243,22.5144268321504,
2.94618935014971));
#102355=CARTESIAN_POINT('Ctrl Pts',(-8.95127391195093,22.5130696588026,
2.96385511953369));
#102356=CARTESIAN_POINT('Ctrl Pts',(-8.94519046739396,22.5121434345011,
2.97592503967383));
#102357=CARTESIAN_POINT('Ctrl Pts',(-8.89519933581948,22.5042003059119,
3.07950859410976));
#102358=CARTESIAN_POINT('Ctrl Pts',(-8.86309288137422,22.4967658512563,
3.17622352672085));
#102359=CARTESIAN_POINT('Ctrl Pts',(-8.8327400315645,22.485067354181,3.33277516322405));
#102360=CARTESIAN_POINT('Ctrl Pts',(-8.82591983383854,22.4808376689838,
3.39046760746644));
#102361=CARTESIAN_POINT('Ctrl Pts',(-8.82306301311328,22.4762955362862,
3.45565344887865));
#102362=CARTESIAN_POINT('Ctrl Pts',(-8.82281304870948,22.4757955684185,
3.46287620746148));
#102363=CARTESIAN_POINT('Ctrl Pts',(-8.82253987534896,22.4750563212384,
3.47363330925202));
#102364=CARTESIAN_POINT('Ctrl Pts',(-8.82246606920406,22.4748144086654,
3.47716603026419));
#102365=CARTESIAN_POINT('Ctrl Pts',(-8.82236680724217,22.4744012329279,
3.48322222468937));
#102366=CARTESIAN_POINT('Ctrl Pts',(-8.82233356161298,22.4742295460422,
3.48574550000601));
#102367=CARTESIAN_POINT('Ctrl Pts',(-8.82227647693805,22.4738406707824,
3.4914762806554));
#102368=CARTESIAN_POINT('Ctrl Pts',(-8.82225763042966,22.4736237607589,
3.49468378844386));
#102369=CARTESIAN_POINT('Ctrl Pts',(-8.82224200968322,22.4730356617882,
3.5034086028157));
#102370=CARTESIAN_POINT('Ctrl Pts',(-8.82227090019157,22.4726658539685,
3.50892595983525));
#102371=CARTESIAN_POINT('Ctrl Pts',(-8.82260658671649,22.4708407285318,
3.53629727294185));
#102372=CARTESIAN_POINT('Ctrl Pts',(-8.82348291434856,22.4694140885965,
3.55814152245687));
#102373=CARTESIAN_POINT('Ctrl Pts',(-8.82646554322228,22.4665888039135,
3.60197732634387));
#102374=CARTESIAN_POINT('Ctrl Pts',(-8.82858343186148,22.4651911535401,
3.62395893556084));
#102375=CARTESIAN_POINT('Ctrl Pts',(-8.84364252023728,22.4575637294245,
3.74461019498027));
#102376=CARTESIAN_POINT('Ctrl Pts',(-8.86842959271848,22.451570705444,3.8413878645372));
#102377=CARTESIAN_POINT('Ctrl Pts',(-8.91524778213248,22.4434261306559,
3.95953002665625));
#102378=CARTESIAN_POINT('Ctrl Pts',(-8.92630147549828,22.441635180557,3.98479532497319));
#102379=CARTESIAN_POINT('Ctrl Pts',(-8.94188725538245,22.4392562645065,
4.01726577477724));
#102380=CARTESIAN_POINT('Ctrl Pts',(-8.94562554409381,22.438695451663,4.02484375067802));
#102381=CARTESIAN_POINT('Ctrl Pts',(-8.95188010281223,22.4377724854518,
4.03718596801832));
#102382=CARTESIAN_POINT('Ctrl Pts',(-8.95434814028535,22.4374120107708,
4.04197441798461));
#102383=CARTESIAN_POINT('Ctrl Pts',(-8.95919466099341,22.4367111802419,
4.05122122754505));
#102384=CARTESIAN_POINT('Ctrl Pts',(-8.96156916056801,22.4363709698971,
4.05568155066113));
#102385=CARTESIAN_POINT('Ctrl Pts',(-8.96713533219878,22.4355806092977,
4.06597692018125));
#102386=CARTESIAN_POINT('Ctrl Pts',(-8.97034784957455,22.4351297304064,
4.07180043908619));
#102387=CARTESIAN_POINT('Ctrl Pts',(-8.98098622415399,22.4336533737674,
4.09070486482942));
#102388=CARTESIAN_POINT('Ctrl Pts',(-8.98861311858687,22.4326207845875,
4.10367031759685));
#102389=CARTESIAN_POINT('Ctrl Pts',(-9.03897376584941,22.4259593845019,
4.18564727621822));
#102390=CARTESIAN_POINT('Ctrl Pts',(-9.08848988703125,22.4200788734109,
4.25021889189771));
#102391=CARTESIAN_POINT('Ctrl Pts',(-9.18181894980893,22.4101099413912,
4.34892088516813));
#102392=CARTESIAN_POINT('Ctrl Pts',(-9.22212393923692,22.4060800458334,
4.38600017319625));
#102393=CARTESIAN_POINT('Ctrl Pts',(-9.27747622969541,22.4010000842008,
4.43022317345313));
#102394=CARTESIAN_POINT('Ctrl Pts',(-9.29029715278954,22.3998525706572,
4.44004131549207));
#102395=CARTESIAN_POINT('Ctrl Pts',(-9.31200724324838,22.3979624104561,
4.45596925213839));
#102396=CARTESIAN_POINT('Ctrl Pts',(-9.32078543596382,22.3972120907018,
4.46222598234168));
#102397=CARTESIAN_POINT('Ctrl Pts',(-9.3330592981464,22.3961834447916,4.47072260171185));
#102398=CARTESIAN_POINT('Ctrl Pts',(-9.33648243869067,22.3958987267403,
4.47306562800808));
#102399=CARTESIAN_POINT('Ctrl Pts',(-9.34230170452359,22.3954184675781,
4.47700373552385));
#102400=CARTESIAN_POINT('Ctrl Pts',(-9.34469140782919,22.3952223113362,
4.4786081937138));
#102401=CARTESIAN_POINT('Ctrl Pts',(-9.34928838053649,22.3948470448317,
4.48167023326546));
#102402=CARTESIAN_POINT('Ctrl Pts',(-9.3514947004904,22.3946678414313,4.48312915501743));
#102403=CARTESIAN_POINT('Ctrl Pts',(-9.35679941576814,22.3942390982952,
4.48661125265021));
#102404=CARTESIAN_POINT('Ctrl Pts',(-9.35990249202658,22.3939900243667,
4.4886272991484));
#102405=CARTESIAN_POINT('Ctrl Pts',(-9.37121650887726,22.3930879398452,
4.49590233375147));
#102406=CARTESIAN_POINT('Ctrl Pts',(-9.37948345079794,22.3924403334364,
4.50107410538978));
#102407=CARTESIAN_POINT('Ctrl Pts',(-9.44008453232324,22.3877689425157,
4.53794673751422));
#102408=CARTESIAN_POINT('Ctrl Pts',(-9.49476130446408,22.3839591405728,
4.56563343118322));
#102409=CARTESIAN_POINT('Ctrl Pts',(-9.61324844901511,22.3760254775498,
4.6144506639708));
#102410=CARTESIAN_POINT('Ctrl Pts',(-9.67720627388599,22.3719166010519,
4.63462797072597));
#102411=CARTESIAN_POINT('Ctrl Pts',(-9.77641450351613,22.3654534218445,
4.65685365246097));
#102412=CARTESIAN_POINT('Ctrl Pts',(-9.81061522235923,22.3632114144455,
4.66294191221591));
#102413=CARTESIAN_POINT('Ctrl Pts',(-9.85407119560418,22.360320449151,4.66870996523399));
#102414=CARTESIAN_POINT('Ctrl Pts',(-9.86312324148109,22.3597160055256,
4.66980466062905));
#102415=CARTESIAN_POINT('Ctrl Pts',(-9.87768728091765,22.3587394961209,
4.67139458605251));
#102416=CARTESIAN_POINT('Ctrl Pts',(-9.88319176462538,22.3583695078131,
4.67195627557292));
#102417=CARTESIAN_POINT('Ctrl Pts',(-9.89368419471227,22.3576624144286,
4.67295229181495));
#102418=CARTESIAN_POINT('Ctrl Pts',(-9.89867136521094,22.3573255362428,
4.67339364058538));
#102419=CARTESIAN_POINT('Ctrl Pts',(-9.91008268752092,22.3565528383528,
4.67433021487081));
#102420=CARTESIAN_POINT('Ctrl Pts',(-9.91650834573871,22.3561163785527,
4.67480454435788));
#102421=CARTESIAN_POINT('Ctrl Pts',(-9.93642374858349,22.3547592541236,
4.67611044748734));
#102422=CARTESIAN_POINT('Ctrl Pts',(-9.94992374396886,22.3538330714803,
4.67676253616903));
#102423=CARTESIAN_POINT('Ctrl Pts',(-10.0648869280207,22.3458897644536,
4.68033380304585));
#102424=CARTESIAN_POINT('Ctrl Pts',(-10.1663054591593,22.3384550576385,
4.67035557181679));
#102425=CARTESIAN_POINT('Ctrl Pts',(-10.3216792027605,22.3267564904808,
4.63445238220202));
#102426=CARTESIAN_POINT('Ctrl Pts',(-10.3771606099677,22.3225269778226,
4.6172337234391));
#102427=CARTESIAN_POINT('Ctrl Pts',(-10.4378774894707,22.3179850082533,
4.59334833926638));
#102428=CARTESIAN_POINT('Ctrl Pts',(-10.4445781936335,22.3174850449339,
4.59064087722309));
#102429=CARTESIAN_POINT('Ctrl Pts',(-10.4545175154729,22.3167458031383,
4.58651800517167));
#102430=CARTESIAN_POINT('Ctrl Pts',(-10.457775217083,22.3165038914559,4.58514948227599));
#102431=CARTESIAN_POINT('Ctrl Pts',(-10.4633488664232,22.3160907167106,
4.58277848999989));
#102432=CARTESIAN_POINT('Ctrl Pts',(-10.4656677994781,22.3159190299324,
4.58178321829983));
#102433=CARTESIAN_POINT('Ctrl Pts',(-10.4709270063596,22.3155301542001,
4.57950595426882));
#102434=CARTESIAN_POINT('Ctrl Pts',(-10.4738652530577,22.3153132436011,
4.57821939937418));
#102435=CARTESIAN_POINT('Ctrl Pts',(-10.4818431766499,22.3147251415353,
4.57468723629766));
#102436=CARTESIAN_POINT('Ctrl Pts',(-10.4868724673683,22.3143553312203,
4.57241815829007));
#102437=CARTESIAN_POINT('Ctrl Pts',(-10.5117445920313,22.3125301734291,
4.56098550127302));
#102438=CARTESIAN_POINT('Ctrl Pts',(-10.5313470467539,22.3111035048499,
4.55130548609623));
#102439=CARTESIAN_POINT('Ctrl Pts',(-10.5701860929453,22.3082781985637,
4.53076200553939));
#102440=CARTESIAN_POINT('Ctrl Pts',(-10.5894089015904,22.306880554198,4.51989202215604));
#102441=CARTESIAN_POINT('Ctrl Pts',(-10.6935227010269,22.299253094247,4.45709099403719));
#102442=CARTESIAN_POINT('Ctrl Pts',(-10.7718699014231,22.2932600281749,
4.39510572286816));
#102443=CARTESIAN_POINT('Ctrl Pts',(-10.8607810826766,22.2851154590572,
4.30430783653869));
#102444=CARTESIAN_POINT('Ctrl Pts',(-10.8793713184431,22.2833245679962,
4.2839394502097));
#102445=CARTESIAN_POINT('Ctrl Pts',(-10.9027024312337,22.2809457194186,
4.2565016728679));
#102446=CARTESIAN_POINT('Ctrl Pts',(-10.9081065550702,22.2803849130357,
4.25000595921701));
#102447=CARTESIAN_POINT('Ctrl Pts',(-10.9168407726508,22.2794619547381,
4.23927469893849));
#102448=CARTESIAN_POINT('Ctrl Pts',(-10.9202125886999,22.2791014814536,
4.23507337922244));
#102449=CARTESIAN_POINT('Ctrl Pts',(-10.9266910506768,22.2784006516936,
4.22688671200349));
#102450=CARTESIAN_POINT('Ctrl Pts',(-10.9298011095357,22.2780604407084,
4.22290420584305));
#102451=CARTESIAN_POINT('Ctrl Pts',(-10.9369451270782,22.277270075748,4.21363374761644));
#102452=CARTESIAN_POINT('Ctrl Pts',(-10.9409600797858,22.2768191931112,
4.20833143512559));
#102453=CARTESIAN_POINT('Ctrl Pts',(-10.9539083181515,22.2753428114237,
4.19092708919635));
#102454=CARTESIAN_POINT('Ctrl Pts',(-10.9626543923604,22.2743102006057,
4.17868829843754));
#102455=CARTESIAN_POINT('Ctrl Pts',(-11.0170827983842,22.267648847812,4.09935467149147));
#102456=CARTESIAN_POINT('Ctrl Pts',(-11.0559518974809,22.2617684135024,
4.02786787465041));
#102457=CARTESIAN_POINT('Ctrl Pts',(-11.1081962309625,22.251799525032,3.90247740819524));
#102458=CARTESIAN_POINT('Ctrl Pts',(-11.125691408251,22.2477695946559,3.85058005713566));
#102459=CARTESIAN_POINT('Ctrl Pts',(-11.1435971408276,22.2426895940734,
3.7820307305509));
#102460=CARTESIAN_POINT('Ctrl Pts',(-11.1473562455867,22.2415420751095,
3.76632584231397));
#102461=CARTESIAN_POINT('Ctrl Pts',(-11.1530844231083,22.2396519069557,
3.74001574606053));
#102462=CARTESIAN_POINT('Ctrl Pts',(-11.1552328557163,22.2389015845913,
3.72945220626803));
#102463=CARTESIAN_POINT('Ctrl Pts',(-11.158006889313,22.2378729357296,3.71478434210418));
#102464=CARTESIAN_POINT('Ctrl Pts',(-11.1587562048868,22.2375882172899,
3.71070436222177));
#102465=CARTESIAN_POINT('Ctrl Pts',(-11.1599889217081,22.2371079576655,
3.70378677243828));
#102466=CARTESIAN_POINT('Ctrl Pts',(-11.160483500761,22.2369118013473,3.70095121856903));
#102467=CARTESIAN_POINT('Ctrl Pts',(-11.1614126174234,22.2365365348493,
3.69550649776286));
#102468=CARTESIAN_POINT('Ctrl Pts',(-11.1618487656391,22.2363573315308,
3.69289765346815));
#102469=CARTESIAN_POINT('Ctrl Pts',(-11.1628739931369,22.2359285887898,
3.68663555787491));
#102470=CARTESIAN_POINT('Ctrl Pts',(-11.1634546559265,22.2356795151727,
3.68298092770368));
#102471=CARTESIAN_POINT('Ctrl Pts',(-11.1655027123365,22.2347774334213,
3.66968666387292));
#102472=CARTESIAN_POINT('Ctrl Pts',(-11.1668676573237,22.2341298294264,
3.66003131533279));
#102473=CARTESIAN_POINT('Ctrl Pts',(-11.1759244496307,22.2294582006022,
3.5896710404321));
#102474=CARTESIAN_POINT('Ctrl Pts',(-11.1789959182013,22.2256481846331,
3.52845733912431));
#102475=CARTESIAN_POINT('Ctrl Pts',(-11.1754351561762,22.2177144705944,
3.4003562508788));
#102476=CARTESIAN_POINT('Ctrl Pts',(-11.1678730882563,22.2136057509646,
3.33372158964951));
#102477=CARTESIAN_POINT('Ctrl Pts',(-11.147854678902,22.20714278727,3.23404806842098));
#102478=CARTESIAN_POINT('Ctrl Pts',(-11.139515708418,22.204900828335,3.20032620765442));
#102479=CARTESIAN_POINT('Ctrl Pts',(-11.1271222322066,22.202009917753,3.15827837162324));
#102480=CARTESIAN_POINT('Ctrl Pts',(-11.1244430034573,22.2014054782605,
3.14956295590559));
#102481=CARTESIAN_POINT('Ctrl Pts',(-11.1199757669009,22.2004289739334,
3.13561015535049));
#102482=CARTESIAN_POINT('Ctrl Pts',(-11.1182515319567,22.2000589865309,
3.13035261825761));
#102483=CARTESIAN_POINT('Ctrl Pts',(-11.1148966498186,22.199351893824,3.1203612380389));
#102484=CARTESIAN_POINT('Ctrl Pts',(-11.1132727335552,22.199015015403,3.11562524959459));
#102485=CARTESIAN_POINT('Ctrl Pts',(-11.1094900218632,22.1982423154793,
3.10481843620123));
#102486=CARTESIAN_POINT('Ctrl Pts',(-11.1073115218441,22.1978058538687,
3.09875472874456));
#102487=CARTESIAN_POINT('Ctrl Pts',(-11.1004095095312,22.1964487181342,
3.08002781103546));
#102488=CARTESIAN_POINT('Ctrl Pts',(-11.0955178379286,22.1955225258633,
3.06742819270565));
#102489=CARTESIAN_POINT('Ctrl Pts',(-11.0520514506142,22.1875792821989,
2.96093996121632));
#102490=CARTESIAN_POINT('Ctrl Pts',(-11.0017112746471,22.1801446587205,
2.87233450560586));
#102491=CARTESIAN_POINT('Ctrl Pts',(-10.9057528400591,22.1684461080741,
2.74496913577792));
#102492=CARTESIAN_POINT('Ctrl Pts',(-10.8674685214916,22.1642165322775,
2.70127615598767));
#102493=CARTESIAN_POINT('Ctrl Pts',(-10.8209648769333,22.1596745030138,
2.65550964603116));
#102494=CARTESIAN_POINT('Ctrl Pts',(-10.8157674885821,22.1591745380301,
2.65048796462936));
#102495=CARTESIAN_POINT('Ctrl Pts',(-10.8079604742552,22.1584352942642,
2.64308260636843));
#102496=CARTESIAN_POINT('Ctrl Pts',(-10.8053859303956,22.158193382256,2.6406624345386));
#102497=CARTESIAN_POINT('Ctrl Pts',(-10.8009540939124,22.1577802071477,
2.63653374711593));
#102498=CARTESIAN_POINT('Ctrl Pts',(-10.7991021641032,22.1576085203302,
2.63481957824148));
#102499=CARTESIAN_POINT('Ctrl Pts',(-10.7948837821957,22.1572196447708,
2.6309400921671));
#102500=CARTESIAN_POINT('Ctrl Pts',(-10.7925139854522,22.1570027343824,
2.62877848162224));
#102501=CARTESIAN_POINT('Ctrl Pts',(-10.7860439712692,22.1564146334494,
2.62292510136028));
#102502=CARTESIAN_POINT('Ctrl Pts',(-10.7819265321687,22.1560448240476,
2.61925236086059));
#102503=CARTESIAN_POINT('Ctrl Pts',(-10.7613711949434,22.1542196780974,
2.60117484588003));
#102504=CARTESIAN_POINT('Ctrl Pts',(-10.7445591625958,22.1527930200011,
2.58719960814795));
#102505=CARTESIAN_POINT('Ctrl Pts',(-10.7100023957452,22.1499677216212,
2.56006431494759));
#102506=CARTESIAN_POINT('Ctrl Pts',(-10.6922573015275,22.1485700750568,
2.54691951023992));
#102507=CARTESIAN_POINT('Ctrl Pts',(-10.5925589793672,22.1409426282226,
2.47732179414901));
#102508=CARTESIAN_POINT('Ctrl Pts',(-10.5040795022807,22.1349495775568,
2.43093442470316));
#102509=CARTESIAN_POINT('Ctrl Pts',(-10.384980745302,22.1268050063642,2.38660653282203));
#102510=CARTESIAN_POINT('Ctrl Pts',(-10.3588141458205,22.1250140936948,
2.37790044789053));
#102511=CARTESIAN_POINT('Ctrl Pts',(-10.3242614242211,22.1226352204215,
2.36773634263888));
#102512=CARTESIAN_POINT('Ctrl Pts',(-10.3161298633127,22.1220744116739,
2.36543913148922));
#102513=CARTESIAN_POINT('Ctrl Pts',(-10.3027748378282,22.1211514504798,
2.36182098044806));
#102514=CARTESIAN_POINT('Ctrl Pts',(-10.297565686207,22.1207909766841,2.36044800745204));
#102515=CARTESIAN_POINT('Ctrl Pts',(-10.2874525042433,22.1200901466426,
2.35785655311483));
#102516=CARTESIAN_POINT('Ctrl Pts',(-10.2825496826949,22.1197499358918,
2.35663379842887));
#102517=CARTESIAN_POINT('Ctrl Pts',(-10.2711757775239,22.1189595725276,
2.35387479117138));
#102518=CARTESIAN_POINT('Ctrl Pts',(-10.2646992988388,22.1185086912616,
2.35236174050038));
#102519=CARTESIAN_POINT('Ctrl Pts',(-10.2435346084948,22.1170323187422,
2.34760587771566));
#102520=CARTESIAN_POINT('Ctrl Pts',(-10.2287975443728,22.1159997158441,
2.34458969805409));
#102521=CARTESIAN_POINT('Ctrl Pts',(-10.1341854029018,22.1093380645483,
2.3271068079901));
#102522=CARTESIAN_POINT('Ctrl Pts',(-10.0530668290272,22.1034572933146,
2.32065122416567));
#102523=CARTESIAN_POINT('Ctrl Pts',(-9.91805451334948,22.0935462558775,
2.32386829630545));
#102524=CARTESIAN_POINT('Ctrl Pts',(-9.86431471500832,22.089575070732,2.32885069407818));
#102525=CARTESIAN_POINT('Ctrl Pts',(-9.81110406355273,22.0857064764352,
2.33749693002826));
#102526=CARTESIAN_POINT('Ctrl Pts',(-9.8111040696154,21.9876672748127,2.33749692904314));
#102527=CARTESIAN_POINT('Ctrl Pts',(-9.87819815585959,21.9926487009463,
2.32659476442867));
#102528=CARTESIAN_POINT('Ctrl Pts',(-9.94610318052165,21.9976751846187,
2.32152147714435));
#102529=CARTESIAN_POINT('Ctrl Pts',(-10.0297196451487,22.00362504353,2.32252114418055));
#102530=CARTESIAN_POINT('Ctrl Pts',(-10.0453554859209,22.0047268891869,
2.32301969032066));
#102531=CARTESIAN_POINT('Ctrl Pts',(-10.0657045114906,22.0061430931441,
2.32407466935722));
#102532=CARTESIAN_POINT('Ctrl Pts',(-10.0704299822049,22.0064707135964,
2.32434822948283));
#102533=CARTESIAN_POINT('Ctrl Pts',(-10.0792908738116,22.0070825405063,
2.32491480928958));
#102534=CARTESIAN_POINT('Ctrl Pts',(-10.0834266303263,22.0073670813893,
2.32520118881562));
#102535=CARTESIAN_POINT('Ctrl Pts',(-10.0904299953181,22.0078470813904,
2.32572330513678));
#102536=CARTESIAN_POINT('Ctrl Pts',(-10.0932983845497,22.008043154678,2.32594772166279));
#102537=CARTESIAN_POINT('Ctrl Pts',(-10.0988014649904,22.0084182906247,
2.32639856621338));
#102538=CARTESIAN_POINT('Ctrl Pts',(-10.1014362429372,22.0085974461927,
2.32662335806366));
#102539=CARTESIAN_POINT('Ctrl Pts',(-10.1077556991021,22.009026108058,2.3271839611209));
#102540=CARTESIAN_POINT('Ctrl Pts',(-10.1114396246146,22.0092751485481,
2.32752826783353));
#102541=CARTESIAN_POINT('Ctrl Pts',(-10.1248284910324,22.0101773777237,
2.32884329119695));
#102542=CARTESIAN_POINT('Ctrl Pts',(-10.1345232268833,22.0108251585374,
2.32991722283237));
#102543=CARTESIAN_POINT('Ctrl Pts',(-10.2036744343364,22.0154134420393,
2.33844829569929));
#102544=CARTESIAN_POINT('Ctrl Pts',(-10.2625065764362,22.0191489360262,
2.3503140327401));
#102545=CARTESIAN_POINT('Ctrl Pts',(-10.3641372597904,22.0256893678699,
2.37902499041741));
#102546=CARTESIAN_POINT('Ctrl Pts',(-10.4073284980213,22.0284982663367,
2.39398719840255));
#102547=CARTESIAN_POINT('Ctrl Pts',(-10.4986206969682,22.034668816066,2.4316872714663));
#102548=CARTESIAN_POINT('Ctrl Pts',(-10.5462678604914,22.0380401343023,
2.45524881100488));
#102549=CARTESIAN_POINT('Ctrl Pts',(-10.6017886737427,22.04225582356,2.4875428173464));
#102550=CARTESIAN_POINT('Ctrl Pts',(-10.6113376715883,22.0429915644591,
2.49327988400616));
#102551=CARTESIAN_POINT('Ctrl Pts',(-10.626009712147,22.0441394877179,2.50238061645066));
#102552=CARTESIAN_POINT('Ctrl Pts',(-10.6311904698151,22.0445482590806,
2.50565037207584));
#102553=CARTESIAN_POINT('Ctrl Pts',(-10.6405315712947,22.0452916676645,
2.5116482823902));
#102554=CARTESIAN_POINT('Ctrl Pts',(-10.6447006135056,22.0456257922874,
2.51436267868494));
#102555=CARTESIAN_POINT('Ctrl Pts',(-10.6536345911874,22.0463469084196,
2.52026038105914));
#102556=CARTESIAN_POINT('Ctrl Pts',(-10.6583937240264,22.0467342110984,
2.52345220195346));
#102557=CARTESIAN_POINT('Ctrl Pts',(-10.671201771032,22.0477852557383,2.5321783956718));
#102558=CARTESIAN_POINT('Ctrl Pts',(-10.6792052866337,22.0484514461455,
2.53777827719809));
#102559=CARTESIAN_POINT('Ctrl Pts',(-10.7195987911834,22.0518628586171,
2.56679578148276));
#102560=CARTESIAN_POINT('Ctrl Pts',(-10.7508478065048,22.0546664204829,
2.59174923253043));
#102561=CARTESIAN_POINT('Ctrl Pts',(-10.8527462201602,22.0643928472976,
2.68197645400811));
#102562=CARTESIAN_POINT('Ctrl Pts',(-10.9166419077113,22.0715637869243,
2.75427696612489));
#102563=CARTESIAN_POINT('Ctrl Pts',(-10.9887476401344,22.0807726416558,
2.85933425571479));
#102564=CARTESIAN_POINT('Ctrl Pts',(-11.0054237510702,22.0830033183512,
2.88583555632829));
#102565=CARTESIAN_POINT('Ctrl Pts',(-11.0239520512199,22.0855824663701,
2.91806209146585));
#102566=CARTESIAN_POINT('Ctrl Pts',(-11.0268403802859,22.0859877026338,
2.92317388271512));
#102567=CARTESIAN_POINT('Ctrl Pts',(-11.0313173133216,22.0866206321607,
2.93123740048873));
#102568=CARTESIAN_POINT('Ctrl Pts',(-11.0329317010754,22.0868498784648,
2.93417458789679));
#102569=CARTESIAN_POINT('Ctrl Pts',(-11.0358658954976,22.0872683514378,
2.93956741660968));
#102570=CARTESIAN_POINT('Ctrl Pts',(-11.0371895229283,22.0874578102384,
2.94202085356191));
#102571=CARTESIAN_POINT('Ctrl Pts',(-11.0401496061393,22.0878830685177,
2.94755450564967));
#102572=CARTESIAN_POINT('Ctrl Pts',(-11.0417810969789,22.0881185570915,
2.95063730182402));
#102573=CARTESIAN_POINT('Ctrl Pts',(-11.0459415238944,22.0887220465344,
2.95858385534162));
#102574=CARTESIAN_POINT('Ctrl Pts',(-11.0484502753889,22.0890888349177,
2.96345816937408));
#102575=CARTESIAN_POINT('Ctrl Pts',(-11.0640833448657,22.0913940325237,
2.99436041902814));
#102576=CARTESIAN_POINT('Ctrl Pts',(-11.0762728323061,22.0932803930998,
3.02085298167945));
#102577=CARTESIAN_POINT('Ctrl Pts',(-11.1252789594728,22.1014009318217,
3.13869773644542));
#102578=CARTESIAN_POINT('Ctrl Pts',(-11.1515394416143,22.107306956937,3.23400843240098));
#102579=CARTESIAN_POINT('Ctrl Pts',(-11.1714099394503,22.1160854191793,
3.37145117272148));
#102580=CARTESIAN_POINT('Ctrl Pts',(-11.1751282813674,22.1186810026192,
3.41168791042498));
#102581=CARTESIAN_POINT('Ctrl Pts',(-11.1771612229977,22.1219698142552,
3.46156212338712));
#102582=CARTESIAN_POINT('Ctrl Pts',(-11.1774338716598,22.1226015970142,
3.47109525427539));
#102583=CARTESIAN_POINT('Ctrl Pts',(-11.1776831979547,22.1236116194228,
3.48625326532252));
#102584=CARTESIAN_POINT('Ctrl Pts',(-11.1777354101229,22.1239875141372,
3.49187661778551));
#102585=CARTESIAN_POINT('Ctrl Pts',(-11.1777579330679,22.12469914187,3.50248735174402));
#102586=CARTESIAN_POINT('Ctrl Pts',(-11.1777368402003,22.1250346004664,
3.50747460639836));
#102587=CARTESIAN_POINT('Ctrl Pts',(-11.1776176162082,22.1257947622752,
3.51874195529776));
#102588=CARTESIAN_POINT('Ctrl Pts',(-11.177500923489,22.1262200319672,3.52502165902602));
#102589=CARTESIAN_POINT('Ctrl Pts',(-11.1770712985442,22.1273186830036,
3.54118177586455));
#102590=CARTESIAN_POINT('Ctrl Pts',(-11.1766841937867,22.1279943379136,
3.55105955574499));
#102591=CARTESIAN_POINT('Ctrl Pts',(-11.1726344980923,22.1333752858914,
3.6292322286402));
#102592=CARTESIAN_POINT('Ctrl Pts',(-11.1631542810495,22.1382619715537,
3.69708313900837));
#102593=CARTESIAN_POINT('Ctrl Pts',(-11.1322712700033,22.1483228748747,
3.83150288229873));
#102594=CARTESIAN_POINT('Ctrl Pts',(-11.1107240715515,22.1534802595565,
3.89777451699018));
#102595=CARTESIAN_POINT('Ctrl Pts',(-11.0724600960666,22.160508964899,3.98755598380316));
#102596=CARTESIAN_POINT('Ctrl Pts',(-11.0605461906433,22.1625009499129,
4.01295571691674));
#102597=CARTESIAN_POINT('Ctrl Pts',(-11.0451105398646,22.1648435047048,
4.04302123169852));
#102598=CARTESIAN_POINT('Ctrl Pts',(-11.0424479555176,22.1652398562807,
4.04811528169876));
#102599=CARTESIAN_POINT('Ctrl Pts',(-11.0382332184573,22.1658551284276,
4.05603709300212));
#102600=CARTESIAN_POINT('Ctrl Pts',(-11.0367066066577,22.1660755718294,
4.05887823096716));
#102601=CARTESIAN_POINT('Ctrl Pts',(-11.0338326788969,22.1664860438734,
4.06417452714636));
#102602=CARTESIAN_POINT('Ctrl Pts',(-11.0324882879326,22.1666762401404,
4.0666311327001));
#102603=CARTESIAN_POINT('Ctrl Pts',(-11.0293968325784,22.1671095033239,
4.07223261461879));
#102604=CARTESIAN_POINT('Ctrl Pts',(-11.0276441111894,22.1673522097884,
4.0753743005698));
#102605=CARTESIAN_POINT('Ctrl Pts',(-11.0229414022039,22.1679958006365,
4.08371368619543));
#102606=CARTESIAN_POINT('Ctrl Pts',(-11.019966154278,22.1683951495066,4.08889712820039));
#102607=CARTESIAN_POINT('Ctrl Pts',(-10.9958700737207,22.1715695117732,
4.13014655554927));
#102608=CARTESIAN_POINT('Ctrl Pts',(-10.9728799150741,22.1742368813648,
4.16509202016769));
#102609=CARTESIAN_POINT('Ctrl Pts',(-10.8894099110891,22.1830652620182,
4.27834659497096));
#102610=CARTESIAN_POINT('Ctrl Pts',(-10.8209534468426,22.1890210331115,
4.35024078738506));
#102611=CARTESIAN_POINT('Ctrl Pts',(-10.7223325159853,22.1971690141051,
4.43066401105529));
#102612=CARTESIAN_POINT('Ctrl Pts',(-10.6997094050158,22.1990104191988,
4.44779022300222));
#102613=CARTESIAN_POINT('Ctrl Pts',(-10.6695079570304,22.2014468301798,
4.4689824256468));
#102614=CARTESIAN_POINT('Ctrl Pts',(-10.6624715201355,22.2020129663741,
4.47380661549748));
#102615=CARTESIAN_POINT('Ctrl Pts',(-10.6508937936291,22.2029423739758,
4.48156076251719));
#102616=CARTESIAN_POINT('Ctrl Pts',(-10.6463835665918,22.2033039192836,
4.48453671555779));
#102617=CARTESIAN_POINT('Ctrl Pts',(-10.6376240831623,22.2040051846983,
4.49023029213341));
#102618=CARTESIAN_POINT('Ctrl Pts',(-10.633377526254,22.2043447486263,4.49295186729208));
#102619=CARTESIAN_POINT('Ctrl Pts',(-10.6235315483333,22.2051311940205,
4.49917319402068));
#102620=CARTESIAN_POINT('Ctrl Pts',(-10.6179199592271,22.2055787829027,
4.50265327223217));
#102621=CARTESIAN_POINT('Ctrl Pts',(-10.5996551740386,22.2070337597525,
4.51376877773323));
#102622=CARTESIAN_POINT('Ctrl Pts',(-10.5868878861677,22.2080479780482,
4.521213022314));
#102623=CARTESIAN_POINT('Ctrl Pts',(-10.4972929581787,22.2151490589301,
4.57121822607051));
#102624=CARTESIAN_POINT('Ctrl Pts',(-10.4160683329059,22.2215359757464,
4.60530098705531));
#102625=CARTESIAN_POINT('Ctrl Pts',(-10.2648545038587,22.2331084453963,
4.64970413056364));
#102626=CARTESIAN_POINT('Ctrl Pts',(-10.1962561672777,22.2382401029016,
4.66338006127205));
#102627=CARTESIAN_POINT('Ctrl Pts',(-10.1196963622983,22.2436002962789,
4.67167381637525));
#102628=CARTESIAN_POINT('Ctrl Pts',(-10.1125415343706,22.2440976516662,
4.67238268523291));
#102629=CARTESIAN_POINT('Ctrl Pts',(-10.1018692408524,22.2448337560238,
4.67334144574814));
#102630=CARTESIAN_POINT('Ctrl Pts',(-10.0983565815229,22.2450751073661,
4.67364111815887));
#102631=CARTESIAN_POINT('Ctrl Pts',(-10.0923289282043,22.2454876089015,
4.67412809827691));
#102632=CARTESIAN_POINT('Ctrl Pts',(-10.0898146275256,22.2456591793799,
4.67432310514116));
#102633=CARTESIAN_POINT('Ctrl Pts',(-10.084097475031,22.2460481710457,4.67474805287377));
#102634=CARTESIAN_POINT('Ctrl Pts',(-10.0808942975097,22.2462653117054,
4.67497297257901));
#102635=CARTESIAN_POINT('Ctrl Pts',(-10.072166906762,22.2468548490445,4.67554993091432));
#102636=CARTESIAN_POINT('Ctrl Pts',(-10.0666409811312,22.2472258526874,
4.67587613511491));
#102637=CARTESIAN_POINT('Ctrl Pts',(-10.0390549149078,22.2490675228593,
4.67730949252029));
#102638=CARTESIAN_POINT('Ctrl Pts',(-10.0169673805789,22.2505088823298,
4.67783495775458));
#102639=CARTESIAN_POINT('Ctrl Pts',(-9.88946870907654,22.2587044625537,
4.67728029977967));
#102640=CARTESIAN_POINT('Ctrl Pts',(-9.7845925480739,22.264994905042,4.66267366183043));
#102641=CARTESIAN_POINT('Ctrl Pts',(-9.64330073198281,22.2742607490217,
4.62319378677043));
#102642=CARTESIAN_POINT('Ctrl Pts',(-9.6041642032603,22.2769115890524,4.61000544851472));
#102643=CARTESIAN_POINT('Ctrl Pts',(-9.55688348055992,22.2802624258923,
4.59125381733467));
#102644=CARTESIAN_POINT('Ctrl Pts',(-9.54800729939772,22.2808980551269,
4.58760734332668));
#102645=CARTESIAN_POINT('Ctrl Pts',(-9.5339897647633,22.2819128038305,4.58164749024288));
#102646=CARTESIAN_POINT('Ctrl Pts',(-9.52881862772023,22.2822895397315,
4.57940490319199));
#102647=CARTESIAN_POINT('Ctrl Pts',(-9.51910439997351,22.2830018712729,
4.5751089891964));
#102648=CARTESIAN_POINT('Ctrl Pts',(-9.51455784723318,22.2833371860097,
4.57306375941842));
#102649=CARTESIAN_POINT('Ctrl Pts',(-9.50433138319463,22.2840958210331,
4.56838517396512));
#102650=CARTESIAN_POINT('Ctrl Pts',(-9.49865924618378,22.2845196985873,
4.56573528775604));
#102651=CARTESIAN_POINT('Ctrl Pts',(-9.48414646467492,22.2856123594336,
4.55881376738984));
#102652=CARTESIAN_POINT('Ctrl Pts',(-9.47533777135234,22.2862833748265,
4.5544766472432));
#102653=CARTESIAN_POINT('Ctrl Pts',(-9.41127134674679,22.2912223968423,
4.52193089179353));
#102654=CARTESIAN_POINT('Ctrl Pts',(-9.35827411487587,22.2956380339668,
4.4895098733112));
#102655=CARTESIAN_POINT('Ctrl Pts',(-9.24684884324462,22.3056486156696,
4.40861671049233));
#102656=CARTESIAN_POINT('Ctrl Pts',(-9.19004305398253,22.3112703110453,
4.3583650252624));
#102657=CARTESIAN_POINT('Ctrl Pts',(-9.11910618930527,22.3187658104108,
4.28225708113894));
#102658=CARTESIAN_POINT('Ctrl Pts',(-9.10051586444404,22.3207818004421,
4.26080788694628));
#102659=CARTESIAN_POINT('Ctrl Pts',(-9.07910038322968,22.3231485600952,
4.23421536687438));
#102660=CARTESIAN_POINT('Ctrl Pts',(-9.07551678478683,22.3235461902141,
4.2296979493774));
#102661=CARTESIAN_POINT('Ctrl Pts',(-9.06997814901695,22.3241630059763,
4.22260974741094));
#102662=CARTESIAN_POINT('Ctrl Pts',(-9.06800032426337,22.3243837265553,
4.22005700845329));
#102663=CARTESIAN_POINT('Ctrl Pts',(-9.06432732872563,22.3247944338049,
4.21527585840877));
#102664=CARTESIAN_POINT('Ctrl Pts',(-9.06262961694608,22.3249845901798,
4.21304955409555));
#102665=CARTESIAN_POINT('Ctrl Pts',(-9.05877223844409,22.325417411436,4.20795357316349));
#102666=CARTESIAN_POINT('Ctrl Pts',(-9.05661774594752,22.3256597186396,
4.2050800553665));
#102667=CARTESIAN_POINT('Ctrl Pts',(-9.05092545067806,22.3263015403717,
4.19741525190562));
#102668=CARTESIAN_POINT('Ctrl Pts',(-9.04741073412138,22.326699532731,4.19260683503569));
#102669=CARTESIAN_POINT('Ctrl Pts',(-9.01985583148657,22.3298351551966,
4.15430293275221));
#102670=CARTESIAN_POINT('Ctrl Pts',(-8.99755020494375,22.3324680383166,
4.11958868418623));
#102671=CARTESIAN_POINT('Ctrl Pts',(-8.92850905273416,22.3412130264482,
3.99861413492556));
#102672=CARTESIAN_POINT('Ctrl Pts',(-8.89073396578147,22.34711846511,3.90772344497099));
#102673=CARTESIAN_POINT('Ctrl Pts',(-8.85679760744793,22.3552778360896,
3.7847053408878));
#102674=CARTESIAN_POINT('Ctrl Pts',(-8.85001288766764,22.3571946755338,
3.75592626053806));
#102675=CARTESIAN_POINT('Ctrl Pts',(-8.84265125391466,22.3597170408715,
3.7184348657173));
#102676=CARTESIAN_POINT('Ctrl Pts',(-8.84107795065384,22.3602910276958,
3.70992757688324));
#102677=CARTESIAN_POINT('Ctrl Pts',(-8.83867001929862,22.3612300615691,
3.69605412718506));
#102678=CARTESIAN_POINT('Ctrl Pts',(-8.83777850998507,22.3615933124716,
3.69069806325441));
#102679=CARTESIAN_POINT('Ctrl Pts',(-8.83613188361129,22.3622956058562,
3.68036466643513));
#102680=CARTESIAN_POINT('Ctrl Pts',(-8.83537157930525,22.362634477094,3.6753882709818));
#102681=CARTESIAN_POINT('Ctrl Pts',(-8.83369670316043,22.3634160242503,
3.66393436495275));
#102682=CARTESIAN_POINT('Ctrl Pts',(-8.83280415631846,22.363859379701,3.65745385267506));
#102683=CARTESIAN_POINT('Ctrl Pts',(-8.83018421592774,22.3652499822013,
3.63718324080177));
#102684=CARTESIAN_POINT('Ctrl Pts',(-8.82864694847033,22.3662031046965,
3.62337021566095));
#102685=CARTESIAN_POINT('Ctrl Pts',(-8.8183640135199,22.3738462357418,3.51328323041129));
#102686=CARTESIAN_POINT('Ctrl Pts',(-8.82125974652214,22.3809095118362,
3.41630972939003));
#102687=CARTESIAN_POINT('Ctrl Pts',(-8.84264457109023,22.3912267462604,
3.27739654090259));
#102688=CARTESIAN_POINT('Ctrl Pts',(-8.85175001851315,22.3944414350054,
3.23439434465437));
#102689=CARTESIAN_POINT('Ctrl Pts',(-8.86695993121961,22.398596404737,3.17825796113221));
#102690=CARTESIAN_POINT('Ctrl Pts',(-8.87093200633344,22.3996049338589,
3.16458497021061));
#102691=CARTESIAN_POINT('Ctrl Pts',(-8.87805783415036,22.4012893910498,
3.14161885600952));
#102692=CARTESIAN_POINT('Ctrl Pts',(-8.88108148860042,22.4019711203979,
3.13228727443923));
#102693=CARTESIAN_POINT('Ctrl Pts',(-8.88550042505872,22.4029217137968,
3.11920908282922));
#102694=CARTESIAN_POINT('Ctrl Pts',(-8.88679863271106,22.4031957912578,
3.11543044557834));
#102695=CARTESIAN_POINT('Ctrl Pts',(-8.88905557216204,22.4036634280102,
3.10896846769012));
#102696=CARTESIAN_POINT('Ctrl Pts',(-8.89000485197604,22.4038575290419,
3.10628188626637));
#102697=CARTESIAN_POINT('Ctrl Pts',(-8.89186651707134,22.4042331822237,
3.10107339215072));
#102698=CARTESIAN_POINT('Ctrl Pts',(-8.89277777120447,22.4044148020431,
3.09855113542854));
#102699=CARTESIAN_POINT('Ctrl Pts',(-8.89528419671721,22.4049083189378,
3.09168706619551));
#102700=CARTESIAN_POINT('Ctrl Pts',(-8.89689636493688,22.405219231528,3.08735144489524));
#102701=CARTESIAN_POINT('Ctrl Pts',(-8.90318530934593,22.4064078314259,
3.0707387853088));
#102702=CARTESIAN_POINT('Ctrl Pts',(-8.90804204615833,22.4072756124512,
3.05853027428557));
#102703=CARTESIAN_POINT('Ctrl Pts',(-8.94394057383233,22.41336652772,2.9725107534463));
#102704=CARTESIAN_POINT('Ctrl Pts',(-8.9822382188358,22.4182504608339,2.90194420114871));
#102705=CARTESIAN_POINT('Ctrl Pts',(-9.06913293459486,22.4277886920449,
2.77470281899041));
#102706=CARTESIAN_POINT('Ctrl Pts',(-9.11651815016022,22.4324132483565,
2.71767835181147));
#102707=CARTESIAN_POINT('Ctrl Pts',(-9.17711537741943,22.4380252383403,
2.6573320613409));
#102708=CARTESIAN_POINT('Ctrl Pts',(-9.18541517538,22.4387877941195,2.64930622140219));
#102709=CARTESIAN_POINT('Ctrl Pts',(-9.19824309327323,22.4399580432492,
2.63726159990147));
#102710=CARTESIAN_POINT('Ctrl Pts',(-9.20268659102756,22.4403619255146,
2.63315341031463));
#102711=CARTESIAN_POINT('Ctrl Pts',(-9.21048138048688,22.4410679653809,
2.62605745744712));
#102712=CARTESIAN_POINT('Ctrl Pts',(-9.21381849180469,22.4413694665255,
2.62305424714222));
#102713=CARTESIAN_POINT('Ctrl Pts',(-9.22136893488262,22.4420499645926,
2.61633701413857));
#102714=CARTESIAN_POINT('Ctrl Pts',(-9.22559180334325,22.4424294043394,
2.61263392491907));
#102715=CARTESIAN_POINT('Ctrl Pts',(-9.23703176328023,22.4434543471603,
2.60274592765321));
#102716=CARTESIAN_POINT('Ctrl Pts',(-9.24429737593586,22.4441021511866,
2.59661805677827));
#102717=CARTESIAN_POINT('Ctrl Pts',(-9.27856563252399,22.4471437077546,
2.56841866178803));
#102718=CARTESIAN_POINT('Ctrl Pts',(-9.30646339627353,22.4495811603724,
2.54746764940007));
#102719=CARTESIAN_POINT('Ctrl Pts',(-9.40999842638136,22.4584982259682,
2.47667534578905));
#102720=CARTESIAN_POINT('Ctrl Pts',(-9.4903902305523,22.4652167075591,2.43435964630283));
#102721=CARTESIAN_POINT('Ctrl Pts',(-9.61082865842582,22.4746275634346,
2.38773574905088));
#102722=CARTESIAN_POINT('Ctrl Pts',(-9.6475061800053,22.4774088148649,2.3755735609717));
#102723=CARTESIAN_POINT('Ctrl Pts',(-9.69304183976916,22.4807105504651,
2.36292200037025));
#102724=CARTESIAN_POINT('Ctrl Pts',(-9.70139073836647,22.4813097909009,
2.36070100095704));
#102725=CARTESIAN_POINT('Ctrl Pts',(-9.71344346741404,22.4821653503904,
2.35763629569006));
#102726=CARTESIAN_POINT('Ctrl Pts',(-9.71712788269938,22.4824256132387,
2.35671838746412));
#102727=CARTESIAN_POINT('Ctrl Pts',(-9.72355404630266,22.4828772566101,
2.35515038710305));
#102728=CARTESIAN_POINT('Ctrl Pts',(-9.72629377945689,22.4830690842414,
2.35449229291434));
#102729=CARTESIAN_POINT('Ctrl Pts',(-9.73209828245168,22.4834739386758,
2.3531200436102));
#102730=CARTESIAN_POINT('Ctrl Pts',(-9.7351635684767,22.4836868271169,2.35240833492023));
#102731=CARTESIAN_POINT('Ctrl Pts',(-9.74348659928192,22.4842624983586,
2.35051098893096));
#102732=CARTESIAN_POINT('Ctrl Pts',(-9.74874976963892,22.4846239652978,
2.34934912513089));
#102733=CARTESIAN_POINT('Ctrl Pts',(-9.77295624102721,22.4862754463977,
2.34417947057636));
#102734=CARTESIAN_POINT('Ctrl Pts',(-9.79198976176031,22.487543193226,2.34060282628503));
#102735=CARTESIAN_POINT('Ctrl Pts',(-9.81110406371156,22.4887934941609,
2.33749693000246));
#102736=CARTESIAN_POINT('Origin',(-10.,12.3756328852638,3.5));
#102737=CARTESIAN_POINT('',(-9.81110406371069,23.0867835801461,2.3374969300026));
#102738=CARTESIAN_POINT('',(-9.81110406371074,22.9869701371802,2.33749693000259));
#102739=CARTESIAN_POINT('',(-9.81110406371068,12.3756328852638,2.3374969300026));
#102740=CARTESIAN_POINT('Ctrl Pts',(-9.8111040637107,23.0867835801461,2.3374969300026));
#102741=CARTESIAN_POINT('Ctrl Pts',(-9.751178490704,23.0830160202839,2.347234278241));
#102742=CARTESIAN_POINT('Ctrl Pts',(-9.69207037239346,23.079201471488,2.36159457127933));
#102743=CARTESIAN_POINT('Ctrl Pts',(-9.62000848223303,23.0742571631329,
2.38513328343377));
#102744=CARTESIAN_POINT('Ctrl Pts',(-9.60580053016976,23.0732679368808,
2.39007743795704));
#102745=CARTESIAN_POINT('Ctrl Pts',(-9.585453107092,23.0718285213703,2.39759799862038));
#102746=CARTESIAN_POINT('Ctrl Pts',(-9.57923429217758,23.0713854916472,
2.39995658488689));
#102747=CARTESIAN_POINT('Ctrl Pts',(-9.56832658723452,23.070602795237,2.40419953436903));
#102748=CARTESIAN_POINT('Ctrl Pts',(-9.56362918267486,23.0702638746225,
2.40606165430127));
#102749=CARTESIAN_POINT('Ctrl Pts',(-9.55394898344562,23.0695615340065,
2.40997129725149));
#102750=CARTESIAN_POINT('Ctrl Pts',(-9.54896797150063,23.0691979842158,
2.4120228909651));
#102751=CARTESIAN_POINT('Ctrl Pts',(-9.53621086116104,23.0682612326462,
2.41737998813079));
#102752=CARTESIAN_POINT('Ctrl Pts',(-9.52845605483273,23.0676863731341,
2.42073508502336));
#102753=CARTESIAN_POINT('Ctrl Pts',(-9.49555648831778,23.065223823561,2.43539126066882));
#102754=CARTESIAN_POINT('Ctrl Pts',(-9.47077840523181,23.0633093565331,
2.44748904607397));
#102755=CARTESIAN_POINT('Ctrl Pts',(-9.35860417055929,23.0543551047048,
2.50722045017388));
#102756=CARTESIAN_POINT('Ctrl Pts',(-9.27705128891861,23.0469716630282,
2.56493900388996));
#102757=CARTESIAN_POINT('Ctrl Pts',(-9.18745916098188,23.0381091525356,
2.647145485005));
#102758=CARTESIAN_POINT('Ctrl Pts',(-9.17159883438843,23.0365088076013,
2.66254251359347));
#102759=CARTESIAN_POINT('Ctrl Pts',(-9.14094518393495,23.0333659222212,
2.69402430286012));
#102760=CARTESIAN_POINT('Ctrl Pts',(-9.12614682421654,23.0318234942734,
2.71009318411981));
#102761=CARTESIAN_POINT('Ctrl Pts',(-9.10818058185257,23.0299282155362,
2.73072526878453));
#102762=CARTESIAN_POINT('Ctrl Pts',(-9.10458749754778,23.0295479903052,
2.73491050188852));
#102763=CARTESIAN_POINT('Ctrl Pts',(-9.09895188363171,23.0289499392386,
2.74156896130162));
#102764=CARTESIAN_POINT('Ctrl Pts',(-9.09688988196361,23.0287307571406,
2.74402548733671));
#102765=CARTESIAN_POINT('Ctrl Pts',(-9.09322336460718,23.0283404178905,
2.74842993381425));
#102766=CARTESIAN_POINT('Ctrl Pts',(-9.09161508295561,23.0281689936773,
2.75037457784156));
#102767=CARTESIAN_POINT('Ctrl Pts',(-9.0877695791583,23.0277585909487,2.75505489449824));
#102768=CARTESIAN_POINT('Ctrl Pts',(-9.08553840627414,23.0275200455541,
2.75779548280745));
#102769=CARTESIAN_POINT('Ctrl Pts',(-9.07878073130715,23.0267960916564,
2.76617278471099));
#102770=CARTESIAN_POINT('Ctrl Pts',(-9.07429365720912,23.0263133736313,
2.77184129730732));
#102771=CARTESIAN_POINT('Ctrl Pts',(-9.03422461456419,23.0219806289653,
2.82342951931208));
#102772=CARTESIAN_POINT('Ctrl Pts',(-9.00202823893325,23.0183372044505,
2.87188855632511));
#102773=CARTESIAN_POINT('Ctrl Pts',(-8.92383010259879,23.0084392756755,
3.01088770814555));
#102774=CARTESIAN_POINT('Ctrl Pts',(-8.88574396555258,23.0022659856779,
3.10527994350012));
#102775=CARTESIAN_POINT('Ctrl Pts',(-8.85680672798537,22.9947532088867,
3.21647352985328));
#102776=CARTESIAN_POINT('Ctrl Pts',(-8.8536252171123,22.993861882147,3.22962442973756));
#102777=CARTESIAN_POINT('Ctrl Pts',(-8.84926353835541,22.9925352883519,
3.24911714285368));
#102778=CARTESIAN_POINT('Ctrl Pts',(-8.84790770158202,22.9921055911176,
3.25541883696982));
#102779=CARTESIAN_POINT('Ctrl Pts',(-8.84559072287574,22.9913391912972,
3.26663472064089));
#102780=CARTESIAN_POINT('Ctrl Pts',(-8.84460905456937,22.9910031472258,
3.27154454567591));
#102781=CARTESIAN_POINT('Ctrl Pts',(-8.84260882160657,22.9902937479081,
3.28189149129765));
#102782=CARTESIAN_POINT('Ctrl Pts',(-8.8415971981809,22.9899201823506,3.28732981327721));
#102783=CARTESIAN_POINT('Ctrl Pts',(-8.8390208088264,22.9889280705859,3.30174411591937));
#102784=CARTESIAN_POINT('Ctrl Pts',(-8.83752185456827,22.9883074731128,
3.31073132542408));
#102785=CARTESIAN_POINT('Ctrl Pts',(-8.83082479147894,22.9853112918499,
3.3539705572244));
#102786=CARTESIAN_POINT('Ctrl Pts',(-8.82703589878992,22.9828922857979,
3.38842018872435));
#102787=CARTESIAN_POINT('Ctrl Pts',(-8.8204111533025,22.9756962939875,3.4895105468395));
#102788=CARTESIAN_POINT('Ctrl Pts',(-8.82170864262925,22.9708127131509,
3.55628058586012));
#102789=CARTESIAN_POINT('Ctrl Pts',(-8.83505326406694,22.9613976441742,
3.68380563593608));
#102790=CARTESIAN_POINT('Ctrl Pts',(-8.84625276007084,22.9568842466013,
3.74444685178082));
#102791=CARTESIAN_POINT('Ctrl Pts',(-8.86466004880756,22.9518860704531,
3.81335810222273));
#102792=CARTESIAN_POINT('Ctrl Pts',(-8.86729289943504,22.9512081985965,
3.82274563483428));
#102793=CARTESIAN_POINT('Ctrl Pts',(-8.87108549214189,22.9502815568797,
3.835649799364));
#102794=CARTESIAN_POINT('Ctrl Pts',(-8.87214560527832,22.9500275223116,
3.83919495736716));
#102795=CARTESIAN_POINT('Ctrl Pts',(-8.87399213090569,22.9495935184387,
3.84526560359985));
#102796=CARTESIAN_POINT('Ctrl Pts',(-8.87477036713728,22.9494130902777,
3.847793519165));
#102797=CARTESIAN_POINT('Ctrl Pts',(-8.87641329078853,22.9490373587804,
3.85306692634283));
#102798=CARTESIAN_POINT('Ctrl Pts',(-8.87727953529114,22.9488421540607,
3.85581189687584));
#102799=CARTESIAN_POINT('Ctrl Pts',(-8.87941876427522,22.9483670312179,
3.86250512474029));
#102800=CARTESIAN_POINT('Ctrl Pts',(-8.88070257873264,22.9480877352461,
3.8664499356919));
#102801=CARTESIAN_POINT('Ctrl Pts',(-8.88539754270523,22.9470867324137,
3.88062138938491));
#102802=CARTESIAN_POINT('Ctrl Pts',(-8.8889283470235,22.946371595946,3.89080824224801));
#102803=CARTESIAN_POINT('Ctrl Pts',(-8.8980964020739,22.9446016289321,3.91613017065139));
#102804=CARTESIAN_POINT('Ctrl Pts',(-8.90390614235746,22.9435551365598,
3.93120084378869));
#102805=CARTESIAN_POINT('Ctrl Pts',(-8.9307515929507,22.9390117608701,3.99678645093033));
#102806=CARTESIAN_POINT('Ctrl Pts',(-8.95498424295203,22.9356341429664,
4.04592302664047));
#102807=CARTESIAN_POINT('Ctrl Pts',(-9.02341368975843,22.9272357802339,
4.16329278718968));
#102808=CARTESIAN_POINT('Ctrl Pts',(-9.07140770928212,22.9222185825489,
4.2289666633575));
#102809=CARTESIAN_POINT('Ctrl Pts',(-9.13584619806587,22.9159465830941,
4.30034964010879));
#102810=CARTESIAN_POINT('Ctrl Pts',(-9.14613844965934,22.9149573771656,
4.31132099636075));
#102811=CARTESIAN_POINT('Ctrl Pts',(-9.16128015955294,22.9135179859253,
4.32685447786994));
#102812=CARTESIAN_POINT('Ctrl Pts',(-9.16596286344667,22.913074959806,4.33157762724275));
#102813=CARTESIAN_POINT('Ctrl Pts',(-9.17427314705011,22.912292267597,4.33981888523157));
#102814=CARTESIAN_POINT('Ctrl Pts',(-9.17788386543568,22.9119533475543,
4.34335381400726));
#102815=CARTESIAN_POINT('Ctrl Pts',(-9.18539072392015,22.9112510060069,
4.35060908162623));
#102816=CARTESIAN_POINT('Ctrl Pts',(-9.18928985891481,22.9108874547001,
4.35432613672612));
#102817=CARTESIAN_POINT('Ctrl Pts',(-9.19936996860191,22.9099506947303,
4.36380438174757));
#102818=CARTESIAN_POINT('Ctrl Pts',(-9.20558760151119,22.9093758282771,
4.36952595806485));
#102819=CARTESIAN_POINT('Ctrl Pts',(-9.23235202199716,22.9069132065865,
4.39362836702318));
#102820=CARTESIAN_POINT('Ctrl Pts',(-9.25347772717576,22.9049986724255,
4.41135029094205));
#102821=CARTESIAN_POINT('Ctrl Pts',(-9.35364843628494,22.8960443939538,
4.48956018440189));
#102822=CARTESIAN_POINT('Ctrl Pts',(-9.43953234870287,22.8886610032355,
4.54061028983103));
#102823=CARTESIAN_POINT('Ctrl Pts',(-9.55105769518797,22.8797985408336,
4.5890519957481));
#102824=CARTESIAN_POINT('Ctrl Pts',(-9.57157228371355,22.8781981904997,
4.59728447921133));
#102825=CARTESIAN_POINT('Ctrl Pts',(-9.61279560933652,22.8750553330705,
4.61249482770354));
#102826=CARTESIAN_POINT('Ctrl Pts',(-9.63349187484446,22.8735129375136,
4.61948377621964));
#102827=CARTESIAN_POINT('Ctrl Pts',(-9.65964498676793,22.8716176926594,
4.62751228428989));
#102828=CARTESIAN_POINT('Ctrl Pts',(-9.66492933730371,22.8712374700557,
4.62909394660222));
#102829=CARTESIAN_POINT('Ctrl Pts',(-9.67330360897312,22.8706394221968,
4.63153648483219));
#102830=CARTESIAN_POINT('Ctrl Pts',(-9.67638618673021,22.8704202407028,
4.63242193942965));
#102831=CARTESIAN_POINT('Ctrl Pts',(-9.68190070177898,22.8700299019667,
4.63398159921538));
#102832=CARTESIAN_POINT('Ctrl Pts',(-9.68433117632398,22.869858477668,4.63466057692419));
#102833=CARTESIAN_POINT('Ctrl Pts',(-9.69017051742674,22.8694480740127,
4.63627164126254));
#102834=CARTESIAN_POINT('Ctrl Pts',(-9.69358141641125,22.8692095277826,
4.63719620271137));
#102835=CARTESIAN_POINT('Ctrl Pts',(-9.70398233724887,22.8684855687757,
4.63996529209301));
#102836=CARTESIAN_POINT('Ctrl Pts',(-9.71098538643763,22.8680028465326,
4.64176086965066));
#102837=CARTESIAN_POINT('Ctrl Pts',(-9.77440889144461,22.8636699489553,
4.65740166925768));
#102838=CARTESIAN_POINT('Ctrl Pts',(-9.83177334691347,22.8600263916886,
4.66712110628741));
#102839=CARTESIAN_POINT('Ctrl Pts',(-9.99055656767438,22.8501285153288,
4.68206713353976));
#102840=CARTESIAN_POINT('Ctrl Pts',(-10.0922772414015,22.8439553906687,
4.67849681731113));
#102841=CARTESIAN_POINT('Ctrl Pts',(-10.2056303536822,22.8364427864322,
4.65973888621556));
#102842=CARTESIAN_POINT('Ctrl Pts',(-10.2189394052176,22.8355514355074,
4.65730015068657));
#102843=CARTESIAN_POINT('Ctrl Pts',(-10.2385225069046,22.8342248125344,
4.65336188023546));
#102844=CARTESIAN_POINT('Ctrl Pts',(-10.2448313088402,22.8337951106678,
4.65203916622086));
#102845=CARTESIAN_POINT('Ctrl Pts',(-10.2560207076755,22.8330287056575,
4.64959711640558));
#102846=CARTESIAN_POINT('Ctrl Pts',(-10.2609056605451,22.8326926610611,
4.64849830987026));
#102847=CARTESIAN_POINT('Ctrl Pts',(-10.2711722887196,22.8319832637974,
4.64612008568311));
#102848=CARTESIAN_POINT('Ctrl Pts',(-10.2765522404055,22.8316097008387,
4.6448338383775));
#102849=CARTESIAN_POINT('Ctrl Pts',(-10.2907690779143,22.8306176033824,
4.64132879492533));
#102850=CARTESIAN_POINT('Ctrl Pts',(-10.2995894732042,22.8299970177244,
4.6390453082358));
#102851=CARTESIAN_POINT('Ctrl Pts',(-10.3418155454092,22.8270009915379,
4.627589134115));
#102852=CARTESIAN_POINT('Ctrl Pts',(-10.3748290111891,22.8245821342223,
4.61704874805799));
#102853=CARTESIAN_POINT('Ctrl Pts',(-10.4698757177248,22.8173868189739,
4.58201465924872));
#102854=CARTESIAN_POINT('Ctrl Pts',(-10.5303474313801,22.8125037917916,
4.55369287113804));
#102855=CARTESIAN_POINT('Ctrl Pts',(-10.6414416516414,22.8030885404692,
4.48966620873711));
#102856=CARTESIAN_POINT('Ctrl Pts',(-10.6923033371855,22.7985744075567,
4.45477967851165));
#102857=CARTESIAN_POINT('Ctrl Pts',(-10.7477903296272,22.7935755563251,
4.40994490365898));
#102858=CARTESIAN_POINT('Ctrl Pts',(-10.7552971661018,22.7928976852761,
4.40372358115197));
#102859=CARTESIAN_POINT('Ctrl Pts',(-10.7655456090146,22.7919710444605,
4.39501322580882));
#102860=CARTESIAN_POINT('Ctrl Pts',(-10.7683537751204,22.7917170099989,
4.39260362482078));
#102861=CARTESIAN_POINT('Ctrl Pts',(-10.773149726938,22.7912830062645,4.38844896196955));
#102862=CARTESIAN_POINT('Ctrl Pts',(-10.7751430538494,22.791102578136,4.38671038378503));
#102863=CARTESIAN_POINT('Ctrl Pts',(-10.779293359031,22.79072684665,4.38306580058673));
#102864=CARTESIAN_POINT('Ctrl Pts',(-10.7814492282923,22.7905316419095,
4.38115858472673));
#102865=CARTESIAN_POINT('Ctrl Pts',(-10.7866950358297,22.7900565189346,
4.3764834236517));
#102866=CARTESIAN_POINT('Ctrl Pts',(-10.7897774231587,22.7897772228524,
4.37370698435284));
#102867=CARTESIAN_POINT('Ctrl Pts',(-10.8008169682858,22.7887762191819,
4.36365702880626));
#102868=CARTESIAN_POINT('Ctrl Pts',(-10.8086891347469,22.7880610820009,
4.35629036187227));
#102869=CARTESIAN_POINT('Ctrl Pts',(-10.8280982614162,22.7862911128643,
4.33762111255625));
#102870=CARTESIAN_POINT('Ctrl Pts',(-10.8395062665342,22.7852446191083,
4.32618711053092));
#102871=CARTESIAN_POINT('Ctrl Pts',(-10.8885174577236,22.780701233503,4.27500043614223));
#102872=CARTESIAN_POINT('Ctrl Pts',(-10.9235618016018,22.7773236075959,
4.23288709704573));
#102873=CARTESIAN_POINT('Ctrl Pts',(-11.0029831913953,22.7689252475592,
4.12265787682346));
#102874=CARTESIAN_POINT('Ctrl Pts',(-11.0434784642931,22.7639080602669,
4.05211294508536));
#102875=CARTESIAN_POINT('Ctrl Pts',(-11.0825057016338,22.7576360722458,
3.96422273306177));
#102876=CARTESIAN_POINT('Ctrl Pts',(-11.088346276408,22.756646866013,3.95035951089803));
#102877=CARTESIAN_POINT('Ctrl Pts',(-11.0963839103617,22.7552074744053,
3.93021113356674));
#102878=CARTESIAN_POINT('Ctrl Pts',(-11.0987958727566,22.7547644482282,
3.92401288341935));
#102879=CARTESIAN_POINT('Ctrl Pts',(-11.1029476784655,22.7539817559477,
3.91307022919081));
#102880=CARTESIAN_POINT('Ctrl Pts',(-11.1047097434336,22.7536428358918,
3.90833439369775));
#102881=CARTESIAN_POINT('Ctrl Pts',(-11.1082872586754,22.752940494347,3.89852657963515));
#102882=CARTESIAN_POINT('Ctrl Pts',(-11.1100984913735,22.7525769430562,
3.89345319950344));
#102883=CARTESIAN_POINT('Ctrl Pts',(-11.1146610949147,22.7516401831913,
3.88039072092305));
#102884=CARTESIAN_POINT('Ctrl Pts',(-11.1173613716986,22.7510653168277,
3.87238423118512));
#102885=CARTESIAN_POINT('Ctrl Pts',(-11.1285037661965,22.7486026961152,
3.83813359112886));
#102886=CARTESIAN_POINT('Ctrl Pts',(-11.1361085495252,22.7466881628699,
3.81162833569484));
#102887=CARTESIAN_POINT('Ctrl Pts',(-11.1668491146724,22.737733884525,3.68831582163793));
#102888=CARTESIAN_POINT('Ctrl Pts',(-11.1785820311721,22.7303504928557,
3.58909636281973));
#102889=CARTESIAN_POINT('Ctrl Pts',(-11.1775091561932,22.7214880295139,
3.46750954637182));
#102890=CARTESIAN_POINT('Ctrl Pts',(-11.1766922042522,22.7198876791792,
3.44541984925432));
#102891=CARTESIAN_POINT('Ctrl Pts',(-11.1738330866712,22.7167448218033,
3.40157304017101));
#102892=CARTESIAN_POINT('Ctrl Pts',(-11.1718061170206,22.7152024262992,
3.37982281786415));
#102893=CARTESIAN_POINT('Ctrl Pts',(-11.1685108839151,22.7133071814942,
3.35266432737117));
#102894=CARTESIAN_POINT('Ctrl Pts',(-11.1678080343469,22.7129269588897,
3.3471933111132));
#102895=CARTESIAN_POINT('Ctrl Pts',(-11.1666357598958,22.7123289110269,
3.33854922685531));
#102896=CARTESIAN_POINT('Ctrl Pts',(-11.1661917765163,22.7121097295298,
3.33537287760948));
#102897=CARTESIAN_POINT('Ctrl Pts',(-11.1653752680284,22.7117193907882,
3.32970051216835));
#102898=CARTESIAN_POINT('Ctrl Pts',(-11.1650076979605,22.7115479664872,
3.32720389252114));
#102899=CARTESIAN_POINT('Ctrl Pts',(-11.1641061223085,22.7111375628252,
3.32121385117013));
#102900=CARTESIAN_POINT('Ctrl Pts',(-11.1635644151219,22.7108990165907,
3.3177216313102));
#102901=CARTESIAN_POINT('Ctrl Pts',(-11.1618667165516,22.7101750575611,
3.30709313954435));
#102902=CARTESIAN_POINT('Ctrl Pts',(-11.160660705781,22.7096923352997,3.2999648621416));
#102903=CARTESIAN_POINT('Ctrl Pts',(-11.1491710637265,22.7053594371209,
3.23565961416983));
#102904=CARTESIAN_POINT('Ctrl Pts',(-11.1347341459828,22.7017158793319,
3.17929717413292));
#102905=CARTESIAN_POINT('Ctrl Pts',(-11.0838485488928,22.6918180300698,
3.02814820180221));
#102906=CARTESIAN_POINT('Ctrl Pts',(-11.0392398600315,22.6856449322495,
2.93666150420985));
#102907=CARTESIAN_POINT('Ctrl Pts',(-10.9760264812506,22.6781323423325,
2.84071975452016));
#102908=CARTESIAN_POINT('Ctrl Pts',(-10.9683883585278,22.6772409731502,
2.82955082472361));
#102909=CARTESIAN_POINT('Ctrl Pts',(-10.9568298884922,22.6759143281443,
2.8132590166168));
#102910=CARTESIAN_POINT('Ctrl Pts',(-10.95305697729,22.6754846227743,2.80803250869444));
#102911=CARTESIAN_POINT('Ctrl Pts',(-10.9463828327682,22.6747301183026,
2.79894513986962));
#102912=CARTESIAN_POINT('Ctrl Pts',(-10.943500376574,22.6744060461559,2.79507062673994));
#102913=CARTESIAN_POINT('Ctrl Pts',(-10.9404984449235,22.6740703401572,
2.79108691441192));
#102914=CARTESIAN_POINT('Ctrl Pts',(-10.9404026542334,22.6740596297606,
2.79095984899853));
#102915=CARTESIAN_POINT('Ctrl Pts',(-10.9401945068614,22.6740363607883,
2.79068385992561));
#102916=CARTESIAN_POINT('Ctrl Pts',(-10.9400821405552,22.6740238018383,
2.79053494355861));
#102917=CARTESIAN_POINT('Ctrl Pts',(-10.9366849798909,22.6736441859637,
2.78603499222511));
#102918=CARTESIAN_POINT('Ctrl Pts',(-10.9333700980759,22.6732759603372,
2.78170685499116));
#102919=CARTESIAN_POINT('Ctrl Pts',(-10.9244908013384,22.6722953019204,
2.7702786883632));
#102920=CARTESIAN_POINT('Ctrl Pts',(-10.9188747522893,22.6716808474911,
2.76321942470442));
#102921=CARTESIAN_POINT('Ctrl Pts',(-10.9063397076008,22.6703216620176,
2.74782936847711));
#102922=CARTESIAN_POINT('Ctrl Pts',(-10.8993858476592,22.6695755755493,
2.7395281675355));
#102923=CARTESIAN_POINT('Ctrl Pts',(-10.8781144460172,22.6673163496157,
2.71483521988049));
#102924=CARTESIAN_POINT('Ctrl Pts',(-10.86345670748,22.6657898444177,2.69874403466731));
#102925=CARTESIAN_POINT('Ctrl Pts',(-10.8043753815629,22.65975128346,2.63738955702079));
#102926=CARTESIAN_POINT('Ctrl Pts',(-10.7567755782989,22.6551196603724,
2.59534229879862));
#102927=CARTESIAN_POINT('Ctrl Pts',(-10.6524475488982,22.6455488522504,
2.51720360213104));
#102928=CARTESIAN_POINT('Ctrl Pts',(-10.595536589942,22.640624500551,2.48171002477099));
#102929=CARTESIAN_POINT('Ctrl Pts',(-10.5272797096882,22.6352538046754,
2.44683089371647));
#102930=CARTESIAN_POINT('Ctrl Pts',(-10.5185919055761,22.6345797294726,
2.44252588240749));
#102931=CARTESIAN_POINT('Ctrl Pts',(-10.5065223244178,22.633657303694,2.43672964980951));
#102932=CARTESIAN_POINT('Ctrl Pts',(-10.5031855043475,22.633403751244,2.43514646459337));
#102933=CARTESIAN_POINT('Ctrl Pts',(-10.4974479587568,22.6329703555232,
2.43245722477787));
#102934=CARTESIAN_POINT('Ctrl Pts',(-10.4950508818725,22.6327900561641,
2.43134351950177));
#102935=CARTESIAN_POINT('Ctrl Pts',(-10.4900341296499,22.6324143479675,
2.42903318978926));
#102936=CARTESIAN_POINT('Ctrl Pts',(-10.4874137881076,22.6322190389804,
2.42783809235608));
#102937=CARTESIAN_POINT('Ctrl Pts',(-10.4810009339065,22.631743261178,2.42494165675585));
#102938=CARTESIAN_POINT('Ctrl Pts',(-10.4772036990365,22.6314634185973,
2.42325073915324));
#102939=CARTESIAN_POINT('Ctrl Pts',(-10.4634762491885,22.6304582349115,
2.41722475643673));
#102940=CARTESIAN_POINT('Ctrl Pts',(-10.4534949120126,22.6297395365565,
2.41300651009185));
#102941=CARTESIAN_POINT('Ctrl Pts',(-10.428393497874,22.6279589537935,2.40280428198749));
#102942=CARTESIAN_POINT('Ctrl Pts',(-10.4132046846674,22.6269055364922,
2.39699438958741));
#102943=CARTESIAN_POINT('Ctrl Pts',(-10.3457550286884,22.6223122430691,
2.37278310438681));
#102944=CARTESIAN_POINT('Ctrl Pts',(-10.2923504182,22.6188943098857,2.35776680383763));
#102945=CARTESIAN_POINT('Ctrl Pts',(-10.1803869570358,22.6118273598725,
2.33465613649588));
#102946=CARTESIAN_POINT('Ctrl Pts',(-10.1218823962121,22.6081858122779,
2.32709345723607));
#102947=CARTESIAN_POINT('Ctrl Pts',(-10.0320757670174,22.6024488935694,
2.32227804859184));
#102948=CARTESIAN_POINT('Ctrl Pts',(-10.0010403120032,22.6004408014835,
2.3218419022633));
#102949=CARTESIAN_POINT('Ctrl Pts',(-9.96089153893417,22.5977923301093,
2.32286403517224));
#102950=CARTESIAN_POINT('Ctrl Pts',(-9.95176050739249,22.5971866256816,
2.32320286583241));
#102951=CARTESIAN_POINT('Ctrl Pts',(-9.93710380885206,22.5962085672495,
2.32391760769405));
#102952=CARTESIAN_POINT('Ctrl Pts',(-9.93157511943903,22.5958383027342,
2.3242263150194));
#102953=CARTESIAN_POINT('Ctrl Pts',(-9.92120640916872,22.5951413099788,
2.32487865520179));
#102954=CARTESIAN_POINT('Ctrl Pts',(-9.91636591902299,22.5948148702439,
2.32521323456465));
#102955=CARTESIAN_POINT('Ctrl Pts',(-9.90670274303069,22.5941610195652,
2.32594118689477));
#102956=CARTESIAN_POINT('Ctrl Pts',(-9.90188013924116,22.593833620134,2.32633438897631));
#102957=CARTESIAN_POINT('Ctrl Pts',(-9.89089078943258,22.5930850443722,
2.32729859010483));
#102958=CARTESIAN_POINT('Ctrl Pts',(-9.88472589228886,22.5926632863752,
2.32788853169215));
#102959=CARTESIAN_POINT('Ctrl Pts',(-9.85599229840556,22.5906888598805,
2.33086703344397));
#102960=CARTESIAN_POINT('Ctrl Pts',(-9.83350225220027,22.5891183274746,
2.33385743237855));
#102961=CARTESIAN_POINT('Ctrl Pts',(-9.81110404738658,22.5875279348072,
2.33749693265511));
#102962=CARTESIAN_POINT('Ctrl Pts',(-9.81110406371156,22.4887934941609,
2.33749693000246));
#102963=CARTESIAN_POINT('Ctrl Pts',(-9.81147112136522,22.4888175040634,
2.33743728654779));
#102964=CARTESIAN_POINT('Ctrl Pts',(-9.81183820880857,22.488841507528,2.33737781668908));
#102965=CARTESIAN_POINT('Ctrl Pts',(-9.85155032860022,22.4914373403487,
2.33096357106418));
#102966=CARTESIAN_POINT('Ctrl Pts',(-9.89119577716716,22.493933679374,2.32660934983867));
#102967=CARTESIAN_POINT('Ctrl Pts',(-10.0285358260178,22.502478031877,2.31854791086634));
#102968=CARTESIAN_POINT('Ctrl Pts',(-10.1264065581075,22.5084226337522,
2.32498376589142));
#102969=CARTESIAN_POINT('Ctrl Pts',(-10.2388190935285,22.5158639769365,
2.34659567678142));
#102970=CARTESIAN_POINT('Ctrl Pts',(-10.2552113863922,22.5169636356785,
2.35011165989876));
#102971=CARTESIAN_POINT('Ctrl Pts',(-10.2778488043926,22.5185050531027,
2.35547504427309));
#102972=CARTESIAN_POINT('Ctrl Pts',(-10.2841625673003,22.5189374467861,
2.35702626237878));
#102973=CARTESIAN_POINT('Ctrl Pts',(-10.2950356665279,22.5196865205771,
2.3597933166146));
#102974=CARTESIAN_POINT('Ctrl Pts',(-10.2996011824306,22.5200024067507,
2.36098443568946));
#102975=CARTESIAN_POINT('Ctrl Pts',(-10.3090487474681,22.5206589572948,
2.36350998743947));
#102976=CARTESIAN_POINT('Ctrl Pts',(-10.3139295904058,22.520999747303,2.36484851766386));
#102977=CARTESIAN_POINT('Ctrl Pts',(-10.325373120717,22.5218025968335,2.36806625889796));
#102978=CARTESIAN_POINT('Ctrl Pts',(-10.3319283392438,22.5222654748031,
2.36997113482653));
#102979=CARTESIAN_POINT('Ctrl Pts',(-10.3534428339781,22.523794708362,2.37642636754206));
#102980=CARTESIAN_POINT('Ctrl Pts',(-10.3683275266647,22.5248687923098,
2.38121747572462));
#102981=CARTESIAN_POINT('Ctrl Pts',(-10.4034658004634,22.5274440870409,
2.39330504689871));
#102982=CARTESIAN_POINT('Ctrl Pts',(-10.4236228055717,22.5289533353942,
2.40086307101975));
#102983=CARTESIAN_POINT('Ctrl Pts',(-10.5011617362671,22.5348849452216,
2.43238663638491));
#102984=CARTESIAN_POINT('Ctrl Pts',(-10.5568119147752,22.5394222443518,
2.46032685739353));
#102985=CARTESIAN_POINT('Ctrl Pts',(-10.6687350402838,22.5490281612899,
2.52809236099422));
#102986=CARTESIAN_POINT('Ctrl Pts',(-10.724261561519,22.5540849841267,2.56873312236311));
#102987=CARTESIAN_POINT('Ctrl Pts',(-10.7831945367248,22.5595732580376,
2.62034408004894));
#102988=CARTESIAN_POINT('Ctrl Pts',(-10.7903773918459,22.5602442731153,
2.62679222784452));
#102989=CARTESIAN_POINT('Ctrl Pts',(-10.8001934207664,22.5611632350731,
2.63582458724426));
#102990=CARTESIAN_POINT('Ctrl Pts',(-10.8028947041331,22.5614163340016,
2.63833373650506));
#102991=CARTESIAN_POINT('Ctrl Pts',(-10.8075106366579,22.5618491190787,
2.6426619055685));
#102992=CARTESIAN_POINT('Ctrl Pts',(-10.8094310108728,22.5620292589124,
2.64447473709484));
#102993=CARTESIAN_POINT('Ctrl Pts',(-10.8134330263759,22.5624048188505,
2.64827817362354));
#102994=CARTESIAN_POINT('Ctrl Pts',(-10.8155134846138,22.562600138252,2.65026997547042));
#102995=CARTESIAN_POINT('Ctrl Pts',(-10.8205818650077,22.5630762380493,
2.65515813227322));
#102996=CARTESIAN_POINT('Ctrl Pts',(-10.823561822078,22.5633563896119,2.65806276648798));
#102997=CARTESIAN_POINT('Ctrl Pts',(-10.8342713546468,22.5643643261544,
2.66861286637392));
#102998=CARTESIAN_POINT('Ctrl Pts',(-10.8419106591018,22.5650854190019,
2.67634975740693));
#102999=CARTESIAN_POINT('Ctrl Pts',(-10.8607572041319,22.5668732444412,
2.69597329809755));
#103000=CARTESIAN_POINT('Ctrl Pts',(-10.8718266082196,22.5679314196791,
2.70798969507191));
#103001=CARTESIAN_POINT('Ctrl Pts',(-10.9196437305343,22.5725597724467,
2.76211541975835));
#103002=CARTESIAN_POINT('Ctrl Pts',(-10.9536195014925,22.5760060963925,
2.80658159902901));
#103003=CARTESIAN_POINT('Ctrl Pts',(-11.0280257184825,22.5843824230875,
2.91983096405164));
#103004=CARTESIAN_POINT('Ctrl Pts',(-11.0648762191173,22.5893111180967,
2.99061845228588));
#103005=CARTESIAN_POINT('Ctrl Pts',(-11.09987716372,22.5954853845657,3.07858273864619));
#103006=CARTESIAN_POINT('Ctrl Pts',(-11.1051804603674,22.5964766165181,
3.09269372736918));
#103007=CARTESIAN_POINT('Ctrl Pts',(-11.1124325760055,22.5979183380969,
3.11317559901439));
#103008=CARTESIAN_POINT('Ctrl Pts',(-11.114600609015,22.5983616336624,3.1194676982417));
#103009=CARTESIAN_POINT('Ctrl Pts',(-11.1183205163343,22.5991445485932,
3.1305682585376));
#103010=CARTESIAN_POINT('Ctrl Pts',(-11.1198950063468,22.5994834194811,
3.13536900536065));
#103011=CARTESIAN_POINT('Ctrl Pts',(-11.1230830053116,22.6001854109187,
3.14530492228476));
#103012=CARTESIAN_POINT('Ctrl Pts',(-11.1246922942466,22.6005486596762,
3.15044131169001));
#103013=CARTESIAN_POINT('Ctrl Pts',(-11.128732911939,22.6014841112113,3.16365460811502));
#103014=CARTESIAN_POINT('Ctrl Pts',(-11.131112747975,22.6020579639269,3.17174681409444));
#103015=CARTESIAN_POINT('Ctrl Pts',(-11.140866077134,22.6045112069916,3.20627734420504));
#103016=CARTESIAN_POINT('Ctrl Pts',(-11.1474005465787,22.6064171272024,
3.23294162966112));
#103017=CARTESIAN_POINT('Ctrl Pts',(-11.1733054455582,22.6153654662514,
3.35729330379808));
#103018=CARTESIAN_POINT('Ctrl Pts',(-11.1811654032006,22.6227525912476,
3.45695127777926));
#103019=CARTESIAN_POINT('Ctrl Pts',(-11.1753423374674,22.6316183019501,
3.57844129287645));
#103020=CARTESIAN_POINT('Ctrl Pts',(-11.1736650577098,22.6332174831642,
3.60046428410857));
#103021=CARTESIAN_POINT('Ctrl Pts',(-11.1690890239858,22.6363665548424,
3.6442469414909));
#103022=CARTESIAN_POINT('Ctrl Pts',(-11.1661992143519,22.6379161220559,
3.6659996073744));
#103023=CARTESIAN_POINT('Ctrl Pts',(-11.161823143084,22.6398187828371,3.69311278846275));
#103024=CARTESIAN_POINT('Ctrl Pts',(-11.1609047724736,22.640199503536,3.69855900163287));
#103025=CARTESIAN_POINT('Ctrl Pts',(-11.1593924178605,22.6407981139688,
3.70715833577478));
#103026=CARTESIAN_POINT('Ctrl Pts',(-11.1588238176981,22.6410173646873,
3.71031575032225));
#103027=CARTESIAN_POINT('Ctrl Pts',(-11.157785133408,22.6414076902399,3.71595140548517));
#103028=CARTESIAN_POINT('Ctrl Pts',(-11.1573199923684,22.6415790330228,
3.71843044686254));
#103029=CARTESIAN_POINT('Ctrl Pts',(-11.1561848530464,22.6419890611733,
3.72437492187632));
#103030=CARTESIAN_POINT('Ctrl Pts',(-11.1555072373839,22.6422273151463,
3.72783885786239));
#103031=CARTESIAN_POINT('Ctrl Pts',(-11.1533979532726,22.6429497423578,
3.73836991508846));
#103032=CARTESIAN_POINT('Ctrl Pts',(-11.1519169148759,22.6434312407912,
3.74542714334026));
#103033=CARTESIAN_POINT('Ctrl Pts',(-11.1356474007692,22.6484656539802,
3.81955848126425));
#103034=CARTESIAN_POINT('Ctrl Pts',(-11.1150807901605,22.6527284782774,
3.88524064942433));
#103035=CARTESIAN_POINT('Ctrl Pts',(-11.0549897510122,22.6624843743005,
4.03104857018291));
#103036=CARTESIAN_POINT('Ctrl Pts',(-11.0118651569389,22.6679546790693,
4.10921477243793));
#103037=CARTESIAN_POINT('Ctrl Pts',(-10.9518351398395,22.674721762686,4.19377331474239));
#103038=CARTESIAN_POINT('Ctrl Pts',(-10.9430941193624,22.6756896939809,
4.20560966281997));
#103039=CARTESIAN_POINT('Ctrl Pts',(-10.9301195407496,22.6771035646855,
4.22250685198628));
#103040=CARTESIAN_POINT('Ctrl Pts',(-10.9260613649033,22.6775426982204,
4.22770107648143));
#103041=CARTESIAN_POINT('Ctrl Pts',(-10.9188224618674,22.6783207678073,
4.23680782283906));
#103042=CARTESIAN_POINT('Ctrl Pts',(-10.915659783461,22.6786589844663,4.2407345299276));
#103043=CARTESIAN_POINT('Ctrl Pts',(-10.9090525515149,22.6793620923168,
4.2488309365469));
#103044=CARTESIAN_POINT('Ctrl Pts',(-10.9056043008041,22.679727126805,4.25299745127169));
#103045=CARTESIAN_POINT('Ctrl Pts',(-10.8966288395546,22.6806724810337,
4.26369165649639));
#103046=CARTESIAN_POINT('Ctrl Pts',(-10.8910590770366,22.6812545187207,
4.27018305397498));
#103047=CARTESIAN_POINT('Ctrl Pts',(-10.8665720213626,22.6837941794013,
4.29810083052737));
#103048=CARTESIAN_POINT('Ctrl Pts',(-10.8469504026008,22.6857807215146,
4.31889362858558));
#103049=CARTESIAN_POINT('Ctrl Pts',(-10.7562549315112,22.6947625412879,
4.40825319477484));
#103050=CARTESIAN_POINT('Ctrl Pts',(-10.6774860835743,22.7020901661018,
4.46842776188902));
#103051=CARTESIAN_POINT('Ctrl Pts',(-10.5561125603031,22.7123216985217,
4.53902478374099));
#103052=CARTESIAN_POINT('Ctrl Pts',(-10.5189771668227,22.7153221249059,
4.5580629363984));
#103053=CARTESIAN_POINT('Ctrl Pts',(-10.4754543869269,22.7186356473081,
4.5775313718774));
#103054=CARTESIAN_POINT('Ctrl Pts',(-10.4699839989109,22.7190485542376,
4.57992859760193));
#103055=CARTESIAN_POINT('Ctrl Pts',(-10.4611907064019,22.7197063048984,
4.5837025089888));
#103056=CARTESIAN_POINT('Ctrl Pts',(-10.4578794071982,22.7199526480885,
4.58510572986747));
#103057=CARTESIAN_POINT('Ctrl Pts',(-10.4519783754874,22.7203891969778,
4.58757457314159));
#103058=CARTESIAN_POINT('Ctrl Pts',(-10.4493912094941,22.7205797524303,
4.58864615256977));
#103059=CARTESIAN_POINT('Ctrl Pts',(-10.4438152979682,22.7209886243323,
4.5909323769148));
#103060=CARTESIAN_POINT('Ctrl Pts',(-10.4408253736641,22.7212067596026,
4.59214397415234));
#103061=CARTESIAN_POINT('Ctrl Pts',(-10.4324913688708,22.7218117976014,
4.59548133508704));
#103062=CARTESIAN_POINT('Ctrl Pts',(-10.4271365496538,22.7221971480358,
4.5975802981885));
#103063=CARTESIAN_POINT('Ctrl Pts',(-10.3955233433343,22.7244533815988,
4.60970552942141));
#103064=CARTESIAN_POINT('Ctrl Pts',(-10.3689258232112,22.7262758287322,
4.61882934819671));
#103065=CARTESIAN_POINT('Ctrl Pts',(-10.2711367320055,22.7327908019953,
4.64850681129185));
#103066=CARTESIAN_POINT('Ctrl Pts',(-10.1983723437466,22.7372971067394,
4.66328543607542));
#103067=CARTESIAN_POINT('Ctrl Pts',(-10.0611977866984,22.7458699248212,
4.67789125675449));
#103068=CARTESIAN_POINT('Ctrl Pts',(-9.9972620587247,22.7498964281365,4.67947608504159));
#103069=CARTESIAN_POINT('Ctrl Pts',(-9.92368738043517,22.7547379207235,
4.67531629802573));
#103070=CARTESIAN_POINT('Ctrl Pts',(-9.91386417754612,22.7553884316813,
4.67463723199335));
#103071=CARTESIAN_POINT('Ctrl Pts',(-9.89780262305695,22.7564593338705,
4.67332436275405));
#103072=CARTESIAN_POINT('Ctrl Pts',(-9.89155864602184,22.7568774530901,
4.67276375893351));
#103073=CARTESIAN_POINT('Ctrl Pts',(-9.88035703657543,22.757630924742,4.67166782237895));
#103074=CARTESIAN_POINT('Ctrl Pts',(-9.87539773048635,22.7579656991762,
4.6711508006296));
#103075=CARTESIAN_POINT('Ctrl Pts',(-9.86484506401242,22.7586806518238,
4.66998286923371));
#103076=CARTESIAN_POINT('Ctrl Pts',(-9.85925280675639,22.7590610922839,
4.66932330717715));
#103077=CARTESIAN_POINT('Ctrl Pts',(-9.84416883004046,22.7600915783859,
4.66743449979983));
#103078=CARTESIAN_POINT('Ctrl Pts',(-9.83468718398015,22.7607439680981,
4.66612963614303));
#103079=CARTESIAN_POINT('Ctrl Pts',(-9.78478032163743,22.7642031489257,
4.65864057056181));
#103080=CARTESIAN_POINT('Ctrl Pts',(-9.74468618091658,22.7670714394813,
4.65047018230721));
#103081=CARTESIAN_POINT('Ctrl Pts',(-9.60607438152136,22.7773060954421,
4.61462104282906));
#103082=CARTESIAN_POINT('Ctrl Pts',(-9.51081960894664,22.7849604029738,
4.57622314853734));
#103083=CARTESIAN_POINT('Ctrl Pts',(-9.39975463853945,22.7941176434468,
4.51362555992845));
#103084=CARTESIAN_POINT('Ctrl Pts',(-9.37818275575029,22.795905411481,4.50053725811511));
#103085=CARTESIAN_POINT('Ctrl Pts',(-9.35221351847893,22.7980544293897,
4.48361629021532));
#103086=CARTESIAN_POINT('Ctrl Pts',(-9.34740395648211,22.7984522887774,
4.48043191472639));
#103087=CARTESIAN_POINT('Ctrl Pts',(-9.33990946392472,22.799071789127,4.47539028172277));
#103088=CARTESIAN_POINT('Ctrl Pts',(-9.33720861065951,22.7992949483867,
4.47355703087602));
#103089=CARTESIAN_POINT('Ctrl Pts',(-9.3322094522975,22.7997077771441,4.47013331976912));
#103090=CARTESIAN_POINT('Ctrl Pts',(-9.3299091990891,22.7998976344894,4.46854591658023));
#103091=CARTESIAN_POINT('Ctrl Pts',(-9.3246590072643,22.8003307751176,4.46489510568789));
#103092=CARTESIAN_POINT('Ctrl Pts',(-9.32171286228271,22.8005736944037,
4.46282635045081));
#103093=CARTESIAN_POINT('Ctrl Pts',(-9.31259984992687,22.8013248211682,
4.45636469119734));
#103094=CARTESIAN_POINT('Ctrl Pts',(-9.30646567458109,22.8018300342972,
4.45192569865471));
#103095=CARTESIAN_POINT('Ctrl Pts',(-9.29220492865885,22.8030047461393,
4.44139488898275));
#103096=CARTESIAN_POINT('Ctrl Pts',(-9.284113383506,22.8036714259412,4.43525641821857));
#103097=CARTESIAN_POINT('Ctrl Pts',(-9.25571858082127,22.8060154802308,
4.41313086780707));
#103098=CARTESIAN_POINT('Ctrl Pts',(-9.23586203184508,22.8076631339968,
4.39658025857982));
#103099=CARTESIAN_POINT('Ctrl Pts',(-9.15638711174995,22.8143683300938,
4.32577715628847));
#103100=CARTESIAN_POINT('Ctrl Pts',(-9.10187025245824,22.8192506808579,
4.26612956147161));
#103101=CARTESIAN_POINT('Ctrl Pts',(-9.02559758672961,22.8272924998202,
4.16324122388732));
#103102=CARTESIAN_POINT('Ctrl Pts',(-8.99965975655842,22.8303243938388,
4.1234320808522));
#103103=CARTESIAN_POINT('Ctrl Pts',(-8.97114041427299,22.8341193452375,
4.07327798138237));
#103104=CARTESIAN_POINT('Ctrl Pts',(-8.96620043261456,22.8347960576015,
4.0643209500944));
#103105=CARTESIAN_POINT('Ctrl Pts',(-8.9586266981879,22.8358652675289,4.05015521102481));
#103106=CARTESIAN_POINT('Ctrl Pts',(-8.95591384902843,22.8362549792115,
4.04498919000041));
#103107=CARTESIAN_POINT('Ctrl Pts',(-8.95118988026336,22.8369457530302,
4.03582869820003));
#103108=CARTESIAN_POINT('Ctrl Pts',(-8.94916289856311,22.8372462540806,
4.03184250147239));
#103109=CARTESIAN_POINT('Ctrl Pts',(-8.94456195012644,22.8379379187112,
4.02266543348808));
#103110=CARTESIAN_POINT('Ctrl Pts',(-8.94200350538437,22.8383296111018,
4.01746695332625));
#103111=CARTESIAN_POINT('Ctrl Pts',(-8.93499392710419,22.8394228693472,
4.00295494817141));
#103112=CARTESIAN_POINT('Ctrl Pts',(-8.93062681457883,22.8401272914525,
3.99360165485661));
#103113=CARTESIAN_POINT('Ctrl Pts',(-8.90364757695215,22.8446325630852,
3.93377965412974));
#103114=CARTESIAN_POINT('Ctrl Pts',(-8.88449423721458,22.8485490531958,
3.88183591636507));
#103115=CARTESIAN_POINT('Ctrl Pts',(-8.8557918886302,22.8559891120865,3.78309526674766));
#103116=CARTESIAN_POINT('Ctrl Pts',(-8.84529877326061,22.8594830575908,
3.7366850180096));
#103117=CARTESIAN_POINT('Ctrl Pts',(-8.8325443485864,22.8652935166092,3.65856298320422));
#103118=CARTESIAN_POINT('Ctrl Pts',(-8.82870802096962,22.8676096905187,
3.62716196305031));
#103119=CARTESIAN_POINT('Ctrl Pts',(-8.82355938170878,22.8721946861261,
3.56397130282093));
#103120=CARTESIAN_POINT('Ctrl Pts',(-8.82226142586907,22.8744614045507,
3.53220422301078));
#103121=CARTESIAN_POINT('Ctrl Pts',(-8.82224806909126,22.8770576580766,
3.49480350695868));
#103122=CARTESIAN_POINT('Ctrl Pts',(-8.82228624790393,22.8774456561934,
3.48918632619435));
#103123=CARTESIAN_POINT('Ctrl Pts',(-8.82241384376095,22.87807397988,3.48004105586985));
#103124=CARTESIAN_POINT('Ctrl Pts',(-8.8224789314498,22.8783155708503,3.47651279583978));
#103125=CARTESIAN_POINT('Ctrl Pts',(-8.82262386715468,22.8787465846121,
3.47019586076069));
#103126=CARTESIAN_POINT('Ctrl Pts',(-8.82269776581589,22.8789363264076,
3.46740713543066));
#103127=CARTESIAN_POINT('Ctrl Pts',(-8.82288123665371,22.8793504891829,
3.46130264916024));
#103128=CARTESIAN_POINT('Ctrl Pts',(-8.8229949094535,22.8795746822134,3.45798707941662));
#103129=CARTESIAN_POINT('Ctrl Pts',(-8.82336030858917,22.8802141367617,
3.44850001127749));
#103130=CARTESIAN_POINT('Ctrl Pts',(-8.82364657995732,22.8806275468544,
3.44232983863344));
#103131=CARTESIAN_POINT('Ctrl Pts',(-8.82601751710285,22.8835382509326,
3.39865259496866));
#103132=CARTESIAN_POINT('Ctrl Pts',(-8.82984729060606,22.8859483410634,
3.36125762952449));
#103133=CARTESIAN_POINT('Ctrl Pts',(-8.84745744154454,22.8933813108197,
3.24466624471591));
#103134=CARTESIAN_POINT('Ctrl Pts',(-8.86755307733356,22.8982484577425,
3.16666139223133));
#103135=CARTESIAN_POINT('Ctrl Pts',(-8.91220979989904,22.9063233148052,
3.04596854063539));
#103136=CARTESIAN_POINT('Ctrl Pts',(-8.9317589192599,22.9094085207859,3.00171070797751));
#103137=CARTESIAN_POINT('Ctrl Pts',(-8.95827015169717,22.9132028776575,
2.95047152081461));
#103138=CARTESIAN_POINT('Ctrl Pts',(-8.96266906716406,22.913821594004,2.94221226816856));
#103139=CARTESIAN_POINT('Ctrl Pts',(-8.97010706456577,22.9148506639582,
2.92863928918754));
#103140=CARTESIAN_POINT('Ctrl Pts',(-8.97309004253927,22.9152590407653,
2.92329517325145));
#103141=CARTESIAN_POINT('Ctrl Pts',(-8.97841651523805,22.9159808540324,
2.91392496616363));
#103142=CARTESIAN_POINT('Ctrl Pts',(-8.98074251626196,22.9162936614842,
2.90988904229916));
#103143=CARTESIAN_POINT('Ctrl Pts',(-8.985823708183,22.9169719190666,2.90119216220076));
#103144=CARTESIAN_POINT('Ctrl Pts',(-8.98858721028807,22.917337663036,2.89653621102473));
#103145=CARTESIAN_POINT('Ctrl Pts',(-8.99604882947459,22.9183170101244,
2.88416010059939));
#103146=CARTESIAN_POINT('Ctrl Pts',(-9.0008037896631,22.918932662821,2.87647481220961));
#103147=CARTESIAN_POINT('Ctrl Pts',(-9.01149180577035,22.9202985213205,
2.85963636804076));
#103148=CARTESIAN_POINT('Ctrl Pts',(-9.01746446930144,22.9210501367655,
2.85050947023202));
#103149=CARTESIAN_POINT('Ctrl Pts',(-9.03585962436427,22.9233311021802,
2.82323412441864));
#103150=CARTESIAN_POINT('Ctrl Pts',(-9.0486639307353,22.924874119586,2.80535023943774));
#103151=CARTESIAN_POINT('Ctrl Pts',(-9.10104472787236,22.9310177963152,
2.73635593017204));
#103152=CARTESIAN_POINT('Ctrl Pts',(-9.14429621338611,22.9357427072336,
2.68818591587217));
#103153=CARTESIAN_POINT('Ctrl Pts',(-9.23873658953856,22.9452821294783,
2.59898082414551));
#103154=CARTESIAN_POINT('Ctrl Pts',(-9.28984902514721,22.9500796862204,
2.55816943488881));
#103155=CARTESIAN_POINT('Ctrl Pts',(-9.35215524594312,22.9553360154291,
2.51639101222574));
#103156=CARTESIAN_POINT('Ctrl Pts',(-9.36029212843856,22.9560115706129,
2.51107971980795));
#103157=CARTESIAN_POINT('Ctrl Pts',(-9.37161318720491,22.9569355835336,
2.50388819393825));
#103158=CARTESIAN_POINT('Ctrl Pts',(-9.37474160194837,22.9571892680886,
2.50192151948692));
#103159=CARTESIAN_POINT('Ctrl Pts',(-9.38012349529984,22.9576227916385,
2.49857343397411));
#103160=CARTESIAN_POINT('Ctrl Pts',(-9.38237243874137,22.9578030876769,
2.49718484048716));
#103161=CARTESIAN_POINT('Ctrl Pts',(-9.38708014967686,22.958178674492,2.49429994345847));
#103162=CARTESIAN_POINT('Ctrl Pts',(-9.38953975204667,22.9583738660677,
2.49280506724892));
#103163=CARTESIAN_POINT('Ctrl Pts',(-9.39556010488616,22.9588491648408,
2.48917622304701));
#103164=CARTESIAN_POINT('Ctrl Pts',(-9.39912675074334,22.9591286481999,
2.48705200800242));
#103165=CARTESIAN_POINT('Ctrl Pts',(-9.41201685023571,22.9601314629707,
2.47946699101358));
#103166=CARTESIAN_POINT('Ctrl Pts',(-9.42140445621274,22.9608481911866,
2.47411549184541));
#103167=CARTESIAN_POINT('Ctrl Pts',(-9.4450475607895,22.9626229951323,2.4610653111875));
#103168=CARTESIAN_POINT('Ctrl Pts',(-9.45939109288218,22.9636726724585,
2.45352995178986));
#103169=CARTESIAN_POINT('Ctrl Pts',(-9.52312743210442,22.9682394075834,
2.42170654196351));
#103170=CARTESIAN_POINT('Ctrl Pts',(-9.57403546410357,22.971635936793,2.40060043569637));
#103171=CARTESIAN_POINT('Ctrl Pts',(-9.68653025503974,22.9789689096178,
2.3629537187566));
#103172=CARTESIAN_POINT('Ctrl Pts',(-9.74835386439087,22.9828982796882,
2.34769325374467));
#103173=CARTESIAN_POINT('Ctrl Pts',(-9.8111040637108,22.9869701371802,2.33749693000258));
#103174=CARTESIAN_POINT('Origin',(-10.,12.3756328852638,3.5));
#103175=CARTESIAN_POINT('',(-9.81110406371025,23.5855117083725,2.33749693000267));
#103176=CARTESIAN_POINT('',(-9.81110406371068,23.4873487054734,2.3374969300026));
#103177=CARTESIAN_POINT('',(-9.81110406371068,12.3756328852638,2.3374969300026));
#103178=CARTESIAN_POINT('Ctrl Pts',(-9.81110406370983,23.5855117083725,
2.33749693000274));
#103179=CARTESIAN_POINT('Ctrl Pts',(-9.81101707518383,23.5855055469538,
2.33751106482912));
#103180=CARTESIAN_POINT('Ctrl Pts',(-9.81093008809885,23.5854993859672,
2.337525209443));
#103181=CARTESIAN_POINT('Ctrl Pts',(-9.80226865091188,23.5848859600242,
2.33893460820937));
#103182=CARTESIAN_POINT('Ctrl Pts',(-9.7937095796167,23.5842829952613,2.34042473120738));
#103183=CARTESIAN_POINT('Ctrl Pts',(-9.78169619421968,23.5834419290962,
2.34265347653336));
#103184=CARTESIAN_POINT('Ctrl Pts',(-9.7782277735032,23.5831997197652,2.34331309017284));
#103185=CARTESIAN_POINT('Ctrl Pts',(-9.77195496188742,23.5827628541751,
2.34453528677058));
#103186=CARTESIAN_POINT('Ctrl Pts',(-9.76914955961378,23.5825679030302,
2.34509250685753));
#103187=CARTESIAN_POINT('Ctrl Pts',(-9.76341917038147,23.5821706056214,
2.34625241415772));
#103188=CARTESIAN_POINT('Ctrl Pts',(-9.76049440301973,23.58196831198,2.34685601493027));
#103189=CARTESIAN_POINT('Ctrl Pts',(-9.75301012025541,23.5814518260193,
2.34843029191857));
#103190=CARTESIAN_POINT('Ctrl Pts',(-9.74845396022,23.5811385219708,2.34941693695617));
#103191=CARTESIAN_POINT('Ctrl Pts',(-9.72960140501996,23.5798462921623,
2.35361683134307));
#103192=CARTESIAN_POINT('Ctrl Pts',(-9.71535901643465,23.5788800036326,
2.35706984956996));
#103193=CARTESIAN_POINT('Ctrl Pts',(-9.67728282427724,23.5763143591768,
2.36705725797825));
#103194=CARTESIAN_POINT('Ctrl Pts',(-9.65358324299116,23.5747361805619,
2.37407761130642));
#103195=CARTESIAN_POINT('Ctrl Pts',(-9.5790534432492,23.5697826789619,2.39873151520884));
#103196=CARTESIAN_POINT('Ctrl Pts',(-9.52920128349297,23.5664813304822,
2.41910344002792));
#103197=CARTESIAN_POINT('Ctrl Pts',(-9.41368706332256,23.5585149651967,
2.47582163609594));
#103198=CARTESIAN_POINT('Ctrl Pts',(-9.34977113351562,23.5538328158559,
2.51516277653947));
#103199=CARTESIAN_POINT('Ctrl Pts',(-9.28214195159639,23.5482645163903,
2.56625884324312));
#103200=CARTESIAN_POINT('Ctrl Pts',(-9.2743324726514,23.5476116694787,2.57231505589825));
#103201=CARTESIAN_POINT('Ctrl Pts',(-9.26168569481117,23.546537624221,2.5823799800188));
#103202=CARTESIAN_POINT('Ctrl Pts',(-9.25680251856624,23.5461187197544,
2.58633046711241));
#103203=CARTESIAN_POINT('Ctrl Pts',(-9.24809792827701,23.54536428793,2.5934884305085));
#103204=CARTESIAN_POINT('Ctrl Pts',(-9.24426482642995,23.5450293434679,
2.59668150843771));
#103205=CARTESIAN_POINT('Ctrl Pts',(-9.23615191040966,23.5443145164667,
2.60352756942573));
#103206=CARTESIAN_POINT('Ctrl Pts',(-9.23187776968723,23.5439343746302,
2.60718705198356));
#103207=CARTESIAN_POINT('Ctrl Pts',(-9.22042365434018,23.5429059099274,
2.61713709695367));
#103208=CARTESIAN_POINT('Ctrl Pts',(-9.2132937954423,23.5422552599191,2.6234844424371));
#103209=CARTESIAN_POINT('Ctrl Pts',(-9.1763319139982,23.5388259976685,2.65720399215282));
#103210=CARTESIAN_POINT('Ctrl Pts',(-9.14785211353399,23.5359871673753,
2.68601134459554));
#103211=CARTESIAN_POINT('Ctrl Pts',(-9.05490272319349,23.5260066887844,
2.79026376700387));
#103212=CARTESIAN_POINT('Ctrl Pts',(-8.99851808058813,23.518596891733,2.87233390778798));
#103213=CARTESIAN_POINT('Ctrl Pts',(-8.94007636325438,23.5094011561515,
2.98573965111557));
#103214=CARTESIAN_POINT('Ctrl Pts',(-8.92798151386329,23.5073816021219,
3.01145267386354));
#103215=CARTESIAN_POINT('Ctrl Pts',(-8.91468974465211,23.5050329677426,
3.04258732744809));
#103216=CARTESIAN_POINT('Ctrl Pts',(-8.9125868264393,23.5046570733917,3.04760935444201));
#103217=CARTESIAN_POINT('Ctrl Pts',(-8.90919805317204,23.5040443589991,
3.05586233553087));
#103218=CARTESIAN_POINT('Ctrl Pts',(-8.90789157570977,23.5038063733817,
3.05908465371917));
#103219=CARTESIAN_POINT('Ctrl Pts',(-8.90556316458353,23.5033790790681,
3.06490133280638));
#103220=CARTESIAN_POINT('Ctrl Pts',(-8.90453616203801,23.5031894768288,
3.06749356408747));
#103221=CARTESIAN_POINT('Ctrl Pts',(-8.90229064064518,23.5027723904805,
3.07322074002767));
#103222=CARTESIAN_POINT('Ctrl Pts',(-8.90107634080789,23.5025451566556,
3.07635726568556));
#103223=CARTESIAN_POINT('Ctrl Pts',(-8.89759375199082,23.5018883845145,
3.08546849577285));
#103224=CARTESIAN_POINT('Ctrl Pts',(-8.89536059101781,23.5014608566283,
3.09145663105133));
#103225=CARTESIAN_POINT('Ctrl Pts',(-8.87794080178847,23.4980716490016,
3.13935440930605));
#103226=CARTESIAN_POINT('Ctrl Pts',(-8.86509398194838,23.4952331498113,
3.18208268762178));
#103227=CARTESIAN_POINT('Ctrl Pts',(-8.82882610413601,23.4854898947136,
3.3333714158876));
#103228=CARTESIAN_POINT('Ctrl Pts',(-8.81833889267637,23.47881866449,3.44440884737529));
#103229=CARTESIAN_POINT('Ctrl Pts',(-8.82433587244591,23.4705125533034,
3.57204786151172));
#103230=CARTESIAN_POINT('Ctrl Pts',(-8.82548256202627,23.4694110868983,
3.58880189767733));
#103231=CARTESIAN_POINT('Ctrl Pts',(-8.82757002399933,23.4678674561839,
3.61200606003856));
#103232=CARTESIAN_POINT('Ctrl Pts',(-8.8282067537677,23.4674346908718,3.6184820296495));
#103233=CARTESIAN_POINT('Ctrl Pts',(-8.82939796104694,23.4666850778343,
3.62964650186105));
#103234=CARTESIAN_POINT('Ctrl Pts',(-8.82992702998382,23.4663690260153,
3.63433760745525));
#103235=CARTESIAN_POINT('Ctrl Pts',(-8.83108184921524,23.4657122299756,
3.64405223334209));
#103236=CARTESIAN_POINT('Ctrl Pts',(-8.83171181254191,23.4653713605783,
3.64907514491255));
#103237=CARTESIAN_POINT('Ctrl Pts',(-8.83326715052518,23.4645684979268,
3.6608605197483));
#103238=CARTESIAN_POINT('Ctrl Pts',(-8.83421896024185,23.4641056872272,
3.66761924945302));
#103239=CARTESIAN_POINT('Ctrl Pts',(-8.83754237941596,23.4625774508508,
3.68981938995061));
#103240=CARTESIAN_POINT('Ctrl Pts',(-8.84016239109484,23.4615043128495,
3.70522134540036));
#103241=CARTESIAN_POINT('Ctrl Pts',(-8.84711403406541,23.4589318240004,
3.74168408097576));
#103242=CARTESIAN_POINT('Ctrl Pts',(-8.85171744156,23.4574244609459,3.7626867154389));
#103243=CARTESIAN_POINT('Ctrl Pts',(-8.8718286822172,23.451505029933,3.84376329162419));
#103244=CARTESIAN_POINT('Ctrl Pts',(-8.89149714874639,23.446978559522,3.90269533367618));
#103245=CARTESIAN_POINT('Ctrl Pts',(-8.94259832125502,23.4373688546333,
4.02320134496668));
#103246=CARTESIAN_POINT('Ctrl Pts',(-8.97499687617051,23.4322970140959,
4.08413042525668));
#103247=CARTESIAN_POINT('Ctrl Pts',(-9.01779411951237,23.426795631612,4.14996898455672));
#103248=CARTESIAN_POINT('Ctrl Pts',(-9.02314960528399,23.4261251540622,
4.15799042082109));
#103249=CARTESIAN_POINT('Ctrl Pts',(-9.03068775447707,23.425206734713,4.16898611634926));
#103250=CARTESIAN_POINT('Ctrl Pts',(-9.03278657611005,23.4249536501735,
4.17201699885985));
#103251=CARTESIAN_POINT('Ctrl Pts',(-9.03641354496114,23.424520844159,4.17720246817957));
#103252=CARTESIAN_POINT('Ctrl Pts',(-9.03793475616552,23.4243406692806,
4.17936183746314));
#103253=CARTESIAN_POINT('Ctrl Pts',(-9.04113067826038,23.4239649815283,
4.18386620745407));
#103254=CARTESIAN_POINT('Ctrl Pts',(-9.0428067477167,23.4237695697075,4.18621020387677));
#103255=CARTESIAN_POINT('Ctrl Pts',(-9.04692622004022,23.423293148642,4.19192685818933));
#103256=CARTESIAN_POINT('Ctrl Pts',(-9.04937897316487,23.4230127696446,
4.19529279572514));
#103257=CARTESIAN_POINT('Ctrl Pts',(-9.05830894144836,23.422003469309,4.20741188989303));
#103258=CARTESIAN_POINT('Ctrl Pts',(-9.06488985544988,23.4212812623764,
4.21608845142274));
#103259=CARTESIAN_POINT('Ctrl Pts',(-9.08166197307433,23.4194902052022,
4.23757593195497));
#103260=CARTESIAN_POINT('Ctrl Pts',(-9.09200193049313,23.4184299503672,
4.25026831816613));
#103261=CARTESIAN_POINT('Ctrl Pts',(-9.13892737746803,23.4137868753006,
4.30547799986115));
#103262=CARTESIAN_POINT('Ctrl Pts',(-9.17826047041481,23.4103286950745,
4.34556845318698));
#103263=CARTESIAN_POINT('Ctrl Pts',(-9.27976876738372,23.4019565318056,
4.43523101264957));
#103264=CARTESIAN_POINT('Ctrl Pts',(-9.34438121545476,23.3970435419503,
4.48160685996782));
#103265=CARTESIAN_POINT('Ctrl Pts',(-9.42623512297582,23.3908865465204,
4.52864781979968));
#103266=CARTESIAN_POINT('Ctrl Pts',(-9.43945246130103,23.3898949133534,
4.53590969411713));
#103267=CARTESIAN_POINT('Ctrl Pts',(-9.45870049499698,23.3884526234533,
4.54600871493575));
#103268=CARTESIAN_POINT('Ctrl Pts',(-9.46462189843755,23.3880091668679,
4.54905179621608));
#103269=CARTESIAN_POINT('Ctrl Pts',(-9.47508336334705,23.3872259723091,
4.554316428426));
#103270=CARTESIAN_POINT('Ctrl Pts',(-9.47961256013503,23.3868869833996,
4.55655928264882));
#103271=CARTESIAN_POINT('Ctrl Pts',(-9.48899647778078,23.3861847511278,
4.56113121468938));
#103272=CARTESIAN_POINT('Ctrl Pts',(-9.49385300727551,23.3858213794986,
4.56345628711216));
#103273=CARTESIAN_POINT('Ctrl Pts',(-9.50636043651531,23.3848856167639,
4.56933915897361));
#103274=CARTESIAN_POINT('Ctrl Pts',(-9.51403382576969,23.3843115746743,
4.57284813771647));
#103275=CARTESIAN_POINT('Ctrl Pts',(-9.5468346251224,23.3818575075611,4.58742358237182));
#103276=CARTESIAN_POINT('Ctrl Pts',(-9.57230538530207,23.3799509352076,
4.59769121514611));
#103277=CARTESIAN_POINT('Ctrl Pts',(-9.69173773467153,23.370999836015,4.64104815204983));
#103278=CARTESIAN_POINT('Ctrl Pts',(-9.7892904225141,23.3636104223965,4.66301849242003));
#103279=CARTESIAN_POINT('Ctrl Pts',(-9.91040892687715,23.3547422802659,
4.67454520474798));
#103280=CARTESIAN_POINT('Ctrl Pts',(-9.93245445787871,23.3531425821469,
4.67601900143798));
#103281=CARTESIAN_POINT('Ctrl Pts',(-9.97640594384946,23.3499963265144,
4.67771714839619));
#103282=CARTESIAN_POINT('Ctrl Pts',(-9.99830359624389,23.3484499969593,
4.67795230529546));
#103283=CARTESIAN_POINT('Ctrl Pts',(-10.0257162109439,23.3465506379679,
4.67748214975646));
#103284=CARTESIAN_POINT('Ctrl Pts',(-10.0312351284897,23.3461700970871,
4.67734867658333));
#103285=CARTESIAN_POINT('Ctrl Pts',(-10.0399596876264,23.3455716608668,
4.67707628405724));
#103286=CARTESIAN_POINT('Ctrl Pts',(-10.0431659636651,23.3453524064341,
4.67696306455678));
#103287=CARTESIAN_POINT('Ctrl Pts',(-10.0488932192871,23.3449620061932,
4.67673738918582));
#103288=CARTESIAN_POINT('Ctrl Pts',(-10.0514142872176,23.3447905927912,
4.67662993385771));
#103289=CARTESIAN_POINT('Ctrl Pts',(-10.0574637255756,23.3443803030669,
4.67635260885028));
#103290=CARTESIAN_POINT('Ctrl Pts',(-10.0609916974175,23.3441418591729,
4.6761749673291));
#103291=CARTESIAN_POINT('Ctrl Pts',(-10.0717294179682,23.3434185229589,
4.67558585459938));
#103292=CARTESIAN_POINT('Ctrl Pts',(-10.0789363941969,23.3429363144214,
4.67512393519489));
#103293=CARTESIAN_POINT('Ctrl Pts',(-10.1438050908159,23.3386219393218,
4.67036679437135));
#103294=CARTESIAN_POINT('Ctrl Pts',(-10.2010901683696,23.3349944654803,
4.66189628246485));
#103295=CARTESIAN_POINT('Ctrl Pts',(-10.3567973717927,23.3250901826691,
4.62700485358089));
#103296=CARTESIAN_POINT('Ctrl Pts',(-10.4527548543426,23.3188969946901,
4.59199602132031));
#103297=CARTESIAN_POINT('Ctrl Pts',(-10.5549845392699,23.311363458729,4.53887874889231));
#103298=CARTESIAN_POINT('Ctrl Pts',(-10.5668421380572,23.3104750643262,
4.53245671089563));
#103299=CARTESIAN_POINT('Ctrl Pts',(-10.5841934336795,23.3091520097465,
4.52267029554523));
#103300=CARTESIAN_POINT('Ctrl Pts',(-10.5897742731672,23.3087228757776,
4.5194620175764));
#103301=CARTESIAN_POINT('Ctrl Pts',(-10.5996477774832,23.3079571078968,
4.51367779157077));
#103302=CARTESIAN_POINT('Ctrl Pts',(-10.6039508804681,23.3076211285435,
4.51111990130719));
#103303=CARTESIAN_POINT('Ctrl Pts',(-10.6129782463306,23.3069114815719,
4.50567558451094));
#103304=CARTESIAN_POINT('Ctrl Pts',(-10.6176987134544,23.306537601241,4.50278313175881));
#103305=CARTESIAN_POINT('Ctrl Pts',(-10.6301512448122,23.3055437517526,
4.49503159015562));
#103306=CARTESIAN_POINT('Ctrl Pts',(-10.6378473581646,23.3049217184631,
4.49011574891226));
#103307=CARTESIAN_POINT('Ctrl Pts',(-10.6746750834727,23.3019065936442,
4.46598470553752));
#103308=CARTESIAN_POINT('Ctrl Pts',(-10.7029973879467,23.2994694078982,
4.44557239465249));
#103309=CARTESIAN_POINT('Ctrl Pts',(-10.7833690607167,23.2921902110997,
4.38203867004065));
#103310=CARTESIAN_POINT('Ctrl Pts',(-10.8326601002508,23.2872383952941,
4.33566414290791));
#103311=CARTESIAN_POINT('Ctrl Pts',(-10.9179362468099,23.2778484491652,
4.24035760511454));
#103312=CARTESIAN_POINT('Ctrl Pts',(-10.9546618017348,23.2734280958764,
4.19235733427934));
#103313=CARTESIAN_POINT('Ctrl Pts',(-10.9928773672048,23.268513240034,4.13354969517362));
#103314=CARTESIAN_POINT('Ctrl Pts',(-10.9981035402641,23.267833281333,4.12528395236271));
#103315=CARTESIAN_POINT('Ctrl Pts',(-11.0051666385238,23.2669043259113,
4.11379867257014));
#103316=CARTESIAN_POINT('Ctrl Pts',(-11.0070920513212,23.2666500297705,
4.1106344100599));
#103317=CARTESIAN_POINT('Ctrl Pts',(-11.0103672681286,23.266215695865,4.1051942225876));
#103318=CARTESIAN_POINT('Ctrl Pts',(-11.0117243739554,23.2660351977404,
4.10292276044115));
#103319=CARTESIAN_POINT('Ctrl Pts',(-11.0145413547174,23.2656594528853,
4.09817153244428));
#103320=CARTESIAN_POINT('Ctrl Pts',(-11.015999811051,23.2654643041044,4.09569096588834));
#103321=CARTESIAN_POINT('Ctrl Pts',(-11.0195363656332,23.2649895337436,
4.08962516368918));
#103322=CARTESIAN_POINT('Ctrl Pts',(-11.0216046879249,23.2647105321189,
4.08603421181082));
#103323=CARTESIAN_POINT('Ctrl Pts',(-11.0289707722116,23.2637117749175,
4.07308794941716));
#103324=CARTESIAN_POINT('Ctrl Pts',(-11.0341595256549,23.2629985510409,
4.06367077586474));
#103325=CARTESIAN_POINT('Ctrl Pts',(-11.0467899046986,23.261234276896,4.03998597022747));
#103326=CARTESIAN_POINT('Ctrl Pts',(-11.0540696520248,23.2601914961133,
4.02563406964567));
#103327=CARTESIAN_POINT('Ctrl Pts',(-11.0846417881746,23.2556746723774,
3.96217029645215));
#103328=CARTESIAN_POINT('Ctrl Pts',(-11.1048142069596,23.2523184816334,
3.91162567659839));
#103329=CARTESIAN_POINT('Ctrl Pts',(-11.1463631698139,23.2439127004305,
3.78214928450594));
#103330=CARTESIAN_POINT('Ctrl Pts',(-11.1631533058807,23.2388675161486,
3.70206188922571));
#103331=CARTESIAN_POINT('Ctrl Pts',(-11.1730722110978,23.2325647266658,
3.60593649631977));
#103332=CARTESIAN_POINT('Ctrl Pts',(-11.1743285096681,23.2315763504572,
3.59095862594046));
#103333=CARTESIAN_POINT('Ctrl Pts',(-11.1757266318038,23.2301379501857,
3.56932644287678));
#103334=CARTESIAN_POINT('Ctrl Pts',(-11.1760992571527,23.2296950713407,
3.56268813835158));
#103335=CARTESIAN_POINT('Ctrl Pts',(-11.1766560970862,23.2289125508986,
3.55100020698347));
#103336=CARTESIAN_POINT('Ctrl Pts',(-11.1768640613717,23.2285736543167,
3.54595184013623));
#103337=CARTESIAN_POINT('Ctrl Pts',(-11.177226649725,23.2278712749456,3.53551770266875));
#103338=CARTESIAN_POINT('Ctrl Pts',(-11.1773768125007,23.2275076618275,
3.53013190571305));
#103339=CARTESIAN_POINT('Ctrl Pts',(-11.1776676296243,23.2265705590003,
3.51629357507749));
#103340=CARTESIAN_POINT('Ctrl Pts',(-11.1777542396828,23.2259954091592,
3.50784033621611));
#103341=CARTESIAN_POINT('Ctrl Pts',(-11.1777354735185,23.2235298395984,
3.47178007639624));
#103342=CARTESIAN_POINT('Ctrl Pts',(-11.17675043923,23.2216125609006,3.44418429720845));
#103343=CARTESIAN_POINT('Ctrl Pts',(-11.1677558339711,23.2126571793346,
3.31740688234046));
#103344=CARTESIAN_POINT('Ctrl Pts',(-11.1481673106871,23.2052758565925,
3.21946509557233));
#103345=CARTESIAN_POINT('Ctrl Pts',(-11.1094781170695,23.1964153424189,
3.10421987858845));
#103346=CARTESIAN_POINT('Ctrl Pts',(-11.101854943103,23.1948147655459,3.08346743809587));
#103347=CARTESIAN_POINT('Ctrl Pts',(-11.0855546728982,23.1916730829631,
3.04267931151401));
#103348=CARTESIAN_POINT('Ctrl Pts',(-11.0768953121776,23.1901320484666,
3.02264500061779));
#103349=CARTESIAN_POINT('Ctrl Pts',(-11.0653560135108,23.1882382272865,
2.99786253542938));
#103350=CARTESIAN_POINT('Ctrl Pts',(-11.0629932875171,23.187858115015,2.99287995253891));
#103351=CARTESIAN_POINT('Ctrl Pts',(-11.0592012769998,23.1872602017794,
2.9850262133917));
#103352=CARTESIAN_POINT('Ctrl Pts',(-11.057795147973,23.1870410455657,2.98214406285108));
#103353=CARTESIAN_POINT('Ctrl Pts',(-11.0552614423572,23.1866507281333,
2.9770040923002));
#103354=CARTESIAN_POINT('Ctrl Pts',(-11.0541383869982,23.1864793000443,
2.97474416478042));
#103355=CARTESIAN_POINT('Ctrl Pts',(-11.0514249711527,23.1860688568256,
2.969327704857));
#103356=CARTESIAN_POINT('Ctrl Pts',(-11.0498276564678,23.1858302750649,
2.96617470336081));
#103357=CARTESIAN_POINT('Ctrl Pts',(-11.0449189014065,23.1851060996829,
2.9565923697817));
#103358=CARTESIAN_POINT('Ctrl Pts',(-11.0415623399643,23.1846231989432,
2.95018615736621));
#103359=CARTESIAN_POINT('Ctrl Pts',(-11.010667187408,23.1802838372059,2.89251923053103));
#103360=CARTESIAN_POINT('Ctrl Pts',(-10.9794198699957,23.1766346683611,
2.84332680414146));
#103361=CARTESIAN_POINT('Ctrl Pts',(-10.8841916339141,23.1667390022392,
2.71542884769285));
#103362=CARTESIAN_POINT('Ctrl Pts',(-10.8135123263704,23.1605728638889,
2.64236232592251));
#103363=CARTESIAN_POINT('Ctrl Pts',(-10.72377249514,23.1530675523117,2.57078962122851));
#103364=CARTESIAN_POINT('Ctrl Pts',(-10.7130378007323,23.152175181706,2.5625270015829));
#103365=CARTESIAN_POINT('Ctrl Pts',(-10.696985833039,23.150847328269,2.55060682531489));
#103366=CARTESIAN_POINT('Ctrl Pts',(-10.6917769267933,23.1504174308258,
2.54680467250241));
#103367=CARTESIAN_POINT('Ctrl Pts',(-10.6824684976073,23.1496508062632,
2.54012663008854));
#103368=CARTESIAN_POINT('Ctrl Pts',(-10.6783813325898,23.1493147390655,
2.53723372371194));
#103369=CARTESIAN_POINT('Ctrl Pts',(-10.6697418558365,23.1486054270809,
2.53120100633172));
#103370=CARTESIAN_POINT('Ctrl Pts',(-10.6651856405615,23.148231972833,2.52806702629443));
#103371=CARTESIAN_POINT('Ctrl Pts',(-10.6530706276395,23.1472404753333,
2.51985883693834));
#103372=CARTESIAN_POINT('Ctrl Pts',(-10.645474900742,23.1466203853548,2.51484006952346));
#103373=CARTESIAN_POINT('Ctrl Pts',(-10.6087730332824,23.1436308618374,
2.49119650600975));
#103374=CARTESIAN_POINT('Ctrl Pts',(-10.5789175299784,23.141218240841,2.47377236303456));
#103375=CARTESIAN_POINT('Ctrl Pts',(-10.4896128637742,23.1340512337476,
2.42679080178953));
#103376=CARTESIAN_POINT('Ctrl Pts',(-10.4283836229475,23.1291913554873,
2.40091657292208));
#103377=CARTESIAN_POINT('Ctrl Pts',(-10.3063869741341,23.1197684535021,
2.36111303167791));
#103378=CARTESIAN_POINT('Ctrl Pts',(-10.2460326994818,23.1152235226079,
2.34656773979351));
#103379=CARTESIAN_POINT('Ctrl Pts',(-10.1751812292,23.110196423447,2.33531050179874));
#103380=CARTESIAN_POINT('Ctrl Pts',(-10.1655347545678,23.1095186048482,
2.33390036841459));
#103381=CARTESIAN_POINT('Ctrl Pts',(-10.1522039590012,23.1085920222282,
2.3321204222968));
#103382=CARTESIAN_POINT('Ctrl Pts',(-10.1485340689348,23.1083379943824,
2.33164800490259));
#103383=CARTESIAN_POINT('Ctrl Pts',(-10.1422371049742,23.1079039990078,
2.33086755920325));
#103384=CARTESIAN_POINT('Ctrl Pts',(-10.1396111366587,23.1077235726613,
2.33055107463824));
#103385=CARTESIAN_POINT('Ctrl Pts',(-10.1341252215403,23.1073478415379,
2.32990864772608));
#103386=CARTESIAN_POINT('Ctrl Pts',(-10.131265117865,23.1071526353949,2.32958434016285));
#103387=CARTESIAN_POINT('Ctrl Pts',(-10.1242800923387,23.1066775035493,
2.32881823318869));
#103388=CARTESIAN_POINT('Ctrl Pts',(-10.120153917095,23.1063982000543,2.32838773061533));
#103389=CARTESIAN_POINT('Ctrl Pts',(-10.1052967516266,23.1053971397262,
2.32691692955242));
#103390=CARTESIAN_POINT('Ctrl Pts',(-10.094553477483,23.1046819542787,2.32600214805739));
#103391=CARTESIAN_POINT('Ctrl Pts',(-10.0676889442456,23.1029118413972,
2.32408583909969));
#103392=CARTESIAN_POINT('Ctrl Pts',(-10.051556412582,23.1018652539019,2.32326812836946));
#103393=CARTESIAN_POINT('Ctrl Pts',(-9.98071044339814,23.0973211958324,
2.32113704265959));
#103394=CARTESIAN_POINT('Ctrl Pts',(-9.92595690401097,23.0939430271003,
2.32330610220372));
#103395=CARTESIAN_POINT('Ctrl Pts',(-9.85132243203161,23.0893017531441,
2.33149493546198));
#103396=CARTESIAN_POINT('Ctrl Pts',(-9.83116744989325,23.088044978322,2.33423681635998));
#103397=CARTESIAN_POINT('Ctrl Pts',(-9.8111040637107,23.0867835801461,2.3374969300026));
#103398=CARTESIAN_POINT('',(-9.81115948034543,22.9869737331824,2.33748792667061));
#103399=CARTESIAN_POINT('Ctrl Pts',(-9.8111040637108,22.9869701371802,2.33749693000258));
#103400=CARTESIAN_POINT('Ctrl Pts',(-9.81112581929086,22.9869715488987,
2.33749339492317));
#103401=CARTESIAN_POINT('Ctrl Pts',(-9.81113772457216,22.986972321436,2.33749146071695));
#103402=CARTESIAN_POINT('Ctrl Pts',(-9.81115948034541,22.9869737331824,
2.33748792667061));
#103403=CARTESIAN_POINT('Ctrl Pts',(-9.81115948034545,22.9869737331824,
2.33748792667061));
#103404=CARTESIAN_POINT('Ctrl Pts',(-9.82933045015929,22.9881528593244,
2.33453620215867));
#103405=CARTESIAN_POINT('Ctrl Pts',(-9.84755744172139,22.9893419534045,
2.33201234132762));
#103406=CARTESIAN_POINT('Ctrl Pts',(-9.87752473866595,22.9913121344289,
2.32857647474011));
#103407=CARTESIAN_POINT('Ctrl Pts',(-9.88922322805877,22.992084996478,2.32741236746751));
#103408=CARTESIAN_POINT('Ctrl Pts',(-9.90664980367938,22.9932427720667,
2.32594136700875));
#103409=CARTESIAN_POINT('Ctrl Pts',(-9.9123661130932,22.9936235825559,2.32550085875634));
#103410=CARTESIAN_POINT('Ctrl Pts',(-9.92278582165,22.9943197186435,2.32477438965723));
#103411=CARTESIAN_POINT('Ctrl Pts',(-9.9274881808665,22.9946346197485,2.32447488349496));
#103412=CARTESIAN_POINT('Ctrl Pts',(-9.93667333437253,22.9952512190345,
2.32394517828075));
#103413=CARTESIAN_POINT('Ctrl Pts',(-9.94115590195987,22.995552830928,2.32371237299893));
#103414=CARTESIAN_POINT('Ctrl Pts',(-9.95142206249744,22.9962452442893,
2.32323802138882));
#103415=CARTESIAN_POINT('Ctrl Pts',(-9.95720628667639,22.9966365661914,
2.32301348081542));
#103416=CARTESIAN_POINT('Ctrl Pts',(-9.97301063543375,22.9977091739265,
2.32251661917644));
#103417=CARTESIAN_POINT('Ctrl Pts',(-9.98303276112712,22.9983930800217,
2.32232957076422));
#103418=CARTESIAN_POINT('Ctrl Pts',(-10.0273602127523,23.0014352152979,
2.32206820417229));
#103419=CARTESIAN_POINT('Ctrl Pts',(-10.0616537382153,23.0038351055056,
2.32336484021042));
#103420=CARTESIAN_POINT('Ctrl Pts',(-10.1454009295848,23.009812264309,2.33020241317789));
#103421=CARTESIAN_POINT('Ctrl Pts',(-10.1946523792398,23.0134293086955,
2.33738336818735));
#103422=CARTESIAN_POINT('Ctrl Pts',(-10.3162493957474,23.0225409881098,
2.36305652239483));
#103423=CARTESIAN_POINT('Ctrl Pts',(-10.3875780628195,23.028057242111,2.38535249724469));
#103424=CARTESIAN_POINT('Ctrl Pts',(-10.4671228361506,23.0341257659899,
2.41878376866579));
#103425=CARTESIAN_POINT('Ctrl Pts',(-10.477854160598,23.0349423355658,2.42348352988791));
#103426=CARTESIAN_POINT('Ctrl Pts',(-10.4924121273541,23.0360454522139,
2.43011976763798));
#103427=CARTESIAN_POINT('Ctrl Pts',(-10.4963005318373,23.0363396355962,
2.43191798147123));
#103428=CARTESIAN_POINT('Ctrl Pts',(-10.5028088618272,23.0368311599454,
2.43497101057247));
#103429=CARTESIAN_POINT('Ctrl Pts',(-10.5054340833018,23.0370291827564,
2.43621435998972));
#103430=CARTESIAN_POINT('Ctrl Pts',(-10.5104150897067,23.0374044106437,
2.43859605060154));
#103431=CARTESIAN_POINT('Ctrl Pts',(-10.5127717160224,23.0375817299307,
2.43973254544482));
#103432=CARTESIAN_POINT('Ctrl Pts',(-10.5183548048173,23.0380013657455,
2.44244798634289));
#103433=CARTESIAN_POINT('Ctrl Pts',(-10.5215778931791,23.0382432599517,
2.44403387011638));
#103434=CARTESIAN_POINT('Ctrl Pts',(-10.5328959441981,23.0390915942668,
2.44966725075774));
#103435=CARTESIAN_POINT('Ctrl Pts',(-10.5409517118907,23.0396934361345,
2.4537934098937));
#103436=CARTESIAN_POINT('Ctrl Pts',(-10.6206501318649,23.0456359398445,
2.4957816144695));
#103437=CARTESIAN_POINT('Ctrl Pts',(-10.6882627972059,23.0505922381058,
2.54085482699908));
#103438=CARTESIAN_POINT('Ctrl Pts',(-10.7849351010806,23.0583519991997,
2.62082765707672));
#103439=CARTESIAN_POINT('Ctrl Pts',(-10.8175223657971,23.0611071263157,
2.65104536660552));
#103440=CARTESIAN_POINT('Ctrl Pts',(-10.8657156269797,23.0655092936261,
2.70108817750477));
#103441=CARTESIAN_POINT('Ctrl Pts',(-10.8825250043757,23.0671149856522,
2.71969676622847));
#103442=CARTESIAN_POINT('Ctrl Pts',(-10.906451667302,23.0695200132337,2.74794728007398));
#103443=CARTESIAN_POINT('Ctrl Pts',(-10.9140368210976,23.0703014909455,
2.75718468510322));
#103444=CARTESIAN_POINT('Ctrl Pts',(-10.9275612562168,23.0717313780518,
2.77417596086155));
#103445=CARTESIAN_POINT('Ctrl Pts',(-10.9335472333948,23.0723779169368,
2.78189139164954));
#103446=CARTESIAN_POINT('Ctrl Pts',(-10.9428226510478,23.0734021040643,
2.79415863382085));
#103447=CARTESIAN_POINT('Ctrl Pts',(-10.9461767501791,23.0737772316565,
2.79866117952385));
#103448=CARTESIAN_POINT('Ctrl Pts',(-10.9495588799937,23.0741604490122,
2.80326977505809));
#103449=CARTESIAN_POINT('Ctrl Pts',(-10.9496192707213,23.0741672932999,
2.80335208778239));
#103450=CARTESIAN_POINT('Ctrl Pts',(-10.9497446767683,23.0741815093713,
2.80352306316844));
#103451=CARTESIAN_POINT('Ctrl Pts',(-10.9498096903923,23.0741888812225,
2.80361172710556));
#103452=CARTESIAN_POINT('Ctrl Pts',(-10.9499146882163,23.0742007899018,
2.80375496253993));
#103453=CARTESIAN_POINT('Ctrl Pts',(-10.9499546801361,23.0742053264332,
2.8038095283873));
#103454=CARTESIAN_POINT('Ctrl Pts',(-10.9500515661709,23.0742163185477,
2.80394174569729));
#103455=CARTESIAN_POINT('Ctrl Pts',(-10.9501084554518,23.0742227743144,
2.80401940066855));
#103456=CARTESIAN_POINT('Ctrl Pts',(-10.9502461107579,23.0742383988704,
2.80420735116147));
#103457=CARTESIAN_POINT('Ctrl Pts',(-10.9503268670896,23.0742475680309,
2.80431765375577));
#103458=CARTESIAN_POINT('Ctrl Pts',(-10.9507991597674,23.0743012097293,
2.80496297952106));
#103459=CARTESIAN_POINT('Ctrl Pts',(-10.9511902628288,23.0743456988309,
2.80549831825458));
#103460=CARTESIAN_POINT('Ctrl Pts',(-10.9545578418995,23.0747293642029,
2.81011601408111));
#103461=CARTESIAN_POINT('Ctrl Pts',(-10.9575084330614,23.0750695258186,
2.81421709936473));
#103462=CARTESIAN_POINT('Ctrl Pts',(-10.9642839489682,23.075860080017,2.82376349635286));
#103463=CARTESIAN_POINT('Ctrl Pts',(-10.9680892613445,23.0763112033964,
2.82922244968103));
#103464=CARTESIAN_POINT('Ctrl Pts',(-10.9803604777621,23.0777897166042,
2.84714819049596));
#103465=CARTESIAN_POINT('Ctrl Pts',(-10.9886331075552,23.0788242487294,
2.85974482155988));
#103466=CARTESIAN_POINT('Ctrl Pts',(-11.0401538772754,23.0855197383915,
2.94157502954212));
#103467=CARTESIAN_POINT('Ctrl Pts',(-11.0763389402264,23.0914354698669,
3.01497586133421));
#103468=CARTESIAN_POINT('Ctrl Pts',(-11.1234775660357,23.1014102870791,
3.14244919016272));
#103469=CARTESIAN_POINT('Ctrl Pts',(-11.1387687755876,23.1054106472644,
3.19463026933931));
#103470=CARTESIAN_POINT('Ctrl Pts',(-11.1538499245659,23.1104574535629,
3.26339056072969));
#103471=CARTESIAN_POINT('Ctrl Pts',(-11.1569732609394,23.1116002663262,
3.27916838279357));
#103472=CARTESIAN_POINT('Ctrl Pts',(-11.161643031155,23.1134834758004,3.30558804476212));
#103473=CARTESIAN_POINT('Ctrl Pts',(-11.1633686095288,23.1142314795262,
3.31619565002432));
#103474=CARTESIAN_POINT('Ctrl Pts',(-11.1655579064777,23.1152574471973,
3.33092313036986));
#103475=CARTESIAN_POINT('Ctrl Pts',(-11.1661453747261,23.1155417619797,
3.33502367591212));
#103476=CARTESIAN_POINT('Ctrl Pts',(-11.1671041127655,23.1160214930971,
3.34197681654123));
#103477=CARTESIAN_POINT('Ctrl Pts',(-11.1674865852185,23.1162175220266,
3.34482780353112));
#103478=CARTESIAN_POINT('Ctrl Pts',(-11.1682007026767,23.1165926620113,
3.35030304949369));
#103479=CARTESIAN_POINT('Ctrl Pts',(-11.1685339561704,23.116771865454,3.35292705090696));
#103480=CARTESIAN_POINT('Ctrl Pts',(-11.1693124900505,23.1172007582149,
3.35922687515752));
#103481=CARTESIAN_POINT('Ctrl Pts',(-11.1697492853397,23.1174499806069,
3.36290374754294));
#103482=CARTESIAN_POINT('Ctrl Pts',(-11.1712760585983,23.1183538333206,
3.37629468020565));
#103483=CARTESIAN_POINT('Ctrl Pts',(-11.1722624688999,23.1190030295047,
3.38602048015204));
#103484=CARTESIAN_POINT('Ctrl Pts',(-11.1784705570504,23.1236216894576,
3.45588548354031));
#103485=CARTESIAN_POINT('Ctrl Pts',(-11.1791835156877,23.1273831383303,
3.51634328370099));
#103486=CARTESIAN_POINT('Ctrl Pts',(-11.1708637312362,23.1353046675188,
3.64399862292482));
#103487=CARTESIAN_POINT('Ctrl Pts',(-11.1606809909735,23.1394482905764,
3.7108945379637));
#103488=CARTESIAN_POINT('Ctrl Pts',(-11.1366284329172,23.1459590772207,
3.81046480039585));
#103489=CARTESIAN_POINT('Ctrl Pts',(-11.1269326789683,23.1482116676388,
3.84399848368288));
#103490=CARTESIAN_POINT('Ctrl Pts',(-11.1128407269703,23.1511144503027,
3.88569927459808));
#103491=CARTESIAN_POINT('Ctrl Pts',(-11.1098175015094,23.1517196634186,
3.89431398606395));
#103492=CARTESIAN_POINT('Ctrl Pts',(-11.1048012336015,23.1526970374537,
3.90809303711878));
#103493=CARTESIAN_POINT('Ctrl Pts',(-11.1028713642119,23.1530671130495,
3.91328010469405));
#103494=CARTESIAN_POINT('Ctrl Pts',(-11.0991270511796,23.1537741234056,
3.92313098420012));
#103495=CARTESIAN_POINT('Ctrl Pts',(-11.0973192969696,23.1541108296978,
3.92779722251508));
#103496=CARTESIAN_POINT('Ctrl Pts',(-11.0931191626544,23.1548827778113,
3.93843695559237));
#103497=CARTESIAN_POINT('Ctrl Pts',(-11.0907074721916,23.1553186564355,
3.94440260467422));
#103498=CARTESIAN_POINT('Ctrl Pts',(-11.0830934677002,23.1566726173322,
3.96280152357305));
#103499=CARTESIAN_POINT('Ctrl Pts',(-11.0777266850735,23.157596182324,3.9751651039506));
#103500=CARTESIAN_POINT('Ctrl Pts',(-11.0300216796261,23.1655560583394,
4.08009610726531));
#103501=CARTESIAN_POINT('Ctrl Pts',(-10.9760667377985,23.1730126849874,
4.16688925384512));
#103502=CARTESIAN_POINT('Ctrl Pts',(-10.8750602016379,23.1847159812735,
4.29038261986591));
#103503=CARTESIAN_POINT('Ctrl Pts',(-10.8352233383987,23.1889292672099,
4.33236927401729));
#103504=CARTESIAN_POINT('Ctrl Pts',(-10.7871195674739,23.1934557690624,
4.37612211592631));
#103505=CARTESIAN_POINT('Ctrl Pts',(-10.7817344968149,23.1939551916662,
4.38093039370179));
#103506=CARTESIAN_POINT('Ctrl Pts',(-10.7736498893391,23.1946937439817,
4.38801654283783));
#103507=CARTESIAN_POINT('Ctrl Pts',(-10.770983891727,23.1949355007695,4.39033216899616));
#103508=CARTESIAN_POINT('Ctrl Pts',(-10.7663956429986,23.1953484534316,
4.39428135607766));
#103509=CARTESIAN_POINT('Ctrl Pts',(-10.7644785193549,23.1955200722671,
4.39592076620813));
#103510=CARTESIAN_POINT('Ctrl Pts',(-10.7601120430664,23.1959088463342,
4.3996304960616));
#103511=CARTESIAN_POINT('Ctrl Pts',(-10.7576594925098,23.1961257230802,
4.40169697875158));
#103512=CARTESIAN_POINT('Ctrl Pts',(-10.7509642206263,23.1967138405205,
4.40729171175524));
#103513=CARTESIAN_POINT('Ctrl Pts',(-10.7467050294985,23.1970836993063,
4.41080025953542));
#103514=CARTESIAN_POINT('Ctrl Pts',(-10.7254365992137,23.1989104231113,
4.42807084894456));
#103515=CARTESIAN_POINT('Ctrl Pts',(-10.7080696048275,23.2003385461329,
4.44138798754538));
#103516=CARTESIAN_POINT('Ctrl Pts',(-10.6724560469037,23.2031649719364,
4.46715313371203));
#103517=CARTESIAN_POINT('Ctrl Pts',(-10.6542106184531,23.2045623330808,
4.47958709829406));
#103518=CARTESIAN_POINT('Ctrl Pts',(-10.5519067878126,23.2121854605729,
4.54517140559674));
#103519=CARTESIAN_POINT('Ctrl Pts',(-10.4617311208844,23.2181749113842,
4.58802078615555));
#103520=CARTESIAN_POINT('Ctrl Pts',(-10.3410113574056,23.2263174644757,
4.62763844376149));
#103521=CARTESIAN_POINT('Ctrl Pts',(-10.3144881075835,23.2281107016962,
4.63532120753413));
#103522=CARTESIAN_POINT('Ctrl Pts',(-10.2795252391042,23.2304921148332,
4.64412942324497));
#103523=CARTESIAN_POINT('Ctrl Pts',(-10.2713076620247,23.2310530598692,
4.64610586019299));
#103524=CARTESIAN_POINT('Ctrl Pts',(-10.2578194845839,23.2319761064925,
4.64919675779049));
#103525=CARTESIAN_POINT('Ctrl Pts',(-10.2525611540561,23.232336527722,4.65036382791168));
#103526=CARTESIAN_POINT('Ctrl Pts',(-10.2423568635783,23.2330371552342,
4.65255530186122));
#103527=CARTESIAN_POINT('Ctrl Pts',(-10.2374119472146,23.2333772154745,
4.65358404077084));
#103528=CARTESIAN_POINT('Ctrl Pts',(-10.2259455980152,23.2341670796585,
4.65589264878858));
#103529=CARTESIAN_POINT('Ctrl Pts',(-10.219419696762,23.2346176104722,4.65714917893545));
#103530=CARTESIAN_POINT('Ctrl Pts',(-10.1981106318597,23.2360921595994,
4.66106539550293));
#103531=CARTESIAN_POINT('Ctrl Pts',(-10.1832876786367,23.2371232671596,
4.66349742829467));
#103532=CARTESIAN_POINT('Ctrl Pts',(-10.0873648709804,23.2438334923351,
4.67735721332051));
#103533=CARTESIAN_POINT('Ctrl Pts',(-10.0053209671194,23.24976935697,4.68058022344533));
#103534=CARTESIAN_POINT('Ctrl Pts',(-9.86958271485929,23.2597528662967,
4.67175892140751));
#103535=CARTESIAN_POINT('Ctrl Pts',(-9.81584746281155,23.2637415001055,
4.66452396072934));
#103536=CARTESIAN_POINT('Ctrl Pts',(-9.74707148462057,23.268775173617,4.65038255837818));
#103537=CARTESIAN_POINT('Ctrl Pts',(-9.73141120675879,23.2699161468259,
4.64682735359267));
#103538=CARTESIAN_POINT('Ctrl Pts',(-9.70541135519511,23.271796655567,4.64036301286977));
#103539=CARTESIAN_POINT('Ctrl Pts',(-9.69503039103909,23.2725437718774,
4.63763079636926));
#103540=CARTESIAN_POINT('Ctrl Pts',(-9.68069851937139,23.2735687356609,
4.63364843312371));
#103541=CARTESIAN_POINT('Ctrl Pts',(-9.67671505394268,23.2738529180562,
4.63251889627262));
#103542=CARTESIAN_POINT('Ctrl Pts',(-9.66997472093026,23.2743324917589,
4.63056917064355));
#103543=CARTESIAN_POINT('Ctrl Pts',(-9.66721477364654,23.2745284947388,
4.6297598542318));
#103544=CARTESIAN_POINT('Ctrl Pts',(-9.66192192844809,23.2749036371779,
4.62818672148005));
#103545=CARTESIAN_POINT('Ctrl Pts',(-9.65938861374635,23.2750828687189,
4.62742447414259));
#103546=CARTESIAN_POINT('Ctrl Pts',(-9.65331431013368,23.2755118970093,
4.62557443842932));
#103547=CARTESIAN_POINT('Ctrl Pts',(-9.64977581489861,23.2757612261753,
4.62447845915314));
#103548=CARTESIAN_POINT('Ctrl Pts',(-9.63690677944093,23.2766660344139,
4.62042588963239));
#103549=CARTESIAN_POINT('Ctrl Pts',(-9.62760770321934,23.2773160638543,
4.61736961372478));
#103550=CARTESIAN_POINT('Ctrl Pts',(-9.56146693430513,23.2819196437725,
4.59471403376653));
#103551=CARTESIAN_POINT('Ctrl Pts',(-9.50615404050545,23.2856669362543,
4.57090061935014));
#103552=CARTESIAN_POINT('Ctrl Pts',(-9.39293194450838,23.2935845140801,
4.51150806525642));
#103553=CARTESIAN_POINT('Ctrl Pts',(-9.33579561405133,23.2977378838956,
4.47494210889107));
#103554=CARTESIAN_POINT('Ctrl Pts',(-9.25441931212821,23.3042620349929,
4.41237346487831));
#103555=CARTESIAN_POINT('Ctrl Pts',(-9.22768379963132,23.3065176016736,
4.38985572972593));
#103556=CARTESIAN_POINT('Ctrl Pts',(-9.19527308581868,23.3094237434334,
4.35999597565929));
#103557=CARTESIAN_POINT('Ctrl Pts',(-9.18862811796076,23.3100292086062,
4.35372955074626));
#103558=CARTESIAN_POINT('Ctrl Pts',(-9.17807422803848,23.311006892302,4.34354236850563));
#103559=CARTESIAN_POINT('Ctrl Pts',(-9.1741188085816,23.3113770230975,4.33967014830915));
#103560=CARTESIAN_POINT('Ctrl Pts',(-9.16663988786045,23.3120840749315,
4.33224457101203));
#103561=CARTESIAN_POINT('Ctrl Pts',(-9.16311144050307,23.3124207670553,
4.32869634977843));
#103562=CARTESIAN_POINT('Ctrl Pts',(-9.15509875806343,23.3131925920681,
4.32053539758769));
#103563=CARTESIAN_POINT('Ctrl Pts',(-9.15062952340823,23.3136283610314,
4.31590822888441));
#103564=CARTESIAN_POINT('Ctrl Pts',(-9.13692071714168,23.314981638236,4.30148027813739));
#103565=CARTESIAN_POINT('Ctrl Pts',(-9.12781147823395,23.3159046212112,
4.29155773069694));
#103566=CARTESIAN_POINT('Ctrl Pts',(-9.05129066452536,23.3238682733305,
4.20528003479912));
#103567=CARTESIAN_POINT('Ctrl Pts',(-8.99388978077641,23.331329879206,4.12064719507611));
#103568=CARTESIAN_POINT('Ctrl Pts',(-8.92212701591141,23.3430341715243,
3.97814136760841));
#103569=CARTESIAN_POINT('Ctrl Pts',(-8.89998073013925,23.3472436999236,
3.92472171097933));
#103570=CARTESIAN_POINT('Ctrl Pts',(-8.87957469040795,23.3517666476949,
3.86303482016365));
#103571=CARTESIAN_POINT('Ctrl Pts',(-8.87737090427838,23.3522659706824,
3.85616158552503));
#103572=CARTESIAN_POINT('Ctrl Pts',(-8.87418327210011,23.3530044050559,
3.845896263104));
#103573=CARTESIAN_POINT('Ctrl Pts',(-8.87315132052637,23.353246142325,3.84251946519972));
#103574=CARTESIAN_POINT('Ctrl Pts',(-8.87140820260761,23.3536590732679,
3.83672240812784));
#103575=CARTESIAN_POINT('Ctrl Pts',(-8.87068961010261,23.3538306897738,
3.83430445553303));
#103576=CARTESIAN_POINT('Ctrl Pts',(-8.86907499450222,23.3542194743091,
3.82880690477619));
#103577=CARTESIAN_POINT('Ctrl Pts',(-8.86818377872898,23.3544363637547,
3.82572594397406));
#103578=CARTESIAN_POINT('Ctrl Pts',(-8.86579327630545,23.3550245493437,
3.81733362252417));
#103579=CARTESIAN_POINT('Ctrl Pts',(-8.86431869541627,23.3553944630465,
3.812015219895));
#103580=CARTESIAN_POINT('Ctrl Pts',(-8.85718159024956,23.3572218993939,
3.78555258239075));
#103581=CARTESIAN_POINT('Ctrl Pts',(-8.8520715005743,23.3586506532497,3.76426218723496));
#103582=CARTESIAN_POINT('Ctrl Pts',(-8.84300645704952,23.3614775551634,
3.72124235529943));
#103583=CARTESIAN_POINT('Ctrl Pts',(-8.83906323058472,23.3628747843244,
3.69951980591548));
#103584=CARTESIAN_POINT('Ctrl Pts',(-8.8207261347638,23.3704987079885,3.57937635004485));
#103585=CARTESIAN_POINT('Ctrl Pts',(-8.81823442504374,23.3764890921039,
3.4795532868496));
#103586=CARTESIAN_POINT('Ctrl Pts',(-8.83111435099077,23.3846315207775,
3.35315856518573));
#103587=CARTESIAN_POINT('Ctrl Pts',(-8.83487414616044,23.3864234507394,
3.32582301841254));
#103588=CARTESIAN_POINT('Ctrl Pts',(-8.84103443793159,23.3888033700423,
3.29032099429569));
#103589=CARTESIAN_POINT('Ctrl Pts',(-8.84256855366958,23.3893641722794,
3.28201169674781));
#103590=CARTESIAN_POINT('Ctrl Pts',(-8.84522668774398,23.3902870440368,
3.26843431396956));
#103591=CARTESIAN_POINT('Ctrl Pts',(-8.84629769129515,23.3906474344519,
3.26315606215587));
#103592=CARTESIAN_POINT('Ctrl Pts',(-8.84844320053769,23.3913480450722,
3.25294228852423));
#103593=CARTESIAN_POINT('Ctrl Pts',(-8.84951333011119,23.3916881195162,
3.24800595994144));
#103594=CARTESIAN_POINT('Ctrl Pts',(-8.85206518646545,23.3924780801647,
3.23658984714381));
#103595=CARTESIAN_POINT('Ctrl Pts',(-8.85357007075657,23.3929286937872,
3.23011547110349));
#103596=CARTESIAN_POINT('Ctrl Pts',(-8.85865562653411,23.3944037960693,
3.20904656398069));
#103597=CARTESIAN_POINT('Ctrl Pts',(-8.8624607037958,23.3954353813628,3.19450827504879));
#103598=CARTESIAN_POINT('Ctrl Pts',(-8.8887266483475,23.4021295051825,3.10145911988546));
#103599=CARTESIAN_POINT('Ctrl Pts',(-8.91901963041153,23.4080471221999,
3.02540530811363));
#103600=CARTESIAN_POINT('Ctrl Pts',(-8.98924242682943,23.4191460779312,
2.8914707554874));
#103601=CARTESIAN_POINT('Ctrl Pts',(-9.02696224635812,23.4242793743449,
2.83281345055004));
#103602=CARTESIAN_POINT('Ctrl Pts',(-9.07662172037985,23.4299714584954,
2.76883853567892));
#103603=CARTESIAN_POINT('Ctrl Pts',(-9.08372905434086,23.430764245782,2.75995127693934));
#103604=CARTESIAN_POINT('Ctrl Pts',(-9.09365768594777,23.4318406940891,
2.74789853372323));
#103605=CARTESIAN_POINT('Ctrl Pts',(-9.0963686448159,23.4321315331021,2.74464354034595));
#103606=CARTESIAN_POINT('Ctrl Pts',(-9.10096181598024,23.4326190485995,
2.73918873108227));
#103607=CARTESIAN_POINT('Ctrl Pts',(-9.10283466559849,23.4328163833394,
2.73698112302647));
#103608=CARTESIAN_POINT('Ctrl Pts',(-9.10642145665841,23.4331915239221,
2.73278468344091));
#103609=CARTESIAN_POINT('Ctrl Pts',(-9.10813393017699,23.4333694367857,
2.73079465100173));
#103610=CARTESIAN_POINT('Ctrl Pts',(-9.11222835799636,23.4337920308252,
2.72606865097102));
#103611=CARTESIAN_POINT('Ctrl Pts',(-9.1146163441647,23.4340362754754,2.72333790860702));
#103612=CARTESIAN_POINT('Ctrl Pts',(-9.12314542351985,23.4349009582636,
2.71367508032983));
#103613=CARTESIAN_POINT('Ctrl Pts',(-9.12935581397608,23.4355165638523,
2.70680422210237));
#103614=CARTESIAN_POINT('Ctrl Pts',(-9.18792819945987,23.4412018654453,
2.64351962941284));
#103615=CARTESIAN_POINT('Ctrl Pts',(-9.24562909126624,23.4459266187752,
2.59228458586582));
#103616=CARTESIAN_POINT('Ctrl Pts',(-9.37417809794799,23.4557485472166,
2.49892732677693));
#103617=CARTESIAN_POINT('Ctrl Pts',(-9.44525788318716,23.4608319106327,
2.45785880602235));
#103618=CARTESIAN_POINT('Ctrl Pts',(-9.530797020055,23.4669757749784,2.41968384768958));
#103619=CARTESIAN_POINT('Ctrl Pts',(-9.54164876213505,23.4677552195766,
2.41503523026823));
#103620=CARTESIAN_POINT('Ctrl Pts',(-9.5582154395472,23.4689460590446,2.40823137312488));
#103621=CARTESIAN_POINT('Ctrl Pts',(-9.56388050004409,23.4693534301441,
2.405956074068));
#103622=CARTESIAN_POINT('Ctrl Pts',(-9.57374709562373,23.4700633211342,
2.40208209302186));
#103623=CARTESIAN_POINT('Ctrl Pts',(-9.5779406068059,23.4703651610101,2.40046321725575));
#103624=CARTESIAN_POINT('Ctrl Pts',(-9.5873603871918,23.471043501198,2.39688860455902));
#103625=CARTESIAN_POINT('Ctrl Pts',(-9.59259146604538,23.4714204262742,
2.39494593552422));
#103626=CARTESIAN_POINT('Ctrl Pts',(-9.60661313880329,23.4724314587763,
2.38985179146799));
#103627=CARTESIAN_POINT('Ctrl Pts',(-9.61542758890321,23.4730677604288,
2.38676762563264));
#103628=CARTESIAN_POINT('Ctrl Pts',(-9.65570011603182,23.475978981281,2.37321168722426));
#103629=CARTESIAN_POINT('Ctrl Pts',(-9.68755228883306,23.4782931822013,
2.36396727032804));
#103630=CARTESIAN_POINT('Ctrl Pts',(-9.74996777618204,23.4828532652028,
2.34867601877673));
#103631=CARTESIAN_POINT('Ctrl Pts',(-9.78044374222133,23.4850911448363,
2.34247894706917));
#103632=CARTESIAN_POINT('Ctrl Pts',(-9.81110406371068,23.4873487054734,
2.3374969300026));
#103633=CARTESIAN_POINT('Origin',(-10.,12.3756328852638,3.5));
#103634=CARTESIAN_POINT('',(-9.81110406371068,24.0873412831715,2.3374969300026));
#103635=CARTESIAN_POINT('',(-9.81110406371069,23.9889087884094,2.3374969300026));
#103636=CARTESIAN_POINT('',(-9.81110406371068,12.3756328852638,2.3374969300026));
#103637=CARTESIAN_POINT('Ctrl Pts',(-9.81110406371069,24.0873412831715,
2.3374969300026));
#103638=CARTESIAN_POINT('Ctrl Pts',(-9.74357372492119,24.0824554593664,
2.34846998194783));
#103639=CARTESIAN_POINT('Ctrl Pts',(-9.67707560096892,24.0774182711905,
2.3653149679055));
#103640=CARTESIAN_POINT('Ctrl Pts',(-9.55774576776678,24.0681478523538,
2.40690680585405));
#103641=CARTESIAN_POINT('Ctrl Pts',(-9.50459022776225,24.063930227775,2.42994752981934));
#103642=CARTESIAN_POINT('Ctrl Pts',(-9.44694158882869,24.0593995462754,
2.46015692936817));
#103643=CARTESIAN_POINT('Ctrl Pts',(-9.44057557513891,24.0588999157289,
2.46356788108037));
#103644=CARTESIAN_POINT('Ctrl Pts',(-9.43114311266536,24.058161080565,2.46873408803481));
#103645=CARTESIAN_POINT('Ctrl Pts',(-9.4280526795725,24.057919246332,2.47044485192393));
#103646=CARTESIAN_POINT('Ctrl Pts',(-9.42276799924539,24.0575061730287,
2.4734014192899));
#103647=CARTESIAN_POINT('Ctrl Pts',(-9.42057001289399,24.057334510611,2.47464039522845));
#103648=CARTESIAN_POINT('Ctrl Pts',(-9.41558679633419,24.0569456536593,
2.47747050970815));
#103649=CARTESIAN_POINT('Ctrl Pts',(-9.41280407413561,24.0567287376857,
2.47906596863196));
#103650=CARTESIAN_POINT('Ctrl Pts',(-9.40525148582439,24.0561405330082,
2.48343729971027));
#103651=CARTESIAN_POINT('Ctrl Pts',(-9.40049448221763,24.0557706267073,
2.48623540412376));
#103652=CARTESIAN_POINT('Ctrl Pts',(-9.37697719181959,24.0539438723636,
2.50029187668128));
#103653=CARTESIAN_POINT('Ctrl Pts',(-9.35851213514121,24.0525157692467,
2.51203885762965));
#103654=CARTESIAN_POINT('Ctrl Pts',(-9.32209675321034,24.0496893842896,
2.53665712168377));
#103655=CARTESIAN_POINT('Ctrl Pts',(-9.30416001060986,24.0482920442572,
2.5495321574285));
#103656=CARTESIAN_POINT('Ctrl Pts',(-9.20742490449701,24.0406654568903,
2.62317599148236));
#103657=CARTESIAN_POINT('Ctrl Pts',(-9.13621433393267,24.0346728069635,
2.69323458384475));
#103658=CARTESIAN_POINT('Ctrl Pts',(-9.05760909087374,24.0265292441198,
2.79306718509312));
#103659=CARTESIAN_POINT('Ctrl Pts',(-9.04132611092989,24.0247389821614,
2.81531115529514));
#103660=CARTESIAN_POINT('Ctrl Pts',(-9.02109139216019,24.0223608932655,
2.8450920909953));
#103661=CARTESIAN_POINT('Ctrl Pts',(-9.01641902406435,24.0218002003561,
2.85213049973338));
#103662=CARTESIAN_POINT('Ctrl Pts',(-9.0088923746425,24.0208774118868,2.86373767280989));
#103663=CARTESIAN_POINT('Ctrl Pts',(-9.00599294943121,24.0205169943684,
2.86827691523815));
#103664=CARTESIAN_POINT('Ctrl Pts',(-9.00043433634345,24.0198162614892,
2.87711231068603));
#103665=CARTESIAN_POINT('Ctrl Pts',(-8.99777145246276,24.019476091521,2.88140600828212));
#103666=CARTESIAN_POINT('Ctrl Pts',(-8.99166766671436,24.0186858055833,
2.89139076962594));
#103667=CARTESIAN_POINT('Ctrl Pts',(-8.98824720512307,24.0182349609094,
2.89709406326543));
#103668=CARTESIAN_POINT('Ctrl Pts',(-8.97724846161348,24.0167586368137,
2.91579061538641));
#103669=CARTESIAN_POINT('Ctrl Pts',(-8.96987102631648,24.0157260447666,
2.92889968003823));
#103670=CARTESIAN_POINT('Ctrl Pts',(-8.92429944104744,24.0090645634159,
3.01363378462953));
#103671=CARTESIAN_POINT('Ctrl Pts',(-8.89335218272255,24.0031839340262,
3.08889191535067));
#103672=CARTESIAN_POINT('Ctrl Pts',(-8.85491027822392,23.9932144415457,
3.21918512241161));
#103673=CARTESIAN_POINT('Ctrl Pts',(-8.84310383763222,23.9891841142858,
3.27266916464562));
#103674=CARTESIAN_POINT('Ctrl Pts',(-8.83268291164885,23.9841037123425,
3.34275311502857));
#103675=CARTESIAN_POINT('Ctrl Pts',(-8.83063673390186,23.982956156826,3.35877190580605));
#103676=CARTESIAN_POINT('Ctrl Pts',(-8.82777494406594,23.9810659550975,
3.38554624212253));
#103677=CARTESIAN_POINT('Ctrl Pts',(-8.82677650935534,23.9803156338232,
3.39627967330447));
#103678=CARTESIAN_POINT('Ctrl Pts',(-8.82559809730526,23.9792870091483,
3.41116060795672));
#103679=CARTESIAN_POINT('Ctrl Pts',(-8.82529250078572,23.9790023128278,
3.41529723006494));
#103680=CARTESIAN_POINT('Ctrl Pts',(-8.82481188669995,23.9785220947086,
3.42230673240159));
#103681=CARTESIAN_POINT('Ctrl Pts',(-8.82462553624673,23.9783259577827,
3.42517877234607));
#103682=CARTESIAN_POINT('Ctrl Pts',(-8.82428812759596,23.9779507093295,
3.43069161837056));
#103683=CARTESIAN_POINT('Ctrl Pts',(-8.82413543563939,23.9777715047626,
3.43333227685037));
#103684=CARTESIAN_POINT('Ctrl Pts',(-8.82379047927197,23.9773427681755,
3.43966826776755));
#103685=CARTESIAN_POINT('Ctrl Pts',(-8.82360672973643,23.9770937018829,
3.44336406470333));
#103686=CARTESIAN_POINT('Ctrl Pts',(-8.82300216036569,23.9761916952841,
3.45680043955325));
#103687=CARTESIAN_POINT('Ctrl Pts',(-8.82268486146288,23.9755441576955,
3.46654560823821));
#103688=CARTESIAN_POINT('Ctrl Pts',(-8.82125301953222,23.970859658916,3.53766721136896));
#103689=CARTESIAN_POINT('Ctrl Pts',(-8.82481745000881,23.9670381129837,
3.59905170948979));
#103690=CARTESIAN_POINT('Ctrl Pts',(-8.84222150143454,23.9591015964265,
3.72606693842428));
#103691=CARTESIAN_POINT('Ctrl Pts',(-8.85690332902964,23.9550012799187,
3.79135320048569));
#103692=CARTESIAN_POINT('Ctrl Pts',(-8.88749465769506,23.9485498270871,
3.88811057869496));
#103693=CARTESIAN_POINT('Ctrl Pts',(-8.89940476417073,23.9463104259834,
3.92069908932711));
#103694=CARTESIAN_POINT('Ctrl Pts',(-8.91623804203854,23.9434223797439,
3.96112705635159));
#103695=CARTESIAN_POINT('Ctrl Pts',(-8.91983917181495,23.9428181325545,
3.96950050175579));
#103696=CARTESIAN_POINT('Ctrl Pts',(-8.92578172920347,23.9418418486449,
3.98288795744225));
#103697=CARTESIAN_POINT('Ctrl Pts',(-8.92806198282407,23.9414718873023,
3.987928845543));
#103698=CARTESIAN_POINT('Ctrl Pts',(-8.93247342755905,23.9407647846526,
3.99750090624318));
#103699=CARTESIAN_POINT('Ctrl Pts',(-8.9345981692479,23.9404278698307,4.00203493133102));
#103700=CARTESIAN_POINT('Ctrl Pts',(-8.93952379797838,23.9396550011608,
4.01237371794138));
#103701=CARTESIAN_POINT('Ctrl Pts',(-8.9423435310397,23.9392184064738,4.01816927030507));
#103702=CARTESIAN_POINT('Ctrl Pts',(-8.95122711733754,23.9378605300416,
4.03605354949671));
#103703=CARTESIAN_POINT('Ctrl Pts',(-8.95745154596989,23.9369337221889,
4.04806081943611));
#103704=CARTESIAN_POINT('Ctrl Pts',(-9.0121022850983,23.9289953170451,4.14918390318014));
#103705=CARTESIAN_POINT('Ctrl Pts',(-9.07163837185019,23.9215669463448,
4.23179082672774));
#103706=CARTESIAN_POINT('Ctrl Pts',(-9.18071481933319,23.9098705686517,
4.34807872319119));
#103707=CARTESIAN_POINT('Ctrl Pts',(-9.22351534095563,23.9056371468017,
4.38743388824816));
#103708=CARTESIAN_POINT('Ctrl Pts',(-9.27471694161216,23.9010914306633,
4.42796109787714));
#103709=CARTESIAN_POINT('Ctrl Pts',(-9.28042619009648,23.9005913363944,
4.43239522340341));
#103710=CARTESIAN_POINT('Ctrl Pts',(-9.28898698730006,23.8998519253699,
4.43891855198856));
#103711=CARTESIAN_POINT('Ctrl Pts',(-9.29180756887576,23.8996099742054,
4.44104783768997));
#103712=CARTESIAN_POINT('Ctrl Pts',(-9.29665874937702,23.8991967460305,
4.44467587914371));
#103713=CARTESIAN_POINT('Ctrl Pts',(-9.29868462319215,23.8990250451092,
4.44618083586683));
#103714=CARTESIAN_POINT('Ctrl Pts',(-9.30329625533382,23.8986361598701,
4.44958372055939));
#103715=CARTESIAN_POINT('Ctrl Pts',(-9.30588493877044,23.8984192537893,
4.45147760487521));
#103716=CARTESIAN_POINT('Ctrl Pts',(-9.31294709335089,23.8978311868983,
4.45660012604585));
#103717=CARTESIAN_POINT('Ctrl Pts',(-9.3174356340809,23.8974614068988,4.45980799487661));
#103718=CARTESIAN_POINT('Ctrl Pts',(-9.33981231433111,23.8956366935544,
4.47556378972595));
#103719=CARTESIAN_POINT('Ctrl Pts',(-9.35802598237196,23.8942104215255,
4.48764467117932));
#103720=CARTESIAN_POINT('Ctrl Pts',(-9.3952985797548,23.8913854147618,4.51089996266216));
#103721=CARTESIAN_POINT('Ctrl Pts',(-9.41435644041523,23.889987687607,4.52205883430514));
#103722=CARTESIAN_POINT('Ctrl Pts',(-9.52096836402355,23.8823601062256,
4.58052098527914));
#103723=CARTESIAN_POINT('Ctrl Pts',(-9.61392727158488,23.8763670395781,
4.61711469826957));
#103724=CARTESIAN_POINT('Ctrl Pts',(-9.73710838056421,23.8682223059457,
4.64836550184109));
#103725=CARTESIAN_POINT('Ctrl Pts',(-9.76406263940538,23.8664312287492,
4.65420479131426));
#103726=CARTESIAN_POINT('Ctrl Pts',(-9.79951152840016,23.8640521687142,
4.66059072806934));
#103727=CARTESIAN_POINT('Ctrl Pts',(-9.80784338234675,23.8634913431225,
4.66199926567614));
#103728=CARTESIAN_POINT('Ctrl Pts',(-9.82151059006454,23.8625683620116,
4.66415875806456));
#103729=CARTESIAN_POINT('Ctrl Pts',(-9.82683731468442,23.862207885294,4.66496298920162));
#103730=CARTESIAN_POINT('Ctrl Pts',(-9.83717069919895,23.8615070551732,
4.66645069069539));
#103731=CARTESIAN_POINT('Ctrl Pts',(-9.84217661719173,23.861166847301,4.66713854082958));
#103732=CARTESIAN_POINT('Ctrl Pts',(-9.85378121420336,23.8603764989538,
4.66865707584187));
#103733=CARTESIAN_POINT('Ctrl Pts',(-9.86038275892182,23.8599256299,4.66946411534257));
#103734=CARTESIAN_POINT('Ctrl Pts',(-9.88193529603711,23.8584493350579,
4.671913825944));
#103735=CARTESIAN_POINT('Ctrl Pts',(-9.89691045647981,23.857416798602,4.67332595612959));
#103736=CARTESIAN_POINT('Ctrl Pts',(-9.9929054765429,23.850751635935,4.68052625416412));
#103737=CARTESIAN_POINT('Ctrl Pts',(-10.0742996007773,23.8448669287615,
4.67820524163744));
#103738=CARTESIAN_POINT('Ctrl Pts',(-10.2089777164519,23.8348966307027,
4.66034953611414));
#103739=CARTESIAN_POINT('Ctrl Pts',(-10.262599784569,23.8308696100445,4.64940186962942));
#103740=CARTESIAN_POINT('Ctrl Pts',(-10.3308203454896,23.8257928676023,
4.6304483410427));
#103741=CARTESIAN_POINT('Ctrl Pts',(-10.3462814384368,23.8246458002523,
4.62580849756253));
#103742=CARTESIAN_POINT('Ctrl Pts',(-10.3718981639098,23.8227562969774,
4.617543258122));
#103743=CARTESIAN_POINT('Ctrl Pts',(-10.382107847746,23.8220061940752,4.61409370857377));
#103744=CARTESIAN_POINT('Ctrl Pts',(-10.3961799668054,23.8209777969046,
4.60912294129082));
#103745=CARTESIAN_POINT('Ctrl Pts',(-10.4000834927303,23.8206931144513,
4.60772084261028));
#103746=CARTESIAN_POINT('Ctrl Pts',(-10.4066831482057,23.8202129004431,
4.6053108898631));
#103747=CARTESIAN_POINT('Ctrl Pts',(-10.4093831152979,23.8200167539753,
4.60431372891498));
#103748=CARTESIAN_POINT('Ctrl Pts',(-10.4145573232763,23.8196414944539,
4.60238118839328));
#103749=CARTESIAN_POINT('Ctrl Pts',(-10.4170320940141,23.8194622883326,
4.60144736221059));
#103750=CARTESIAN_POINT('Ctrl Pts',(-10.4229616827652,23.8190335240828,
4.59918705067032));
#103751=CARTESIAN_POINT('Ctrl Pts',(-10.4264134629599,23.8187844318948,
4.59785259346538));
#103752=CARTESIAN_POINT('Ctrl Pts',(-10.4389392675885,23.8178821609235,
4.59294213280805));
#103753=CARTESIAN_POINT('Ctrl Pts',(-10.4479753778139,23.8172343895273,
4.58926960042853));
#103754=CARTESIAN_POINT('Ctrl Pts',(-10.5131930964369,23.8125746184801,
4.56181438548205));
#103755=CARTESIAN_POINT('Ctrl Pts',(-10.5675046499917,23.8087753158279,
4.53380723042979));
#103756=CARTESIAN_POINT('Ctrl Pts',(-10.6764604641247,23.8008441738512,
4.46643468616136));
#103757=CARTESIAN_POINT('Ctrl Pts',(-10.7303923847933,23.7967276251116,
4.42634826377169));
#103758=CARTESIAN_POINT('Ctrl Pts',(-10.8066474358408,23.7902539068963,
4.3588500362639));
#103759=CARTESIAN_POINT('Ctrl Pts',(-10.8316420103137,23.7880095338998,
4.3346703983474));
#103760=CARTESIAN_POINT('Ctrl Pts',(-10.8617975793566,23.7851159035078,
4.30279710120222));
#103761=CARTESIAN_POINT('Ctrl Pts',(-10.8679887042022,23.7845112645562,
4.29609914904853));
#103762=CARTESIAN_POINT('Ctrl Pts',(-10.8778099514203,23.7835345190767,
4.28522313599939));
#103763=CARTESIAN_POINT('Ctrl Pts',(-10.8814895878258,23.7831644919395,
4.28109012853766));
#103764=CARTESIAN_POINT('Ctrl Pts',(-10.8884425259255,23.7824573767328,
4.27316880758897));
#103765=CARTESIAN_POINT('Ctrl Pts',(-10.8917210734431,23.7821205159151,
4.26938524338956));
#103766=CARTESIAN_POINT('Ctrl Pts',(-10.8991627192592,23.7813479322799,
4.26068585021914));
#103767=CARTESIAN_POINT('Ctrl Pts',(-10.9033097783901,23.7809115699771,
4.25575657445314));
#103768=CARTESIAN_POINT('Ctrl Pts',(-10.9160273047438,23.7795550318081,
4.24038605414415));
#103769=CARTESIAN_POINT('Ctrl Pts',(-10.9244584706811,23.7786293446285,
4.22983151600253));
#103770=CARTESIAN_POINT('Ctrl Pts',(-10.9947184730083,23.7706827911356,
4.1387054387195));
#103771=CARTESIAN_POINT('Ctrl Pts',(-11.0460555946995,23.7632438051067,
4.05060750729996));
#103772=CARTESIAN_POINT('Ctrl Pts',(-11.1079450174856,23.7515443441016,
3.90362442750183));
#103773=CARTESIAN_POINT('Ctrl Pts',(-11.126467130191,23.7473180290309,3.84860901352965));
#103774=CARTESIAN_POINT('Ctrl Pts',(-11.1426576443109,23.7427790904938,
3.785448377643));
#103775=CARTESIAN_POINT('Ctrl Pts',(-11.1443873879626,23.7422792162987,
3.77843272299209));
#103776=CARTESIAN_POINT('Ctrl Pts',(-11.1468666841089,23.7415400822145,
3.76796334510997));
#103777=CARTESIAN_POINT('Ctrl Pts',(-11.1476653972407,23.7412981901362,
3.7645216101626));
#103778=CARTESIAN_POINT('Ctrl Pts',(-11.1490080011032,23.7408850381905,
3.75861562905306));
#103779=CARTESIAN_POINT('Ctrl Pts',(-11.1495594720713,23.7407133547336,
3.75615317839993));
#103780=CARTESIAN_POINT('Ctrl Pts',(-11.1507939795114,23.7403244708959,
3.75055651745531));
#103781=CARTESIAN_POINT('Ctrl Pts',(-11.1514721289393,23.7401075489643,
3.7474212776147));
#103782=CARTESIAN_POINT('Ctrl Pts',(-11.1532819811434,23.739519388985,3.73888529136071));
#103783=CARTESIAN_POINT('Ctrl Pts',(-11.1543885694944,23.7391495325236,
3.73347921544909));
#103784=CARTESIAN_POINT('Ctrl Pts',(-11.1596910903611,23.7373237908082,
3.70661483876489));
#103785=CARTESIAN_POINT('Ctrl Pts',(-11.1633272106256,23.7358966061409,
3.68504881959785));
#103786=CARTESIAN_POINT('Ctrl Pts',(-11.1694237019178,23.7330709102144,
3.64152961432118));
#103787=CARTESIAN_POINT('Ctrl Pts',(-11.1718712487657,23.7316733736831,
3.61958386217328));
#103788=CARTESIAN_POINT('Ctrl Pts',(-11.1819462968778,23.7240452066313,
3.49840187809117));
#103789=CARTESIAN_POINT('Ctrl Pts',(-11.1775883343904,23.7180513238473,
3.39858102613226));
#103790=CARTESIAN_POINT('Ctrl Pts',(-11.1560622003909,23.7099068222259,
3.27334077835033));
#103791=CARTESIAN_POINT('Ctrl Pts',(-11.1504437949019,23.7081170279694,
3.24636029860222));
#103792=CARTESIAN_POINT('Ctrl Pts',(-11.1418736435704,23.7057394296445,
3.21139817680151));
#103793=CARTESIAN_POINT('Ctrl Pts',(-11.1397741930354,23.7051787397776,
3.20321520769412));
#103794=CARTESIAN_POINT('Ctrl Pts',(-11.1361922057639,23.704255921768,3.18985269522415));
#103795=CARTESIAN_POINT('Ctrl Pts',(-11.1347618149761,23.7038954712035,
3.1846593893443));
#103796=CARTESIAN_POINT('Ctrl Pts',(-11.1319206323133,23.7031946487214,
3.17461364521116));
#103797=CARTESIAN_POINT('Ctrl Pts',(-11.1305141349725,23.7028544220548,
3.16976010690089));
#103798=CARTESIAN_POINT('Ctrl Pts',(-11.1271838925165,23.7020639661097,
3.15853875187798));
#103799=CARTESIAN_POINT('Ctrl Pts',(-11.1252373610865,23.7016130076908,
3.15217793402919));
#103800=CARTESIAN_POINT('Ctrl Pts',(-11.1187119476671,23.7001361345097,
3.13148258902579));
#103801=CARTESIAN_POINT('Ctrl Pts',(-11.1139123688111,23.699103101537,3.11721977303774));
#103802=CARTESIAN_POINT('Ctrl Pts',(-11.0815667270918,23.6924582498196,
3.02686461374704));
#103803=CARTESIAN_POINT('Ctrl Pts',(-11.0465176558544,23.6865964223549,
2.95370340063427));
#103804=CARTESIAN_POINT('Ctrl Pts',(-10.975584889035,23.6766323653871,2.83792652717423));
#103805=CARTESIAN_POINT('Ctrl Pts',(-10.9436759959894,23.6725884644744,
2.79318789922231));
#103806=CARTESIAN_POINT('Ctrl Pts',(-10.8984726641327,23.6674928353562,
2.738354683249));
#103807=CARTESIAN_POINT('Ctrl Pts',(-10.8879267174741,23.6663431433701,
2.72608597604728));
#103808=CARTESIAN_POINT('Ctrl Pts',(-10.8699277940507,23.6644497853856,
2.7059992457024));
#103809=CARTESIAN_POINT('Ctrl Pts',(-10.8626142665421,23.6636984152081,
2.69805972002774));
#103810=CARTESIAN_POINT('Ctrl Pts',(-10.8523386489115,23.6626685791219,
2.68720782746603));
#103811=CARTESIAN_POINT('Ctrl Pts',(-10.8494690314039,23.6623837025155,
2.68420918480168));
#103812=CARTESIAN_POINT('Ctrl Pts',(-10.8445822445138,23.6619032529932,
2.67915642048078));
#103813=CARTESIAN_POINT('Ctrl Pts',(-10.8425733033742,23.6617070638589,
2.67709442892734));
#103814=CARTESIAN_POINT('Ctrl Pts',(-10.83870441001,23.6613317969085,2.67315239092663));
#103815=CARTESIAN_POINT('Ctrl Pts',(-10.8368456672802,23.6611526255885,
2.67127122319315));
#103816=CARTESIAN_POINT('Ctrl Pts',(-10.8323722001315,23.6607240381542,
2.66677418298574));
#103817=CARTESIAN_POINT('Ctrl Pts',(-10.829751438581,23.660475087089,2.66416431472123));
#103818=CARTESIAN_POINT('Ctrl Pts',(-10.8201873739642,23.6595740980788,
2.65472931909697));
#103819=CARTESIAN_POINT('Ctrl Pts',(-10.813171570096,23.6589274466233,2.64797777895053));
#103820=CARTESIAN_POINT('Ctrl Pts',(-10.7591421904687,23.6540472672213,
2.59725890354204));
#103821=CARTESIAN_POINT('Ctrl Pts',(-10.7086724273206,23.6500511697405,
2.55711931092429));
#103822=CARTESIAN_POINT('Ctrl Pts',(-10.6009091200361,23.6420284569847,
2.48497945380869));
#103823=CARTESIAN_POINT('Ctrl Pts',(-10.5437267541401,23.6380135668804,
2.45323402321985));
#103824=CARTESIAN_POINT('Ctrl Pts',(-10.4640496196473,23.6324492750353,
2.41729868158648));
#103825=CARTESIAN_POINT('Ctrl Pts',(-10.4436378104736,23.6310270875745,
2.4087761015558));
#103826=CARTESIAN_POINT('Ctrl Pts',(-10.4080996547845,23.6285472439129,
2.3950997311493));
#103827=CARTESIAN_POINT('Ctrl Pts',(-10.3930858020622,23.6274984933614,
2.38966966866181));
#103828=CARTESIAN_POINT('Ctrl Pts',(-10.371446705681,23.6259831872884,2.3823373497377));
#103829=CARTESIAN_POINT('Ctrl Pts',(-10.3649075000058,23.6255247898507,
2.38018529746614));
#103830=CARTESIAN_POINT('Ctrl Pts',(-10.3535183347448,23.6247254028659,
2.37654747525841));
#103831=CARTESIAN_POINT('Ctrl Pts',(-10.3486768984253,23.6243852764271,
2.37503546390294));
#103832=CARTESIAN_POINT('Ctrl Pts',(-10.3393249206759,23.6237275980221,
2.37218095110167));
#103833=CARTESIAN_POINT('Ctrl Pts',(-10.3348157944247,23.6234101940062,
2.37083411690671));
#103834=CARTESIAN_POINT('Ctrl Pts',(-10.3241084695806,23.6226557221821,
2.36770571249692));
#103835=CARTESIAN_POINT('Ctrl Pts',(-10.3179035242519,23.6222178947171,
2.36594797299477));
#103836=CARTESIAN_POINT('Ctrl Pts',(-10.2958414568409,23.6206588294125,
2.35989351276056));
#103837=CARTESIAN_POINT('Ctrl Pts',(-10.2799098501674,23.6195286770676,
2.35587789191278));
#103838=CARTESIAN_POINT('Ctrl Pts',(-10.1553293300501,23.6106534633178,
2.32723463508429));
#103839=CARTESIAN_POINT('Ctrl Pts',(-10.0437812076379,23.6024058353221,
2.31780765211192));
#103840=CARTESIAN_POINT('Ctrl Pts',(-9.89190655802231,23.5913047374816,
2.326512558362));
#103841=CARTESIAN_POINT('Ctrl Pts',(-9.85135104491018,23.5883624119763,
2.33095716989985));
#103842=CARTESIAN_POINT('Ctrl Pts',(-9.81110406370983,23.5855117083725,
2.33749693000274));
#103843=CARTESIAN_POINT('Ctrl Pts',(-9.81110406371068,23.4873487054734,
2.3374969300026));
#103844=CARTESIAN_POINT('Ctrl Pts',(-9.87134046747871,23.4917839927589,
2.32770907465656));
#103845=CARTESIAN_POINT('Ctrl Pts',(-9.93228809589294,23.4963001685831,
2.32261115923266));
#103846=CARTESIAN_POINT('Ctrl Pts',(-10.0359488392081,23.5038554906571,
2.32202991350013));
#103847=CARTESIAN_POINT('Ctrl Pts',(-10.0784883483419,23.5069180100853,
2.32409767893046));
#103848=CARTESIAN_POINT('Ctrl Pts',(-10.1271285556948,23.5103134273303,
2.32911421347605));
#103849=CARTESIAN_POINT('Ctrl Pts',(-10.1334249632994,23.5107508777757,
2.32981498112066));
#103850=CARTESIAN_POINT('Ctrl Pts',(-10.1430428503261,23.5114155996187,
2.33096405778238));
#103851=CARTESIAN_POINT('Ctrl Pts',(-10.1463684582694,23.5116448029577,
2.33137578051879));
#103852=CARTESIAN_POINT('Ctrl Pts',(-10.1524574703399,23.5120632344828,
2.33215602332165));
#103853=CARTESIAN_POINT('Ctrl Pts',(-10.1552213248156,23.512252694493,2.33252016085938));
#103854=CARTESIAN_POINT('Ctrl Pts',(-10.1614409551899,23.5126780013161,
2.33336207403037));
#103855=CARTESIAN_POINT('Ctrl Pts',(-10.1648959143414,23.5129135368851,
2.33384539166219));
#103856=CARTESIAN_POINT('Ctrl Pts',(-10.1737765937301,23.5135172285843,
2.33512797518922));
#103857=CARTESIAN_POINT('Ctrl Pts',(-10.1791990445895,23.5138841708593,
2.33594981035684));
#103858=CARTESIAN_POINT('Ctrl Pts',(-10.2134500495516,23.51619255771,2.34138595588647));
#103859=CARTESIAN_POINT('Ctrl Pts',(-10.2421070925027,23.5180817877162,
2.3470334315056));
#103860=CARTESIAN_POINT('Ctrl Pts',(-10.3663252610318,23.5262019958568,
2.37635000323533));
#103861=CARTESIAN_POINT('Ctrl Pts',(-10.4589145078455,23.532105600726,2.41087947671889));
#103862=CARTESIAN_POINT('Ctrl Pts',(-10.5819091289109,23.5408809782114,
2.47525255903733));
#103863=CARTESIAN_POINT('Ctrl Pts',(-10.6166945891777,23.543476180306,2.49580241408152));
#103864=CARTESIAN_POINT('Ctrl Pts',(-10.6583043722647,23.5467645636923,
2.52336221615197));
#103865=CARTESIAN_POINT('Ctrl Pts',(-10.6661906113755,23.547396319413,2.52872451494545));
#103866=CARTESIAN_POINT('Ctrl Pts',(-10.6786222594177,23.5484063085265,
2.53740012702518));
#103867=CARTESIAN_POINT('Ctrl Pts',(-10.6832106654075,23.5487821972534,
2.54065132968317));
#103868=CARTESIAN_POINT('Ctrl Pts',(-10.6918241198066,23.5494938198819,
2.54684769150019));
#103869=CARTESIAN_POINT('Ctrl Pts',(-10.6958540994004,23.5498292794069,
2.54978580994863));
#103870=CARTESIAN_POINT('Ctrl Pts',(-10.7049169270239,23.5505894517735,
2.55648177619441));
#103871=CARTESIAN_POINT('Ctrl Pts',(-10.7099385858221,23.5510147311593,
2.56025444168942));
#103872=CARTESIAN_POINT('Ctrl Pts',(-10.7227857101931,23.5521134241664,
2.57006795574444));
#103873=CARTESIAN_POINT('Ctrl Pts',(-10.7305655930084,23.5527891116465,
2.5761673886878));
#103874=CARTESIAN_POINT('Ctrl Pts',(-10.7915963671532,23.5581737158395,
2.62526859577035));
#103875=CARTESIAN_POINT('Ctrl Pts',(-10.8410740402208,23.5630643210913,
2.6727326305068));
#103876=CARTESIAN_POINT('Ctrl Pts',(-10.9319287784207,23.5731260847822,
2.77651193159085));
#103877=CARTESIAN_POINT('Ctrl Pts',(-10.9729931741445,23.5782801102099,
2.83275892035766));
#103878=CARTESIAN_POINT('Ctrl Pts',(-11.0233236648928,23.5853049567174,
2.9163136988242));
#103879=CARTESIAN_POINT('Ctrl Pts',(-11.0369286076875,23.5872963252596,
2.94083957700686));
#103880=CARTESIAN_POINT('Ctrl Pts',(-11.052252950371,23.5896382580722,2.97095196663099));
#103881=CARTESIAN_POINT('Ctrl Pts',(-11.0548221551108,23.5900345765803,
2.97609321664473));
#103882=CARTESIAN_POINT('Ctrl Pts',(-11.0587742187887,23.5906498088235,
2.98414864770004));
#103883=CARTESIAN_POINT('Ctrl Pts',(-11.0601828736926,23.5908702450764,
2.98704996441718));
#103884=CARTESIAN_POINT('Ctrl Pts',(-11.0627924028258,23.5912807113445,
2.99248131694517));
#103885=CARTESIAN_POINT('Ctrl Pts',(-11.0639961624295,23.591470908929,2.99500983007957));
#103886=CARTESIAN_POINT('Ctrl Pts',(-11.0667257632721,23.5919041844397,
3.00079648307236));
#103887=CARTESIAN_POINT('Ctrl Pts',(-11.0682457040757,23.5921469018397,
3.00405734008063));
#103888=CARTESIAN_POINT('Ctrl Pts',(-11.072250972955,23.5927905403267,3.01275402783155));
#103889=CARTESIAN_POINT('Ctrl Pts',(-11.074709943605,23.5931899255471,3.01820198506493));
#103890=CARTESIAN_POINT('Ctrl Pts',(-11.0940369721877,23.5963652920292,
3.06190615923066));
#103891=CARTESIAN_POINT('Ctrl Pts',(-11.1089005251343,23.5990335542725,
3.10102183620292));
#103892=CARTESIAN_POINT('Ctrl Pts',(-11.1518154039672,23.6078642520082,
3.23504819676));
#103893=CARTESIAN_POINT('Ctrl Pts',(-11.1699908605694,23.6138214759154,
3.33266765648044));
#103894=CARTESIAN_POINT('Ctrl Pts',(-11.1774012379728,23.6219692105759,
3.4596983953908));
#103895=CARTESIAN_POINT('Ctrl Pts',(-11.1780299134458,23.6238085269764,
3.48803290434519));
#103896=CARTESIAN_POINT('Ctrl Pts',(-11.1775178892408,23.6262425554278,
3.52488791624394));
#103897=CARTESIAN_POINT('Ctrl Pts',(-11.177306813993,23.626808469969,3.53341327921837));
#103898=CARTESIAN_POINT('Ctrl Pts',(-11.1768108034502,23.6277376062525,
3.54733482924011));
#103899=CARTESIAN_POINT('Ctrl Pts',(-11.1765812788508,23.6280991038632,
3.5527327770721));
#103900=CARTESIAN_POINT('Ctrl Pts',(-11.1760656664596,23.6288003423067,
3.56316687467385));
#103901=CARTESIAN_POINT('Ctrl Pts',(-11.1757843487723,23.629139927392,3.56820315020917));
#103902=CARTESIAN_POINT('Ctrl Pts',(-11.1750599709616,23.6299265175479,
3.57982951770778));
#103903=CARTESIAN_POINT('Ctrl Pts',(-11.1745938116968,23.6303742308522,
3.58641794771668));
#103904=CARTESIAN_POINT('Ctrl Pts',(-11.1729044815384,23.6318300295772,
3.60774432600491));
#103905=CARTESIAN_POINT('Ctrl Pts',(-11.1714591777559,23.6328449560789,
3.62246274043899));
#103906=CARTESIAN_POINT('Ctrl Pts',(-11.1595324485788,23.6399332840094,
3.72418488387559));
#103907=CARTESIAN_POINT('Ctrl Pts',(-11.1396476297149,23.6463052383613,
3.80979353133322));
#103908=CARTESIAN_POINT('Ctrl Pts',(-11.0871584061359,23.657873777436,3.95833846699633));
#103909=CARTESIAN_POINT('Ctrl Pts',(-11.0580231272876,23.6630166067964,
4.02208885143681));
#103910=CARTESIAN_POINT('Ctrl Pts',(-11.0198284152148,23.6683887776524,
4.08914946789466));
#103911=CARTESIAN_POINT('Ctrl Pts',(-11.0162009289422,23.6688877940868,
4.0953845568575));
#103912=CARTESIAN_POINT('Ctrl Pts',(-11.0107131638716,23.669625865636,4.10462089274858));
#103913=CARTESIAN_POINT('Ctrl Pts',(-11.0088963883889,23.6698675429621,
4.10764759679456));
#103914=CARTESIAN_POINT('Ctrl Pts',(-11.0057581540402,23.6702804071296,
4.11282294373398));
#103915=CARTESIAN_POINT('Ctrl Pts',(-11.0044433745845,23.6704520164085,
4.11497555437633));
#103916=CARTESIAN_POINT('Ctrl Pts',(-11.0014408134876,23.6708408325963,
4.11985615227144));
#103917=CARTESIAN_POINT('Ctrl Pts',(-10.999748796384,23.6710577606218,4.12258147834475));
#103918=CARTESIAN_POINT('Ctrl Pts',(-10.9951141837021,23.6716461548264,
4.12997881679343));
#103919=CARTESIAN_POINT('Ctrl Pts',(-10.9921497894248,23.6720162369256,
4.13463717707898));
#103920=CARTESIAN_POINT('Ctrl Pts',(-10.9772548048278,23.6738458679861,
4.15768425749344));
#103921=CARTESIAN_POINT('Ctrl Pts',(-10.9648443727188,23.6752765654319,
4.17575958856746));
#103922=CARTESIAN_POINT('Ctrl Pts',(-10.9389425843052,23.6781049348365,
4.21131484808431));
#103923=CARTESIAN_POINT('Ctrl Pts',(-10.9254501415301,23.6795017579289,
4.22878263044846));
#103924=CARTESIAN_POINT('Ctrl Pts',(-10.8484566912129,23.6871280880367,
4.32287183720304));
#103925=CARTESIAN_POINT('Ctrl Pts',(-10.7759365424521,23.693121303182,4.39158274027145));
#103926=CARTESIAN_POINT('Ctrl Pts',(-10.6734298073257,23.7012633380182,
4.46661517569012));
#103927=CARTESIAN_POINT('Ctrl Pts',(-10.6506588927732,23.703051283036,4.48208727642169));
#103928=CARTESIAN_POINT('Ctrl Pts',(-10.6202228946633,23.7054266472887,
4.50124417974429));
#103929=CARTESIAN_POINT('Ctrl Pts',(-10.6130294778427,23.7059870125333,
4.50566455623247));
#103930=CARTESIAN_POINT('Ctrl Pts',(-10.6011718177693,23.7069093484708,
4.51277662860465));
#103931=CARTESIAN_POINT('Ctrl Pts',(-10.5965354547339,23.7072696438798,
4.51551440341017));
#103932=CARTESIAN_POINT('Ctrl Pts',(-10.5875131972473,23.707970201043,4.52075894522764));
#103933=CARTESIAN_POINT('Ctrl Pts',(-10.5831296196806,23.7083103178941,
4.52326947891647));
#103934=CARTESIAN_POINT('Ctrl Pts',(-10.5729377798476,23.709100570855,4.52901972464193));
#103935=CARTESIAN_POINT('Ctrl Pts',(-10.5671180032987,23.709551436055,4.53223856760855));
#103936=CARTESIAN_POINT('Ctrl Pts',(-10.5480419593723,23.7110282242833,
4.5425792628818));
#103937=CARTESIAN_POINT('Ctrl Pts',(-10.5346768741699,23.712061266526,4.54949612307497));
#103938=CARTESIAN_POINT('Ctrl Pts',(-10.4486770725449,23.7187013132352,
4.59193467093531));
#103939=CARTESIAN_POINT('Ctrl Pts',(-10.3726920097259,23.7245578603293,
4.62014669435456));
#103940=CARTESIAN_POINT('Ctrl Pts',(-10.2263599942347,23.7356484619345,
4.65792873298871));
#103941=CARTESIAN_POINT('Ctrl Pts',(-10.1568452198501,23.7408363276891,
4.66937548710646));
#103942=CARTESIAN_POINT('Ctrl Pts',(-10.0753228561955,23.7465822273821,
4.67539445579665));
#103943=CARTESIAN_POINT('Ctrl Pts',(-10.0639137914941,23.7473785104806,
4.67607002815331));
#103944=CARTESIAN_POINT('Ctrl Pts',(-10.0482573202014,23.7484588842655,
4.6767685827087));
#103945=CARTESIAN_POINT('Ctrl Pts',(-10.044017386127,23.7487502195074,4.67693480589384));
#103946=CARTESIAN_POINT('Ctrl Pts',(-10.0368818352359,23.7492383287049,
4.6771759349204));
#103947=CARTESIAN_POINT('Ctrl Pts',(-10.0339867027271,23.7494357644113,
4.67726307858167));
#103948=CARTESIAN_POINT('Ctrl Pts',(-10.0284681619974,23.749810913207,4.67740881239099));
#103949=CARTESIAN_POINT('Ctrl Pts',(-10.0258448446948,23.7499887343987,
4.6774693168365));
#103950=CARTESIAN_POINT('Ctrl Pts',(-10.0195999155633,23.7504108760665,
4.67759247001611));
#103951=CARTESIAN_POINT('Ctrl Pts',(-10.0159781468086,23.7506547621857,
4.6776471805346));
#103952=CARTESIAN_POINT('Ctrl Pts',(-10.0031271562201,23.7515169953,4.67778201149794));
#103953=CARTESIAN_POINT('Ctrl Pts',(-9.99389701604686,23.7521305450048,
4.67777035635863));
#103954=CARTESIAN_POINT('Ctrl Pts',(-9.90687749016525,23.7578688342754,
4.67663740819367));
#103955=CARTESIAN_POINT('Ctrl Pts',(-9.82936708318603,23.7626408666315,
4.66791926106481));
#103956=CARTESIAN_POINT('Ctrl Pts',(-9.67322522867196,23.7725136538506,
4.63446693743941));
#103957=CARTESIAN_POINT('Ctrl Pts',(-9.59519432679469,23.7775998045525,
4.60902066409386));
#103958=CARTESIAN_POINT('Ctrl Pts',(-9.51007537320035,23.783717745883,4.57107311953033));
#103959=CARTESIAN_POINT('Ctrl Pts',(-9.49978123401993,23.7844672664242,
4.56630433684951));
#103960=CARTESIAN_POINT('Ctrl Pts',(-9.48414156363063,23.785621604239,4.55878291335345));
#103961=CARTESIAN_POINT('Ctrl Pts',(-9.47874535580714,23.7860227708797,
4.5561367229787));
#103962=CARTESIAN_POINT('Ctrl Pts',(-9.46896687076106,23.7867551038512,
4.55124835685043));
#103963=CARTESIAN_POINT('Ctrl Pts',(-9.46457792052002,23.7870857929138,
4.54901977468096));
#103964=CARTESIAN_POINT('Ctrl Pts',(-9.45504217813098,23.7878086913508,
4.54410236727641));
#103965=CARTESIAN_POINT('Ctrl Pts',(-9.44990106511162,23.7882012672329,
4.54140287147131));
#103966=CARTESIAN_POINT('Ctrl Pts',(-9.43586951722983,23.7892806263323,
4.53390229203741));
#103967=CARTESIAN_POINT('Ctrl Pts',(-9.42702074589338,23.7899700846695,
4.52902473942494));
#103968=CARTESIAN_POINT('Ctrl Pts',(-9.37908291821461,23.793754401468,4.50179078274726));
#103969=CARTESIAN_POINT('Ctrl Pts',(-9.34124265455703,23.7969241584934,
4.47732320150947));
#103970=CARTESIAN_POINT('Ctrl Pts',(-9.23816336621629,23.8060923969847,
4.40196136775153));
#103971=CARTESIAN_POINT('Ctrl Pts',(-9.17675224219001,23.81223090797,4.34628039263864));
#103972=CARTESIAN_POINT('Ctrl Pts',(-9.09584475789561,23.8210602396578,
4.25571334230284));
#103973=CARTESIAN_POINT('Ctrl Pts',(-9.0714468650037,23.8238425884907,4.22552678071012));
#103974=CARTESIAN_POINT('Ctrl Pts',(-9.04491545927201,23.8269671319655,
4.18916417264557));
#103975=CARTESIAN_POINT('Ctrl Pts',(-9.04128968936591,23.827396450313,4.18411130770517));
#103976=CARTESIAN_POINT('Ctrl Pts',(-9.03578616780716,23.8280514172476,
4.17631192022765));
#103977=CARTESIAN_POINT('Ctrl Pts',(-9.03387981337412,23.8282789135404,
4.17358586187757));
#103978=CARTESIAN_POINT('Ctrl Pts',(-9.03039630128335,23.8286957204143,
4.168559278751));
#103979=CARTESIAN_POINT('Ctrl Pts',(-9.02881576758655,23.8288852505089,
4.16626123165446));
#103980=CARTESIAN_POINT('Ctrl Pts',(-9.02526022860582,23.8293125788578,
4.16105205170739));
#103981=CARTESIAN_POINT('Ctrl Pts',(-9.02329009378911,23.8295500519712,
4.15813767322915));
#103982=CARTESIAN_POINT('Ctrl Pts',(-9.01822845273933,23.8301620811689,
4.15057730748148));
#103983=CARTESIAN_POINT('Ctrl Pts',(-9.01515681301003,23.8305353664732,
4.14591803201631));
#103984=CARTESIAN_POINT('Ctrl Pts',(-8.99514757186776,23.8329807594324,
4.11509204584473));
#103985=CARTESIAN_POINT('Ctrl Pts',(-8.97921967928989,23.83499326539,4.08828101444889));
#103986=CARTESIAN_POINT('Ctrl Pts',(-8.91838477902032,23.8431004152923,
3.97595087849477));
#103987=CARTESIAN_POINT('Ctrl Pts',(-8.88301341057005,23.8489002221996,
3.88569912404111));
#103988=CARTESIAN_POINT('Ctrl Pts',(-8.84910802691948,23.8575430177518,
3.75328139299766));
#103989=CARTESIAN_POINT('Ctrl Pts',(-8.8411514169592,23.8601214088915,3.71394678024683));
#103990=CARTESIAN_POINT('Ctrl Pts',(-8.83380844873831,23.8633909176912,
3.66487245297488));
#103991=CARTESIAN_POINT('Ctrl Pts',(-8.83251411780653,23.8640214844554,
3.6554424848073));
#103992=CARTESIAN_POINT('Ctrl Pts',(-8.8306376344257,23.86503001508,3.64042186449809));
#103993=CARTESIAN_POINT('Ctrl Pts',(-8.82998094201227,23.8654056462074,
3.63484081035416));
#103994=CARTESIAN_POINT('Ctrl Pts',(-8.82881680387449,23.8661170593123,
3.62429748091954));
#103995=CARTESIAN_POINT('Ctrl Pts',(-8.82830089151082,23.8664525689335,
3.61933624972127));
#103996=CARTESIAN_POINT('Ctrl Pts',(-8.82720594563834,23.8672132328656,
3.608114290138));
#103997=CARTESIAN_POINT('Ctrl Pts',(-8.82664550426155,23.867638956637,3.60185194325914));
#103998=CARTESIAN_POINT('Ctrl Pts',(-8.82533119818919,23.8687395560514,
3.58571123814033));
#103999=CARTESIAN_POINT('Ctrl Pts',(-8.82465179942531,23.8694167187662,
3.57582748346809));
#104000=CARTESIAN_POINT('Ctrl Pts',(-8.82006612960381,23.8750475378317,
3.49404736808586));
#104001=CARTESIAN_POINT('Ctrl Pts',(-8.82263657538866,23.880203516386,3.42195330452403));
#104002=CARTESIAN_POINT('Ctrl Pts',(-8.84021428314793,23.8903249666973,
3.28454439463232));
#104003=CARTESIAN_POINT('Ctrl Pts',(-8.85423871760985,23.8952546929784,
3.21936607815493));
#104004=CARTESIAN_POINT('Ctrl Pts',(-8.88171902826667,23.9020207411904,
3.12946455934411));
#104005=CARTESIAN_POINT('Ctrl Pts',(-8.89066111072591,23.9039698103572,
3.10349482708682));
#104006=CARTESIAN_POINT('Ctrl Pts',(-8.90255182315797,23.9062690118763,
3.07252460352686));
#104007=CARTESIAN_POINT('Ctrl Pts',(-8.90463883975899,23.9066630258453,
3.0672048435975));
#104008=CARTESIAN_POINT('Ctrl Pts',(-8.90796156923046,23.9072754756593,
3.05891329241829));
#104009=CARTESIAN_POINT('Ctrl Pts',(-8.90917084888182,23.9074954122955,
3.05593110716472));
#104010=CARTESIAN_POINT('Ctrl Pts',(-8.91145580316724,23.9079054561983,
3.05036187505279));
#104011=CARTESIAN_POINT('Ctrl Pts',(-8.91252847711631,23.9080957272876,
3.04777373030479));
#104012=CARTESIAN_POINT('Ctrl Pts',(-8.91500393915851,23.9085298093984,
3.04186068449079));
#104013=CARTESIAN_POINT('Ctrl Pts',(-8.91641278129487,23.9087732548243,
3.03853838210982));
#104014=CARTESIAN_POINT('Ctrl Pts',(-8.92021049494198,23.9094201307703,
3.02969598751237));
#104015=CARTESIAN_POINT('Ctrl Pts',(-8.92262645785426,23.9098220007971,
3.02418754342833));
#104016=CARTESIAN_POINT('Ctrl Pts',(-8.94389196619759,23.9132793238638,
2.97669426681406));
#104017=CARTESIAN_POINT('Ctrl Pts',(-8.96514769616483,23.91620383488,2.93582373661358));
#104018=CARTESIAN_POINT('Ctrl Pts',(-9.04679997268813,23.9261652960619,
2.79904875727945));
#104019=CARTESIAN_POINT('Ctrl Pts',(-9.11857375832019,23.9329792984337,
2.71069002717898));
#104020=CARTESIAN_POINT('Ctrl Pts',(-9.21235095020103,23.9413073693433,
2.62426737635624));
#104021=CARTESIAN_POINT('Ctrl Pts',(-9.22301784118901,23.9422465285172,
2.61478965782006));
#104022=CARTESIAN_POINT('Ctrl Pts',(-9.23879946104927,23.9436259298127,
2.60127245310413));
#104023=CARTESIAN_POINT('Ctrl Pts',(-9.24377996373205,23.9440598305615,
2.59707767890721));
#104024=CARTESIAN_POINT('Ctrl Pts',(-9.25266851812704,23.9448318456982,
2.58971651964758));
#104025=CARTESIAN_POINT('Ctrl Pts',(-9.25656258072849,23.9451692770237,
2.58653343756683));
#104026=CARTESIAN_POINT('Ctrl Pts',(-9.26471310577264,23.9458739828845,
2.57995767895249));
#104027=CARTESIAN_POINT('Ctrl Pts',(-9.26897293000333,23.9462414205239,
2.57656937967643));
#104028=CARTESIAN_POINT('Ctrl Pts',(-9.28011209737974,23.9472000875652,
2.56783457507285));
#104029=CARTESIAN_POINT('Ctrl Pts',(-9.28702744792748,23.947793127955,2.56253474482892));
#104030=CARTESIAN_POINT('Ctrl Pts',(-9.31816369053002,23.9504544824182,
2.53921614096332));
#104031=CARTESIAN_POINT('Ctrl Pts',(-9.34301129544578,23.9525552717841,
2.52205729629554));
#104032=CARTESIAN_POINT('Ctrl Pts',(-9.45090600407031,23.9615896100804,
2.45351803230599));
#104033=CARTESIAN_POINT('Ctrl Pts',(-9.53950756581154,23.9688387292814,
2.41162038657657));
#104034=CARTESIAN_POINT('Ctrl Pts',(-9.67111414646436,23.9789284319097,
2.36836242325051));
#104035=CARTESIAN_POINT('Ctrl Pts',(-9.71063223727229,23.9818710067288,
2.35761802839803));
#104036=CARTESIAN_POINT('Ctrl Pts',(-9.75644342183527,23.9851283194583,
2.34769335938745));
#104037=CARTESIAN_POINT('Ctrl Pts',(-9.76226284372576,23.9855392802199,
2.34647867424707));
#104038=CARTESIAN_POINT('Ctrl Pts',(-9.77160924513654,23.9861945355241,
2.3446015404726));
#104039=CARTESIAN_POINT('Ctrl Pts',(-9.77513039715869,23.9864403121219,
2.34391107618617));
#104040=CARTESIAN_POINT('Ctrl Pts',(-9.78140418235259,23.986876229845,2.34271059479256));
#104041=CARTESIAN_POINT('Ctrl Pts',(-9.7841555412148,23.9870667169374,2.34219428696871));
#104042=CARTESIAN_POINT('Ctrl Pts',(-9.79008677168292,23.9874758726541,
2.3411031364476));
#104043=CARTESIAN_POINT('Ctrl Pts',(-9.79326717875975,23.9876943573053,
2.34053156790238));
#104044=CARTESIAN_POINT('Ctrl Pts',(-9.80132929731045,23.9882459899798,
2.33911690704655));
#104045=CARTESIAN_POINT('Ctrl Pts',(-9.80621410020899,23.9885781716899,
2.33829150358947));
#104046=CARTESIAN_POINT('Ctrl Pts',(-9.8111040637107,23.9889087884094,2.3374969300026));
#104047=CARTESIAN_POINT('Origin',(-10.,12.3756328852638,3.5));
#104048=CARTESIAN_POINT('',(-9.81111852688625,24.5869833862071,2.3377666957199));
#104049=CARTESIAN_POINT('',(-9.81110406371068,24.4872084044306,2.3374969300026));
#104050=CARTESIAN_POINT('',(-9.81110406371068,12.3756328852638,2.3374969300026));
#104051=CARTESIAN_POINT('Ctrl Pts',(-9.81106550641579,24.5871379729677,
2.3375031958607));
#104052=CARTESIAN_POINT('Ctrl Pts',(-9.778173526296,24.5850437659178,2.3428489564553));
#104053=CARTESIAN_POINT('Ctrl Pts',(-9.74552537487917,24.5829249747512,
2.34958792665165));
#104054=CARTESIAN_POINT('Ctrl Pts',(-9.69640028524721,24.5796436570711,
2.36192153158769));
#104055=CARTESIAN_POINT('Ctrl Pts',(-9.67968798209671,24.578510716744,2.36651177816805));
#104056=CARTESIAN_POINT('Ctrl Pts',(-9.65696427979307,24.576944422228,2.37329580545251));
#104057=CARTESIAN_POINT('Ctrl Pts',(-9.65085992780051,24.5765210873338,
2.37517243335176));
#104058=CARTESIAN_POINT('Ctrl Pts',(-9.64008411827752,24.5757690635254,
2.37858135013507));
#104059=CARTESIAN_POINT('Ctrl Pts',(-9.6354063896023,24.5754410275816,2.38009342880476));
#104060=CARTESIAN_POINT('Ctrl Pts',(-9.62616119321268,24.5747894698107,
2.38314600635575));
#104061=CARTESIAN_POINT('Ctrl Pts',(-9.62159344271248,24.5744659908854,
2.38468534807298));
#104062=CARTESIAN_POINT('Ctrl Pts',(-9.61187893550175,24.5737746212577,
2.38802570450796));
#104063=CARTESIAN_POINT('Ctrl Pts',(-9.60673499493011,24.5734064826443,
2.38983450395624));
#104064=CARTESIAN_POINT('Ctrl Pts',(-9.59344754898872,24.5724501115701,
2.39461079770613));
#104065=CARTESIAN_POINT('Ctrl Pts',(-9.58532403193604,24.5718601108319,
2.39763253925453));
#104066=CARTESIAN_POINT('Ctrl Pts',(-9.55243902486903,24.5694495494772,
2.41027984960885));
#104067=CARTESIAN_POINT('Ctrl Pts',(-9.52797490025081,24.5676045735673,
2.42065161258633));
#104068=CARTESIAN_POINT('Ctrl Pts',(-9.47288282225408,24.5633266875081,
2.4462396207243));
#104069=CARTESIAN_POINT('Ctrl Pts',(-9.44252575845392,24.5608786715716,
2.46197997257215));
#104070=CARTESIAN_POINT('Ctrl Pts',(-9.35966027936587,24.553950521184,2.50963058102462));
#104071=CARTESIAN_POINT('Ctrl Pts',(-9.30889970784357,24.5494111218619,
2.54436077492083));
#104072=CARTESIAN_POINT('Ctrl Pts',(-9.22869765334448,24.5418804429928,
2.60897964518787));
#104073=CARTESIAN_POINT('Ctrl Pts',(-9.19771488896222,24.5388692792818,
2.63677125413567));
#104074=CARTESIAN_POINT('Ctrl Pts',(-9.16068629150373,24.5351978929914,
2.67370577889197));
#104075=CARTESIAN_POINT('Ctrl Pts',(-9.15321076810281,24.5344527322241,
2.6813684234149));
#104076=CARTESIAN_POINT('Ctrl Pts',(-9.1429902628072,24.5334296931726,2.69213459637554));
#104077=CARTESIAN_POINT('Ctrl Pts',(-9.14015588710096,24.5331455160698,
2.69515200016651));
#104078=CARTESIAN_POINT('Ctrl Pts',(-9.13537820777708,24.5326658032224,
2.70029224045094));
#104079=CARTESIAN_POINT('Ctrl Pts',(-9.13342669187868,24.5324696570292,
2.70240734305236));
#104080=CARTESIAN_POINT('Ctrl Pts',(-9.12970488291039,24.5320952308081,
2.70647091939302));
#104081=CARTESIAN_POINT('Ctrl Pts',(-9.12793333795856,24.531916854214,2.70841821022375));
#104082=CARTESIAN_POINT('Ctrl Pts',(-9.1236959602389,24.5314897758885,2.713107446587));
#104083=CARTESIAN_POINT('Ctrl Pts',(-9.12123642734107,24.5312415412185,
2.71585508673062));
#104084=CARTESIAN_POINT('Ctrl Pts',(-9.11232467045768,24.5303406457329,
2.72590534856023));
#104085=CARTESIAN_POINT('Ctrl Pts',(-9.10595001833896,24.5296934264287,
2.73327666940665));
#104086=CARTESIAN_POINT('Ctrl Pts',(-9.06068387280957,24.5250697928318,
2.78695244278102));
#104087=CARTESIAN_POINT('Ctrl Pts',(-9.02531292741572,24.5213037480345,
2.83611848664304));
#104088=CARTESIAN_POINT('Ctrl Pts',(-8.96681235378847,24.5143387984332,
2.9322604603614));
#104089=CARTESIAN_POINT('Ctrl Pts',(-8.9427314072081,24.5111414827707,2.97847547796598));
#104090=CARTESIAN_POINT('Ctrl Pts',(-8.90881892498954,24.5058541984097,
3.05563777050059));
#104091=CARTESIAN_POINT('Ctrl Pts',(-8.89706814976645,24.5038092040746,
3.08566315361815));
#104092=CARTESIAN_POINT('Ctrl Pts',(-8.881940128703,24.500810441796,3.12954292168344));
#104093=CARTESIAN_POINT('Ctrl Pts',(-8.87755909375188,24.4998869983706,
3.14303682556338));
#104094=CARTESIAN_POINT('Ctrl Pts',(-8.87016269936401,24.4982219540112,
3.16730227886122));
#104095=CARTESIAN_POINT('Ctrl Pts',(-8.86705498124146,24.4974833440926,
3.17804399389608));
#104096=CARTESIAN_POINT('Ctrl Pts',(-8.86253687891457,24.4963461876596,
3.1945368323374));
#104097=CARTESIAN_POINT('Ctrl Pts',(-8.86101607572831,24.4959512104584,
3.20025724912627));
#104098=CARTESIAN_POINT('Ctrl Pts',(-8.85952930082603,24.495552378179,3.20602440887385));
#104099=CARTESIAN_POINT('Ctrl Pts',(-8.85952012227789,24.495549915502,3.20606001911393));
#104100=CARTESIAN_POINT('Ctrl Pts',(-8.85950107683156,24.495544804418,3.2061339245243));
#104101=CARTESIAN_POINT('Ctrl Pts',(-8.85949121019862,24.4955421560037,
3.20617221974486));
#104102=CARTESIAN_POINT('Ctrl Pts',(-8.85947073554607,24.4955366589677,
3.20625170428873));
#104103=CARTESIAN_POINT('Ctrl Pts',(-8.85946012782387,24.4955338103348,
3.20629289370946));
#104104=CARTESIAN_POINT('Ctrl Pts',(-8.85943811365089,24.4955278971827,
3.20637839316351));
#104105=CARTESIAN_POINT('Ctrl Pts',(-8.85942670755547,24.4955248326535,
3.20642270326927));
#104106=CARTESIAN_POINT('Ctrl Pts',(-8.8594030346878,24.49551847074,3.20651468921928));
#104107=CARTESIAN_POINT('Ctrl Pts',(-8.85939076831832,24.4955151733415,
3.20656236518473));
#104108=CARTESIAN_POINT('Ctrl Pts',(-8.85936530789049,24.4955083272984,
3.20666134850182));
#104109=CARTESIAN_POINT('Ctrl Pts',(-8.85935211431048,24.4955047786402,
3.2067126559523));
#104110=CARTESIAN_POINT('Ctrl Pts',(-8.85932472701947,24.4954974101549,
3.206819189983));
#104111=CARTESIAN_POINT('Ctrl Pts',(-8.85931053385455,24.4954935903094,
3.20687441671485));
#104112=CARTESIAN_POINT('Ctrl Pts',(-8.8592810689919,24.49548565784,3.20698910138323));
#104113=CARTESIAN_POINT('Ctrl Pts',(-8.85926579793959,24.4954815451975,
3.20704855945387));
#104114=CARTESIAN_POINT('Ctrl Pts',(-8.85923409251358,24.4954730037076,
3.20717204507373));
#104115=CARTESIAN_POINT('Ctrl Pts',(-8.85921765887455,24.4954685748343,
3.20723607284032));
#104116=CARTESIAN_POINT('Ctrl Pts',(-8.85918353647414,24.4954593754534,
3.2073690650028));
#104117=CARTESIAN_POINT('Ctrl Pts',(-8.85916584858057,24.4954546049193,
3.20743802960041));
#104118=CARTESIAN_POINT('Ctrl Pts',(-8.85912911834146,24.4954446946245,
3.20758129374695));
#104119=CARTESIAN_POINT('Ctrl Pts',(-8.85911007699933,24.4954395548312,
3.20765559355693));
#104120=CARTESIAN_POINT('Ctrl Pts',(-8.85907053235528,24.495428876064,3.2078099604862));
#104121=CARTESIAN_POINT('Ctrl Pts',(-8.85905003021955,24.4954233370515,
3.20789002791908));
#104122=CARTESIAN_POINT('Ctrl Pts',(-8.85900744762761,24.4954118273193,
3.20805639951062));
#104123=CARTESIAN_POINT('Ctrl Pts',(-8.85898536853677,24.4954058565562,
3.20814270400968));
#104124=CARTESIAN_POINT('Ctrl Pts',(-8.85893950615215,24.49539344801,3.20832205927806));
#104125=CARTESIAN_POINT('Ctrl Pts',(-8.85891572444684,24.4953870101754,
3.20841511045768));
#104126=CARTESIAN_POINT('Ctrl Pts',(-8.8588663206733,24.495373629143,3.20860851225019));
#104127=CARTESIAN_POINT('Ctrl Pts',(-8.85884070046377,24.4953666858868,
3.20870886331933));
#104128=CARTESIAN_POINT('Ctrl Pts',(-8.85878747251416,24.4953522523952,
3.2089174651584));
#104129=CARTESIAN_POINT('Ctrl Pts',(-8.85875986694311,24.4953447620914,
3.20902571646158));
#104130=CARTESIAN_POINT('Ctrl Pts',(-8.85871160224477,24.4953316581035,
3.20921509210886));
#104131=CARTESIAN_POINT('Ctrl Pts',(-8.85869093635798,24.4953260446358,
3.20929621475369));
#104132=CARTESIAN_POINT('Ctrl Pts',(-8.85744766898421,24.4949881781523,
3.21417875902125));
#104133=CARTESIAN_POINT('Ctrl Pts',(-8.85625538587042,24.4946549557038,
3.21898778095268));
#104134=CARTESIAN_POINT('Ctrl Pts',(-8.85362777611421,24.4938991545359,
3.22987993290495));
#104135=CARTESIAN_POINT('Ctrl Pts',(-8.85221046756938,24.4934760076995,
3.23596721235092));
#104136=CARTESIAN_POINT('Ctrl Pts',(-8.84868319001925,24.492381542043,3.25168204862117));
#104137=CARTESIAN_POINT('Ctrl Pts',(-8.84664553828063,24.4917079410663,
3.26132516430873));
#104138=CARTESIAN_POINT('Ctrl Pts',(-8.83008356101068,24.4858530889064,
3.34487511716343));
#104139=CARTESIAN_POINT('Ctrl Pts',(-8.8225617934004,24.4804473462329,3.41997802999067));
#104140=CARTESIAN_POINT('Ctrl Pts',(-8.82204275818911,24.4709838669453,
3.54925293191191));
#104141=CARTESIAN_POINT('Ctrl Pts',(-8.82553758840936,24.4669933287691,
3.60318553001316));
#104142=CARTESIAN_POINT('Ctrl Pts',(-8.83761037549097,24.4604019906188,
3.69312403347695));
#104143=CARTESIAN_POINT('Ctrl Pts',(-8.84420510662729,24.4577684582247,
3.72931483947473));
#104144=CARTESIAN_POINT('Ctrl Pts',(-8.85385975541533,24.4547920040582,
3.77109960806783));
#104145=CARTESIAN_POINT('Ctrl Pts',(-8.85528285600135,24.4543698941246,
3.77704714773884));
#104146=CARTESIAN_POINT('Ctrl Pts',(-8.85754245877454,24.4537246759209,
3.78617589847587));
#104147=CARTESIAN_POINT('Ctrl Pts',(-8.85834604254963,24.4534997717774,
3.7893650298247));
#104148=CARTESIAN_POINT('Ctrl Pts',(-8.85985428385718,24.4530859739321,
3.79524659805779));
#104149=CARTESIAN_POINT('Ctrl Pts',(-8.86055512015956,24.4528968753134,
3.79793988269276));
#104150=CARTESIAN_POINT('Ctrl Pts',(-8.86216722315777,24.45246898817,3.80404623514055));
#104151=CARTESIAN_POINT('Ctrl Pts',(-8.86308430442793,24.4522305354783,
3.80745770951602));
#104152=CARTESIAN_POINT('Ctrl Pts',(-8.86550146617423,24.4516145638811,
3.81629065868477));
#104153=CARTESIAN_POINT('Ctrl Pts',(-8.86702508342782,24.4512383413307,
3.82170568153532));
#104154=CARTESIAN_POINT('Ctrl Pts',(-8.87743453692639,24.4487448876755,
3.85771007281686));
#104155=CARTESIAN_POINT('Ctrl Pts',(-8.88752031353462,24.4466898726167,
3.88794210014765));
#104156=CARTESIAN_POINT('Ctrl Pts',(-8.90988361725549,24.4426918637017,
3.94689396370194));
#104157=CARTESIAN_POINT('Ctrl Pts',(-8.92210130103532,24.4407489850332,
3.97560752330536));
#104158=CARTESIAN_POINT('Ctrl Pts',(-8.96534164812484,24.4344837771879,
4.06697596633123));
#104159=CARTESIAN_POINT('Ctrl Pts',(-9.00080025394839,24.4302040522692,
4.12735871889088));
#104160=CARTESIAN_POINT('Ctrl Pts',(-9.05506728485749,24.4242709184256,
4.2033850162583));
#104161=CARTESIAN_POINT('Ctrl Pts',(-9.06930227533093,24.422761251279,4.22211491838378));
#104162=CARTESIAN_POINT('Ctrl Pts',(-9.09461263305664,24.4201423493734,
4.25342488786535));
#104163=CARTESIAN_POINT('Ctrl Pts',(-9.10541341805402,24.4190434348606,
4.26621808095122));
#104164=CARTESIAN_POINT('Ctrl Pts',(-9.12112824306675,24.4174677930225,
4.28404646106886));
#104165=CARTESIAN_POINT('Ctrl Pts',(-9.12582067659058,24.4170001276418,
4.2892749363753));
#104166=CARTESIAN_POINT('Ctrl Pts',(-9.13400433839749,24.4161891490678,
4.29823095386762));
#104167=CARTESIAN_POINT('Ctrl Pts',(-9.13747359043889,24.4158467605432,
4.3019783868873));
#104168=CARTESIAN_POINT('Ctrl Pts',(-9.14417562802156,24.4151879279886,
4.30912403537428));
#104169=CARTESIAN_POINT('Ctrl Pts',(-9.14740456327196,24.4148716513653,
4.31252574141736));
#104170=CARTESIAN_POINT('Ctrl Pts',(-9.1550555144395,24.4141248407655,4.3204902507853));
#104171=CARTESIAN_POINT('Ctrl Pts',(-9.15949427059681,24.4136935910788,
4.3250366970065));
#104172=CARTESIAN_POINT('Ctrl Pts',(-9.17280307358579,24.4124063638712,
4.33844951855604));
#104173=CARTESIAN_POINT('Ctrl Pts',(-9.18177795118553,24.4115458360644,
4.34721013213532));
#104174=CARTESIAN_POINT('Ctrl Pts',(-9.26170169013972,24.4039450928261,
4.42277114416103));
#104175=CARTESIAN_POINT('Ctrl Pts',(-9.34053466081499,24.3968245810713,
4.48065739024635));
#104176=CARTESIAN_POINT('Ctrl Pts',(-9.47848218459731,24.3852336643963,
4.55772757507243));
#104177=CARTESIAN_POINT('Ctrl Pts',(-9.53360231003288,24.3808074611513,
4.58316358829024));
#104178=CARTESIAN_POINT('Ctrl Pts',(-9.59730119746411,24.3760775846879,
4.60678917022509));
#104179=CARTESIAN_POINT('Ctrl Pts',(-9.60418479230835,24.3755713750257,
4.6092695438965));
#104180=CARTESIAN_POINT('Ctrl Pts',(-9.61445181787299,24.3748241033848,
4.61286132882159));
#104181=CARTESIAN_POINT('Ctrl Pts',(-9.61781773621291,24.3745803499737,
4.61402174844764));
#104182=CARTESIAN_POINT('Ctrl Pts',(-9.62358785230638,24.3741646535518,
4.61598179935642));
#104183=CARTESIAN_POINT('Ctrl Pts',(-9.62598942904145,24.3739922780917,
4.61678895710871));
#104184=CARTESIAN_POINT('Ctrl Pts',(-9.63143555399285,24.3736028428096,
4.61859983362698));
#104185=CARTESIAN_POINT('Ctrl Pts',(-9.63448161013199,24.373386056207,4.61959887724968));
#104186=CARTESIAN_POINT('Ctrl Pts',(-9.64276246156687,24.3727993996682,
4.62227742854087));
#104187=CARTESIAN_POINT('Ctrl Pts',(-9.64800507924434,24.3724308948974,
4.62393276674868));
#104188=CARTESIAN_POINT('Ctrl Pts',(-9.67387049230317,24.3706262073116,
4.63190094452035));
#104189=CARTESIAN_POINT('Ctrl Pts',(-9.69465388351345,24.3692178779321,
4.63768365346537));
#104190=CARTESIAN_POINT('Ctrl Pts',(-9.73706102257202,24.3664063569308,
4.64823686467416));
#104191=CARTESIAN_POINT('Ctrl Pts',(-9.75868360882956,24.3650048173268,
4.65297497861202));
#104192=CARTESIAN_POINT('Ctrl Pts',(-9.87832533580387,24.357362894595,4.67567825337601));
#104193=CARTESIAN_POINT('Ctrl Pts',(-9.97818090239306,24.3513614706143,
4.68175654317401));
#104194=CARTESIAN_POINT('Ctrl Pts',(-10.1051429738336,24.3432064532232,
4.67337177083322));
#104195=CARTESIAN_POINT('Ctrl Pts',(-10.132600255881,24.3414141115809,4.67058674967412));
#104196=CARTESIAN_POINT('Ctrl Pts',(-10.1683087617237,24.3390334699319,
4.66569236838154));
#104197=CARTESIAN_POINT('Ctrl Pts',(-10.1766719156577,24.3384723469898,
4.6644541918869));
#104198=CARTESIAN_POINT('Ctrl Pts',(-10.190343552091,24.3375488883831,4.66227941686375));
#104199=CARTESIAN_POINT('Ctrl Pts',(-10.1956603155959,24.3371882323909,
4.66139620713384));
#104200=CARTESIAN_POINT('Ctrl Pts',(-10.2059518599833,24.3364870601956,
4.65961392255995));
#104201=CARTESIAN_POINT('Ctrl Pts',(-10.210927290817,24.3361466896402,4.65871924754895));
#104202=CARTESIAN_POINT('Ctrl Pts',(-10.2224375582474,24.3353559716996,
4.65657289657576));
#104203=CARTESIAN_POINT('Ctrl Pts',(-10.2289678023463,24.3349048954224,
4.65529782945498));
#104204=CARTESIAN_POINT('Ctrl Pts',(-10.2502297358889,24.3334279581042,
4.65095896885672));
#104205=CARTESIAN_POINT('Ctrl Pts',(-10.2649130588474,24.3323949828224,
4.64766828982858));
#104206=CARTESIAN_POINT('Ctrl Pts',(-10.3587882224366,24.3257038638226,
4.62473247398366));
#104207=CARTESIAN_POINT('Ctrl Pts',(-10.4358065826944,24.3197911702094,
4.59718737828363));
#104208=CARTESIAN_POINT('Ctrl Pts',(-10.5584952957335,24.3098035278222,
4.53833970052955));
#104209=CARTESIAN_POINT('Ctrl Pts',(-10.6059498155291,24.3057875353895,
4.51138109818273));
#104210=CARTESIAN_POINT('Ctrl Pts',(-10.6647965237534,24.3007230571944,
4.47231704075621));
#104211=CARTESIAN_POINT('Ctrl Pts',(-10.6780412340188,24.2995775363267,
4.46312770991178));
#104212=CARTESIAN_POINT('Ctrl Pts',(-10.6998105800994,24.2976902994671,
4.44735215117807));
#104213=CARTESIAN_POINT('Ctrl Pts',(-10.7084407374898,24.2969409341223,
4.44091587747201));
#104214=CARTESIAN_POINT('Ctrl Pts',(-10.7202705833178,24.2959134049267,
4.43183825534769));
#104215=CARTESIAN_POINT('Ctrl Pts',(-10.7235460771481,24.2956288631527,
4.42929721988055));
#104216=CARTESIAN_POINT('Ctrl Pts',(-10.7290720604629,24.2951488572233,
4.4249633889364));
#104217=CARTESIAN_POINT('Ctrl Pts',(-10.7313295018371,24.2949527786357,
4.42317956033893));
#104218=CARTESIAN_POINT('Ctrl Pts',(-10.7356480371724,24.2945777307675,
4.41974127489869));
#104219=CARTESIAN_POINT('Ctrl Pts',(-10.7377101217449,24.2943986680624,
4.41808813518947));
#104220=CARTESIAN_POINT('Ctrl Pts',(-10.7426440921362,24.2939702259037,
4.41410529468319));
#104221=CARTESIAN_POINT('Ctrl Pts',(-10.7455106271219,24.2937213122776,
4.4117689636762));
#104222=CARTESIAN_POINT('Ctrl Pts',(-10.7558922725725,24.2928196379011,
4.40322584877651));
#104223=CARTESIAN_POINT('Ctrl Pts',(-10.7633415182733,24.2921722834478,
4.39693913023562));
#104224=CARTESIAN_POINT('Ctrl Pts',(-10.8170872479234,24.2874916293172,
4.35042629776266));
#104225=CARTESIAN_POINT('Ctrl Pts',(-10.8602630555789,24.2836735960284,
4.30672544048429));
#104226=CARTESIAN_POINT('Ctrl Pts',(-10.9429776746966,24.2757374633022,
4.20877233243274));
#104227=CARTESIAN_POINT('Ctrl Pts',(-10.9816825631639,24.2716341345672,
4.15411301328122));
#104228=CARTESIAN_POINT('Ctrl Pts',(-11.0331112299902,24.265178722192,4.06655092375093));
#104229=CARTESIAN_POINT('Ctrl Pts',(-11.0493500838197,24.2629387020381,
4.03587573431201));
#104230=CARTESIAN_POINT('Ctrl Pts',(-11.0681129690451,24.260050307342,3.99629904144079));
#104231=CARTESIAN_POINT('Ctrl Pts',(-11.0719197916083,24.2594464064131,
3.98802254641771));
#104232=CARTESIAN_POINT('Ctrl Pts',(-11.0778816794069,24.258470794376,3.9746543011807));
#104233=CARTESIAN_POINT('Ctrl Pts',(-11.0800976217184,24.2581011590103,
3.96958997669834));
#104234=CARTESIAN_POINT('Ctrl Pts',(-11.0842505095648,24.25739475823,3.95991402722388));
#104235=CARTESIAN_POINT('Ctrl Pts',(-11.0861938946848,24.2570582195747,
3.95530528411999));
#104236=CARTESIAN_POINT('Ctrl Pts',(-11.0905708013905,24.2562863318043,
3.94473791837185));
#104237=CARTESIAN_POINT('Ctrl Pts',(-11.0929849340541,24.2558503434936,
3.93877148944935));
#104238=CARTESIAN_POINT('Ctrl Pts',(-11.1003103474507,24.2544948382353,
3.92023138508594));
#104239=CARTESIAN_POINT('Ctrl Pts',(-11.1050543047041,24.2535698120514,
3.90759322241757));
#104240=CARTESIAN_POINT('Ctrl Pts',(-11.1436710583243,24.2456157496913,
3.79908247855799));
#104241=CARTESIAN_POINT('Ctrl Pts',(-11.1652068601323,24.2381670520375,
3.69929427076204));
#104242=CARTESIAN_POINT('Ctrl Pts',(-11.1784864565149,24.2264595884829,
3.54027072943912));
#104243=CARTESIAN_POINT('Ctrl Pts',(-11.1790413562769,24.2222348213543,
3.4822477865585));
#104244=CARTESIAN_POINT('Ctrl Pts',(-11.174858617989,24.2176978845472,3.41720856954971));
#104245=CARTESIAN_POINT('Ctrl Pts',(-11.1743289768438,24.2171983687719,
3.41000747855053));
#104246=CARTESIAN_POINT('Ctrl Pts',(-11.1734418367923,24.2164598111208,
3.39929360219905));
#104247=CARTESIAN_POINT('Ctrl Pts',(-11.1731347264072,24.2162181376278,
3.39577698232172));
#104248=CARTESIAN_POINT('Ctrl Pts',(-11.1725811076617,24.2158053088983,
3.38975042692776));
#104249=CARTESIAN_POINT('Ctrl Pts',(-11.1723423443561,24.2156337310799,
3.38723985426329));
#104250=CARTESIAN_POINT('Ctrl Pts',(-11.1717815771572,24.215244960192,3.3815378271182));
#104251=CARTESIAN_POINT('Ctrl Pts',(-11.1714545989229,24.2150280461342,
3.37834691022124));
#104252=CARTESIAN_POINT('Ctrl Pts',(-11.1705298386934,24.2144399985982,
3.36967199072267));
#104253=CARTESIAN_POINT('Ctrl Pts',(-11.1699065480027,24.2140702453971,
3.3641907028999));
#104254=CARTESIAN_POINT('Ctrl Pts',(-11.1666246857412,24.212246184056,3.33703092392216));
#104255=CARTESIAN_POINT('Ctrl Pts',(-11.1634017743239,24.2108205077062,
3.31542335974056));
#104256=CARTESIAN_POINT('Ctrl Pts',(-11.1557157619461,24.2079959327418,
3.27217615644928));
#104257=CARTESIAN_POINT('Ctrl Pts',(-11.151241214385,24.2065980635236,3.25054782031563));
#104258=CARTESIAN_POINT('Ctrl Pts',(-11.1232762191888,24.1989722249328,
3.1322484195828));
#104259=CARTESIAN_POINT('Ctrl Pts',(-11.088220324039,24.1929809626272,3.03873249527051));
#104260=CARTESIAN_POINT('Ctrl Pts',(-11.028941951065,24.1848351983103,2.92629557063618));
#104261=CARTESIAN_POINT('Ctrl Pts',(-11.0152026045046,24.1830406777031,
2.90231965838381));
#104262=CARTESIAN_POINT('Ctrl Pts',(-10.9961731016209,24.1806575421282,
2.87166430001134));
#104263=CARTESIAN_POINT('Ctrl Pts',(-10.9916351406955,24.1800961895335,
2.86452667891526));
#104264=CARTESIAN_POINT('Ctrl Pts',(-10.9840798939414,24.1791724601592,
2.85292127145348));
#104265=CARTESIAN_POINT('Ctrl Pts',(-10.9811080588686,24.1788117655393,
2.84842414580067));
#104266=CARTESIAN_POINT('Ctrl Pts',(-10.9752897878399,24.1781105950015,
2.83974971178937));
#104267=CARTESIAN_POINT('Ctrl Pts',(-10.9724471191786,24.1777702652364,
2.83557000942539));
#104268=CARTESIAN_POINT('Ctrl Pts',(-10.9658018196126,24.1769797533639,
2.82593312819351));
#104269=CARTESIAN_POINT('Ctrl Pts',(-10.9619797204256,24.1765288433951,
2.82048964925511));
#104270=CARTESIAN_POINT('Ctrl Pts',(-10.9493682636117,24.1750529204122,
2.80284792968513));
#104271=CARTESIAN_POINT('Ctrl Pts',(-10.9403917085939,24.1740208074746,
2.79078599342776));
#104272=CARTESIAN_POINT('Ctrl Pts',(-10.8814272828743,24.1673529998721,
2.7146427605901));
#104273=CARTESIAN_POINT('Ctrl Pts',(-10.8251590871369,24.1614650438022,
2.65572043733789));
#104274=CARTESIAN_POINT('Ctrl Pts',(-10.721744802459,24.1515002652096,2.56771512893189));
#104275=CARTESIAN_POINT('Ctrl Pts',(-10.6777945409312,24.1474819509128,
2.53528979877945));
#104276=CARTESIAN_POINT('Ctrl Pts',(-10.6181464308509,24.1424147791954,
2.49737844406073));
#104277=CARTESIAN_POINT('Ctrl Pts',(-10.6043628919056,24.1412690152447,
2.48901011670976));
#104278=CARTESIAN_POINT('Ctrl Pts',(-10.5810937382364,24.1393813318692,
2.47552887568332));
#104279=CARTESIAN_POINT('Ctrl Pts',(-10.5717022884101,24.1386317721532,
2.47025851242008));
#104280=CARTESIAN_POINT('Ctrl Pts',(-10.5585945231385,24.1376038693147,
2.46313721822583));
#104281=CARTESIAN_POINT('Ctrl Pts',(-10.5549390746922,24.1373191535429,
2.4611761967489));
#104282=CARTESIAN_POINT('Ctrl Pts',(-10.5487286491935,24.1368388131403,
2.45788665499965));
#104283=CARTESIAN_POINT('Ctrl Pts',(-10.5461790436348,24.1366425742519,
2.45654812893116));
#104284=CARTESIAN_POINT('Ctrl Pts',(-10.541277090975,24.1362671492125,2.45399752607333));
#104285=CARTESIAN_POINT('Ctrl Pts',(-10.5389255431997,24.1360878699456,
2.45278401276746));
#104286=CARTESIAN_POINT('Ctrl Pts',(-10.5332729265085,24.135658833079,2.4498910696929));
#104287=CARTESIAN_POINT('Ctrl Pts',(-10.52996796064,24.1354095424291,2.44821925227834));
#104288=CARTESIAN_POINT('Ctrl Pts',(-10.5179145463092,24.1345058191473,
2.44219327030303));
#104289=CARTESIAN_POINT('Ctrl Pts',(-10.5091195866238,24.1338568152216,
2.43793229193465));
#104290=CARTESIAN_POINT('Ctrl Pts',(-10.4455584040963,24.1292335402041,
2.40810924459237));
#104291=CARTESIAN_POINT('Ctrl Pts',(-10.3889420389112,24.1254677652967,
2.38668345425721));
#104292=CARTESIAN_POINT('Ctrl Pts',(-10.2661655423819,24.1175459860524,
2.35073756470135));
#104293=CARTESIAN_POINT('Ctrl Pts',(-10.1999009423255,24.1134062802498,
2.33737914950645));
#104294=CARTESIAN_POINT('Ctrl Pts',(-10.0982076998485,24.1069008963359,
2.32583370260708));
#104295=CARTESIAN_POINT('Ctrl Pts',(-10.063401842772,24.1046495063003,2.32344099761911));
#104296=CARTESIAN_POINT('Ctrl Pts',(-10.0194159832921,24.1017479459793,
2.32237465938294));
#104297=CARTESIAN_POINT('Ctrl Pts',(-10.0102864085954,24.1011426970592,
2.32225953398003));
#104298=CARTESIAN_POINT('Ctrl Pts',(-9.99562078069965,24.1001651928335,
2.32224513138096));
#104299=CARTESIAN_POINT('Ctrl Pts',(-9.99008504743967,24.0997950225358,
2.32227872565096));
#104300=CARTESIAN_POINT('Ctrl Pts',(-9.97954409971858,24.0990877825575,
2.32241701763618));
#104301=CARTESIAN_POINT('Ctrl Pts',(-9.9745389007896,24.0987509411749,2.32251460505739));
#104302=CARTESIAN_POINT('Ctrl Pts',(-9.96309843183033,24.0979786130508,
2.32281064054415));
#104303=CARTESIAN_POINT('Ctrl Pts',(-9.9566639092263,24.097542488493,2.32302995189951));
#104304=CARTESIAN_POINT('Ctrl Pts',(-9.93675454604167,24.0961874904716,
2.32387201741309));
#104305=CARTESIAN_POINT('Ctrl Pts',(-9.92328877352544,24.0952631240218,
2.3246735005663));
#104306=CARTESIAN_POINT('Ctrl Pts',(-9.87674450865754,24.0920394019108,
2.32824707018164));
#104307=CARTESIAN_POINT('Ctrl Pts',(-9.8438033470503,24.0897070781581,2.3321836006));
#104308=CARTESIAN_POINT('Ctrl Pts',(-9.81110406371069,24.0873412831715,
2.3374969300026));
#104309=CARTESIAN_POINT('Ctrl Pts',(-9.8111040637107,23.9889087884094,2.3374969300026));
#104310=CARTESIAN_POINT('Ctrl Pts',(-9.81191529024896,23.9889636364787,
2.33736511323545));
#104311=CARTESIAN_POINT('Ctrl Pts',(-9.81272665881509,23.9890184414769,
2.33723414495445));
#104312=CARTESIAN_POINT('Ctrl Pts',(-9.84172904331265,23.9909755864873,
2.33258382552641));
#104313=CARTESIAN_POINT('Ctrl Pts',(-9.87007769787267,23.9928258615754,
2.32908978796103));
#104314=CARTESIAN_POINT('Ctrl Pts',(-9.97499901218653,23.9995357008595,
2.32001627997921));
#104315=CARTESIAN_POINT('Ctrl Pts',(-10.0519381221756,24.0041966484075,
2.32089410523933));
#104316=CARTESIAN_POINT('Ctrl Pts',(-10.1886920676342,24.0127588545096,
2.33587475697394));
#104317=CARTESIAN_POINT('Ctrl Pts',(-10.2485237563857,24.0166018568367,
2.34716578101397));
#104318=CARTESIAN_POINT('Ctrl Pts',(-10.3166652259444,24.0212397627773,
2.36557763965318));
#104319=CARTESIAN_POINT('Ctrl Pts',(-10.3260863158081,24.0218867679212,
2.36824973507468));
#104320=CARTESIAN_POINT('Ctrl Pts',(-10.3414665093096,24.0229530620515,
2.37281998657419));
#104321=CARTESIAN_POINT('Ctrl Pts',(-10.3474458774571,24.023370112437,2.3746487129173));
#104322=CARTESIAN_POINT('Ctrl Pts',(-10.3581652644104,24.0241224177185,
2.3780206985772));
#104323=CARTESIAN_POINT('Ctrl Pts',(-10.3629106168192,24.0244571020804,
2.37954661304432));
#104324=CARTESIAN_POINT('Ctrl Pts',(-10.3730056981297,24.025172684895,2.38286364372141));
#104325=CARTESIAN_POINT('Ctrl Pts',(-10.3783525134138,24.0255538508584,
2.38466316162746));
#104326=CARTESIAN_POINT('Ctrl Pts',(-10.3927804073928,24.026588362199,2.38963468164101));
#104327=CARTESIAN_POINT('Ctrl Pts',(-10.4018357254085,24.0272440831808,
2.39287957797434));
#104328=CARTESIAN_POINT('Ctrl Pts',(-10.4498670089184,24.0307574448773,
2.41075807055968));
#104329=CARTESIAN_POINT('Ctrl Pts',(-10.4880818226941,24.0336789275895,
2.42733802668741));
#104330=CARTESIAN_POINT('Ctrl Pts',(-10.6226302890315,24.0444329518062,
2.49439363666767));
#104331=CARTESIAN_POINT('Ctrl Pts',(-10.7127299581438,24.0525975143552,
2.5561119203801));
#104332=CARTESIAN_POINT('Ctrl Pts',(-10.8070925010526,24.0616903809206,
2.64206304080867));
#104333=CARTESIAN_POINT('Ctrl Pts',(-10.8207923809904,24.063024375184,2.65516031133632));
#104334=CARTESIAN_POINT('Ctrl Pts',(-10.8379217989654,24.0647038632244,
2.67234647965151));
#104335=CARTESIAN_POINT('Ctrl Pts',(-10.8416470526713,24.0650698367928,
2.67613500356579));
#104336=CARTESIAN_POINT('Ctrl Pts',(-10.8475259149516,24.0656483527517,
2.68219520539779));
#104337=CARTESIAN_POINT('Ctrl Pts',(-10.8496962698398,24.0658621420012,
2.68445042566917));
#104338=CARTESIAN_POINT('Ctrl Pts',(-10.8538069716921,24.0662674239749,
2.6887560870136));
#104339=CARTESIAN_POINT('Ctrl Pts',(-10.8557489187102,24.0664590330245,
2.69080483221791));
#104340=CARTESIAN_POINT('Ctrl Pts',(-10.8603095886263,24.066909422426,2.695651097327));
#104341=CARTESIAN_POINT('Ctrl Pts',(-10.8629220511306,24.0671677296809,
2.69845444282798));
#104342=CARTESIAN_POINT('Ctrl Pts',(-10.8715131306733,24.0680184160729,
2.7077639257757));
#104343=CARTESIAN_POINT('Ctrl Pts',(-10.8774323894889,24.0686065498161,
2.7143247823347));
#104344=CARTESIAN_POINT('Ctrl Pts',(-10.9100096679501,24.0718589289608,
2.75126059547338));
#104345=CARTESIAN_POINT('Ctrl Pts',(-10.9351671856618,24.0744299334073,
2.7829286334952));
#104346=CARTESIAN_POINT('Ctrl Pts',(-11.0235730783276,24.0839638950252,
2.90680182008208));
#104347=CARTESIAN_POINT('Ctrl Pts',(-11.0752147353238,24.0906787363243,
3.00654358945951));
#104348=CARTESIAN_POINT('Ctrl Pts',(-11.1174671347088,24.0990208610115,
3.12766277933815));
#104349=CARTESIAN_POINT('Ctrl Pts',(-11.1225780280356,24.1001044803195,
3.14336807468007));
#104350=CARTESIAN_POINT('Ctrl Pts',(-11.1292268821546,24.1016269788217,
3.16536068582546));
#104351=CARTESIAN_POINT('Ctrl Pts',(-11.1310459698255,24.1020567983486,
3.17156152276821));
#104352=CARTESIAN_POINT('Ctrl Pts',(-11.1341021067961,24.1028026432653,
3.18230573883432));
#104353=CARTESIAN_POINT('Ctrl Pts',(-11.1353631215619,24.1031178911798,
3.1868421910346));
#104354=CARTESIAN_POINT('Ctrl Pts',(-11.1379249104958,24.1037742936354,
3.19627702412192));
#104355=CARTESIAN_POINT('Ctrl Pts',(-11.1392213338658,24.1041155802914,
3.20117647501722));
#104356=CARTESIAN_POINT('Ctrl Pts',(-11.142199783399,24.104921707053,3.21273379444466));
#104357=CARTESIAN_POINT('Ctrl Pts',(-11.1438552669073,24.105387384604,3.21939824849787));
#104358=CARTESIAN_POINT('Ctrl Pts',(-11.1491435059492,24.1069355322548,
3.24151183037535));
#104359=CARTESIAN_POINT('Ctrl Pts',(-11.1525221377801,24.1080259960737,
3.25701932123866));
#104360=CARTESIAN_POINT('Ctrl Pts',(-11.1598239857355,24.1106477872416,
3.29412368946212));
#104361=CARTESIAN_POINT('Ctrl Pts',(-11.1634587080319,24.1121875447555,
3.31577063013765));
#104362=CARTESIAN_POINT('Ctrl Pts',(-11.1753706476987,24.1183102831794,
3.40128183167365));
#104363=CARTESIAN_POINT('Ctrl Pts',(-11.1790086177185,24.1230165690624,
3.46567274180069));
#104364=CARTESIAN_POINT('Ctrl Pts',(-11.1756942409554,24.1325613930551,
3.59561513165207));
#104365=CARTESIAN_POINT('Ctrl Pts',(-11.1685441374264,24.1373833301956,
3.66095184226147));
#104366=CARTESIAN_POINT('Ctrl Pts',(-11.1541277724144,24.1426625009959,
3.7349014289201));
#104367=CARTESIAN_POINT('Ctrl Pts',(-11.1521491590677,24.1433385277543,
3.74442161725159));
#104368=CARTESIAN_POINT('Ctrl Pts',(-11.149255948915,24.144263065487,3.75752570171869));
#104369=CARTESIAN_POINT('Ctrl Pts',(-11.1484421054994,24.144516810971,3.76113110578009));
#104370=CARTESIAN_POINT('Ctrl Pts',(-11.1470171253302,24.1449504145443,
3.76730836856232));
#104371=CARTESIAN_POINT('Ctrl Pts',(-11.1464142844339,24.1451307300009,
3.76988208259098));
#104372=CARTESIAN_POINT('Ctrl Pts',(-11.1451370641186,24.1455063015767,
3.77525342519396));
#104373=CARTESIAN_POINT('Ctrl Pts',(-11.1444610897819,24.1457014587139,
3.77805063911787));
#104374=CARTESIAN_POINT('Ctrl Pts',(-11.1427853326147,24.1461766221915,
3.78487535163241));
#104375=CARTESIAN_POINT('Ctrl Pts',(-11.1417744905766,24.1464560052845,
3.78890014949772));
#104376=CARTESIAN_POINT('Ctrl Pts',(-11.1380570442915,24.1474581975698,
3.8033773253675));
#104377=CARTESIAN_POINT('Ctrl Pts',(-11.1352279128659,24.1481744128238,
3.81379809423215));
#104378=CARTESIAN_POINT('Ctrl Pts',(-11.1278009076869,24.1499477201924,
3.83973830325954));
#104379=CARTESIAN_POINT('Ctrl Pts',(-11.1230255800533,24.1509964301968,
3.85520501594267));
#104380=CARTESIAN_POINT('Ctrl Pts',(-11.1006447766295,24.1555563401294,
3.92272340332944));
#104381=CARTESIAN_POINT('Ctrl Pts',(-11.0797269337279,24.1589473524532,
3.97360817774133));
#104382=CARTESIAN_POINT('Ctrl Pts',(-11.0194381504682,24.167342000269,4.09529633153584));
#104383=CARTESIAN_POINT('Ctrl Pts',(-10.9761859717322,24.1723425770645,
4.16384540049577));
#104384=CARTESIAN_POINT('Ctrl Pts',(-10.9169637275359,24.1785961981693,
4.23925572066521));
#104385=CARTESIAN_POINT('Ctrl Pts',(-10.907444081569,24.1795857399449,4.25091058282987));
#104386=CARTESIAN_POINT('Ctrl Pts',(-10.893399380992,24.1810254102074,4.2674482601571));
#104387=CARTESIAN_POINT('Ctrl Pts',(-10.8890518873859,24.1814683718461,
4.27248043629549));
#104388=CARTESIAN_POINT('Ctrl Pts',(-10.8813277272416,24.1822508620973,
4.28126948771694));
#104389=CARTESIAN_POINT('Ctrl Pts',(-10.8779690424634,24.182589644258,4.28504199528249));
#104390=CARTESIAN_POINT('Ctrl Pts',(-10.8709806206956,24.1832916125095,
4.29279051687329));
#104391=CARTESIAN_POINT('Ctrl Pts',(-10.8673476865037,24.1836549277722,
4.29676347451588));
#104392=CARTESIAN_POINT('Ctrl Pts',(-10.8579487165592,24.184590889867,4.30690167835532));
#104393=CARTESIAN_POINT('Ctrl Pts',(-10.8521434878504,24.1851651907578,
4.3130300046301));
#104394=CARTESIAN_POINT('Ctrl Pts',(-10.8271375366571,24.1876235091398,
4.33886565849901));
#104395=CARTESIAN_POINT('Ctrl Pts',(-10.8073166493765,24.189534199184,4.35795786992865));
#104396=CARTESIAN_POINT('Ctrl Pts',(-10.7128009902719,24.198483481559,4.44282170940828));
#104397=CARTESIAN_POINT('Ctrl Pts',(-10.6306340208212,24.2058659765903,
4.49964634278999));
#104398=CARTESIAN_POINT('Ctrl Pts',(-10.5227216164905,24.2147272092718,
4.55562535048993));
#104399=CARTESIAN_POINT('Ctrl Pts',(-10.5028350691704,24.2163265857171,
4.5652416419023));
#104400=CARTESIAN_POINT('Ctrl Pts',(-10.4626914948827,24.2194747874122,
4.58327848382458));
#104401=CARTESIAN_POINT('Ctrl Pts',(-10.4424454050007,24.2210233204887,
4.59170412995736));
#104402=CARTESIAN_POINT('Ctrl Pts',(-10.4168196816447,24.2229248666298,
4.60153842403963));
#104403=CARTESIAN_POINT('Ctrl Pts',(-10.411651012751,24.2233054738132,4.60348040007461));
#104404=CARTESIAN_POINT('Ctrl Pts',(-10.4034583209276,24.2239039286604,
4.60649298863004));
#104405=CARTESIAN_POINT('Ctrl Pts',(-10.4004433342001,24.2241231365364,
4.60758768832645));
#104406=CARTESIAN_POINT('Ctrl Pts',(-10.395049705165,24.2245134033883,4.60952113720498));
#104407=CARTESIAN_POINT('Ctrl Pts',(-10.3926728531371,24.2246847301414,
4.6103645590727));
#104408=CARTESIAN_POINT('Ctrl Pts',(-10.3869632402317,24.2250947371436,
4.61236997896257));
#104409=CARTESIAN_POINT('Ctrl Pts',(-10.3836279463389,24.2253329859171,
4.61352463780255));
#104410=CARTESIAN_POINT('Ctrl Pts',(-10.373462612011,24.2260554437884,4.61699272153963));
#104411=CARTESIAN_POINT('Ctrl Pts',(-10.3666163143677,24.2265369773123,
4.61925848087774));
#104412=CARTESIAN_POINT('Ctrl Pts',(-10.2940548524148,24.2315918070207,
4.64253520452934));
#104413=CARTESIAN_POINT('Ctrl Pts',(-10.2266249458674,24.2358723645131,
4.65779920550411));
#104414=CARTESIAN_POINT('Ctrl Pts',(-10.0703481299661,24.2456276582886,
4.67898802644893));
#104415=CARTESIAN_POINT('Ctrl Pts',(-9.98140506213337,24.2510804180271,
4.68093760653492));
#104416=CARTESIAN_POINT('Ctrl Pts',(-9.87841685996031,24.2578286773854,
4.67155012466697));
#104417=CARTESIAN_POINT('Ctrl Pts',(-9.86377060047379,24.2587979480084,
4.66993746571443));
#104418=CARTESIAN_POINT('Ctrl Pts',(-9.84261795209693,24.260213427659,4.66720583096438));
#104419=CARTESIAN_POINT('Ctrl Pts',(-9.83608426693785,24.2606528087374,
4.66630621635849));
#104420=CARTESIAN_POINT('Ctrl Pts',(-9.82456899746088,24.2614311719526,
4.66462202214448));
#104421=CARTESIAN_POINT('Ctrl Pts',(-9.81958420850442,24.2617694330122,
4.66386022869601));
#104422=CARTESIAN_POINT('Ctrl Pts',(-9.80926497968736,24.2624724895564,
4.66221531988234));
#104423=CARTESIAN_POINT('Ctrl Pts',(-9.80393143145864,24.2628374274638,
4.66132743551747));
#104424=CARTESIAN_POINT('Ctrl Pts',(-9.79018358906478,24.2637822218593,
4.65894140482426));
#104425=CARTESIAN_POINT('Ctrl Pts',(-9.78177927292031,24.2643637922863,
4.65738835905638));
#104426=CARTESIAN_POINT('Ctrl Pts',(-9.74541060061829,24.2668983584304,
4.65025753844924));
#104427=CARTESIAN_POINT('Ctrl Pts',(-9.7176391828448,24.2688801271902,4.64375709536075));
#104428=CARTESIAN_POINT('Ctrl Pts',(-9.5948034139582,24.2778612078305,4.61025869106878));
#104429=CARTESIAN_POINT('Ctrl Pts',(-9.503133469902,24.2851936833931,4.57236962114452));
#104430=CARTESIAN_POINT('Ctrl Pts',(-9.38105678563893,24.2954296788097,
4.50286723195353));
#104431=CARTESIAN_POINT('Ctrl Pts',(-9.34594086655984,24.2984298107287,
4.48032690123639));
#104432=CARTESIAN_POINT('Ctrl Pts',(-9.30724293608549,24.3017431118799,
4.45248012518211));
#104433=CARTESIAN_POINT('Ctrl Pts',(-9.30242124055299,24.3021560575304,
4.4489544860329));
#104434=CARTESIAN_POINT('Ctrl Pts',(-9.29473930253434,24.3028138786995,
4.44324723573708));
#104435=CARTESIAN_POINT('Ctrl Pts',(-9.29186194567442,24.3030602536743,
4.44108899472839));
#104436=CARTESIAN_POINT('Ctrl Pts',(-9.28676129659575,24.3034968983908,
4.43722647281982));
#104437=CARTESIAN_POINT('Ctrl Pts',(-9.28453414621374,24.3036875174806,
4.43552740316397));
#104438=CARTESIAN_POINT('Ctrl Pts',(-9.27975323057566,24.3040966156015,
4.43185303369437));
#104439=CARTESIAN_POINT('Ctrl Pts',(-9.2772015164985,24.3043149128093,4.42987517342508));
#104440=CARTESIAN_POINT('Ctrl Pts',(-9.27012279949983,24.3049204527922,
4.42434164157424));
#104441=CARTESIAN_POINT('Ctrl Pts',(-9.26561360709267,24.3053061414466,
4.4207631766241));
#104442=CARTESIAN_POINT('Ctrl Pts',(-9.2392060405879,24.3075658400765,4.39948889934357));
#104443=CARTESIAN_POINT('Ctrl Pts',(-9.21791966020004,24.3093912876951,
4.38104390819895));
#104444=CARTESIAN_POINT('Ctrl Pts',(-9.14289506408989,24.3159271951498,
4.31116965183271));
#104445=CARTESIAN_POINT('Ctrl Pts',(-9.09339600043173,24.3204503386145,
4.25544413312255));
#104446=CARTESIAN_POINT('Ctrl Pts',(-9.01202441224111,24.3290167748111,
4.14422301126975));
#104447=CARTESIAN_POINT('Ctrl Pts',(-8.97877066676186,24.3330180236281,
4.09009158106499));
#104448=CARTESIAN_POINT('Ctrl Pts',(-8.94558002571878,24.3378315387344,
4.02477657225738));
#104449=CARTESIAN_POINT('Ctrl Pts',(-8.94123149980395,24.3384817836427,
4.01594688326271));
#104450=CARTESIAN_POINT('Ctrl Pts',(-8.93429513935819,24.3395524271792,
4.00140553972513));
#104451=CARTESIAN_POINT('Ctrl Pts',(-8.93164129360405,24.3399705582732,
3.99572576810771));
#104452=CARTESIAN_POINT('Ctrl Pts',(-8.92695756794208,24.3407241724259,
3.98548932293499));
#104453=CARTESIAN_POINT('Ctrl Pts',(-8.9249110376468,24.3410590784532,3.98094039692475));
#104454=CARTESIAN_POINT('Ctrl Pts',(-8.92061417091324,24.3417744453672,
3.97122505188383));
#104455=CARTESIAN_POINT('Ctrl Pts',(-8.91837190116292,24.342155169453,3.966055223606));
#104456=CARTESIAN_POINT('Ctrl Pts',(-8.91241692689779,24.3431867626496,
3.95205083106616));
#104457=CARTESIAN_POINT('Ctrl Pts',(-8.90877487370587,24.343839982006,3.94318687825367));
#104458=CARTESIAN_POINT('Ctrl Pts',(-8.890109885129,24.3473097340914,3.89613504604175));
#104459=CARTESIAN_POINT('Ctrl Pts',(-8.87698397865023,24.3501881860563,
3.85723011591546));
#104460=CARTESIAN_POINT('Ctrl Pts',(-8.83803160479263,24.3605111905588,
3.71819327413174));
#104461=CARTESIAN_POINT('Ctrl Pts',(-8.82337406762189,24.3682506968201,
3.61544043113425));
#104462=CARTESIAN_POINT('Ctrl Pts',(-8.82206404542765,24.3773963265622,
3.48795472708509));
#104463=CARTESIAN_POINT('Ctrl Pts',(-8.82255861041381,24.3791060169908,
3.46380370478829));
#104464=CARTESIAN_POINT('Ctrl Pts',(-8.82408714899806,24.381174854874,3.43399658779826));
#104465=CARTESIAN_POINT('Ctrl Pts',(-8.82441999866294,24.3815675345662,
3.42831215364252));
#104466=CARTESIAN_POINT('Ctrl Pts',(-8.8250074128629,24.3821807442675,3.41938964404949));
#104467=CARTESIAN_POINT('Ctrl Pts',(-8.82523416205303,24.3824027440407,
3.41614991977712));
#104468=CARTESIAN_POINT('Ctrl Pts',(-8.82567904546122,24.3828126220791,
3.41014999161365));
#104469=CARTESIAN_POINT('Ctrl Pts',(-8.82589351054565,24.3830006912897,
3.40738963363798));
#104470=CARTESIAN_POINT('Ctrl Pts',(-8.82640968761386,24.3834324359487,
3.40103615878903));
#104471=CARTESIAN_POINT('Ctrl Pts',(-8.82671816705856,24.3836757339303,
3.39744365181161));
#104472=CARTESIAN_POINT('Ctrl Pts',(-8.82772930759005,24.3844300184669,
3.38627028580868));
#104473=CARTESIAN_POINT('Ctrl Pts',(-8.8284889965435,24.384937968062,3.37869459828809));
#104474=CARTESIAN_POINT('Ctrl Pts',(-8.83044156344638,24.3861202274647,
3.36095760769738));
#104475=CARTESIAN_POINT('Ctrl Pts',(-8.83169349994172,24.3867916629658,
3.35080328051745));
#104476=CARTESIAN_POINT('Ctrl Pts',(-8.83661329461588,24.3891590559477,
3.31477189462154));
#104477=CARTESIAN_POINT('Ctrl Pts',(-8.84101012210147,24.3908245986558,
3.28900064600185));
#104478=CARTESIAN_POINT('Ctrl Pts',(-8.86277904510676,24.3976472359572,
3.18285033400713));
#104479=CARTESIAN_POINT('Ctrl Pts',(-8.88768594380953,24.4026239926642,
3.10425542019625));
#104480=CARTESIAN_POINT('Ctrl Pts',(-8.93884366034744,24.4106652551332,
2.98704032478918));
#104481=CARTESIAN_POINT('Ctrl Pts',(-8.95952683311905,24.4135854895129,
2.94628956197865));
#104482=CARTESIAN_POINT('Ctrl Pts',(-8.98762379648753,24.4172555736018,
2.89809292741013));
#104483=CARTESIAN_POINT('Ctrl Pts',(-8.99283873979115,24.4179258958574,
2.88940693841259));
#104484=CARTESIAN_POINT('Ctrl Pts',(-9.00121937018993,24.4189869698737,
2.8758477214116));
#104485=CARTESIAN_POINT('Ctrl Pts',(-9.00431025744655,24.4193749994365,
2.87092866233433));
#104486=CARTESIAN_POINT('Ctrl Pts',(-9.01008422527972,24.4200939320146,
2.86188872424522));
#104487=CARTESIAN_POINT('Ctrl Pts',(-9.01275697642874,24.4204244490011,
2.85776137422834));
#104488=CARTESIAN_POINT('Ctrl Pts',(-9.01874523034053,24.4211600364058,
2.84863982828143));
#104489=CARTESIAN_POINT('Ctrl Pts',(-9.02207315595482,24.4215655630385,
2.84365399241824));
#104490=CARTESIAN_POINT('Ctrl Pts',(-9.03177626224032,24.4227387606132,
2.8293546098887));
#104491=CARTESIAN_POINT('Ctrl Pts',(-9.03824729854296,24.4235100134031,
2.82010723535407));
#104492=CARTESIAN_POINT('Ctrl Pts',(-9.09326260967914,24.4299779948076,
2.74384539671418));
#104493=CARTESIAN_POINT('Ctrl Pts',(-9.14860328150742,24.4359460769373,
2.68203848534737));
#104494=CARTESIAN_POINT('Ctrl Pts',(-9.26704529509314,24.4476577550002,
2.57490567406071));
#104495=CARTESIAN_POINT('Ctrl Pts',(-9.32907179068441,24.4533545926746,
2.52898020952262));
#104496=CARTESIAN_POINT('Ctrl Pts',(-9.40308516353879,24.4593926849135,
2.4846806186782));
#104497=CARTESIAN_POINT('Ctrl Pts',(-9.41108482824211,24.4600359119414,
2.48001975416346));
#104498=CARTESIAN_POINT('Ctrl Pts',(-9.42229269438758,24.4609232531667,
2.47366551515474));
#104499=CARTESIAN_POINT('Ctrl Pts',(-9.42545475454424,24.4611720819424,
2.47189204480144));
#104500=CARTESIAN_POINT('Ctrl Pts',(-9.43091896944154,24.4615994006953,
2.468860472488));
#104501=CARTESIAN_POINT('Ctrl Pts',(-9.43321720788587,24.4617783208176,
2.46759542259409));
#104502=CARTESIAN_POINT('Ctrl Pts',(-9.43805940247676,24.4621535608969,
2.46495111172499));
#104503=CARTESIAN_POINT('Ctrl Pts',(-9.44060424744939,24.4623497694241,
2.46357352957027));
#104504=CARTESIAN_POINT('Ctrl Pts',(-9.4468840481462,24.4628315472717,2.46020399903846));
#104505=CARTESIAN_POINT('Ctrl Pts',(-9.45062476116366,24.463116451531,2.458222755026));
#104506=CARTESIAN_POINT('Ctrl Pts',(-9.46444467316649,24.464161687603,2.45099826826977));
#104507=CARTESIAN_POINT('Ctrl Pts',(-9.47458929777979,24.4649146582012,
2.44588057652014));
#104508=CARTESIAN_POINT('Ctrl Pts',(-9.54715197539782,24.4702110383263,
2.41058253436047));
#104509=CARTESIAN_POINT('Ctrl Pts',(-9.61206200005963,24.4744881663096,
2.38581490445392));
#104510=CARTESIAN_POINT('Ctrl Pts',(-9.72232003540705,24.4815720685054,
2.35455823863656));
#104511=CARTESIAN_POINT('Ctrl Pts',(-9.76650114682695,24.4843643460958,
2.34474448913894));
#104512=CARTESIAN_POINT('Ctrl Pts',(-9.81110406371068,24.4872084044306,
2.3374969300026));
#104513=CARTESIAN_POINT('Origin',(-10.,12.3756328852638,3.5));
#104514=CARTESIAN_POINT('',(-8.88740821192766,24.85,3.88630891215967));
#104515=CARTESIAN_POINT('Ctrl Pts',(-9.81110406371068,24.4872084044306,
2.3374969300026));
#104516=CARTESIAN_POINT('Ctrl Pts',(-9.84744767330581,24.4895258166764,
2.33159143147981));
#104517=CARTESIAN_POINT('Ctrl Pts',(-9.88407135600494,24.4918772584382,
2.32738971255254));
#104518=CARTESIAN_POINT('Ctrl Pts',(-9.93585211116218,24.4952622625889,
2.32390221340624));
#104519=CARTESIAN_POINT('Ctrl Pts',(-9.9508652393094,24.4962506731116,2.32317941167113));
#104520=CARTESIAN_POINT('Ctrl Pts',(-9.97253398679687,24.4976891501419,
2.32255153283919));
#104521=CARTESIAN_POINT('Ctrl Pts',(-9.97918181701203,24.4981320730973,
2.32241523663539));
#104522=CARTESIAN_POINT('Ctrl Pts',(-9.9908831335633,24.4989146801423,2.32227444633923));
#104523=CARTESIAN_POINT('Ctrl Pts',(-9.9959362053581,24.4992536194162,2.32224617121823));
#104524=CARTESIAN_POINT('Ctrl Pts',(-10.006377803737,24.4999560951491,2.32225494150819));
#104525=CARTESIAN_POINT('Ctrl Pts',(-10.0117661979241,24.5003197619567,
2.3222964489739));
#104526=CARTESIAN_POINT('Ctrl Pts',(-10.025608102459,24.5012570208635,2.32249807902151));
#104527=CARTESIAN_POINT('Ctrl Pts',(-10.0340603947914,24.5018322727855,
2.3227122561429));
#104528=CARTESIAN_POINT('Ctrl Pts',(-10.0701066742898,24.5042985381159,
2.32401415126517));
#104529=CARTESIAN_POINT('Ctrl Pts',(-10.0976581075266,24.5062164080555,
2.32598111791656));
#104530=CARTESIAN_POINT('Ctrl Pts',(-10.2241537223738,24.5151801732983,
2.33949529173965));
#104531=CARTESIAN_POINT('Ctrl Pts',(-10.3214424889142,24.5225696808515,
2.3625973129843));
#104532=CARTESIAN_POINT('Ctrl Pts',(-10.435370567593,24.5314392822114,2.40545077646408));
#104533=CARTESIAN_POINT('Ctrl Pts',(-10.4558762463951,24.5330425250445,
2.4138312852233));
#104534=CARTESIAN_POINT('Ctrl Pts',(-10.495869957306,24.5361687506067,2.43150870911483));
#104535=CARTESIAN_POINT('Ctrl Pts',(-10.5153637212961,24.537692178363,2.44077338014174));
#104536=CARTESIAN_POINT('Ctrl Pts',(-10.5394916397183,24.53956783786,2.45306444652941));
#104537=CARTESIAN_POINT('Ctrl Pts',(-10.5443725547072,24.5399467473109,
2.45559404104909));
#104538=CARTESIAN_POINT('Ctrl Pts',(-10.5520707813183,24.5405433270755,
2.45965237231793));
#104539=CARTESIAN_POINT('Ctrl Pts',(-10.5548997961721,24.5407623395513,
2.46115855356095));
#104540=CARTESIAN_POINT('Ctrl Pts',(-10.5599533487098,24.5411531187626,
2.46387562324609));
#104541=CARTESIAN_POINT('Ctrl Pts',(-10.562180114459,24.5413251477094,2.46508213084928));
#104542=CARTESIAN_POINT('Ctrl Pts',(-10.5675261852479,24.5417377956757,
2.46800108843247));
#104543=CARTESIAN_POINT('Ctrl Pts',(-10.5706416429414,24.5419779743059,
2.46972050365281));
#104544=CARTESIAN_POINT('Ctrl Pts',(-10.5801336042773,24.5427089811739,
2.4750153630886));
#104545=CARTESIAN_POINT('Ctrl Pts',(-10.5864848000015,24.5431970647081,
2.47863616142687));
#104546=CARTESIAN_POINT('Ctrl Pts',(-10.6450295576518,24.547690392334,2.51273854727147));
#104547=CARTESIAN_POINT('Ctrl Pts',(-10.6948454971311,24.5514732908712,
2.54714107492292));
#104548=CARTESIAN_POINT('Ctrl Pts',(-10.8176511937564,24.5612818958166,
2.64672573467748));
#104549=CARTESIAN_POINT('Ctrl Pts',(-10.8855451811361,24.5672476308877,
2.71741578046518));
#104550=CARTESIAN_POINT('Ctrl Pts',(-10.9522485518537,24.57453703089,2.80681101364116));
#104551=CARTESIAN_POINT('Ctrl Pts',(-10.9603630488586,24.5754524221367,
2.81809746798643));
#104552=CARTESIAN_POINT('Ctrl Pts',(-10.9719499482024,24.5768039345743,
2.83483083477734));
#104553=CARTESIAN_POINT('Ctrl Pts',(-10.9755805266181,24.5772341123044,
2.84016717763361));
#104554=CARTESIAN_POINT('Ctrl Pts',(-10.981963221781,24.5780025971655,2.84971651246152));
#104555=CARTESIAN_POINT('Ctrl Pts',(-10.9847325658078,24.5783402534562,
2.85391784145478));
#104556=CARTESIAN_POINT('Ctrl Pts',(-10.9904685240862,24.5790486096619,
2.86274232934819));
#104557=CARTESIAN_POINT('Ctrl Pts',(-10.9934298809175,24.5794194926574,
2.86736874409735));
#104558=CARTESIAN_POINT('Ctrl Pts',(-11.0011033812624,24.5803943313984,
2.87954350429007));
#104559=CARTESIAN_POINT('Ctrl Pts',(-11.0057624567711,24.5810001998471,
2.88712471412224));
#104560=CARTESIAN_POINT('Ctrl Pts',(-11.0267906901765,24.5838007984269,
2.92222729309866));
#104561=CARTESIAN_POINT('Ctrl Pts',(-11.0421176833835,24.5860322226038,
2.95035391782175));
#104562=CARTESIAN_POINT('Ctrl Pts',(-11.1006501734712,24.5954044951267,
3.06903849499745));
#104563=CARTESIAN_POINT('Ctrl Pts',(-11.133340926597,24.6028720028285,3.16430418967029));
#104564=CARTESIAN_POINT('Ctrl Pts',(-11.1551715559829,24.6107333941226,
3.27035363368577));
#104565=CARTESIAN_POINT('Ctrl Pts',(-11.1567014679258,24.6113112850736,
3.27818815235943));
#104566=CARTESIAN_POINT('Ctrl Pts',(-11.1634462987685,24.6139893387851,
3.31469710120222));
#104567=CARTESIAN_POINT('Ctrl Pts',(-11.1676758582834,24.6160630055586,
3.34354595595367));
#104568=CARTESIAN_POINT('Ctrl Pts',(-11.1714244154802,24.6184660213716,
3.37797554935323));
#104569=CARTESIAN_POINT('Ctrl Pts',(-11.1719798354967,24.618844630165,3.38343072517334));
#104570=CARTESIAN_POINT('Ctrl Pts',(-11.1728262985415,24.6194608623473,
3.3923630708616));
#104571=CARTESIAN_POINT('Ctrl Pts',(-11.1731400170512,24.6196996730503,
3.39583793275172));
#104572=CARTESIAN_POINT('Ctrl Pts',(-11.1736758913255,24.6201271783819,
3.40208325588426));
#104573=CARTESIAN_POINT('Ctrl Pts',(-11.1739036878909,24.6203161796981,
3.40485317222141));
#104574=CARTESIAN_POINT('Ctrl Pts',(-11.1743822722149,24.6207298953925,
3.41093609399126));
#104575=CARTESIAN_POINT('Ctrl Pts',(-11.1746288480315,24.620954374219,3.4142493690343));
#104576=CARTESIAN_POINT('Ctrl Pts',(-11.1753007899725,24.6216007991028,
3.42382571591282));
#104577=CARTESIAN_POINT('Ctrl Pts',(-11.1756901163328,24.6220207953815,
3.43009132261101));
#104578=CARTESIAN_POINT('Ctrl Pts',(-11.1782855297841,24.6252152931303,
3.47805295471361));
#104579=CARTESIAN_POINT('Ctrl Pts',(-11.1783232241898,24.627880759095,3.519841793099));
#104580=CARTESIAN_POINT('Ctrl Pts',(-11.1715019384844,24.6360688363326,
3.65018982671148));
#104581=CARTESIAN_POINT('Ctrl Pts',(-11.1568579807933,24.6414247655147,
3.73802116742698));
#104582=CARTESIAN_POINT('Ctrl Pts',(-11.1221808252907,24.6494204005243,
3.85946314593704));
#104583=CARTESIAN_POINT('Ctrl Pts',(-11.110158144781,24.6518351000848,3.89503417950717));
#104584=CARTESIAN_POINT('Ctrl Pts',(-11.0929674978348,24.6549356787997,
3.93887194002238));
#104585=CARTESIAN_POINT('Ctrl Pts',(-11.0893677045515,24.6555688947879,
3.94773265056259));
#104586=CARTESIAN_POINT('Ctrl Pts',(-11.0834667544391,24.6565825742762,
3.96176496215947));
#104587=CARTESIAN_POINT('Ctrl Pts',(-11.0812354864862,24.6569606712743,
3.96696564017513));
#104588=CARTESIAN_POINT('Ctrl Pts',(-11.0769856110184,24.6576713587674,
3.97667754354162));
#104589=CARTESIAN_POINT('Ctrl Pts',(-11.0749759131138,24.6580036391707,
3.98119255167981));
#104590=CARTESIAN_POINT('Ctrl Pts',(-11.0704128130022,24.6587497940021,
3.99127279919678));
#104591=CARTESIAN_POINT('Ctrl Pts',(-11.0678443232913,24.6591641795745,
3.99683100970883));
#104592=CARTESIAN_POINT('Ctrl Pts',(-11.0601045360422,24.6603966729942,
4.01324260471443));
#104593=CARTESIAN_POINT('Ctrl Pts',(-11.0548103987138,24.6612189993113,
4.02403683324936));
#104594=CARTESIAN_POINT('Ctrl Pts',(-11.0175125867451,24.6668771620815,
4.09722748314501));
#104595=CARTESIAN_POINT('Ctrl Pts',(-10.9801624161662,24.6719029745937,
4.15672747834859));
#104596=CARTESIAN_POINT('Ctrl Pts',(-10.8924717794376,24.6824965971428,
4.27213356121441));
#104597=CARTESIAN_POINT('Ctrl Pts',(-10.8416157609093,24.6880543584961,
4.32727242856068));
#104598=CARTESIAN_POINT('Ctrl Pts',(-10.7710390506492,24.6948163454437,
4.39050004775844));
#104599=CARTESIAN_POINT('Ctrl Pts',(-10.7558724303697,24.6962200674192,
4.40340939677099));
#104600=CARTESIAN_POINT('Ctrl Pts',(-10.7361950044635,24.6979722378829,
4.41931550669535));
#104601=CARTESIAN_POINT('Ctrl Pts',(-10.7319820484678,24.69834348231,4.42267348991208));
#104602=CARTESIAN_POINT('Ctrl Pts',(-10.7252814219442,24.6989276109887,
4.42793951744813));
#104603=CARTESIAN_POINT('Ctrl Pts',(-10.7228089856875,24.6991417990795,
4.4298666892926));
#104604=CARTESIAN_POINT('Ctrl Pts',(-10.7181023376188,24.6995469419265,
4.43350523041063));
#104605=CARTESIAN_POINT('Ctrl Pts',(-10.715869662876,24.6997380240306,4.43521848166122));
#104606=CARTESIAN_POINT('Ctrl Pts',(-10.710618964948,24.7001848684021,4.43921780400885));
#104607=CARTESIAN_POINT('Ctrl Pts',(-10.707595985527,24.7004401819263,4.4414973812903));
#104608=CARTESIAN_POINT('Ctrl Pts',(-10.6977004217185,24.7012697984553,
4.44888487469039));
#104609=CARTESIAN_POINT('Ctrl Pts',(-10.690782922766,24.7018401504645,4.45393256996105));
#104610=CARTESIAN_POINT('Ctrl Pts',(-10.6333959288998,24.7064989980139,
4.49485618716958));
#104611=CARTESIAN_POINT('Ctrl Pts',(-10.5802169131868,24.7103604762319,
4.52678123939741));
#104612=CARTESIAN_POINT('Ctrl Pts',(-10.439462011152,24.7200974689023,4.5968353116984));
#104613=CARTESIAN_POINT('Ctrl Pts',(-10.349330878844,24.7259281099295,4.62877821214286));
#104614=CARTESIAN_POINT('Ctrl Pts',(-10.2423306590079,24.7330885267044,
4.65263912210892));
#104615=CARTESIAN_POINT('Ctrl Pts',(-10.2282655523376,24.7340334742023,
4.65550677304565));
#104616=CARTESIAN_POINT('Ctrl Pts',(-10.2077139414109,24.7354211779157,
4.65930705481101));
#104617=CARTESIAN_POINT('Ctrl Pts',(-10.201266146849,24.735857540156,4.66044382200123));
#104618=CARTESIAN_POINT('Ctrl Pts',(-10.1898230547305,24.7366338640599,
4.66236303820255));
#104619=CARTESIAN_POINT('Ctrl Pts',(-10.1848315267483,24.7369731378763,
4.66316719780408));
#104620=CARTESIAN_POINT('Ctrl Pts',(-10.1744284135187,24.7376816342498,
4.66477453633613));
#104621=CARTESIAN_POINT('Ctrl Pts',(-10.1690161110633,24.7380510203235,
4.66557219613443));
#104622=CARTESIAN_POINT('Ctrl Pts',(-10.1549275179755,24.7390146948843,
4.6675483683054));
#104623=CARTESIAN_POINT('Ctrl Pts',(-10.1462434261853,24.739610801227,4.66866786611394));
#104624=CARTESIAN_POINT('Ctrl Pts',(-10.1073997039169,24.7422871092663,
4.67323563103416));
#104625=CARTESIAN_POINT('Ctrl Pts',(-10.0771283640713,24.7443999204743,
4.67561365615504));
#104626=CARTESIAN_POINT('Ctrl Pts',(-9.94814003051134,24.7535243028678,
4.68074342291793));
#104627=CARTESIAN_POINT('Ctrl Pts',(-9.84938454656352,24.7608553383744,
4.67224325478121));
#104628=CARTESIAN_POINT('Ctrl Pts',(-9.71478833380063,24.7708602454614,
4.64335748139481));
#104629=CARTESIAN_POINT('Ctrl Pts',(-9.67713166219693,24.7736544798527,
4.63329992910002));
#104630=CARTESIAN_POINT('Ctrl Pts',(-9.63439214308377,24.7767721707989,
4.6195807832112));
#104631=CARTESIAN_POINT('Ctrl Pts',(-9.62875890158339,24.7771819827859,
4.61772549654814));
#104632=CARTESIAN_POINT('Ctrl Pts',(-9.61968878589105,24.7778397617332,
4.61466215092699));
#104633=CARTESIAN_POINT('Ctrl Pts',(-9.61624316678565,24.7780891603604,
4.6134805899254));
#104634=CARTESIAN_POINT('Ctrl Pts',(-9.61018203740412,24.7785269536142,
4.61137064950751));
#104635=CARTESIAN_POINT('Ctrl Pts',(-9.6075643216126,24.7787157210086,4.61044900969929));
#104636=CARTESIAN_POINT('Ctrl Pts',(-9.60491925481046,24.7789061574666,
4.60950721869302));
#104637=CARTESIAN_POINT('Ctrl Pts',(-9.60488870787621,24.7789083567089,
4.6094963408627));
#104638=CARTESIAN_POINT('Ctrl Pts',(-9.60482845106778,24.7789126948493,
4.60947488047688));
#104639=CARTESIAN_POINT('Ctrl Pts',(-9.60479874117483,24.7789148337508,
4.60946429799146));
#104640=CARTESIAN_POINT('Ctrl Pts',(-9.60474012446376,24.7789190536628,
4.60944341641778));
#104641=CARTESIAN_POINT('Ctrl Pts',(-9.60471121765258,24.7789211346748,
4.60943311740364));
#104642=CARTESIAN_POINT('Ctrl Pts',(-9.60465417506417,24.7789252411204,
4.60941279156947));
#104643=CARTESIAN_POINT('Ctrl Pts',(-9.60462603923627,24.7789272665595,
4.60940276479833));
#104644=CARTESIAN_POINT('Ctrl Pts',(-9.60457050807002,24.778931264064,4.60938297276363));
#104645=CARTESIAN_POINT('Ctrl Pts',(-9.60454311273798,24.7789332361307,
4.60937320756493));
#104646=CARTESIAN_POINT('Ctrl Pts',(-9.60448903373301,24.7789371289709,
4.60935392858415));
#104647=CARTESIAN_POINT('Ctrl Pts',(-9.60446235003137,24.7789390497481,
4.60934441485042));
#104648=CARTESIAN_POINT('Ctrl Pts',(-9.60440966684827,24.7789428419896,
4.60932562919048));
#104649=CARTESIAN_POINT('Ctrl Pts',(-9.60438366735648,24.7789447134561,
4.60931635731546));
#104650=CARTESIAN_POINT('Ctrl Pts',(-9.60433232661003,24.778948408951,4.60929804626983));
#104651=CARTESIAN_POINT('Ctrl Pts',(-9.60430698532761,24.7789502329829,
4.60928900714078));
#104652=CARTESIAN_POINT('Ctrl Pts',(-9.60425693616873,24.7789538354003,
4.60927115288266));
#104653=CARTESIAN_POINT('Ctrl Pts',(-9.60423222832188,24.7789556137851,
4.60926233781244));
#104654=CARTESIAN_POINT('Ctrl Pts',(-9.60418342265416,24.778959126595,4.60924492347402));
#104655=CARTESIAN_POINT('Ctrl Pts',(-9.60415932478083,24.7789608610253,
4.60923632423244));
#104656=CARTESIAN_POINT('Ctrl Pts',(-9.60411171661651,24.7789642875457,
4.60921933367699));
#104657=CARTESIAN_POINT('Ctrl Pts',(-9.60408820632863,24.7789659796366,
4.60921094240684));
#104658=CARTESIAN_POINT('Ctrl Pts',(-9.60404175207241,24.7789693230123,
4.60919436033169));
#104659=CARTESIAN_POINT('Ctrl Pts',(-9.60401880808486,24.7789709742994,
4.60918616955991));
#104660=CARTESIAN_POINT('Ctrl Pts',(-9.60397346620513,24.7789742375263,
4.60916998138069));
#104661=CARTESIAN_POINT('Ctrl Pts',(-9.60395106826876,24.7789758494703,
4.6091619839952));
#104662=CARTESIAN_POINT('Ctrl Pts',(-9.60390679912848,24.7789790354076,
4.6091461757869));
#104663=CARTESIAN_POINT('Ctrl Pts',(-9.60388492791828,24.7789806094023,
4.60913836499738));
#104664=CARTESIAN_POINT('Ctrl Pts',(-9.60384169381251,24.7789837207695,
4.60912292350905));
#104665=CARTESIAN_POINT('Ctrl Pts',(-9.60382033091821,24.7789852581429,
4.60911529284419));
#104666=CARTESIAN_POINT('Ctrl Pts',(-9.6037780958261,24.7789882975381,4.6091002054116));
#104667=CARTESIAN_POINT('Ctrl Pts',(-9.60375722365093,24.7789897995591,
4.60909274868355));
#104668=CARTESIAN_POINT('Ctrl Pts',(-9.60371595334081,24.778992769451,4.60907800326786));
#104669=CARTESIAN_POINT('Ctrl Pts',(-9.60369555515816,24.7789942373262,
4.60907071459299));
#104670=CARTESIAN_POINT('Ctrl Pts',(-9.60365521676299,24.7789971400851,
4.6090562996301));
#104671=CARTESIAN_POINT('Ctrl Pts',(-9.60363527654893,24.7789985749698,
4.60904917336967));
#104672=CARTESIAN_POINT('Ctrl Pts',(-9.60359583877762,24.7790014128522,
4.60903507784664));
#104673=CARTESIAN_POINT('Ctrl Pts',(-9.6035763412221,24.7790028158506,4.60902810861126));
#104674=CARTESIAN_POINT('Ctrl Pts',(-9.60027553212759,24.7792403315723,
4.60784816430784));
#104675=CARTESIAN_POINT('Ctrl Pts',(-9.59699939059866,24.779475611179,4.60666061417405));
#104676=CARTESIAN_POINT('Ctrl Pts',(-9.59013873376859,24.7799674441173,
4.60413922673925));
#104677=CARTESIAN_POINT('Ctrl Pts',(-9.58655533969737,24.7802238318712,
4.60280243171948));
#104678=CARTESIAN_POINT('Ctrl Pts',(-9.57717070350627,24.7808941319978,
4.5992492955189));
#104679=CARTESIAN_POINT('Ctrl Pts',(-9.57138028382695,24.7813065467064,
4.5970044532125));
#104680=CARTESIAN_POINT('Ctrl Pts',(-9.52772179376773,24.7844091653559,
4.57968037391898));
#104681=CARTESIAN_POINT('Ctrl Pts',(-9.49063763219807,24.7870056159933,
4.56268861581218));
#104682=CARTESIAN_POINT('Ctrl Pts',(-9.35961276667372,24.7962913842629,
4.49421488816823));
#104683=CARTESIAN_POINT('Ctrl Pts',(-9.27193149659004,24.8027742899929,
4.43192005708362));
#104684=CARTESIAN_POINT('Ctrl Pts',(-9.18215429882838,24.810794602548,4.34763309535276));
#104685=CARTESIAN_POINT('Ctrl Pts',(-9.17066210892228,24.8118504202317,
4.33639229921493));
#104686=CARTESIAN_POINT('Ctrl Pts',(-9.15488697911064,24.8133436908852,
4.32031739833469));
#104687=CARTESIAN_POINT('Ctrl Pts',(-9.1504079253251,24.8137728288019,4.31567760544476));
#104688=CARTESIAN_POINT('Ctrl Pts',(-9.14269129747648,24.8145213380263,
4.30755153657204));
#104689=CARTESIAN_POINT('Ctrl Pts',(-9.13943629395877,24.8148399713782,
4.30408196247375));
#104690=CARTESIAN_POINT('Ctrl Pts',(-9.13268243933127,24.815507268165,4.29679490829198));
#104691=CARTESIAN_POINT('Ctrl Pts',(-9.12918757255436,24.8158560866118,
4.29297389091868));
#104692=CARTESIAN_POINT('Ctrl Pts',(-9.12094573429126,24.8166871949752,
4.28384270810267));
#104693=CARTESIAN_POINT('Ctrl Pts',(-9.11622155757175,24.8171704022077,
4.27851233387102));
#104694=CARTESIAN_POINT('Ctrl Pts',(-9.10040013098923,24.8188122601994,
4.26033112934403));
#104695=CARTESIAN_POINT('Ctrl Pts',(-9.08953296617723,24.8199800456983,
4.24728380099273));
#104696=CARTESIAN_POINT('Ctrl Pts',(-9.0640900145919,24.8228145551844,4.21535742015004));
#104697=CARTESIAN_POINT('Ctrl Pts',(-9.04979871954204,24.8244913992758,
4.19626225746629));
#104698=CARTESIAN_POINT('Ctrl Pts',(-8.97328829329972,24.8339608209114,
4.08728723908584));
#104699=CARTESIAN_POINT('Ctrl Pts',(-8.92325344280207,24.8421525464417,
3.98954522966905));
#104700=CARTESIAN_POINT('Ctrl Pts',(-8.88740821192768,24.85,3.88630891215973));
#104701=CARTESIAN_POINT('',(-9.99063336962939,24.85,4.67771275306651));
#104702=CARTESIAN_POINT('Origin',(-10.,24.85,3.5));
#104703=CARTESIAN_POINT('',(-11.1772880725875,24.7251753227386,3.4996108612957));
#104704=CARTESIAN_POINT('Ctrl Pts',(-11.1777499294838,24.7254411208432,
3.49959244531692));
#104705=CARTESIAN_POINT('Ctrl Pts',(-11.177755138959,24.7264977516175,3.51464676629648));
#104706=CARTESIAN_POINT('Ctrl Pts',(-11.1774717063853,24.7275454784774,
3.52970041717589));
#104707=CARTESIAN_POINT('Ctrl Pts',(-11.176514931794,24.7292825855865,3.5548657671731));
#104708=CARTESIAN_POINT('Ctrl Pts',(-11.1759996106182,24.7299769475529,
3.56498126463823));
#104709=CARTESIAN_POINT('Ctrl Pts',(-11.1750130228752,24.7310313066549,
3.58042410351479));
#104710=CARTESIAN_POINT('Ctrl Pts',(-11.1746358678129,24.7313943558125,
3.58575674975724));
#104711=CARTESIAN_POINT('Ctrl Pts',(-11.1738818741506,24.7320542601341,
3.59547667609124));
#104712=CARTESIAN_POINT('Ctrl Pts',(-11.1735167171838,24.7323514918127,
3.59986473645066));
#104713=CARTESIAN_POINT('Ctrl Pts',(-11.1727548552257,24.7329309160681,
3.60843792390885));
#104714=CARTESIAN_POINT('Ctrl Pts',(-11.1723603351763,24.7332131755401,
3.61262317314638));
#104715=CARTESIAN_POINT('Ctrl Pts',(-11.1714052847838,24.7338580797188,
3.62220540717993));
#104716=CARTESIAN_POINT('Ctrl Pts',(-11.1708298467939,24.7342202311984,
3.6276008400157));
#104717=CARTESIAN_POINT('Ctrl Pts',(-11.1691539993501,24.7352074834157,
3.64234685982795));
#104718=CARTESIAN_POINT('Ctrl Pts',(-11.1679787057468,24.7358301342547,
3.65168867624558));
#104719=CARTESIAN_POINT('Ctrl Pts',(-11.1627134868986,24.7383627554835,
3.68983954298161));
#104720=CARTESIAN_POINT('Ctrl Pts',(-11.1576684580273,24.7402416619903,
3.71850783311194));
#104721=CARTESIAN_POINT('Ctrl Pts',(-11.1292884404647,24.7488563029863,
3.850841905454));
#104722=CARTESIAN_POINT('Ctrl Pts',(-11.0930608022952,24.7551722476283,
3.95121806583432));
#104723=CARTESIAN_POINT('Ctrl Pts',(-11.0287903288429,24.7639539015492,
4.07423517106098));
#104724=CARTESIAN_POINT('Ctrl Pts',(-11.0125214477603,24.766052892499,4.1024578178727));
#104725=CARTESIAN_POINT('Ctrl Pts',(-10.9920344070001,24.7686064114546,
4.13481948699576));
#104726=CARTESIAN_POINT('Ctrl Pts',(-10.9889271063245,24.7689914956883,
4.13964929499859));
#104727=CARTESIAN_POINT('Ctrl Pts',(-10.9840731037844,24.7695900030116,
4.14707416339296));
#104728=CARTESIAN_POINT('Ctrl Pts',(-10.9823511581631,24.7698017482794,
4.14968534558134));
#104729=CARTESIAN_POINT('Ctrl Pts',(-10.9790877091956,24.7702020135359,
4.15459144700913));
#104730=CARTESIAN_POINT('Ctrl Pts',(-10.9775485453295,24.7703903596084,
4.15688777268823));
#104731=CARTESIAN_POINT('Ctrl Pts',(-10.9740299880956,24.7708199052824,
4.1620974630601));
#104732=CARTESIAN_POINT('Ctrl Pts',(-10.9720455930406,24.7710614381586,
4.16500739283712));
#104733=CARTESIAN_POINT('Ctrl Pts',(-10.9668676986757,24.7716897286675,
4.17252759723005));
#104734=CARTESIAN_POINT('Ctrl Pts',(-10.9636543138194,24.7720777558613,
4.17712397395204));
#104735=CARTESIAN_POINT('Ctrl Pts',(-10.942303085645,24.7746428588401,4.20720463085144));
#104736=CARTESIAN_POINT('Ctrl Pts',(-10.923190669809,24.7768772868424,4.23197819458875));
#104737=CARTESIAN_POINT('Ctrl Pts',(-10.880005956051,24.7817557488319,4.28356942238958));
#104738=CARTESIAN_POINT('Ctrl Pts',(-10.8556416763558,24.7844079493489,
4.31010406952791));
#104739=CARTESIAN_POINT('Ctrl Pts',(-10.7942681953594,24.7907991994936,
4.37108247915779));
#104740=CARTESIAN_POINT('Ctrl Pts',(-10.7561796642247,24.794537550629,4.40434474924715));
#104741=CARTESIAN_POINT('Ctrl Pts',(-10.6660180958196,24.8028110218165,
4.4733907771597));
#104742=CARTESIAN_POINT('Ctrl Pts',(-10.6129611859212,24.8072976730081,
4.50764608395494));
#104743=CARTESIAN_POINT('Ctrl Pts',(-10.5480076864262,24.8123730922583,
4.54254328992698));
#104744=CARTESIAN_POINT('Ctrl Pts',(-10.5385389146906,24.8131034392807,
4.54746588737711));
#104745=CARTESIAN_POINT('Ctrl Pts',(-10.5228662783851,24.8142972168318,
4.55534502160448));
#104746=CARTESIAN_POINT('Ctrl Pts',(-10.5167012833396,24.8147630257581,
4.55837708150735));
#104747=CARTESIAN_POINT('Ctrl Pts',(-10.5055373821334,24.8155999278717,
4.56374689920736));
#104748=CARTESIAN_POINT('Ctrl Pts',(-10.5005479463032,24.8159716068183,
4.56610377795259));
#104749=CARTESIAN_POINT('Ctrl Pts',(-10.4898274131765,24.816765305957,4.57107602443963));
#104750=CARTESIAN_POINT('Ctrl Pts',(-10.4840915072767,24.8171869894317,
4.57368066003593));
#104751=CARTESIAN_POINT('Ctrl Pts',(-10.4683589149601,24.8183357350052,
4.58067301635831));
#104752=CARTESIAN_POINT('Ctrl Pts',(-10.4583215383363,24.8190600242207,
4.58496802739729));
#104753=CARTESIAN_POINT('Ctrl Pts',(-10.3978096110724,24.8233784268121,
4.60987154956482));
#104754=CARTESIAN_POINT('Ctrl Pts',(-10.3460108542058,24.8268724573501,
4.62709570526503));
#104755=CARTESIAN_POINT('Ctrl Pts',(-10.2278172088294,24.8346155777747,
4.65747649500275));
#104756=CARTESIAN_POINT('Ctrl Pts',(-10.1611131367921,24.8388311140296,
4.66862920440857));
#104757=CARTESIAN_POINT('Ctrl Pts',(-10.0704127195105,24.8447069487161,
4.67587786445373));
#104758=CARTESIAN_POINT('Ctrl Pts',(-10.0469510018944,24.8462402573117,
4.67704807608586));
#104759=CARTESIAN_POINT('Ctrl Pts',(-10.0175322526035,24.8481948932828,
4.67763448103727));
#104760=CARTESIAN_POINT('Ctrl Pts',(-10.011592342945,24.8485911865705,4.67770792881751));
#104761=CARTESIAN_POINT('Ctrl Pts',(-10.0029659410544,24.8491693767408,
4.67774932906654));
#104762=CARTESIAN_POINT('Ctrl Pts',(-10.0002796214192,24.8493498039276,
4.6777530303329));
#104763=CARTESIAN_POINT('Ctrl Pts',(-9.99526997388056,24.849687011182,4.67774279339686));
#104764=CARTESIAN_POINT('Ctrl Pts',(-9.99295662562748,24.8498430187347,
4.67773123047548));
#104765=CARTESIAN_POINT('Ctrl Pts',(-9.99063336962939,24.85,4.67771275306651));
#104766=CARTESIAN_POINT('Ctrl Pts',(-9.81111852688625,24.5869833862071,
2.3377666957199));
#104767=CARTESIAN_POINT('Ctrl Pts',(-9.85758225208399,24.5899974122869,
2.33012084493045));
#104768=CARTESIAN_POINT('Ctrl Pts',(-9.90447666972509,24.5929707932202,
2.32524743637886));
#104769=CARTESIAN_POINT('Ctrl Pts',(-9.95144430870241,24.5959479723899,
2.32319483958211));
#104770=CARTESIAN_POINT('Ctrl Pts',(-9.99850100085462,24.5989307964518,
2.3211383509512));
#104771=CARTESIAN_POINT('Ctrl Pts',(-10.0456310486077,24.6019179804784,
2.32191398031387));
#104772=CARTESIAN_POINT('Ctrl Pts',(-10.0924623693727,24.6049688698172,
2.32552525705089));
#104773=CARTESIAN_POINT('Ctrl Pts',(-10.1265100711087,24.6071869531115,
2.32815075791698));
#104774=CARTESIAN_POINT('Ctrl Pts',(-10.1603995448042,24.609439100678,2.33227422482323));
#104775=CARTESIAN_POINT('Ctrl Pts',(-10.1939848786067,24.6117498453562,
2.33787895204113));
#104776=CARTESIAN_POINT('Ctrl Pts',(-10.1940023012851,24.6117510440747,
2.33788185954119));
#104777=CARTESIAN_POINT('Ctrl Pts',(-10.1940197238821,24.611752242809,2.33788476743961));
#104778=CARTESIAN_POINT('Ctrl Pts',(-10.1940371463977,24.6117534415591,
2.33788767573637));
#104779=CARTESIAN_POINT('Ctrl Pts',(-10.2367172506162,24.614690031112,2.34501215831637));
#104780=CARTESIAN_POINT('Ctrl Pts',(-10.2790701141076,24.6177291627391,
2.35456197197645));
#104781=CARTESIAN_POINT('Ctrl Pts',(-10.3208151990413,24.6208120221985,
2.3664622507935));
#104782=CARTESIAN_POINT('Ctrl Pts',(-10.3259059137602,24.6211879696436,
2.36791346174752));
#104783=CARTESIAN_POINT('Ctrl Pts',(-10.3309875465595,24.6215645673753,
2.3693995805412));
#104784=CARTESIAN_POINT('Ctrl Pts',(-10.3360595537553,24.6219417087332,
2.370920431718));
#104785=CARTESIAN_POINT('Ctrl Pts',(-10.3809908088543,24.6252826808388,
2.3843931555439));
#104786=CARTESIAN_POINT('Ctrl Pts',(-10.4251713239778,24.6286657673699,
2.4005953434563));
#104787=CARTESIAN_POINT('Ctrl Pts',(-10.4682696908998,24.6320320939319,
2.41939152864877));
#104788=CARTESIAN_POINT('Ctrl Pts',(-10.5113259988402,24.6353951353516,
2.43816937095576));
#104789=CARTESIAN_POINT('Ctrl Pts',(-10.5533024644096,24.6387411565441,
2.4595359027969));
#104790=CARTESIAN_POINT('Ctrl Pts',(-10.5938896487488,24.6420331412891,
2.48332486996171));
#104791=CARTESIAN_POINT('Ctrl Pts',(-10.6344549721495,24.6453233529159,
2.50710102398963));
#104792=CARTESIAN_POINT('Ctrl Pts',(-10.6736325624402,24.6485594959849,
2.53329695268629));
#104793=CARTESIAN_POINT('Ctrl Pts',(-10.7111326005979,24.6517290789581,
2.56171762936817));
#104794=CARTESIAN_POINT('Ctrl Pts',(-10.7486288368082,24.6548983405826,
2.59013542461513));
#104795=CARTESIAN_POINT('Ctrl Pts',(-10.7844477718312,24.6580011120596,
2.62077757904407));
#104796=CARTESIAN_POINT('Ctrl Pts',(-10.8183190897181,24.6610496044806,
2.65341995634774));
#104797=CARTESIAN_POINT('Ctrl Pts',(-10.8522250946285,24.6641012188093,
2.6860957621383));
#104798=CARTESIAN_POINT('Ctrl Pts',(-10.8841792539821,24.6670986487837,
2.72077604476894));
#104799=CARTESIAN_POINT('Ctrl Pts',(-10.9139323064,24.6700769647453,2.75720509748594));
#104800=CARTESIAN_POINT('Ctrl Pts',(-10.9437036423241,24.6730571109076,
2.7936565361686));
#104801=CARTESIAN_POINT('Ctrl Pts',(-10.9712707281535,24.6760185377855,
2.83185910709269));
#104802=CARTESIAN_POINT('Ctrl Pts',(-10.9964107211274,24.6790146045598,
2.87152292044512));
#104803=CARTESIAN_POINT('Ctrl Pts',(-11.0195880748556,24.6817767731687,
2.90809024300694));
#104804=CARTESIAN_POINT('Ctrl Pts',(-11.0407025532645,24.6845689829593,
2.94590008222233));
#104805=CARTESIAN_POINT('Ctrl Pts',(-11.0596054484233,24.6874407681847,
2.98469547749695));
#104806=CARTESIAN_POINT('Ctrl Pts',(-11.0612431100617,24.6876895667131,
2.98805653568687));
#104807=CARTESIAN_POINT('Ctrl Pts',(-11.0628642004715,24.6879389625114,
2.99142500702423));
#104808=CARTESIAN_POINT('Ctrl Pts',(-11.0644686388172,24.68818898779,2.9948007338952));
#104809=CARTESIAN_POINT('Ctrl Pts',(-11.069938513088,24.6890413775638,3.00630931046723));
#104810=CARTESIAN_POINT('Ctrl Pts',(-11.0752147010818,24.6899011034306,
3.01790177900417));
#104811=CARTESIAN_POINT('Ctrl Pts',(-11.0802940068402,24.6907694454115,
3.02957106735435));
#104812=CARTESIAN_POINT('Ctrl Pts',(-11.080302334643,24.6907708691062,3.02959019979827));
#104813=CARTESIAN_POINT('Ctrl Pts',(-11.0803106619167,24.6907722928241,
3.02960933244874));
#104814=CARTESIAN_POINT('Ctrl Pts',(-11.0803189886612,24.6907737165651,
3.02962846530571));
#104815=CARTESIAN_POINT('Ctrl Pts',(-11.0980581824247,24.6938068369181,
3.07038886749672));
#104816=CARTESIAN_POINT('Ctrl Pts',(-11.1134484878215,24.6969518887715,
3.1122243160909));
#104817=CARTESIAN_POINT('Ctrl Pts',(-11.1264093147121,24.7001441311768,
3.1548603050666));
#104818=CARTESIAN_POINT('Ctrl Pts',(-11.1283581804571,24.7006241354177,
3.1612713017659));
#104819=CARTESIAN_POINT('Ctrl Pts',(-11.1302521166983,24.7011052066318,
3.16770030250139));
#104820=CARTESIAN_POINT('Ctrl Pts',(-11.1320908541742,24.7015871247156,
3.17414627226733));
#104821=CARTESIAN_POINT('Ctrl Pts',(-11.1452476288099,24.7050354079559,
3.2202693173635));
#104822=CARTESIAN_POINT('Ctrl Pts',(-11.1555788799508,24.7085263128591,
3.26726742745412));
#104823=CARTESIAN_POINT('Ctrl Pts',(-11.1630189724679,24.7119977437618,
3.31480118396534));
#104824=CARTESIAN_POINT('Ctrl Pts',(-11.163505756299,24.7122248694905,3.31791118079));
#104825=CARTESIAN_POINT('Ctrl Pts',(-11.1639801586827,24.7124519118566,
3.32102345279043));
#104826=CARTESIAN_POINT('Ctrl Pts',(-11.164442159325,24.7126788534689,3.3241378973602));
#104827=CARTESIAN_POINT('Ctrl Pts',(-11.1719266982414,24.7163553707144,
3.37459276571997));
#104828=CARTESIAN_POINT('Ctrl Pts',(-11.1761583601084,24.7200050807238,
3.42562366407079));
#104829=CARTESIAN_POINT('Ctrl Pts',(-11.177088112557,24.7235849415198,3.47682444544406));
#104830=CARTESIAN_POINT('Ctrl Pts',(-11.1772259797544,24.7241157767712,
3.48441669028381));
#104831=CARTESIAN_POINT('Ctrl Pts',(-11.1772912923578,24.724645136589,3.49201266219816));
#104832=CARTESIAN_POINT('Ctrl Pts',(-11.1772839403217,24.7251729446244,
3.49961102606475));
#104833=CARTESIAN_POINT('Origin',(-10.,13.2,3.5));
#104834=CARTESIAN_POINT('',(-11.2887076826321,24.8493336655152,2.80606944570028));
#104835=CARTESIAN_POINT('Ctrl Pts',(-11.4635,24.3883362350912,3.49999997785042));
#104836=CARTESIAN_POINT('Ctrl Pts',(-11.4635000018663,24.395579963598,3.62331606172117));
#104837=CARTESIAN_POINT('Ctrl Pts',(-11.4479149340742,24.4031789408495,
3.74617229420536));
#104838=CARTESIAN_POINT('Ctrl Pts',(-11.4135023702327,24.4112209615172,
3.87953776065764));
#104839=CARTESIAN_POINT('Ctrl Pts',(-11.4097158080832,24.4120531990573,
3.89336906389607));
#104840=CARTESIAN_POINT('Ctrl Pts',(-11.3944544626202,24.4152158225676,
3.94606133427072));
#104841=CARTESIAN_POINT('Ctrl Pts',(-11.3815703952692,24.4175055471079,
3.98449732434018));
#104842=CARTESIAN_POINT('Ctrl Pts',(-11.3635408172435,24.4202952829669,
4.03168459175159));
#104843=CARTESIAN_POINT('Ctrl Pts',(-11.3598793841164,24.4208438625688,
4.04098071408713));
#104844=CARTESIAN_POINT('Ctrl Pts',(-11.3539475279854,24.4217051345132,
4.05560041503075));
#104845=CARTESIAN_POINT('Ctrl Pts',(-11.3517402773549,24.422019927099,4.06094915423817));
#104846=CARTESIAN_POINT('Ctrl Pts',(-11.3475794328349,24.4226029604457,
4.07086477634955));
#104847=CARTESIAN_POINT('Ctrl Pts',(-11.3456342046423,24.42287147745,4.07543506046806));
#104848=CARTESIAN_POINT('Ctrl Pts',(-11.3412742813686,24.4234644773029,
4.08553562258562));
#104849=CARTESIAN_POINT('Ctrl Pts',(-11.3388485659881,24.4237885821161,
4.09106106454632));
#104850=CARTESIAN_POINT('Ctrl Pts',(-11.3317313952652,24.4247230165747,
4.10700434748986));
#104851=CARTESIAN_POINT('Ctrl Pts',(-11.3269519738796,24.4253303518495,
4.11738258469905));
#104852=CARTESIAN_POINT('Ctrl Pts',(-11.2869594721666,24.4302541468916,
4.20161359863359));
#104853=CARTESIAN_POINT('Ctrl Pts',(-11.245730053618,24.4343494708593,4.27245401872569));
#104854=CARTESIAN_POINT('Ctrl Pts',(-11.1598023548768,24.4416896338265,
4.39515953833734));
#104855=CARTESIAN_POINT('Ctrl Pts',(-11.1169837864255,24.4449552872432,
4.44805012002431));
#104856=CARTESIAN_POINT('Ctrl Pts',(-11.0295668328515,24.4512703469944,
4.54185162390309));
#104857=CARTESIAN_POINT('Ctrl Pts',(-10.9858093329547,24.4542977738486,
4.5833471592725));
#104858=CARTESIAN_POINT('Ctrl Pts',(-10.9340911712786,24.4578968947417,
4.62665790456836));
#104859=CARTESIAN_POINT('Ctrl Pts',(-10.9285232061192,24.4582846449281,
4.63125107805963));
#104860=CARTESIAN_POINT('Ctrl Pts',(-10.9201781975705,24.4588665703848,
4.63803199885728));
#104861=CARTESIAN_POINT('Ctrl Pts',(-10.9174267499958,24.4590585634451,
4.64025124580611));
#104862=CARTESIAN_POINT('Ctrl Pts',(-10.912492148537,24.4594031724113,4.64420194586975));
#104863=CARTESIAN_POINT('Ctrl Pts',(-10.910312064616,24.4595555178638,4.64593715312667));
#104864=CARTESIAN_POINT('Ctrl Pts',(-10.9055693978202,24.4598871635893,
4.64968993768724));
#104865=CARTESIAN_POINT('Ctrl Pts',(-10.9030050561334,24.4600666200175,
4.65170515118098));
#104866=CARTESIAN_POINT('Ctrl Pts',(-10.8957850234587,24.4605722196446,
4.65734014887833));
#104867=CARTESIAN_POINT('Ctrl Pts',(-10.8911142125169,24.4608996884417,
4.66094034570658));
#104868=CARTESIAN_POINT('Ctrl Pts',(-10.8628120579187,24.4628855913374,
4.68248382919634));
#104869=CARTESIAN_POINT('Ctrl Pts',(-10.8386627672836,24.4645868936193,
4.69973212397364));
#104870=CARTESIAN_POINT('Ctrl Pts',(-10.7003484769693,24.4742939808631,
4.79230392769391));
#104871=CARTESIAN_POINT('Ctrl Pts',(-10.5765835940818,24.4827631050378,
4.85207111966067));
#104872=CARTESIAN_POINT('Ctrl Pts',(-10.4394697239234,24.491123169717,4.89597640648737));
#104873=CARTESIAN_POINT('Ctrl Pts',(-10.4326180876373,24.4915386264112,
4.89811493025721));
#104874=CARTESIAN_POINT('Ctrl Pts',(-10.3863888699656,24.4943261510023,
4.91217155789038));
#104875=CARTESIAN_POINT('Ctrl Pts',(-10.3465372549996,24.4966521934943,
4.92247575411468));
#104876=CARTESIAN_POINT('Ctrl Pts',(-10.2964727829022,24.4994801231183,
4.93319125224792));
#104877=CARTESIAN_POINT('Ctrl Pts',(-10.2866226167697,24.5000320879207,
4.93519363124327));
#104878=CARTESIAN_POINT('Ctrl Pts',(-10.2710522017688,24.5008977667151,
4.93819214693685));
#104879=CARTESIAN_POINT('Ctrl Pts',(-10.2653454395408,24.5012136096911,
4.9392559698209));
#104880=CARTESIAN_POINT('Ctrl Pts',(-10.2547846627948,24.501795484248,4.94115970323365));
#104881=CARTESIAN_POINT('Ctrl Pts',(-10.2499324635919,24.5020618115898,
4.94200911199761));
#104882=CARTESIAN_POINT('Ctrl Pts',(-10.2391514052299,24.502651340826,4.94384035448484));
#104883=CARTESIAN_POINT('Ctrl Pts',(-10.2332205823806,24.5029741618651,
4.94481020389869));
#104884=CARTESIAN_POINT('Ctrl Pts',(-10.2161384625526,24.5038997795505,
4.9474956668982));
#104885=CARTESIAN_POINT('Ctrl Pts',(-10.2049729446481,24.5044996793862,
4.94911891925363));
#104886=CARTESIAN_POINT('Ctrl Pts',(-10.1189888017754,24.5090821648202,
4.96060566999701));
#104887=CARTESIAN_POINT('Ctrl Pts',(-10.0435233147649,24.512879248679,4.96479857723339));
#104888=CARTESIAN_POINT('Ctrl Pts',(-9.88163229136688,24.520844135936,4.96126494639229));
#104889=CARTESIAN_POINT('Ctrl Pts',(-9.79554223507775,24.5249689316798,
4.95172386410779));
#104890=CARTESIAN_POINT('Ctrl Pts',(-9.69573501150379,24.5300355703903,
4.93160443934707));
#104891=CARTESIAN_POINT('Ctrl Pts',(-9.68071823376365,24.530805965361,4.92833034948654));
#104892=CARTESIAN_POINT('Ctrl Pts',(-9.63259659367964,24.5333083496372,
4.91704165517477));
#104893=CARTESIAN_POINT('Ctrl Pts',(-9.59972109482159,24.5350694079443,
4.9081082236652));
#104894=CARTESIAN_POINT('Ctrl Pts',(-9.5616180561903,24.5372024727957,4.8963121211659));
#104895=CARTESIAN_POINT('Ctrl Pts',(-9.55605687438356,24.5375161260877,
4.89455396716141));
#104896=CARTESIAN_POINT('Ctrl Pts',(-9.54707851662153,24.5380265052009,
4.89165633491366));
#104897=CARTESIAN_POINT('Ctrl Pts',(-9.5436547230652,24.5382220763641,4.89053738254849));
#104898=CARTESIAN_POINT('Ctrl Pts',(-9.53757649539273,24.5385710086285,
4.88852605114987));
#104899=CARTESIAN_POINT('Ctrl Pts',(-9.53492045651033,24.538724077553,4.88763868149646));
#104900=CARTESIAN_POINT('Ctrl Pts',(-9.52920025562792,24.5390550287183,
4.88570932203383));
#104901=CARTESIAN_POINT('Ctrl Pts',(-9.5261370379425,24.5392330527241,4.88466480320889));
#104902=CARTESIAN_POINT('Ctrl Pts',(-9.51765033131726,24.5397284337715,
4.8817394830145));
#104903=CARTESIAN_POINT('Ctrl Pts',(-9.51223446587876,24.5400470203795,
4.87983694083723));
#104904=CARTESIAN_POINT('Ctrl Pts',(-9.48166789665751,24.5418584323435,
4.86889675250147));
#104905=CARTESIAN_POINT('Ctrl Pts',(-9.45675873963097,24.543385765376,4.85920389838867));
#104906=CARTESIAN_POINT('Ctrl Pts',(-9.37704677461605,24.5484092102983,
4.82564458406915));
#104907=CARTESIAN_POINT('Ctrl Pts',(-9.32343814439683,24.5519977727624,
4.7991026054702));
#104908=CARTESIAN_POINT('Ctrl Pts',(-9.1701248636585,24.5626337651942,4.71112709619329));
#104909=CARTESIAN_POINT('Ctrl Pts',(-9.07597529543186,24.5696254019425,
4.64092463223607));
#104910=CARTESIAN_POINT('Ctrl Pts',(-8.97925383984117,24.5770862114638,
4.54889500252843));
#104911=CARTESIAN_POINT('Ctrl Pts',(-8.96751546543043,24.5779980380897,
4.53734235752755));
#104912=CARTESIAN_POINT('Ctrl Pts',(-8.95143117755654,24.5792568712628,
4.52096900141471));
#104913=CARTESIAN_POINT('Ctrl Pts',(-8.94691885059354,24.5796110954741,
4.51631411084658));
#104914=CARTESIAN_POINT('Ctrl Pts',(-8.93917155568424,24.5802211774092,
4.50821504939365));
#104915=CARTESIAN_POINT('Ctrl Pts',(-8.93592208732818,24.5804776560974,
4.50478493747898));
#104916=CARTESIAN_POINT('Ctrl Pts',(-8.92921402783208,24.5810083777484,
4.49763492826492));
#104917=CARTESIAN_POINT('Ctrl Pts',(-8.92575807271136,24.5812825069712,
4.49391263742694));
#104918=CARTESIAN_POINT('Ctrl Pts',(-8.9176823337168,24.5819247888391,4.48512320841413));
#104919=CARTESIAN_POINT('Ctrl Pts',(-8.91307862203848,24.5822922639096,
4.48004142096585));
#104920=CARTESIAN_POINT('Ctrl Pts',(-8.89810036189819,24.5834924193799,
4.46327236724111));
#104921=CARTESIAN_POINT('Ctrl Pts',(-8.88787708262172,24.5843188550253,
4.45145105355931));
#104922=CARTESIAN_POINT('Ctrl Pts',(-8.82905446905561,24.5891218810937,
4.38118990268194));
#104923=CARTESIAN_POINT('Ctrl Pts',(-8.7848757227542,24.5929177281757,4.31919706638321));
#104924=CARTESIAN_POINT('Ctrl Pts',(-8.70345403042831,24.6006596570788,
4.18375918724548));
#104925=CARTESIAN_POINT('Ctrl Pts',(-8.66718379933786,24.6045806957516,
4.11004755984359));
#104926=CARTESIAN_POINT('Ctrl Pts',(-8.63392977878911,24.6091291859393,
4.02513690643022));
#104927=CARTESIAN_POINT('Ctrl Pts',(-8.63066084081614,24.6095894608739,
4.01655288459715));
#104928=CARTESIAN_POINT('Ctrl Pts',(-8.62591918267693,24.6102778839544,
4.00374021046289));
#104929=CARTESIAN_POINT('Ctrl Pts',(-8.62438468157175,24.610504076599,3.99953457068266));
#104930=CARTESIAN_POINT('Ctrl Pts',(-8.61157673757472,24.6124216633605,
3.96392498613783));
#104931=CARTESIAN_POINT('Ctrl Pts',(-8.60136179717959,24.6141481840516,
3.93215321390143));
#104932=CARTESIAN_POINT('Ctrl Pts',(-8.59065790584223,24.6162424510754,
3.89448789498059));
#104933=CARTESIAN_POINT('Ctrl Pts',(-8.58910680518603,24.6165541441918,
3.88890388048037));
#104934=CARTESIAN_POINT('Ctrl Pts',(-8.58664891288582,24.6170618547681,
3.8798471217667));
#104935=CARTESIAN_POINT('Ctrl Pts',(-8.58572164321746,24.6172567344192,
3.87637994146533));
#104936=CARTESIAN_POINT('Ctrl Pts',(-8.58409716027383,24.6176042139065,
3.87021502175787));
#104937=CARTESIAN_POINT('Ctrl Pts',(-8.58339487498002,24.6177565231765,
3.86751861665172));
#104938=CARTESIAN_POINT('Ctrl Pts',(-8.58190269489624,24.6180847051419,
3.86172160675026));
#104939=CARTESIAN_POINT('Ctrl Pts',(-8.58111526902468,24.6182607144955,
3.85862042235416));
#104940=CARTESIAN_POINT('Ctrl Pts',(-8.5789568448732,24.6187510792355,3.85000132629544));
#104941=CARTESIAN_POINT('Ctrl Pts',(-8.57760783866035,24.6190666595984,
3.84447803167807));
#104942=CARTESIAN_POINT('Ctrl Pts',(-8.57012627559957,24.6208692607581,
3.81305257397498));
#104943=CARTESIAN_POINT('Ctrl Pts',(-8.56466947326265,24.6223910501948,
3.78699629919708));
#104944=CARTESIAN_POINT('Ctrl Pts',(-8.54932364263577,24.6273957936799,
3.70226284497424));
#104945=CARTESIAN_POINT('Ctrl Pts',(-8.54230133417534,24.6309723995269,
3.64312920424746));
#104946=CARTESIAN_POINT('Ctrl Pts',(-8.53207499372629,24.6417452004105,
3.464690987229));
#104947=CARTESIAN_POINT('Ctrl Pts',(-8.53982592728949,24.6488867605369,
3.34523565727496));
#104948=CARTESIAN_POINT('Ctrl Pts',(-8.5650444587117,24.6564706953814,3.21189487508679));
#104949=CARTESIAN_POINT('Ctrl Pts',(-8.56836792683034,24.6573800027911,
3.19580991689321));
#104950=CARTESIAN_POINT('Ctrl Pts',(-8.57337056494595,24.6586338798893,
3.17350011417296));
#104951=CARTESIAN_POINT('Ctrl Pts',(-8.57482106808563,24.6589857107325,
3.16722570065227));
#104952=CARTESIAN_POINT('Ctrl Pts',(-8.57739807127232,24.6595911519306,
3.15640439105564));
#104953=CARTESIAN_POINT('Ctrl Pts',(-8.57850506558081,24.6598453837492,
3.15185298760238));
#104954=CARTESIAN_POINT('Ctrl Pts',(-8.58084515730162,24.6603709560869,
3.1424289661995));
#104955=CARTESIAN_POINT('Ctrl Pts',(-8.58208154456644,24.6606421868409,
3.13755722329685));
#104956=CARTESIAN_POINT('Ctrl Pts',(-8.58504173066293,24.6612767747781,
3.12614019124224));
#104957=CARTESIAN_POINT('Ctrl Pts',(-8.58678589489024,24.6616394700238,
3.11960026840541));
#104958=CARTESIAN_POINT('Ctrl Pts',(-8.59263318847584,24.6628198925167,
3.0982706489947));
#104959=CARTESIAN_POINT('Ctrl Pts',(-8.59692368266008,24.6636315605696,
3.08353309255072));
#104960=CARTESIAN_POINT('Ctrl Pts',(-8.62061907680284,24.6678479460841,
3.00666776536701));
#104961=CARTESIAN_POINT('Ctrl Pts',(-8.64392146022601,24.6711230271572,
2.94581531298684));
#104962=CARTESIAN_POINT('Ctrl Pts',(-8.71120619595036,24.6790336963597,
2.80003090210626));
#104963=CARTESIAN_POINT('Ctrl Pts',(-8.75959512102653,24.6835644107795,
2.71747821255996));
#104964=CARTESIAN_POINT('Ctrl Pts',(-8.84147816930817,24.6905304984309,
2.60468519608415));
#104965=CARTESIAN_POINT('Ctrl Pts',(-8.86886636110479,24.6927757703943,
2.57032401669929));
#104966=CARTESIAN_POINT('Ctrl Pts',(-8.90221808844528,24.6954835989025,
2.53213991235389));
#104967=CARTESIAN_POINT('Ctrl Pts',(-8.90671636453008,24.6958483040477,
2.52706158292328));
#104968=CARTESIAN_POINT('Ctrl Pts',(-8.9135767666852,24.6964040823174,2.51942418206164));
#104969=CARTESIAN_POINT('Ctrl Pts',(-8.9159130500219,24.6965932744127,2.51684189420938));
#104970=CARTESIAN_POINT('Ctrl Pts',(-8.9201300306212,24.696934681482,2.51221418313363));
#104971=CARTESIAN_POINT('Ctrl Pts',(-8.92200735548343,24.6970866438092,
2.51016575689477));
#104972=CARTESIAN_POINT('Ctrl Pts',(-8.92612155707991,24.6974196164102,
2.50570216924225));
#104973=CARTESIAN_POINT('Ctrl Pts',(-8.92836073875178,24.6976007986044,
2.50328921961814));
#104974=CARTESIAN_POINT('Ctrl Pts',(-8.93472158718561,24.6981153156287,
2.49648096169963));
#104975=CARTESIAN_POINT('Ctrl Pts',(-8.93886223483111,24.6984500469811,
2.49210357784372));
#104976=CARTESIAN_POINT('Ctrl Pts',(-8.96514761182479,24.7005729972829,
2.46465688362201));
#104977=CARTESIAN_POINT('Ctrl Pts',(-8.98801494050295,24.7024110248755,
2.44229457314978));
#104978=CARTESIAN_POINT('Ctrl Pts',(-9.06913004502535,24.7088449214015,
2.36801060646379));
#104979=CARTESIAN_POINT('Ctrl Pts',(-9.13078472063797,24.7135840159466,
2.32000722160854));
#104980=CARTESIAN_POINT('Ctrl Pts',(-9.28170458027993,24.7244392028596,
2.22077670231669));
#104981=CARTESIAN_POINT('Ctrl Pts',(-9.37314312970547,24.7304734505406,
2.17356958565135));
#104982=CARTESIAN_POINT('Ctrl Pts',(-9.47872953172093,24.7367537743011,
2.13243892198275));
#104983=CARTESIAN_POINT('Ctrl Pts',(-9.48871864341625,24.7373418199948,
2.12867305645963));
#104984=CARTESIAN_POINT('Ctrl Pts',(-9.50483337108708,24.7382808602949,
2.12279841371202));
#104985=CARTESIAN_POINT('Ctrl Pts',(-9.51093321359506,24.7386341189606,
2.12062047282893));
#104986=CARTESIAN_POINT('Ctrl Pts',(-9.52181242709276,24.7392603271643,
2.11681730217711));
#104987=CARTESIAN_POINT('Ctrl Pts',(-9.52658609819783,24.7395337934034,
2.11517618127699));
#104988=CARTESIAN_POINT('Ctrl Pts',(-9.53657714288246,24.7401034547862,
2.11179910009288));
#104989=CARTESIAN_POINT('Ctrl Pts',(-9.54179600802381,24.740399495334,2.11006777652027));
#104990=CARTESIAN_POINT('Ctrl Pts',(-9.55544474031845,24.7411698138853,
2.10562512846453));
#104991=CARTESIAN_POINT('Ctrl Pts',(-9.5638897461,24.7416425648028,2.10296080500888));
#104992=CARTESIAN_POINT('Ctrl Pts',(-9.60161143856802,24.7437375506052,
2.09143533247172));
#104993=CARTESIAN_POINT('Ctrl Pts',(-9.63113854289351,24.7453326734003,
2.08341633970984));
#104994=CARTESIAN_POINT('Ctrl Pts',(-9.76256127341549,24.7522668315409,
2.05211286210986));
#104995=CARTESIAN_POINT('Ctrl Pts',(-9.86652560519187,24.7572924626429,
2.03885655074291));
#104996=CARTESIAN_POINT('Ctrl Pts',(-10.049821750975,24.7662462257915,2.03522622605583));
#104997=CARTESIAN_POINT('Ctrl Pts',(-10.1286117379348,24.7701356663777,
2.04003411296748));
#104998=CARTESIAN_POINT('Ctrl Pts',(-10.2136108745967,24.7747166634902,
2.05215591160948));
#104999=CARTESIAN_POINT('Ctrl Pts',(-10.2205938664149,24.77509590483,2.05320338257555));
#105000=CARTESIAN_POINT('Ctrl Pts',(-10.2310693060105,24.7756695302105,
2.05485233193566));
#105001=CARTESIAN_POINT('Ctrl Pts',(-10.234567696452,24.7758618898867,2.05541604538168));
#105002=CARTESIAN_POINT('Ctrl Pts',(-10.2408116964493,24.7762066848808,
2.05644545233857));
#105003=CARTESIAN_POINT('Ctrl Pts',(-10.2435580608097,24.7763588513825,
2.05690628307582));
#105004=CARTESIAN_POINT('Ctrl Pts',(-10.2463215290558,24.7765124767258,
2.05737809711842));
#105005=CARTESIAN_POINT('Ctrl Pts',(-10.24633997186,24.7765135020118,2.05738124626981));
#105006=CARTESIAN_POINT('Ctrl Pts',(-10.2463760006676,24.7765155049964,
2.0573873989829));
#105007=CARTESIAN_POINT('Ctrl Pts',(-10.2463935866133,24.7765164826898,
2.05739040250173));
#105008=CARTESIAN_POINT('Ctrl Pts',(-10.2464279463137,24.7765183929633,
2.05739627147121));
#105009=CARTESIAN_POINT('Ctrl Pts',(-10.2464447200985,24.7765193255432,
2.05739913689714));
#105010=CARTESIAN_POINT('Ctrl Pts',(-10.2464794233633,24.7765212549957,
2.05740506579658));
#105011=CARTESIAN_POINT('Ctrl Pts',(-10.2464973528097,24.7765222518692,
2.05740812930731));
#105012=CARTESIAN_POINT('Ctrl Pts',(-10.2465330208745,24.7765242350491,
2.05741422440733));
#105013=CARTESIAN_POINT('Ctrl Pts',(-10.2465507594836,24.7765252213545,
2.05741725598776));
#105014=CARTESIAN_POINT('Ctrl Pts',(-10.2465860492748,24.776527183586,2.05742328778672));
#105015=CARTESIAN_POINT('Ctrl Pts',(-10.2466036004998,24.7765281595141,
2.05742628800551));
#105016=CARTESIAN_POINT('Ctrl Pts',(-10.2466385190393,24.776530101185,2.05743225766117));
#105017=CARTESIAN_POINT('Ctrl Pts',(-10.2466558863204,24.7765310669256,
2.05743522708548));
#105018=CARTESIAN_POINT('Ctrl Pts',(-10.246690440319,24.7765329884064,2.05744113570391));
#105019=CARTESIAN_POINT('Ctrl Pts',(-10.2467076270006,24.7765339441443,
2.05744407488523));
#105020=CARTESIAN_POINT('Ctrl Pts',(-10.2467418230542,24.7765358457994,
2.05744992355424));
#105021=CARTESIAN_POINT('Ctrl Pts',(-10.2467588324099,24.7765367917153,
2.05745283303266));
#105022=CARTESIAN_POINT('Ctrl Pts',(-10.2467926769059,24.7765386738973,
2.05745862280581));
#105023=CARTESIAN_POINT('Ctrl Pts',(-10.2468095120883,24.7765396101654,
2.0574615031014));
#105024=CARTESIAN_POINT('Ctrl Pts',(-10.24684301143,24.7765414732282,2.05746723503623));
#105025=CARTESIAN_POINT('Ctrl Pts',(-10.2468596755882,24.7765424000224,
2.05747008666916));
#105026=CARTESIAN_POINT('Ctrl Pts',(-10.246892835798,24.7765442442984,2.05747576175936));
#105027=CARTESIAN_POINT('Ctrl Pts',(-10.2469093319104,24.7765451617833,
2.05747858522112));
#105028=CARTESIAN_POINT('Ctrl Pts',(-10.2469421592163,24.7765469876168,
2.05748420449685));
#105029=CARTESIAN_POINT('Ctrl Pts',(-10.246958490336,24.776547895961,2.05748700029238));
#105030=CARTESIAN_POINT('Ctrl Pts',(-10.246990990437,24.7765497036668,2.05749256469436));
#105031=CARTESIAN_POINT('Ctrl Pts',(-10.2470071594422,24.7765506030293,
2.05749533329926));
#105032=CARTESIAN_POINT('Ctrl Pts',(-10.2470393381155,24.7765523929265,
2.05750084378281));
#105033=CARTESIAN_POINT('Ctrl Pts',(-10.2470553478132,24.7765532834625,
2.05750358566105));
#105034=CARTESIAN_POINT('Ctrl Pts',(-10.2470872108334,24.7765550558702,
2.05750904318216));
#105035=CARTESIAN_POINT('Ctrl Pts',(-10.2471030640796,24.7765559377375,
2.05751175880661));
#105036=CARTESIAN_POINT('Ctrl Pts',(-10.2471346167457,24.7765576929486,
2.05751716424087));
#105037=CARTESIAN_POINT('Ctrl Pts',(-10.2471503162071,24.7765585662944,
2.0575198540526));
#105038=CARTESIAN_POINT('Ctrl Pts',(-10.2471815640315,24.7765603046135,
2.05752520831324));
#105039=CARTESIAN_POINT('Ctrl Pts',(-10.2471971123952,24.7765611695865,
2.05752787275722));
#105040=CARTESIAN_POINT('Ctrl Pts',(-10.2472280605454,24.7765628912992,
2.05753317669935));
#105041=CARTESIAN_POINT('Ctrl Pts',(-10.2472434603715,24.7765637480408,
2.05753581619937));
#105042=CARTESIAN_POINT('Ctrl Pts',(-10.2472741141421,24.7765654534398,
2.05754107070088));
#105043=CARTESIAN_POINT('Ctrl Pts',(-10.2472893680398,24.7765663020943,
2.05754368568958));
#105044=CARTESIAN_POINT('Ctrl Pts',(-10.2506106921682,24.7767510881966,
2.05811311735182));
#105045=CARTESIAN_POINT('Ctrl Pts',(-10.2539147711035,24.7769356469184,
2.05869129262764));
#105046=CARTESIAN_POINT('Ctrl Pts',(-10.2633945038406,24.777467209496,2.06038374355463));
#105047=CARTESIAN_POINT('Ctrl Pts',(-10.2695649408737,24.7778157029102,
2.06152637482485));
#105048=CARTESIAN_POINT('Ctrl Pts',(-10.309905386508,24.78010954313,2.06926522280969));
#105049=CARTESIAN_POINT('Ctrl Pts',(-10.3438358665295,24.7821116019836,
2.07703833997617));
#105050=CARTESIAN_POINT('Ctrl Pts',(-10.4750927500418,24.7900605614435,
2.11207647409098));
#105051=CARTESIAN_POINT('Ctrl Pts',(-10.5697689891208,24.7962172688534,
2.14818300691642));
#105052=CARTESIAN_POINT('Ctrl Pts',(-10.7219531574316,24.8062743759023,
2.22507325015998));
#105053=CARTESIAN_POINT('Ctrl Pts',(-10.7816325622165,24.8102710585901,
2.26076345786754));
#105054=CARTESIAN_POINT('Ctrl Pts',(-10.8471794523685,24.8146999884512,
2.30658897239966));
#105055=CARTESIAN_POINT('Ctrl Pts',(-10.8557356383931,24.8152790883476,
2.31270920560289));
#105056=CARTESIAN_POINT('Ctrl Pts',(-10.8695022649851,24.8162125626134,
2.32278259531661));
#105057=CARTESIAN_POINT('Ctrl Pts',(-10.8747533986159,24.8165690406242,
2.32667928501118));
#105058=CARTESIAN_POINT('Ctrl Pts',(-10.8840463434081,24.817200692118,2.33367233037473));
#105059=CARTESIAN_POINT('Ctrl Pts',(-10.8880984200942,24.8174763873705,
2.33675481202467));
#105060=CARTESIAN_POINT('Ctrl Pts',(-10.8965953259198,24.8180551073032,
2.34328882623105));
#105061=CARTESIAN_POINT('Ctrl Pts',(-10.9010365056694,24.8183579475871,
2.34674498282833));
#105062=CARTESIAN_POINT('Ctrl Pts',(-10.9127247917844,24.8191559676965,
2.35594962211374));
#105063=CARTESIAN_POINT('Ctrl Pts',(-10.9199375872474,24.8196494540083,
2.36174139429228));
#105064=CARTESIAN_POINT('Ctrl Pts',(-10.9534299806413,24.8219464180653,
2.38916162396316));
#105065=CARTESIAN_POINT('Ctrl Pts',(-10.9790058968157,24.8237160800438,
2.41163502741689));
#105066=CARTESIAN_POINT('Ctrl Pts',(-11.0486162052943,24.8286040907748,
2.4772424776392));
#105067=CARTESIAN_POINT('Ctrl Pts',(-11.0907444791636,24.8316459644391,
2.52229546849885));
#105068=CARTESIAN_POINT('Ctrl Pts',(-11.1903499069329,24.839294572911,2.64329506440552));
#105069=CARTESIAN_POINT('Ctrl Pts',(-11.2434844536331,24.8438285581612,
2.72242722466037));
#105070=CARTESIAN_POINT('Ctrl Pts',(-11.2885639077417,24.8486931558207,
2.80614460752589));
#105071=CARTESIAN_POINT('',(-10.2623899083091,24.85,2.06021397908663));
#105072=CARTESIAN_POINT('Origin',(-10.,24.85,3.5));
#105073=CARTESIAN_POINT('Ctrl Pts',(-10.2623899083091,24.85,2.06021397908664));
#105074=CARTESIAN_POINT('Ctrl Pts',(-10.2594291274866,24.8498363566195,
2.05967439959548));
#105075=CARTESIAN_POINT('Ctrl Pts',(-10.256466711301,24.8496722872369,2.05914395823387));
#105076=CARTESIAN_POINT('Ctrl Pts',(-10.2495003369242,24.8492857040767,
2.05791874490304));
#105077=CARTESIAN_POINT('Ctrl Pts',(-10.2454950964487,24.8490628530452,
2.05723150803905));
#105078=CARTESIAN_POINT('Ctrl Pts',(-10.2318922187377,24.8483040924933,
2.05495574909106));
#105079=CARTESIAN_POINT('Ctrl Pts',(-10.2222817924645,24.8477648259318,
2.05344627314409));
#105080=CARTESIAN_POINT('Ctrl Pts',(-10.1366597278067,24.8429354567096,
2.04087129779938));
#105081=CARTESIAN_POINT('Ctrl Pts',(-10.0599065236917,24.8384371606082,
2.03571107639373));
#105082=CARTESIAN_POINT('Ctrl Pts',(-9.9114909712501,24.8297375046267,2.03742409576804));
#105083=CARTESIAN_POINT('Ctrl Pts',(-9.84002556585704,24.8255488279043,
2.04350711946446));
#105084=CARTESIAN_POINT('Ctrl Pts',(-9.73415547869234,24.8194489279163,
2.06040810974973));
#105085=CARTESIAN_POINT('Ctrl Pts',(-9.69923591611017,24.8174533692662,
2.06729649282874));
#105086=CARTESIAN_POINT('Ctrl Pts',(-9.65492351731635,24.8149439803839,
2.07772952557621));
#105087=CARTESIAN_POINT('Ctrl Pts',(-9.64527003937403,24.8143986904231,
2.08010643275622));
#105088=CARTESIAN_POINT('Ctrl Pts',(-9.62969205842779,24.8135209256829,
2.08411087592061));
#105089=CARTESIAN_POINT('Ctrl Pts',(-9.62375236723478,24.8131867597424,
2.08567765218341));
#105090=CARTESIAN_POINT('Ctrl Pts',(-9.61239062822369,24.8125485100706,
2.08875130067945));
#105091=CARTESIAN_POINT('Ctrl Pts',(-9.60696707107859,24.8122442608207,
2.09025213804092));
#105092=CARTESIAN_POINT('Ctrl Pts',(-9.59461306451122,24.8115521574829,
2.09374764358471));
#105093=CARTESIAN_POINT('Ctrl Pts',(-9.58768840368262,24.8111648897485,
2.09576233947958));
#105094=CARTESIAN_POINT('Ctrl Pts',(-9.56939847084298,24.8101436835533,
2.10123066129191));
#105095=CARTESIAN_POINT('Ctrl Pts',(-9.55805975092885,24.8095123166296,
2.10477164371196));
#105096=CARTESIAN_POINT('Ctrl Pts',(-9.44711984981179,24.8033497224776,
2.14090533450214));
#105097=CARTESIAN_POINT('Ctrl Pts',(-9.35124464501,24.7981709366138,2.18396996148269));
#105098=CARTESIAN_POINT('Ctrl Pts',(-9.2074362515418,24.7900845131843,2.26813332286317));
#105099=CARTESIAN_POINT('Ctrl Pts',(-9.15612277868303,24.7871179047295,
2.30270149573792));
#105100=CARTESIAN_POINT('Ctrl Pts',(-9.07312472955213,24.7819668770101,
2.36660750829619));
#105101=CARTESIAN_POINT('Ctrl Pts',(-9.04027133112096,24.7798218370941,
2.39428904757625));
#105102=CARTESIAN_POINT('Ctrl Pts',(-8.99251277724177,24.7764642644149,
2.43826321416674));
#105103=CARTESIAN_POINT('Ctrl Pts',(-8.97667927815003,24.7753078888398,
2.4535153594305));
#105104=CARTESIAN_POINT('Ctrl Pts',(-8.9573893874117,24.7738356455471,2.47295347379868));
#105105=CARTESIAN_POINT('Ctrl Pts',(-8.9536039602147,24.7735435862806,2.47681048551136));
#105106=CARTESIAN_POINT('Ctrl Pts',(-8.9476144688594,24.7730762779439,2.4829812417967));
#105107=CARTESIAN_POINT('Ctrl Pts',(-8.94539643301385,24.7729020752378,
2.48528142975762));
#105108=CARTESIAN_POINT('Ctrl Pts',(-8.94125808053997,24.7725748560262,
2.48960128431257));
#105109=CARTESIAN_POINT('Ctrl Pts',(-8.93933596065272,24.7724219786784,
2.4916192127733));
#105110=CARTESIAN_POINT('Ctrl Pts',(-8.93500671525298,24.7720755884838,
2.49619032356477));
#105111=CARTESIAN_POINT('Ctrl Pts',(-8.93260303121468,24.7718818085198,
2.49874664888472));
#105112=CARTESIAN_POINT('Ctrl Pts',(-8.92626014115257,24.7713666314852,
2.50554112952221));
#105113=CARTESIAN_POINT('Ctrl Pts',(-8.92233687401905,24.7710440414058,
2.50979400421134));
#105114=CARTESIAN_POINT('Ctrl Pts',(-8.89337719090628,24.7686342084671,
2.54156265153593));
#105115=CARTESIAN_POINT('Ctrl Pts',(-8.86937479010189,24.7664768400813,
2.56999873215808));
#105116=CARTESIAN_POINT('Ctrl Pts',(-8.7883482310404,24.7586993941512,2.67377031262303));
#105117=CARTESIAN_POINT('Ctrl Pts',(-8.73755798709282,24.7528962203545,
2.75367815763544));
#105118=CARTESIAN_POINT('Ctrl Pts',(-8.6706006785835,24.7440600485939,2.88567406886136));
#105119=CARTESIAN_POINT('Ctrl Pts',(-8.64901589062444,24.7409184795032,
2.93471973653624));
#105120=CARTESIAN_POINT('Ctrl Pts',(-8.6230749560714,24.7367160872126,3.00369817624602));
#105121=CARTESIAN_POINT('Ctrl Pts',(-8.61637362965541,24.7355799342274,
3.02269904348583));
#105122=CARTESIAN_POINT('Ctrl Pts',(-8.60542880601142,24.7336314169476,
3.0559021658724));
#105123=CARTESIAN_POINT('Ctrl Pts',(-8.60100489649089,24.7328130529847,
3.07004136745481));
#105124=CARTESIAN_POINT('Ctrl Pts',(-8.59495357559442,24.7316469384374,
3.09046505487861));
#105125=CARTESIAN_POINT('Ctrl Pts',(-8.59315219487416,24.7312932573747,
3.09669666350399));
#105126=CARTESIAN_POINT('Ctrl Pts',(-8.59009106938137,24.7306805393406,
3.10755629750223));
#105127=CARTESIAN_POINT('Ctrl Pts',(-8.58881254406872,24.7304208644429,
3.11217888492791));
#105128=CARTESIAN_POINT('Ctrl Pts',(-8.58639071393676,24.7299215642372,
3.12110572856197));
#105129=CARTESIAN_POINT('Ctrl Pts',(-8.585244288526,24.7296818350373,3.12540907637286));
#105130=CARTESIAN_POINT('Ctrl Pts',(-8.58257537698971,24.7291155787591,
3.13561443681155));
#105131=CARTESIAN_POINT('Ctrl Pts',(-8.58107007635882,24.7287896376719,
3.14152088765067));
#105132=CARTESIAN_POINT('Ctrl Pts',(-8.575895979721,24.7276454689081,3.16236615632213));
#105133=CARTESIAN_POINT('Ctrl Pts',(-8.57242577636303,24.7268339518618,
3.17735354631624));
#105134=CARTESIAN_POINT('Ctrl Pts',(-8.54073177751143,24.7189532020088,
3.32477559623948));
#105135=CARTESIAN_POINT('Ctrl Pts',(-8.53078058614313,24.7125837730757,
3.46045864479805));
#105136=CARTESIAN_POINT('Ctrl Pts',(-8.54311181185355,24.7034578039853,
3.64886156462657));
#105137=CARTESIAN_POINT('Ctrl Pts',(-8.54951165455615,24.7008456605647,
3.70190512406436));
#105138=CARTESIAN_POINT('Ctrl Pts',(-8.56309925339042,24.6968466833171,
3.77885745477992));
#105139=CARTESIAN_POINT('Ctrl Pts',(-8.56802205626959,24.6955543758325,
3.80312414779316));
#105140=CARTESIAN_POINT('Ctrl Pts',(-8.57475636307608,24.6939400496898,
3.83247791672164));
#105141=CARTESIAN_POINT('Ctrl Pts',(-8.57598380297924,24.6936510743543,
3.83769639974791));
#105142=CARTESIAN_POINT('Ctrl Pts',(-8.5779590661662,24.6931939501931,3.84589196899726));
#105143=CARTESIAN_POINT('Ctrl Pts',(-8.57868763310969,24.6930269483273,
3.84887365450549));
#105144=CARTESIAN_POINT('Ctrl Pts',(-8.58009416556339,24.6927075804416,
3.85455240104829));
#105145=CARTESIAN_POINT('Ctrl Pts',(-8.58077044850768,24.6925553165901,
3.8572498616597));
#105146=CARTESIAN_POINT('Ctrl Pts',(-8.58233499923653,24.6922060118392,
3.86341576020236));
#105147=CARTESIAN_POINT('Ctrl Pts',(-8.58322831146318,24.6920086835411,
3.86688288479015));
#105148=CARTESIAN_POINT('Ctrl Pts',(-8.58595346981265,24.6914130519202,
3.87730138884182));
#105149=CARTESIAN_POINT('Ctrl Pts',(-8.58782379238331,24.6910126417514,
3.88424247799121));
#105150=CARTESIAN_POINT('Ctrl Pts',(-8.6080231778388,24.686775995411,3.9570658750242));
#105151=CARTESIAN_POINT('Ctrl Pts',(-8.63089566489016,24.6827176243203,
4.02159376841027));
#105152=CARTESIAN_POINT('Ctrl Pts',(-8.69836500900632,24.6725707099685,
4.17653850077667));
#105153=CARTESIAN_POINT('Ctrl Pts',(-8.74795193193392,24.6664707888472,
4.26441976847686));
#105154=CARTESIAN_POINT('Ctrl Pts',(-8.83224632023054,24.6580391922193,
4.38329851656673));
#105155=CARTESIAN_POINT('Ctrl Pts',(-8.86001182765142,24.6554863607658,
4.41885390904803));
#105156=CARTESIAN_POINT('Ctrl Pts',(-8.89595055852964,24.6524394681986,
4.46073355825489));
#105157=CARTESIAN_POINT('Ctrl Pts',(-8.90260325712436,24.6518853607138,
4.46832563477504));
#105158=CARTESIAN_POINT('Ctrl Pts',(-8.91320950731871,24.6510172282972,
4.48017980742984));
#105159=CARTESIAN_POINT('Ctrl Pts',(-8.91711073153144,24.6507010834561,
4.48448812255364));
#105160=CARTESIAN_POINT('Ctrl Pts',(-8.92445670384538,24.6501116381319,
4.49250414566848));
#105161=CARTESIAN_POINT('Ctrl Pts',(-8.92789520938317,24.6498380867601,
4.49621743604652));
#105162=CARTESIAN_POINT('Ctrl Pts',(-8.93561663412909,24.6492289971289,
4.50446963312238));
#105163=CARTESIAN_POINT('Ctrl Pts',(-8.93990947702241,24.6488938793912,
4.50899914673763));
#105164=CARTESIAN_POINT('Ctrl Pts',(-8.95083950925738,24.6480493627953,
4.52038501185914));
#105165=CARTESIAN_POINT('Ctrl Pts',(-8.95751508060099,24.6475415869777,
4.52720421835969));
#105166=CARTESIAN_POINT('Ctrl Pts',(-8.9966891442227,24.6446069756169,4.56644592139786));
#105167=CARTESIAN_POINT('Ctrl Pts',(-9.03063352376917,24.6422433383268,
4.59739178513435));
#105168=CARTESIAN_POINT('Ctrl Pts',(-9.16117987816289,24.633685300483,4.70561387469747));
#105169=CARTESIAN_POINT('Ctrl Pts',(-9.26598987975165,24.6278595022033,
4.77214370741468));
#105170=CARTESIAN_POINT('Ctrl Pts',(-9.41182376773701,24.6197144978389,
4.84062852762631));
#105171=CARTESIAN_POINT('Ctrl Pts',(-9.44633523751368,24.6177804703049,
4.8552457441372));
#105172=CARTESIAN_POINT('Ctrl Pts',(-9.48734177391967,24.6154337611059,
4.87078613349755));
#105173=CARTESIAN_POINT('Ctrl Pts',(-9.49333162252724,24.6150897798904,
4.87301137392175));
#105174=CARTESIAN_POINT('Ctrl Pts',(-9.50255520585566,24.6145579871835,
4.8763693783042));
#105175=CARTESIAN_POINT('Ctrl Pts',(-9.50577874114772,24.6143717384551,
4.87753015777379));
#105176=CARTESIAN_POINT('Ctrl Pts',(-9.51168709327346,24.6140295974502,
4.87963431869737));
#105177=CARTESIAN_POINT('Ctrl Pts',(-9.51437065346074,24.6138739068898,
4.88058121308144));
#105178=CARTESIAN_POINT('Ctrl Pts',(-9.5203627398795,24.6135255933434,4.88267588836327));
#105179=CARTESIAN_POINT('Ctrl Pts',(-9.5236726129921,24.6133327426844,4.88381961737125));
#105180=CARTESIAN_POINT('Ctrl Pts',(-9.53334725792986,24.6127677974792,
4.88712387576559));
#105181=CARTESIAN_POINT('Ctrl Pts',(-9.53972276040559,24.6123939291749,
4.88925242040763));
#105182=CARTESIAN_POINT('Ctrl Pts',(-9.58432240659645,24.6097686921195,
4.90380189305999));
#105183=CARTESIAN_POINT('Ctrl Pts',(-9.62302644756556,24.6074404703867,
4.9146865424151));
#105184=CARTESIAN_POINT('Ctrl Pts',(-9.75920354549396,24.5991877266641,
4.94699827364544));
#105185=CARTESIAN_POINT('Ctrl Pts',(-9.8583829156248,24.5930905596194,4.96004549770521));
#105186=CARTESIAN_POINT('Ctrl Pts',(-10.0220096834828,24.583415024782,4.96472960852542));
#105187=CARTESIAN_POINT('Ctrl Pts',(-10.0859542143189,24.5797239646815,
4.96237162434377));
#105188=CARTESIAN_POINT('Ctrl Pts',(-10.1647329946187,24.5753089594819,
4.95427932492971));
#105189=CARTESIAN_POINT('Ctrl Pts',(-10.1798945711884,24.5744651323343,
4.95248176661586));
#105190=CARTESIAN_POINT('Ctrl Pts',(-10.2017665091955,24.573255985346,4.94954088811324));
#105191=CARTESIAN_POINT('Ctrl Pts',(-10.2085010349554,24.5728847991195,
4.9485875296794));
#105192=CARTESIAN_POINT('Ctrl Pts',(-10.2202522670661,24.5722390050332,
4.94684034448711));
#105193=CARTESIAN_POINT('Ctrl Pts',(-10.2252719048963,24.5719637547877,
4.9460672921226));
#105194=CARTESIAN_POINT('Ctrl Pts',(-10.2349818645042,24.5714324545567,
4.9445201176456));
#105195=CARTESIAN_POINT('Ctrl Pts',(-10.2396726328913,24.5711763069097,
4.94374924301355));
#105196=CARTESIAN_POINT('Ctrl Pts',(-10.2508358201856,24.5705679179475,
4.94185879528529));
#105197=CARTESIAN_POINT('Ctrl Pts',(-10.2573046527188,24.5702163294641,
4.9407184707012));
#105198=CARTESIAN_POINT('Ctrl Pts',(-10.2804258077683,24.5689629438389,
4.93648198575687));
#105199=CARTESIAN_POINT('Ctrl Pts',(-10.2970321296506,24.5680688368206,
4.93314028421529));
#105200=CARTESIAN_POINT('Ctrl Pts',(-10.4232811516126,24.5613107676496,
4.90544633022203));
#105201=CARTESIAN_POINT('Ctrl Pts',(-10.5298502132546,24.5558721878848,
4.86883446621369));
#105202=CARTESIAN_POINT('Ctrl Pts',(-10.7102209707958,24.5461494729348,
4.78261117248292));
#105203=CARTESIAN_POINT('Ctrl Pts',(-10.7856900925438,24.5418802834471,
4.73781762438034));
#105204=CARTESIAN_POINT('Ctrl Pts',(-10.8639450952309,24.5367548153914,
4.68131755219346));
#105205=CARTESIAN_POINT('Ctrl Pts',(-10.8711501083713,24.5362758105037,
4.67601435681554));
#105206=CARTESIAN_POINT('Ctrl Pts',(-10.8813941578492,24.5355838378299,
4.66832850467759));
#105207=CARTESIAN_POINT('Ctrl Pts',(-10.8844732311435,24.5353744189112,
4.66599925344385));
#105208=CARTESIAN_POINT('Ctrl Pts',(-10.8897905057381,24.5350102172733,
4.66194367143839));
#105209=CARTESIAN_POINT('Ctrl Pts',(-10.8920330133011,24.5348558257488,
4.66022297113469));
#105210=CARTESIAN_POINT('Ctrl Pts',(-10.8966939342908,24.5345332454733,
4.65662509512259));
#105211=CARTESIAN_POINT('Ctrl Pts',(-10.899111454672,24.5343649805011,4.65474681821634));
#105212=CARTESIAN_POINT('Ctrl Pts',(-10.905496296162,24.5339181022548,4.64975395110147));
#105213=CARTESIAN_POINT('Ctrl Pts',(-10.9094534031084,24.5336385948903,
4.64662644155455));
#105214=CARTESIAN_POINT('Ctrl Pts',(-10.9261746208772,24.532446944159,4.63326977395955));
#105215=CARTESIAN_POINT('Ctrl Pts',(-10.9387824430841,24.5315221616816,
4.62284784674164));
#105216=CARTESIAN_POINT('Ctrl Pts',(-11.0306268022558,24.5246055754881,
4.5442989036557));
#105217=CARTESIAN_POINT('Ctrl Pts',(-11.1025349205422,24.5182068137967,
4.46807391483109));
#105218=CARTESIAN_POINT('Ctrl Pts',(-11.2036854259467,24.5081851635343,
4.33481653555556));
#105219=CARTESIAN_POINT('Ctrl Pts',(-11.2384033829476,24.5044777918534,
4.2823909842636));
#105220=CARTESIAN_POINT('Ctrl Pts',(-11.2866596134648,24.4989271085745,
4.19821859625217));
#105221=CARTESIAN_POINT('Ctrl Pts',(-11.3026268927655,24.4970047640162,
4.16795630382618));
#105222=CARTESIAN_POINT('Ctrl Pts',(-11.3214916805296,24.494616809187,4.12894770061124));
#105223=CARTESIAN_POINT('Ctrl Pts',(-11.325386549232,24.4941167315327,4.12069797185017));
#105224=CARTESIAN_POINT('Ctrl Pts',(-11.331511122883,24.4933187147972,4.10740495130876));
#105225=CARTESIAN_POINT('Ctrl Pts',(-11.3337898650438,24.4930190922183,
4.10238462987594));
#105226=CARTESIAN_POINT('Ctrl Pts',(-11.3380659612539,24.4924515972576,
4.09282068563827));
#105227=CARTESIAN_POINT('Ctrl Pts',(-11.3400686728381,24.4921835442227,
4.08827955506737));
#105228=CARTESIAN_POINT('Ctrl Pts',(-11.3445763650981,24.4915749528857,
4.07791593089748));
#105229=CARTESIAN_POINT('Ctrl Pts',(-11.3470667080947,24.491234916802,4.07208715284194));
#105230=CARTESIAN_POINT('Ctrl Pts',(-11.3534337245679,24.4903554051297,
4.05691271196101));
#105231=CARTESIAN_POINT('Ctrl Pts',(-11.3572515273751,24.4898179199295,
4.04754261374875));
#105232=CARTESIAN_POINT('Ctrl Pts',(-11.3828935532509,24.4861351589582,
3.98269239327272));
#105233=CARTESIAN_POINT('Ctrl Pts',(-11.4014083083704,24.4831031324559,
3.92596051283679));
#105234=CARTESIAN_POINT('Ctrl Pts',(-11.4430675317994,24.4748791585684,
3.76572625701971));
#105235=CARTESIAN_POINT('Ctrl Pts',(-11.4585112309955,24.46987996121,3.66061611863117));
#105236=CARTESIAN_POINT('Ctrl Pts',(-11.4631583753308,24.4636910495957,
3.53651482612231));
#105237=CARTESIAN_POINT('Ctrl Pts',(-11.4634999999691,24.4627726088713,
3.51825682543672));
#105238=CARTESIAN_POINT('Ctrl Pts',(-11.4635,24.4618423224409,3.5000000024766));
#105239=CARTESIAN_POINT('Origin',(-10.,24.85,3.5));
#105240=CARTESIAN_POINT('',(-11.3004035488554,24.85,2.82859635082588));
#105241=CARTESIAN_POINT('',(-11.4635,24.85,3.5));
#105242=CARTESIAN_POINT('Origin',(-10.,24.85,3.5));
#105243=CARTESIAN_POINT('Ctrl Pts',(-11.3004035488553,24.85,2.82859635082581));
#105244=CARTESIAN_POINT('Ctrl Pts',(-11.3125618755898,24.85,2.85843423653158));
#105245=CARTESIAN_POINT('Ctrl Pts',(-11.3236469117651,24.85,2.88866598859084));
#105246=CARTESIAN_POINT('Ctrl Pts',(-11.3336107592203,24.85,2.91926079192103));
#105247=CARTESIAN_POINT('Ctrl Pts',(-11.351398587096,24.85,2.97387976295373));
#105248=CARTESIAN_POINT('Ctrl Pts',(-11.3656158973012,24.85,3.02965613094422));
#105249=CARTESIAN_POINT('Ctrl Pts',(-11.3763225973211,24.85,3.08625266725227));
#105250=CARTESIAN_POINT('Ctrl Pts',(-11.3802128743286,24.85,3.10681700579705));
#105251=CARTESIAN_POINT('Ctrl Pts',(-11.3836391895696,24.85,3.12748960196462));
#105252=CARTESIAN_POINT('Ctrl Pts',(-11.3866028162641,24.85,3.14825403475913));
#105253=CARTESIAN_POINT('Ctrl Pts',(-11.3891864342721,24.85,3.16635596459899));
#105254=CARTESIAN_POINT('Ctrl Pts',(-11.3914188580782,24.85,3.18453415298079));
#105255=CARTESIAN_POINT('Ctrl Pts',(-11.3932974125123,24.85,3.20274227033469));
#105256=CARTESIAN_POINT('Ctrl Pts',(-11.3992038488262,24.85,3.25999112274849));
#105257=CARTESIAN_POINT('Ctrl Pts',(-11.4016259665454,24.85,3.31758827200733));
#105258=CARTESIAN_POINT('Ctrl Pts',(-11.4006269322846,24.85,3.37519248066477));
#105259=CARTESIAN_POINT('Ctrl Pts',(-11.3999593676723,24.85,3.41368418483278));
#105260=CARTESIAN_POINT('Ctrl Pts',(-11.3977631279099,24.85,3.45217902944069));
#105261=CARTESIAN_POINT('Ctrl Pts',(-11.3940446763944,24.85,3.49057134449431));
#105262=CARTESIAN_POINT('Ctrl Pts',(-11.3924040169226,24.85,3.50751084607837));
#105263=CARTESIAN_POINT('Ctrl Pts',(-11.3904668951253,24.85,3.52443032836664));
#105264=CARTESIAN_POINT('Ctrl Pts',(-11.3882332939498,24.85,3.54132038036121));
#105265=CARTESIAN_POINT('Ctrl Pts',(-11.3867101763176,24.85,3.55283789579101));
#105266=CARTESIAN_POINT('Ctrl Pts',(-11.385048893467,24.85,3.56434288508996));
#105267=CARTESIAN_POINT('Ctrl Pts',(-11.383252385453,24.85,3.57581506234222));
#105268=CARTESIAN_POINT('Ctrl Pts',(-11.3745487112871,24.85,3.63139516106727));
#105269=CARTESIAN_POINT('Ctrl Pts',(-11.3626636031163,24.85,3.68630052936635));
#105270=CARTESIAN_POINT('Ctrl Pts',(-11.3476521220032,24.85,3.74021322586292));
#105271=CARTESIAN_POINT('Ctrl Pts',(-11.3330120872859,24.85,3.79279189831172));
#105272=CARTESIAN_POINT('Ctrl Pts',(-11.3153979702509,24.85,3.84442733350712));
#105273=CARTESIAN_POINT('Ctrl Pts',(-11.2948184588981,24.85,3.89480080308046));
#105274=CARTESIAN_POINT('Ctrl Pts',(-11.28259085348,24.85,3.92473090680962));
#105275=CARTESIAN_POINT('Ctrl Pts',(-11.2693156001385,24.85,3.95421497642643));
#105276=CARTESIAN_POINT('Ctrl Pts',(-11.2549882247325,24.85,3.98318007522436));
#105277=CARTESIAN_POINT('Ctrl Pts',(-11.2448400683478,24.85,4.00369620912678));
#105278=CARTESIAN_POINT('Ctrl Pts',(-11.2341639691643,24.85,4.0239518800964));
#105279=CARTESIAN_POINT('Ctrl Pts',(-11.2229570283328,24.85,4.04391943548386));
#105280=CARTESIAN_POINT('Ctrl Pts',(-11.2180985058252,24.85,4.05257592959147));
#105281=CARTESIAN_POINT('Ctrl Pts',(-11.2131400386115,24.85,4.06117831142199));
#105282=CARTESIAN_POINT('Ctrl Pts',(-11.2080890554702,24.85,4.06971182776291));
#105283=CARTESIAN_POINT('Ctrl Pts',(-11.1812246840833,24.85,4.11509854670538));
#105284=CARTESIAN_POINT('Ctrl Pts',(-11.1516963968566,24.85,4.15863054938992));
#105285=CARTESIAN_POINT('Ctrl Pts',(-11.1195205442675,24.85,4.20001692638652));
#105286=CARTESIAN_POINT('Ctrl Pts',(-11.1125970057767,24.85,4.20892236792339));
#105287=CARTESIAN_POINT('Ctrl Pts',(-11.1055507414306,24.85,4.21772833257868));
#105288=CARTESIAN_POINT('Ctrl Pts',(-11.0983816907031,24.85,4.22643169138809));
#105289=CARTESIAN_POINT('Ctrl Pts',(-11.0643171649521,24.85,4.26778664918564));
#105290=CARTESIAN_POINT('Ctrl Pts',(-11.0274823323406,24.85,4.30682867683741));
#105291=CARTESIAN_POINT('Ctrl Pts',(-10.9881733610665,24.85,4.34342341161918));
#105292=CARTESIAN_POINT('Ctrl Pts',(-10.9564831645753,24.85,4.37292543871853));
#105293=CARTESIAN_POINT('Ctrl Pts',(-10.9231840933228,24.85,4.40083613613505));
#105294=CARTESIAN_POINT('Ctrl Pts',(-10.8884241147858,24.85,4.42706182455881));
#105295=CARTESIAN_POINT('Ctrl Pts',(-10.8802209909417,24.85,4.43325091267364));
#105296=CARTESIAN_POINT('Ctrl Pts',(-10.8719430995626,24.85,4.43934102278144));
#105297=CARTESIAN_POINT('Ctrl Pts',(-10.8635972985758,24.85,4.44532811031609));
#105298=CARTESIAN_POINT('Ctrl Pts',(-10.8209284670976,24.85,4.47593775814561));
#105299=CARTESIAN_POINT('Ctrl Pts',(-10.7764485190081,24.85,4.50388699710063));
#105300=CARTESIAN_POINT('Ctrl Pts',(-10.7304487595703,24.85,4.52906821597762));
#105301=CARTESIAN_POINT('Ctrl Pts',(-10.6846750591674,24.85,4.55412568546749));
#105302=CARTESIAN_POINT('Ctrl Pts',(-10.6373952802604,24.85,4.57644253090575));
#105303=CARTESIAN_POINT('Ctrl Pts',(-10.5888840527018,24.85,4.59586320662698));
#105304=CARTESIAN_POINT('Ctrl Pts',(-10.5645845311458,24.85,4.60559112224716));
#105305=CARTESIAN_POINT('Ctrl Pts',(-10.5399759463448,24.85,4.61459157026943));
#105306=CARTESIAN_POINT('Ctrl Pts',(-10.515093012538,24.85,4.62283999060172));
#105307=CARTESIAN_POINT('Ctrl Pts',(-10.4967624813286,24.85,4.62891636115766));
#105308=CARTESIAN_POINT('Ctrl Pts',(-10.4782830689616,24.85,4.63458454898126));
#105309=CARTESIAN_POINT('Ctrl Pts',(-10.4596689220486,24.85,4.6398335167748));
#105310=CARTESIAN_POINT('Ctrl Pts',(-10.4506717510829,24.85,4.64237061185912));
#105311=CARTESIAN_POINT('Ctrl Pts',(-10.4416440578635,24.85,4.6448093832563));
#105312=CARTESIAN_POINT('Ctrl Pts',(-10.4325999392588,24.85,4.64714563599666));
#105313=CARTESIAN_POINT('Ctrl Pts',(-10.3837719044625,24.85,4.65975876449322));
#105314=CARTESIAN_POINT('Ctrl Pts',(-10.3343687941817,24.85,4.66941559578891));
#105315=CARTESIAN_POINT('Ctrl Pts',(-10.2846440492021,24.85,4.67598884653307));
#105316=CARTESIAN_POINT('Ctrl Pts',(-10.2359323305191,24.85,4.68242818254602));
#105317=CARTESIAN_POINT('Ctrl Pts',(-10.1869110047086,24.85,4.68590832870446));
#105318=CARTESIAN_POINT('Ctrl Pts',(-10.1378247465409,24.85,4.68626042890209));
#105319=CARTESIAN_POINT('Ctrl Pts',(-10.0887384883732,24.85,4.68661252909973));
#105320=CARTESIAN_POINT('Ctrl Pts',(-10.039586391101,24.85,4.68383676613634));
#105321=CARTESIAN_POINT('Ctrl Pts',(-9.99063336962943,24.85,4.67771275306651));
#105322=CARTESIAN_POINT('Ctrl Pts',(-8.88741263453866,24.85,3.88631788102315));
#105323=CARTESIAN_POINT('Ctrl Pts',(-8.81508513359861,24.85,3.73963918744251));
#105324=CARTESIAN_POINT('Ctrl Pts',(-8.78311241042471,24.85,3.59288578274215));
#105325=CARTESIAN_POINT('Ctrl Pts',(-8.76395555587307,24.85,3.29953678129824));
#105326=CARTESIAN_POINT('Ctrl Pts',(-8.78327471948896,24.85,3.14104654297177));
#105327=CARTESIAN_POINT('Ctrl Pts',(-8.87385485848026,24.85,2.84353830916111));
#105328=CARTESIAN_POINT('Ctrl Pts',(-8.9447791067978,24.85,2.70306361360872));
#105329=CARTESIAN_POINT('Ctrl Pts',(-9.13798618895579,24.85,2.4539623946865));
#105330=CARTESIAN_POINT('Ctrl Pts',(-9.26068603117401,24.85,2.34761760023775));
#105331=CARTESIAN_POINT('Ctrl Pts',(-9.52437211317925,24.85,2.18773266971445));
#105332=CARTESIAN_POINT('Ctrl Pts',(-9.66339960403327,24.85,2.13073968047222));
#105333=CARTESIAN_POINT('Ctrl Pts',(-9.95596335995801,24.85,2.05973084110956));
#105334=CARTESIAN_POINT('Ctrl Pts',(-10.1100968233425,24.85,2.04702898053788));
#105335=CARTESIAN_POINT('Ctrl Pts',(-10.2623899083091,24.85,2.06021397908666));
#105336=CARTESIAN_POINT('Origin',(-10.,24.85,3.5));
#105337=CARTESIAN_POINT('Ctrl Pts',(-10.5090140092792,13.1337998239626,
2.44023125247533));
#105338=CARTESIAN_POINT('Ctrl Pts',(-10.8605022655926,13.1601924775763,
2.60904375492577));
#105339=CARTESIAN_POINT('Ctrl Pts',(-11.3762582958501,13.2129702164138,
3.3207757270411));
#105340=CARTESIAN_POINT('Ctrl Pts',(-10.8990613565784,13.2921330404754,
4.55894989925235));
#105341=CARTESIAN_POINT('Ctrl Pts',(-9.60213183554956,13.3712882961471,
4.82960051060231));
#105342=CARTESIAN_POINT('Ctrl Pts',(-8.6680683892318,13.4504435518189,3.89129233265225));
#105343=CARTESIAN_POINT('Ctrl Pts',(-8.94638477794343,13.5295988074907,
2.59588490110802));
#105344=CARTESIAN_POINT('Ctrl Pts',(-10.1841644808861,13.6087540631624,
2.12409172341792));
#105345=CARTESIAN_POINT('Ctrl Pts',(-11.2541792099669,13.6879093188342,
2.90481120670036));
#105346=CARTESIAN_POINT('Ctrl Pts',(-11.182332230381,13.767064574506,4.22755695617222));
#105347=CARTESIAN_POINT('Ctrl Pts',(-10.0339701846483,13.8462198301777,
4.88781414517024));
#105348=CARTESIAN_POINT('Ctrl Pts',(-8.85469118695272,13.9253750858495,
4.28452438368559));
#105349=CARTESIAN_POINT('Ctrl Pts',(-8.71818818692633,14.0045303415213,
2.96692304576068));
#105350=CARTESIAN_POINT('Ctrl Pts',(-9.74875435949711,14.083685597193,2.13468707585548));
#105351=CARTESIAN_POINT('Ctrl Pts',(-11.0080732815695,14.1628408528648,
2.54553861657238));
#105352=CARTESIAN_POINT('Ctrl Pts',(-11.3495611174537,14.2419961085365,
3.82541187780965));
#105353=CARTESIAN_POINT('Ctrl Pts',(-10.4622981596486,14.3211513642083,
4.80900243763703));
#105354=CARTESIAN_POINT('Ctrl Pts',(-9.154121563492,14.4003066198801,4.60077124308019));
#105355=CARTESIAN_POINT('Ctrl Pts',(-8.61610143836823,14.4794618755519,
3.3903079498792));
#105356=CARTESIAN_POINT('Ctrl Pts',(-9.3380953065286,14.5586171312236,2.2797174047905));
#105357=CARTESIAN_POINT('Ctrl Pts',(-10.6627410645075,14.6377723868954,
2.28017139776325));
#105358=CARTESIAN_POINT('Ctrl Pts',(-11.3839734156908,14.7169276425671,
3.39125671511969));
#105359=CARTESIAN_POINT('Ctrl Pts',(-10.8451236777656,14.7960828982389,
4.60135074808574));
#105360=CARTESIAN_POINT('Ctrl Pts',(-9.53680453925627,14.8752381539106,
4.80868540180449));
#105361=CARTESIAN_POINT('Ctrl Pts',(-8.65021625863274,14.9543934095824,
3.82448630689678));
#105362=CARTESIAN_POINT('Ctrl Pts',(-8.99258099578772,15.0335486652542,
2.54484846228196));
#105363=CARTESIAN_POINT('Ctrl Pts',(-10.2521820169156,15.112703920926,2.1348583434421));
#105364=CARTESIAN_POINT('Ctrl Pts',(-11.2821759977529,15.1918591765977,
2.96780433840964));
#105365=CARTESIAN_POINT('Ctrl Pts',(-11.1447725563174,15.2710144322695,
4.28530459413146));
#105366=CARTESIAN_POINT('Ctrl Pts',(-9.96507497325763,15.3501696879412,
4.88779960875228));
#105367=CARTESIAN_POINT('Ctrl Pts',(-8.81717597805976,15.429324943613,4.22672886591294));
#105368=CARTESIAN_POINT('Ctrl Pts',(-8.74621627703462,15.5084801992848,
2.90398499394259));
#105369=CARTESIAN_POINT('Ctrl Pts',(-9.81680335943576,15.5876354549565,
2.12390171050809));
#105370=CARTESIAN_POINT('Ctrl Pts',(-11.0541875791356,15.6667907106283,
2.59673035065145));
#105371=CARTESIAN_POINT('Ctrl Pts',(-11.3317535956899,15.7459459663,3.89196922303317));
#105372=CARTESIAN_POINT('Ctrl Pts',(-10.3967827084337,15.8251012219718,
4.83032740095482));
#105373=CARTESIAN_POINT('Ctrl Pts',(-9.10054853769248,15.9042564776436,
4.55744719886774));
#105374=CARTESIAN_POINT('Ctrl Pts',(-8.62324821084428,15.9834117333153,
3.3217809704406));
#105375=CARTESIAN_POINT('Ctrl Pts',(-9.39945480685586,16.0625669889871,
2.24837985697228));
#105376=CARTESIAN_POINT('Ctrl Pts',(-10.7224466426081,16.1417222446589,
2.3145556276125));
#105377=CARTESIAN_POINT('Ctrl Pts',(-11.3876642339107,16.2208775003306,
3.46005647279232));
#105378=CARTESIAN_POINT('Ctrl Pts',(-10.789439324166,16.3000327560024,4.64192515731166));
#105379=CARTESIAN_POINT('Ctrl Pts',(-9.47244457819178,16.3791880116741,
4.78409220399535));
#105380=CARTESIAN_POINT('Ctrl Pts',(-8.63577924136583,16.4583432673459,
3.75711715841716));
#105381=CARTESIAN_POINT('Ctrl Pts',(-9.04121155694682,16.5374985230177,
2.49604171754569));
#105382=CARTESIAN_POINT('Ctrl Pts',(-10.3196029348599,16.6166537786894,
2.14905163848878));
#105383=CARTESIAN_POINT('Ctrl Pts',(-11.3070017790651,16.6958090343612,
3.03207494087031));
#105384=CARTESIAN_POINT('Ctrl Pts',(-11.1043997885858,16.774964290033,4.34113531516184));
#105385=CARTESIAN_POINT('Ctrl Pts',(-9.89626231124403,16.8541195457047,
4.88435761397571));
#105386=CARTESIAN_POINT('Ctrl Pts',(-8.78257607198402,16.9332748013765,
4.16714802775323));
#105387=CARTESIAN_POINT('Ctrl Pts',(-8.77733169845742,17.0124300570483,
2.84251255841355));
#105388=CARTESIAN_POINT('Ctrl Pts',(-9.88530409531549,17.09158531272,2.11650718798777));
#105389=CARTESIAN_POINT('Ctrl Pts',(-11.0977049822458,17.1707405683918,
2.65014631647928));
#105390=CARTESIAN_POINT('Ctrl Pts',(-11.3106658790912,17.2498958240635,
3.95756143284488));
#105391=CARTESIAN_POINT('Ctrl Pts',(-10.3302898462604,17.3290510797353,
4.84837536646819));
#105392=CARTESIAN_POINT('Ctrl Pts',(-9.04919104546304,17.4082063354071,
4.5115185828314));
#105393=CARTESIAN_POINT('Ctrl Pts',(-8.63378613096917,17.4873615910788,
3.25369292436326));
#105394=CARTESIAN_POINT('Ctrl Pts',(-9.4622935588648,17.5665168467506,2.2201252816769));
#105395=CARTESIAN_POINT('Ctrl Pts',(-10.7803727103917,17.6456721024224,
2.35185978891218));
#105396=CARTESIAN_POINT('Ctrl Pts',(-11.3879370090656,17.7248273580941,
3.52895462496553));
#105397=CARTESIAN_POINT('Ctrl Pts',(-10.7318104499819,17.8039826137659,
4.67968681298818));
#105398=CARTESIAN_POINT('Ctrl Pts',(-9.40938407382203,17.8831378694376,
4.75633607732401));
#105399=CARTESIAN_POINT('Ctrl Pts',(-8.62470252432374,17.9622931251094,
3.68911468700078));
#105400=CARTESIAN_POINT('Ctrl Pts',(-9.09220377228481,18.0414483807812,
2.4497078880678));
#105401=CARTESIAN_POINT('Ctrl Pts',(-10.3862366179896,18.1206036364529,
2.16657254176879));
#105402=CARTESIAN_POINT('Ctrl Pts',(-11.3286081996048,18.1997588921247,
3.09749812002438));
#105403=CARTESIAN_POINT('Ctrl Pts',(-11.0613067020991,18.2789141477965,
4.394894181186));
#105404=CARTESIAN_POINT('Ctrl Pts',(-9.82770517227246,18.3580694034682,
4.87750571823832));
#105405=CARTESIAN_POINT('Ctrl Pts',(-8.75097488171399,18.43722465914,4.10592389400942));
#105406=CARTESIAN_POINT('Ctrl Pts',(-8.81145875345403,18.5163799148118,
2.78265962284292));
#105407=CARTESIAN_POINT('Ctrl Pts',(-9.95408734611271,18.5955351704835,
2.11252043631124));
#105408=CARTESIAN_POINT('Ctrl Pts',(-11.1385185570414,18.6746904261553,
2.70565561202124));
#105409=CARTESIAN_POINT('Ctrl Pts',(-11.2863497763831,18.7538456818271,
4.02202659342217));
#105410=CARTESIAN_POINT('Ctrl Pts',(-10.2629834257514,18.8330009374988,
4.8631020611902));
#105411=CARTESIAN_POINT('Ctrl Pts',(-9.00017555241863,18.9121561931706,
4.4630984297877));
#105412=CARTESIAN_POINT('Ctrl Pts',(-8.64768926105856,18.9913114488423,
3.18621157321436));
#105413=CARTESIAN_POINT('Ctrl Pts',(-9.52645677047307,19.0704667045141,
2.19502324878559));
#105414=CARTESIAN_POINT('Ctrl Pts',(-10.8363765915541,19.1496219601858,
2.39199200880984));
#105415=CARTESIAN_POINT('Ctrl Pts',(-11.3847910665814,19.2287772158577,
3.59778145712457));
#105416=CARTESIAN_POINT('Ctrl Pts',(-10.6723790060287,19.3079324715294,
4.71454270558623));
#105417=CARTESIAN_POINT('Ctrl Pts',(-9.34777835383489,19.3870877272012,
4.72548538780132));
#105418=CARTESIAN_POINT('Ctrl Pts',(-8.61701339166654,19.4662429828729,
3.62064639493691));
#105419=CARTESIAN_POINT('Ctrl Pts',(-9.1454320393717,19.5453982385447,2.40596110119043));
#105420=CARTESIAN_POINT('Ctrl Pts',(-10.4519189366623,19.6245534942164,
2.18737789667895));
#105421=CARTESIAN_POINT('Ctrl Pts',(-11.3469420391427,19.7037087498882,
3.16391272765676));
#105422=CARTESIAN_POINT('Ctrl Pts',(-11.0155994422605,19.78286400556,4.44644877532865));
#105423=CARTESIAN_POINT('Ctrl Pts',(-9.75957242386244,19.8620192612317,
4.86726079885059));
#105424=CARTESIAN_POINT('Ctrl Pts',(-8.72245024619805,19.9411745169035,
4.04320726983491));
#105425=CARTESIAN_POINT('Ctrl Pts',(-8.84851338145853,20.0203297725752,
2.72457361486673));
#105426=CARTESIAN_POINT('Ctrl Pts',(-10.0229836873447,20.0994850282471,
2.11195127551048));
#105427=CARTESIAN_POINT('Ctrl Pts',(-11.176527772959,20.1786402839188,2.76312150872955));
#105428=CARTESIAN_POINT('Ctrl Pts',(-11.2588651821356,20.2577955395905,
4.08520591644964));
#105429=CARTESIAN_POINT('Ctrl Pts',(-10.195029233715,20.3369507952623,4.87447121084345));
#105430=CARTESIAN_POINT('Ctrl Pts',(-8.95362279179843,20.4161060509341,
4.41230600655548));
#105431=CARTESIAN_POINT('Ctrl Pts',(-8.6649233554112,20.4952613066058,3.11950313468514));
#105432=CARTESIAN_POINT('Ctrl Pts',(-9.59178639711394,20.5744165622776,
2.17313558874325));
#105433=CARTESIAN_POINT('Ctrl Pts',(-10.8903203393042,20.6535718179494,
2.43485343503247));
#105434=CARTESIAN_POINT('Ctrl Pts',(-11.3782341554329,20.7327270736211,
3.66636743743653));
#105435=CARTESIAN_POINT('Ctrl Pts',(-10.6112913817496,20.8118823292929,
4.74640697929671));
#105436=CARTESIAN_POINT('Ctrl Pts',(-9.28777916327362,20.8910375849647,
4.69161612576101));
#105437=CARTESIAN_POINT('Ctrl Pts',(-8.61273078299548,20.9701928406364,
3.55188093091511));
#105438=CARTESIAN_POINT('Ctrl Pts',(-9.20076524821148,21.0493480963082,
2.36490911246084));
#105439=CARTESIAN_POINT('Ctrl Pts',(-10.5164881045002,21.1285033519799,
2.21141645620059));
#105440=CARTESIAN_POINT('Ctrl Pts',(-11.3619581384099,21.2076586076517,
3.2311551736411));
#105441=CARTESIAN_POINT('Ctrl Pts',(-10.9673905935855,21.2868138633234,
4.49567211012625));
#105442=CARTESIAN_POINT('Ctrl Pts',(-9.69203188820424,21.3659691189952,
4.85364809073771));
#105443=CARTESIAN_POINT('Ctrl Pts',(-8.69707242631543,21.445124374667,3.9791526366132));
#105444=CARTESIAN_POINT('Ctrl Pts',(-8.88840431081413,21.5242796303387,
2.66839760989743));
#105445=CARTESIAN_POINT('Ctrl Pts',(-10.091823415966,21.6034348860105,2.11480110752238));
#105446=CARTESIAN_POINT('Ctrl Pts',(-11.2116390070345,21.6825901416822,
2.82240245862798));
#105447=CARTESIAN_POINT('Ctrl Pts',(-11.2282797954346,21.7617453973541,
4.14694378084031));
#105448=CARTESIAN_POINT('Ctrl Pts',(-10.1265946525276,21.8409006530258,
4.88245481133823));
#105449=CARTESIAN_POINT('Ctrl Pts',(-8.90964743072545,21.9200559086976,
4.3592664232458));
#105450=CARTESIAN_POINT('Ctrl Pts',(-8.68544596361199,21.9992111643693,
3.05373192265566));
#105451=CARTESIAN_POINT('Ctrl Pts',(-9.65812152114782,22.0783664200411,
2.15451621446482));
#105452=CARTESIAN_POINT('Ctrl Pts',(-10.9420710812999,22.1575216757129,
2.48033849282147));
#105453=CARTESIAN_POINT('Ctrl Pts',(-11.368282426372,22.2366769313846,3.73454362732737));
#105454=CARTESIAN_POINT('Ctrl Pts',(-10.5486980460349,22.3158321870564,
4.77520114715896));
#105455=CARTESIAN_POINT('Ctrl Pts',(-9.22953429003054,22.3949874427282,
4.65481171678237));
#105456=CARTESIAN_POINT('Ctrl Pts',(-8.61186524708977,22.4741426983999,
3.4829876756009));
#105457=CARTESIAN_POINT('Ctrl Pts',(-9.25806710397417,22.5532979540717,
2.32665303970874));
#105458=CARTESIAN_POINT('Ctrl Pts',(-10.5797850770295,22.6324532097434,
2.23862900937123));
#105459=CARTESIAN_POINT('Ctrl Pts',(-11.3736195102213,22.7116084654152,
3.29905982880227));
#105460=CARTESIAN_POINT('Ctrl Pts',(-10.9167989025253,22.790763721087,4.54244294028871));
#105461=CARTESIAN_POINT('Ctrl Pts',(-9.62524992855897,22.8699189767587,
4.83670112444038));
#105462=CARTESIAN_POINT('Ctrl Pts',(-8.67490393222552,22.9490742324305,
3.91391777108728));
#105463=CARTESIAN_POINT('Ctrl Pts',(-8.93103328280782,23.0282294881023,
2.6142699794191));
#105464=CARTESIAN_POINT('Ctrl Pts',(-10.1604369698711,23.107384743774,2.12106291135225));
#105465=CARTESIAN_POINT('Ctrl Pts',(-11.2437657716457,23.1865399994458,
2.88335244562916));
#105466=CARTESIAN_POINT('Ctrl Pts',(-11.1946689586256,23.2656952551175,
4.20708811094663));
#105467=CARTESIAN_POINT('Ctrl Pts',(-10.0578482372994,23.3448505107893,
4.88703320755515));
#105468=CARTESIAN_POINT('Ctrl Pts',(-8.86835780799071,23.424005766461,4.30411030628588));
#105469=CARTESIAN_POINT('Ctrl Pts',(-8.70920649628835,23.5031610221328,
2.9890599785474));
#105470=CARTESIAN_POINT('Ctrl Pts',(-9.72529882267551,23.5823162778046,
2.1392109193126));
#105471=CARTESIAN_POINT('Ctrl Pts',(-10.9915012041141,23.6614715334763,
2.52833527778638));
#105472=CARTESIAN_POINT('Ctrl Pts',(-11.3549606661359,23.7406267891481,
3.80214184282734));
#105473=CARTESIAN_POINT('Ctrl Pts',(-10.4847526509621,23.8197820448198,
4.80085477316038));
#105474=CARTESIAN_POINT('Ctrl Pts',(-9.17318820920556,23.8989373004917,
4.61516187852302));
#105475=CARTESIAN_POINT('Ctrl Pts',(-8.61441698141044,23.9780925561634,
3.41413812328771));
#105476=CARTESIAN_POINT('Ctrl Pts',(-9.31720017393552,24.0572478118352,
2.29128366298484));
#105477=CARTESIAN_POINT('Ctrl Pts',(-10.6416468237176,24.1364030675069,
2.26895514761134));
#105478=CARTESIAN_POINT('Ctrl Pts',(-11.3819110892539,24.2155583231787,
3.36744673195469));
#105479=CARTESIAN_POINT('Ctrl Pts',(-10.8639227816716,24.2947135788505,
4.58667042735669));
#105480=CARTESIAN_POINT('Ctrl Pts',(-9.55944130977617,24.3738688345222,
4.8164148973843));
#105481=CARTESIAN_POINT('Ctrl Pts',(-8.65590291890877,24.453024090194,3.84775305145438));
#105482=CARTESIAN_POINT('Ctrl Pts',(-8.97648042349053,24.5321793458658,
2.56215183432611));
#105483=CARTESIAN_POINT('Ctrl Pts',(-10.2282993048877,24.6113346015375,
2.13105295154821));
#105484=CARTESIAN_POINT('Ctrl Pts',(-11.2735200365463,24.6904898572092,
2.94517306433958));
#105485=CARTESIAN_POINT('Ctrl Pts',(-11.1567064504975,24.7696514771236,
4.2669496034009));
#105486=CARTESIAN_POINT('Ctrl Pts',(-10.3802617790044,24.8224280118139,
4.67883450561543));
#105487=CARTESIAN_POINT('Ctrl Pts',(-9.99036782849491,24.8488194612803,
4.67563271633731));
#105488=CARTESIAN_POINT('Ctrl Pts',(-10.5513374813396,13.1902385453535,
2.35211365225463));
#105489=CARTESIAN_POINT('Ctrl Pts',(-10.9320512660756,13.2166311989672,
2.5349625684396));
#105490=CARTESIAN_POINT('Ctrl Pts',(-11.4906913536254,13.2694089378048,
3.30587359591926));
#105491=CARTESIAN_POINT('Ctrl Pts',(-10.9738164664813,13.3485717618664,
4.64699941391677));
#105492=CARTESIAN_POINT('Ctrl Pts',(-9.56904991278341,13.4277270175382,
4.94015406912171));
#105493=CARTESIAN_POINT('Ctrl Pts',(-8.55732100450931,13.5068822732099,
3.92382748847622));
#105494=CARTESIAN_POINT('Ctrl Pts',(-8.85877883075876,13.5860375288817,
2.52070958288531));
#105495=CARTESIAN_POINT('Ctrl Pts',(-10.1994773801761,13.6651927845534,
2.00968776902748));
#105496=CARTESIAN_POINT('Ctrl Pts',(-11.3584616418533,13.7443480402252,
2.85532247789389));
#105497=CARTESIAN_POINT('Ctrl Pts',(-11.2806407331068,13.823503295897,4.28805182654041));
#105498=CARTESIAN_POINT('Ctrl Pts',(-10.0367947359074,13.9026585515687,
5.00320804814235));
#105499=CARTESIAN_POINT('Ctrl Pts',(-8.75946110552875,13.9818138072405,
4.34975597894302));
#105500=CARTESIAN_POINT('Ctrl Pts',(-8.61160816070229,14.0609690629123,
2.92259878912427));
#105501=CARTESIAN_POINT('Ctrl Pts',(-9.72786379921332,14.140124318584,2.02116410331367));
#105502=CARTESIAN_POINT('Ctrl Pts',(-11.091892509704,14.2192795742558,2.46617710793435));
#105503=CARTESIAN_POINT('Ctrl Pts',(-11.4617743595397,14.2984348299276,
3.85246920878199));
#105504=CARTESIAN_POINT('Ctrl Pts',(-10.5007373045184,14.3775900855993,
4.91784330858839));
#105505=CARTESIAN_POINT('Ctrl Pts',(-9.08378850443773,14.4567453412711,
4.69229811680502));
#105506=CARTESIAN_POINT('Ctrl Pts',(-8.50103310814551,14.5359005969429,
3.3811872806365));
#105507=CARTESIAN_POINT('Ctrl Pts',(-9.28305928730295,14.6150558526146,
2.17825340697768));
#105508=CARTESIAN_POINT('Ctrl Pts',(-10.7178466262713,14.6942111082864,
2.178745148536));
#105509=CARTESIAN_POINT('Ctrl Pts',(-11.4990479698752,14.7733663639581,
3.382214933763));
#105510=CARTESIAN_POINT('Ctrl Pts',(-10.9153939801766,14.8525216196299,
4.69292580646453));
#105511=CARTESIAN_POINT('Ctrl Pts',(-9.49829078563862,14.9316768753017,
4.9174999118759));
#105512=CARTESIAN_POINT('Ctrl Pts',(-8.5379845058244,15.0108321309734,3.85146667854391));
#105513=CARTESIAN_POINT('Ctrl Pts',(-8.90881616947513,15.0899873866452,
2.4654295687286));
#105514=CARTESIAN_POINT('Ctrl Pts',(-10.2731504349797,15.1691426423169,
2.02134961144923));
#105515=CARTESIAN_POINT('Ctrl Pts',(-11.3887863051869,15.2482978979887,
2.92355335945149));
#105516=CARTESIAN_POINT('Ctrl Pts',(-11.239958049093,15.3274531536604,4.35060106228906));
#105517=CARTESIAN_POINT('Ctrl Pts',(-9.96217102883449,15.4066084093323,
5.00319230305103));
#105518=CARTESIAN_POINT('Ctrl Pts',(-8.71882658387331,15.485763665004,4.28715488227258));
#105519=CARTESIAN_POINT('Ctrl Pts',(-8.64196672908225,15.5649189206758,
2.85442756723797));
#105520=CARTESIAN_POINT('Ctrl Pts',(-9.80157093408568,15.6440741763475,
2.00948195693348));
#105521=CARTESIAN_POINT('Ctrl Pts',(-11.1418411166389,15.7232294320193,
2.52162532982622));
#105522=CARTESIAN_POINT('Ctrl Pts',(-11.4424861788233,15.802384687691,3.92456066090555));
#105523=CARTESIAN_POINT('Ctrl Pts',(-10.4297743777558,15.8815399433628,
4.94094139891786));
#105524=CARTESIAN_POINT('Ctrl Pts',(-9.02576099129743,15.9606951990346,
4.64537176707374));
#105525=CARTESIAN_POINT('Ctrl Pts',(-8.50877412011141,16.0398504547064,
3.306962423248));
#105526=CARTESIAN_POINT('Ctrl Pts',(-9.34952070437594,16.1190057103781,
2.14431020625923));
#105527=CARTESIAN_POINT('Ctrl Pts',(-10.7825166008728,16.1981609660499,
2.21598835665465));
#105528=CARTESIAN_POINT('Ctrl Pts',(-11.5030456720688,16.2773162217216,
3.45673525033684));
#105529=CARTESIAN_POINT('Ctrl Pts',(-10.8550795866552,16.3564714773934,
4.73687389469326));
#105530=CARTESIAN_POINT('Ctrl Pts',(-9.42857942566512,16.4356267330652,
4.89086184005273));
#105531=CARTESIAN_POINT('Ctrl Pts',(-8.52234708014868,16.5147819887369,
3.77849592338659));
#105532=CARTESIAN_POINT('Ctrl Pts',(-8.96149026216576,16.5939372444087,
2.41256464315734));
#105533=CARTESIAN_POINT('Ctrl Pts',(-10.3461772641267,16.6730925000805,
2.03672304990142));
#105534=CARTESIAN_POINT('Ctrl Pts',(-11.415676299355,16.7522477557522,2.99316793083631));
#105535=CARTESIAN_POINT('Ctrl Pts',(-11.1962283684358,16.831403011424,4.41107399339338));
#105536=CARTESIAN_POINT('Ctrl Pts',(-9.88763673495018,16.9105582670957,
4.99946411346035));
#105537=CARTESIAN_POINT('Ctrl Pts',(-8.6813497664918,16.9897135227675,4.22262001948248));
#105538=CARTESIAN_POINT('Ctrl Pts',(-8.67566933405057,17.0688687784393,
2.78784382463254));
#105539=CARTESIAN_POINT('Ctrl Pts',(-9.87576736581714,17.148024034111,2.00147259501467));
#105540=CARTESIAN_POINT('Ctrl Pts',(-11.188976902664,17.2271792897828,2.57948272377994));
#105541=CARTESIAN_POINT('Ctrl Pts',(-11.4196450617917,17.3063345454545,
3.99560672858512));
#105542=CARTESIAN_POINT('Ctrl Pts',(-10.3577527703159,17.3854898011263,
4.960490015789));
#105543=CARTESIAN_POINT('Ctrl Pts',(-8.97013322880461,17.4646450567981,
4.59562428070742));
#105544=CARTESIAN_POINT('Ctrl Pts',(-8.52018824670579,17.5438003124699,
3.23321299563051));
#105545=CARTESIAN_POINT('Ctrl Pts',(-9.41758436987738,17.6229555681416,
2.11370632091287));
#105546=CARTESIAN_POINT('Ctrl Pts',(-10.8452591025203,17.7021108238134,
2.25639428254181));
#105547=CARTESIAN_POINT('Ctrl Pts',(-11.5033411279189,17.7812660794852,
3.5313621427124));
#105548=CARTESIAN_POINT('Ctrl Pts',(-10.7926589896463,17.8604213351569,
4.77777535467742));
#105549=CARTESIAN_POINT('Ctrl Pts',(-9.36027556954837,17.9395765908287,
4.86079784831231));
#105550=CARTESIAN_POINT('Ctrl Pts',(-8.51034935677729,18.0187318465004,
3.70483918578783));
#105551=CARTESIAN_POINT('Ctrl Pts',(-9.01672237574194,18.0978871021722,
2.36237825068194));
#105552=CARTESIAN_POINT('Ctrl Pts',(-10.4183514014968,18.177042357844,2.05570078039427));
#105553=CARTESIAN_POINT('Ctrl Pts',(-11.4390792494977,18.2561976135157,
3.06403091330536));
#105554=CARTESIAN_POINT('Ctrl Pts',(-11.1495521800918,18.3353528691875,
4.46930279899226));
#105555=CARTESIAN_POINT('Ctrl Pts',(-9.81337921032534,18.4145081248593,
4.99204249662981));
#105556=CARTESIAN_POINT('Ctrl Pts',(-8.64712100199181,18.493663380531,4.15630522444703));
#105557=CARTESIAN_POINT('Ctrl Pts',(-8.71263398375444,18.5728186362028,
2.72301424008924));
#105558=CARTESIAN_POINT('Ctrl Pts',(-9.9502698030027,18.6519738918746,1.99715435310386));
#105559=CARTESIAN_POINT('Ctrl Pts',(-11.2331840425896,18.7311291475463,
2.63960750352496));
#105560=CARTESIAN_POINT('Ctrl Pts',(-11.3933071249595,18.8102844032181,
4.06543203519537));
#105561=CARTESIAN_POINT('Ctrl Pts',(-10.2848499588316,18.8894396588898,
4.97644120500673));
#105562=CARTESIAN_POINT('Ctrl Pts',(-8.91704219793103,18.9685949145616,
4.54317809113592));
#105563=CARTESIAN_POINT('Ctrl Pts',(-8.53524739357896,19.0477501702333,
3.16012070838186));
#105564=CARTESIAN_POINT('Ctrl Pts',(-9.48708262108046,19.1269054259051,
2.08651710541289));
#105565=CARTESIAN_POINT('Ctrl Pts',(-10.9059195916668,19.2060606815769,
2.29986341430553));
#105566=CARTESIAN_POINT('Ctrl Pts',(-11.4999336067621,19.2852159372486,
3.60591178496073));
#105567=CARTESIAN_POINT('Ctrl Pts',(-10.7282859428849,19.3643711929204,
4.81552944333614));
#105568=CARTESIAN_POINT('Ctrl Pts',(-9.29354746015517,19.4435264485922,
4.82738198715927));
#105569=CARTESIAN_POINT('Ctrl Pts',(-8.50202088849231,19.5226817042639,
3.63067789550905));
#105570=CARTESIAN_POINT('Ctrl Pts',(-9.07437646418891,19.6018369599357,
2.31499400809925));
#105571=CARTESIAN_POINT('Ctrl Pts',(-10.4894950704046,19.6809922156074,
2.07823605794153));
#105572=CARTESIAN_POINT('Ctrl Pts',(-11.4589375102327,19.7601474712792,
3.13596775949951));
#105573=CARTESIAN_POINT('Ctrl Pts',(-11.1000444552377,19.839302726951,4.52514405201858));
#105574=CARTESIAN_POINT('Ctrl Pts',(-9.7395813634678,19.9184579826227,4.98094573318362));
#105575=CARTESIAN_POINT('Ctrl Pts',(-8.61622460147083,19.9976132382945,
4.08837384145925));
#105576=CARTESIAN_POINT('Ctrl Pts',(-8.75276962816412,20.0767684939663,
2.66009849954996));
#105577=CARTESIAN_POINT('Ctrl Pts',(-10.024894733861,20.155923749638,1.99653786774855));
#105578=CARTESIAN_POINT('Ctrl Pts',(-11.2743536469417,20.2350790053098,
2.70185157181484));
#105579=CARTESIAN_POINT('Ctrl Pts',(-11.3635372430076,20.3142342609816,
4.13386458949784));
#105580=CARTESIAN_POINT('Ctrl Pts',(-10.2112455149443,20.3933895166533,
4.98875567616181));
#105581=CARTESIAN_POINT('Ctrl Pts',(-8.86661867063735,20.4725447723251,
4.4881623819698));
#105582=CARTESIAN_POINT('Ctrl Pts',(-8.55391446756972,20.5517000279969,
3.08786559985373));
#105583=CARTESIAN_POINT('Ctrl Pts',(-9.55784427233645,20.6308552836686,
2.06280953127903));
#105584=CARTESIAN_POINT('Ctrl Pts',(-10.9643486515284,20.7100105393404,
2.34628868030886));
#105585=CARTESIAN_POINT('Ctrl Pts',(-11.4928315018848,20.7891657950121,
3.68020054902433));
#105586=CARTESIAN_POINT('Ctrl Pts',(-10.6621190077965,20.8683210506839,
4.85004316612566));
#105587=CARTESIAN_POINT('Ctrl Pts',(-9.2285594598184,20.9474763063557,4.79069656536787));
#105588=CARTESIAN_POINT('Ctrl Pts',(-8.49738218968395,21.0266315620274,
3.55619472403284));
#105589=CARTESIAN_POINT('Ctrl Pts',(-9.13431051598326,21.1057868176992,
2.27052863060953));
#105590=CARTESIAN_POINT('Ctrl Pts',(-10.5594330322662,21.1849420733709,
2.10427337443985));
#105591=CARTESIAN_POINT('Ctrl Pts',(-11.4752021673908,21.2640973290427,
3.20880127710866));
#105592=CARTESIAN_POINT('Ctrl Pts',(-11.0478271395602,21.3432525847144,
4.57846020626129));
#105593=CARTESIAN_POINT('Ctrl Pts',(-9.66642497063913,21.4224078403863,
4.96620115627938));
#105594=CARTESIAN_POINT('Ctrl Pts',(-8.58873666785621,21.501563096058,4.01899319671312));
#105595=CARTESIAN_POINT('Ctrl Pts',(-8.79597740657156,21.5807183517298,
2.59925157485461));
#105596=CARTESIAN_POINT('Ctrl Pts',(-10.099458344886,21.6598736074015,1.9996246574538));
#105597=CARTESIAN_POINT('Ctrl Pts',(-11.3123843081986,21.7390288630733,
2.76606161124914));
#105598=CARTESIAN_POINT('Ctrl Pts',(-11.3304087440624,21.818184118745,4.20073583083093));
#105599=CARTESIAN_POINT('Ctrl Pts',(-10.1371207385322,21.8973393744168,
4.99740309668184));
#105600=CARTESIAN_POINT('Ctrl Pts',(-8.81898684838297,21.9764946300886,
4.4307126659695));
#105601=CARTESIAN_POINT('Ctrl Pts',(-8.57614348859796,22.0556498857604,
3.01662564628873));
#105602=CARTESIAN_POINT('Ctrl Pts',(-9.62969502603374,22.1348051414321,
2.04264199417463));
#105603=CARTESIAN_POINT('Ctrl Pts',(-11.0204023616999,22.2139603971039,
2.3955557274683));
#105604=CARTESIAN_POINT('Ctrl Pts',(-11.4820523069404,22.2931156527756,
3.75404544943282));
#105605=CARTESIAN_POINT('Ctrl Pts',(-10.5943211644514,22.3722709084474,
4.88123151005539));
#105606=CARTESIAN_POINT('Ctrl Pts',(-9.16547164469076,22.4514261641192,
4.75083194518341));
#105607=CARTESIAN_POINT('Ctrl Pts',(-8.49644468624091,22.5305814197909,
3.48157313568008));
#105608=CARTESIAN_POINT('Ctrl Pts',(-9.19637690365897,22.6097366754627,
2.22909164378287));
#105609=CARTESIAN_POINT('Ctrl Pts',(-10.6279930183855,22.6888919311344,
2.13374859565661));
#105610=CARTESIAN_POINT('Ctrl Pts',(-11.4878331583777,22.7680471868062,
3.28235206523099));
#105611=CARTESIAN_POINT('Ctrl Pts',(-10.9930288530349,22.8472024424779,
4.62911993513292));
#105612=CARTESIAN_POINT('Ctrl Pts',(-9.59409022786481,22.9263576981498,
4.94784508445347));
#105613=CARTESIAN_POINT('Ctrl Pts',(-8.56472490889904,23.0055129538215,
3.94833418576464));
#105614=CARTESIAN_POINT('Ctrl Pts',(-8.84215089025304,23.0846682094933,
2.54062334279264));
#105615=CARTESIAN_POINT('Ctrl Pts',(-10.1737769752306,23.163823465165,2.00640711744365));
#105616=CARTESIAN_POINT('Ctrl Pts',(-11.3471823474695,23.2429787208368,
2.83207946480194));
#105617=CARTESIAN_POINT('Ctrl Pts',(-11.2940032350308,23.3221339765085,
4.2658810387686));
#105618=CARTESIAN_POINT('Ctrl Pts',(-10.0626581997178,23.4012892321803,
5.00236217716447));
#105619=CARTESIAN_POINT('Ctrl Pts',(-8.77426407810743,23.4804444878521,
4.37097043088206));
#105620=CARTESIAN_POINT('Ctrl Pts',(-8.60187966088841,23.5595997435238,
2.94657636252054));
#105621=CARTESIAN_POINT('Ctrl Pts',(-9.70245798255812,23.6387549991956,
2.02606409508629));
#105622=CARTESIAN_POINT('Ctrl Pts',(-11.0739424979592,23.7179102548674,
2.4475433467726));
#105623=CARTESIAN_POINT('Ctrl Pts',(-11.4676228696329,23.7970655105391,
3.82726431806394));
#105624=CARTESIAN_POINT('Ctrl Pts',(-10.5250588407825,23.8762207662109,
4.90901818250252));
#105625=CARTESIAN_POINT('Ctrl Pts',(-9.10444050268076,23.9553760218826,
4.70788530410297));
#105626=CARTESIAN_POINT('Ctrl Pts',(-8.49920859204261,24.0345312775544,
3.40699888414332));
#105627=CARTESIAN_POINT('Ctrl Pts',(-9.26042676724236,24.1136865332262,
2.1907813758452));
#105628=CARTESIAN_POINT('Ctrl Pts',(-10.6949984425754,24.192841788898,2.16659629016257));
#105629=CARTESIAN_POINT('Ctrl Pts',(-11.49681416522,24.2719970445697,3.35642519927706));
#105630=CARTESIAN_POINT('Ctrl Pts',(-10.9357561910591,24.3511523002415,
4.67702484714226));
#105631=CARTESIAN_POINT('Ctrl Pts',(-9.52280975725156,24.4303075559132,
4.92587209917784));
#105632=CARTESIAN_POINT('Ctrl Pts',(-8.54414400025217,24.509462811585,3.87666800524516));
#105633=CARTESIAN_POINT('Ctrl Pts',(-8.89137686757647,24.5886180672568,
2.48417168070902));
#105634=CARTESIAN_POINT('Ctrl Pts',(-10.2472819243751,24.6677733229285,
2.01722780901545));
#105635=CARTESIAN_POINT('Ctrl Pts',(-11.3794106185394,24.7469285786003,
2.89904034130693));
#105636=CARTESIAN_POINT('Ctrl Pts',(-11.2528842221252,24.8260901985145,
4.3307198916829));
#105637=CARTESIAN_POINT('Ctrl Pts',(-10.4118797668908,24.8788667332049,
4.77685217969272));
#105638=CARTESIAN_POINT('Ctrl Pts',(-9.98956693316758,24.9052581826713,
4.77338416819561));
#105639=CARTESIAN_POINT('Ctrl Pts',(-10.5936609534001,13.2466772667445,
2.26399605203392));
#105640=CARTESIAN_POINT('Ctrl Pts',(-11.0036002665585,13.2730699203582,
2.46088138195343));
#105641=CARTESIAN_POINT('Ctrl Pts',(-11.6051244114009,13.3258476591958,
3.29097146479741));
#105642=CARTESIAN_POINT('Ctrl Pts',(-11.0485715763842,13.4050104832573,
4.73504892858119));
#105643=CARTESIAN_POINT('Ctrl Pts',(-9.53596799001725,13.4841657389291,
5.0507076276411));
#105644=CARTESIAN_POINT('Ctrl Pts',(-8.44657361978682,13.5633209946008,
3.95636264430017));
#105645=CARTESIAN_POINT('Ctrl Pts',(-8.77117288357405,13.6424762502726,
2.44553426466258));
#105646=CARTESIAN_POINT('Ctrl Pts',(-10.2147902794661,13.7216315059443,
1.89528381463706));
#105647=CARTESIAN_POINT('Ctrl Pts',(-11.4627440737396,13.8007867616161,
2.80583374908742));
#105648=CARTESIAN_POINT('Ctrl Pts',(-11.3789492358326,13.8799420172879,
4.3485466969086));
#105649=CARTESIAN_POINT('Ctrl Pts',(-10.0396192871665,13.9590972729597,
5.11860195111448));
#105650=CARTESIAN_POINT('Ctrl Pts',(-8.6642310241048,14.0382525286314,4.41498757420045));
#105651=CARTESIAN_POINT('Ctrl Pts',(-8.50502813447824,14.1174077843032,
2.87827453248787));
#105652=CARTESIAN_POINT('Ctrl Pts',(-9.70697323892953,14.1965630399749,
1.90764113077184));
#105653=CARTESIAN_POINT('Ctrl Pts',(-11.1757117378384,14.2757182956467,
2.38681559929634));
#105654=CARTESIAN_POINT('Ctrl Pts',(-11.5739876016257,14.3548735513185,
3.8795265397543));
#105655=CARTESIAN_POINT('Ctrl Pts',(-10.5391764493883,14.4340288069902,
5.02668417953975));
#105656=CARTESIAN_POINT('Ctrl Pts',(-9.01345544538346,14.513184062662,4.78382499052982));
#105657=CARTESIAN_POINT('Ctrl Pts',(-8.3859647779228,14.5923393183338,3.37206661139379));
#105658=CARTESIAN_POINT('Ctrl Pts',(-9.22802326807728,14.6714945740055,
2.07678940916483));
#105659=CARTESIAN_POINT('Ctrl Pts',(-10.7729521880352,14.7506498296773,
2.07731889930876));
#105660=CARTESIAN_POINT('Ctrl Pts',(-11.6141225240595,14.829805085349,3.37317315240631));
#105661=CARTESIAN_POINT('Ctrl Pts',(-10.9856642825877,14.9089603410208,
4.78450086484332));
#105662=CARTESIAN_POINT('Ctrl Pts',(-9.45977703202094,14.9881155966926,
5.02631442194729));
#105663=CARTESIAN_POINT('Ctrl Pts',(-8.42575275301606,15.0672708523643,
3.87844705019104));
#105664=CARTESIAN_POINT('Ctrl Pts',(-8.82505134316252,15.1464261080361,
2.38601067517526));
#105665=CARTESIAN_POINT('Ctrl Pts',(-10.2941188530438,15.2255813637079,
1.90784087945636));
#105666=CARTESIAN_POINT('Ctrl Pts',(-11.495396612621,15.3047366193796,2.87930238049334));
#105667=CARTESIAN_POINT('Ctrl Pts',(-11.3351435418684,15.3838918750514,
4.41589753044666));
#105668=CARTESIAN_POINT('Ctrl Pts',(-9.95926708441137,15.4630471307231,
5.11858499734976));
#105669=CARTESIAN_POINT('Ctrl Pts',(-8.62047718968688,15.5422023863949,
4.34758089863223));
#105670=CARTESIAN_POINT('Ctrl Pts',(-8.53771718112988,15.6213576420667,
2.80487014053335));
#105671=CARTESIAN_POINT('Ctrl Pts',(-9.78633850873561,15.7005128977384,
1.89506220335889));
#105672=CARTESIAN_POINT('Ctrl Pts',(-11.2294946541421,15.7796681534102,
2.44652030900095));
#105673=CARTESIAN_POINT('Ctrl Pts',(-11.5532187619568,15.858823409082,3.95715209877795));
#105674=CARTESIAN_POINT('Ctrl Pts',(-10.462766047078,15.9379786647537,5.05155539688088));
#105675=CARTESIAN_POINT('Ctrl Pts',(-8.95097344490238,16.0171339204255,
4.73329633527975));
#105676=CARTESIAN_POINT('Ctrl Pts',(-8.39430002937858,16.0962891760973,
3.2921438760554));
#105677=CARTESIAN_POINT('Ctrl Pts',(-9.29958660189599,16.175444431769,2.04024055554619));
#105678=CARTESIAN_POINT('Ctrl Pts',(-10.8425865591376,16.2545996874408,
2.1174210856968));
#105679=CARTESIAN_POINT('Ctrl Pts',(-11.6184271102268,16.3337549431125,
3.45341402788135));
#105680=CARTESIAN_POINT('Ctrl Pts',(-10.9207198491445,16.4129101987843,
4.83182263207488));
#105681=CARTESIAN_POINT('Ctrl Pts',(-9.38471427313846,16.4920654544561,
4.99763147611009));
#105682=CARTESIAN_POINT('Ctrl Pts',(-8.40891491893154,16.5712207101278,
3.79987468835603));
#105683=CARTESIAN_POINT('Ctrl Pts',(-8.88176896738465,16.6503759657996,
2.32908756876899));
#105684=CARTESIAN_POINT('Ctrl Pts',(-10.3727515933935,16.7295312214714,
1.92439446131403));
#105685=CARTESIAN_POINT('Ctrl Pts',(-11.5243508196448,16.8086864771431,
2.95426092080234));
#105686=CARTESIAN_POINT('Ctrl Pts',(-11.2880569482855,16.8878417328149,
4.48101267162488));
#105687=CARTESIAN_POINT('Ctrl Pts',(-9.87901115865631,16.9669969884866,
5.11457061294499));
#105688=CARTESIAN_POINT('Ctrl Pts',(-8.5801234609996,17.0461522441584,4.27809201121172));
#105689=CARTESIAN_POINT('Ctrl Pts',(-8.5740069696437,17.1253074998302,2.73317509085155));
#105690=CARTESIAN_POINT('Ctrl Pts',(-9.86623063631879,17.2044627555019,
1.88643800204158));
#105691=CARTESIAN_POINT('Ctrl Pts',(-11.2802488230823,17.2836180111737,
2.5088191310806));
#105692=CARTESIAN_POINT('Ctrl Pts',(-11.528624244492,17.3627732668455,4.03365202432535));
#105693=CARTESIAN_POINT('Ctrl Pts',(-10.3852156943715,17.4419285225172,
5.07260466510981));
#105694=CARTESIAN_POINT('Ctrl Pts',(-8.89107541214616,17.521083778189,4.67972997858343));
#105695=CARTESIAN_POINT('Ctrl Pts',(-8.40659036244245,17.6002390338608,
3.21273306689779));
#105696=CARTESIAN_POINT('Ctrl Pts',(-9.37287518088994,17.6793942895325,
2.00728736014882));
#105697=CARTESIAN_POINT('Ctrl Pts',(-10.9101454946488,17.7585495452043,
2.16092877617142));
#105698=CARTESIAN_POINT('Ctrl Pts',(-11.6187452467723,17.8377048008761,
3.53376966045927));
#105699=CARTESIAN_POINT('Ctrl Pts',(-10.8535075293106,17.9168600565478,
4.87586389636666));
#105700=CARTESIAN_POINT('Ctrl Pts',(-9.31116706527467,17.9960153122196,
4.9652596193006));
#105701=CARTESIAN_POINT('Ctrl Pts',(-8.39599618923083,18.0751705678913,
3.72056368457489));
#105702=CARTESIAN_POINT('Ctrl Pts',(-8.94124097919904,18.1543258235631,
2.27504861329608));
#105703=CARTESIAN_POINT('Ctrl Pts',(-10.4504661850041,18.2334810792348,
1.94482901901976));
#105704=CARTESIAN_POINT('Ctrl Pts',(-11.5495502993905,18.3126363349066,
3.03056370658632));
#105705=CARTESIAN_POINT('Ctrl Pts',(-11.2377976580847,18.3917915905784,
4.54371141679851));
#105706=CARTESIAN_POINT('Ctrl Pts',(-9.79905324837822,18.4709468462501,
5.1065792750213));
#105707=CARTESIAN_POINT('Ctrl Pts',(-8.54326712226964,18.5501021019219,
4.20668655488465));
#105708=CARTESIAN_POINT('Ctrl Pts',(-8.61380921405485,18.6292573575937,
2.66336885733557));
#105709=CARTESIAN_POINT('Ctrl Pts',(-9.94645225989268,18.7084126132654,
1.88178826989647));
#105710=CARTESIAN_POINT('Ctrl Pts',(-11.3278495281379,18.7875678689372,
2.57355939502869));
#105711=CARTESIAN_POINT('Ctrl Pts',(-11.5002644735358,18.866723124609,4.10883747696858));
#105712=CARTESIAN_POINT('Ctrl Pts',(-10.3067164919117,18.9458783802807,
5.08978034882327));
#105713=CARTESIAN_POINT('Ctrl Pts',(-8.83390884344341,19.0250336359525,
4.62325775248417));
#105714=CARTESIAN_POINT('Ctrl Pts',(-8.42280552609934,19.1041888916243,
3.13402984354935));
#105715=CARTESIAN_POINT('Ctrl Pts',(-9.44770847168781,19.183344147296,1.97801096204018));
#105716=CARTESIAN_POINT('Ctrl Pts',(-10.9754625917795,19.2624994029678,
2.20773481980123));
#105717=CARTESIAN_POINT('Ctrl Pts',(-11.6150761469429,19.3416546586395,
3.6140421127969));
#105718=CARTESIAN_POINT('Ctrl Pts',(-10.7841928797412,19.4208099143114,
4.91651618108603));
#105719=CARTESIAN_POINT('Ctrl Pts',(-9.23931656647548,19.4999651699831,
4.92927858651721));
#105720=CARTESIAN_POINT('Ctrl Pts',(-8.38702838531804,19.5791204256548,
3.64070939608118));
#105721=CARTESIAN_POINT('Ctrl Pts',(-9.00332088900616,19.6582756813266,
2.22402691500807));
#105722=CARTESIAN_POINT('Ctrl Pts',(-10.527071204147,19.7374309369984,1.9690942192041));
#105723=CARTESIAN_POINT('Ctrl Pts',(-11.570932981323,19.8165861926701,3.10802279134227));
#105724=CARTESIAN_POINT('Ctrl Pts',(-11.1844894682147,19.8957414483419,
4.60383932870849));
#105725=CARTESIAN_POINT('Ctrl Pts',(-9.71959030307317,19.9748967040136,
5.09463066751667));
#105726=CARTESIAN_POINT('Ctrl Pts',(-8.50999895674359,20.0540519596854,
4.13354041308357));
#105727=CARTESIAN_POINT('Ctrl Pts',(-8.65702587486972,20.1332072153571,
2.59562338423319));
#105728=CARTESIAN_POINT('Ctrl Pts',(-10.0268057803772,20.212362471029,1.88112445998662));
#105729=CARTESIAN_POINT('Ctrl Pts',(-11.3721795209244,20.2915177267007,
2.64058163490015));
#105730=CARTESIAN_POINT('Ctrl Pts',(-11.4682093038797,20.3706729823725,
4.18252326254603));
#105731=CARTESIAN_POINT('Ctrl Pts',(-10.2274617961735,20.4498282380442,
5.10304014148018));
#105732=CARTESIAN_POINT('Ctrl Pts',(-8.77961454947628,20.528983493716,4.56401875738413));
#105733=CARTESIAN_POINT('Ctrl Pts',(-8.44290557972825,20.6081387493877,
3.05622806502234));
#105734=CARTESIAN_POINT('Ctrl Pts',(-9.52390214755894,20.6872940050596,
1.95248347381479));
#105735=CARTESIAN_POINT('Ctrl Pts',(-11.0383769637525,20.7664492607313,
2.25772392558526));
#105736=CARTESIAN_POINT('Ctrl Pts',(-11.6074288483367,20.845604516403,3.69403366061213));
#105737=CARTESIAN_POINT('Ctrl Pts',(-10.7129466338434,20.9247597720748,
4.95367935295463));
#105738=CARTESIAN_POINT('Ctrl Pts',(-9.1693397563632,21.0039150277466,4.88977700497472));
#105739=CARTESIAN_POINT('Ctrl Pts',(-8.38203359637242,21.0830702834183,
3.56050851715058));
#105740=CARTESIAN_POINT('Ctrl Pts',(-9.06785578375502,21.1622255390901,
2.17614814875822));
#105741=CARTESIAN_POINT('Ctrl Pts',(-10.6023779600323,21.2413807947618,
1.99713029267914));
#105742=CARTESIAN_POINT('Ctrl Pts',(-11.5884461963717,21.3205360504337,
3.18644738057619));
#105743=CARTESIAN_POINT('Ctrl Pts',(-11.1282636855349,21.3996913061054,
4.66124830239637));
#105744=CARTESIAN_POINT('Ctrl Pts',(-9.64081805307402,21.4788465617771,
5.07875422182102));
#105745=CARTESIAN_POINT('Ctrl Pts',(-8.480400909397,21.5580018174489,4.05883375681306));
#105746=CARTESIAN_POINT('Ctrl Pts',(-8.70355050232897,21.6371570731207,
2.53010553981177));
#105747=CARTESIAN_POINT('Ctrl Pts',(-10.1070932738061,21.7163123287924,
1.88444820738525));
#105748=CARTESIAN_POINT('Ctrl Pts',(-11.4131296093626,21.7954675844642,
2.70972076387029));
#105749=CARTESIAN_POINT('Ctrl Pts',(-11.4325376926902,21.874622840136,4.25452788082157));
#105750=CARTESIAN_POINT('Ctrl Pts',(-10.1476468245369,21.9537780958077,
5.11235138202542));
#105751=CARTESIAN_POINT('Ctrl Pts',(-8.7283262660405,22.0329333514795,4.50215890869321));
#105752=CARTESIAN_POINT('Ctrl Pts',(-8.46684101358396,22.1120886071513,
2.9795193699218));
#105753=CARTESIAN_POINT('Ctrl Pts',(-9.60126853091967,22.191243862823,1.93076777388446));
#105754=CARTESIAN_POINT('Ctrl Pts',(-11.0987336420998,22.2703991184948,
2.31077296211515));
#105755=CARTESIAN_POINT('Ctrl Pts',(-11.5958221875089,22.3495543741665,
3.77354727153826));
#105756=CARTESIAN_POINT('Ctrl Pts',(-10.6399442828679,22.4287096298383,
4.98726187295182));
#105757=CARTESIAN_POINT('Ctrl Pts',(-9.101408999351,22.5078648855101,4.84685217358446));
#105758=CARTESIAN_POINT('Ctrl Pts',(-8.38102412539203,22.5870201411818,
3.48015859575926));
#105759=CARTESIAN_POINT('Ctrl Pts',(-9.13468670334375,22.6661753968536,
2.131530247857));
#105760=CARTESIAN_POINT('Ctrl Pts',(-10.6762009597416,22.7453306525254,
2.02886818194197));
#105761=CARTESIAN_POINT('Ctrl Pts',(-11.6020468065343,22.8244859081971,
3.2656443016597));
#105762=CARTESIAN_POINT('Ctrl Pts',(-11.0692588035446,22.9036411638689,
4.71579692997711));
#105763=CARTESIAN_POINT('Ctrl Pts',(-9.5629305271706,22.9827964195406,5.05898904446656));
#105764=CARTESIAN_POINT('Ctrl Pts',(-8.4545458855726,23.0619516752124,3.98275060044199));
#105765=CARTESIAN_POINT('Ctrl Pts',(-8.75326849769826,23.1411069308841,
2.4669767061662));
#105766=CARTESIAN_POINT('Ctrl Pts',(-10.1871169805901,23.220262186556,1.89175132353505));
#105767=CARTESIAN_POINT('Ctrl Pts',(-11.4505989232932,23.2994174422277,
2.7808064839747));
#105768=CARTESIAN_POINT('Ctrl Pts',(-11.3933375114359,23.3785726978995,
4.32467396659057));
#105769=CARTESIAN_POINT('Ctrl Pts',(-10.0674681621363,23.4577279535712,
5.1176911467738));
#105770=CARTESIAN_POINT('Ctrl Pts',(-8.68017034822411,23.536883209243,4.43783055547826));
#105771=CARTESIAN_POINT('Ctrl Pts',(-8.49455282548853,23.6160384649147,
2.90409274649368));
#105772=CARTESIAN_POINT('Ctrl Pts',(-9.67961714244069,23.6951937205865,
1.91291727085999));
#105773=CARTESIAN_POINT('Ctrl Pts',(-11.1563837918041,23.7743489762583,
2.36675141575881));
#105774=CARTESIAN_POINT('Ctrl Pts',(-11.5802850731297,23.8535042319301,
3.85238679330052));
#105775=CARTESIAN_POINT('Ctrl Pts',(-10.5653650306028,23.9326594876018,
5.01718159184469));
#105776=CARTESIAN_POINT('Ctrl Pts',(-9.03569279615594,24.0118147432736,
4.80060872968292));
#105777=CARTESIAN_POINT('Ctrl Pts',(-8.38400020267482,24.0909699989453,
3.39985964499894));
#105778=CARTESIAN_POINT('Ctrl Pts',(-9.20365336054916,24.1701252546171,
2.09027908870557));
#105779=CARTESIAN_POINT('Ctrl Pts',(-10.7483500614332,24.2492805102888,
2.06423743271381));
#105780=CARTESIAN_POINT('Ctrl Pts',(-11.6117172411862,24.3284357659606,
3.34540366659943));
#105781=CARTESIAN_POINT('Ctrl Pts',(-11.0075896004464,24.4075910216325,
4.76737926692783));
#105782=CARTESIAN_POINT('Ctrl Pts',(-9.48617820472693,24.4867462773041,
5.03532930097137));
#105783=CARTESIAN_POINT('Ctrl Pts',(-8.43238508159559,24.5659015329759,
3.90558295903594));
#105784=CARTESIAN_POINT('Ctrl Pts',(-8.80627331166242,24.6450567886476,
2.40619152709192));
#105785=CARTESIAN_POINT('Ctrl Pts',(-10.2662645438622,24.7242120443195,
1.90340266648265));
#105786=CARTESIAN_POINT('Ctrl Pts',(-11.4853012005323,24.8033672999912,
2.8529076182743));
#105787=CARTESIAN_POINT('Ctrl Pts',(-11.349061993753,24.8825289199055,4.39449017996491));
#105788=CARTESIAN_POINT('Ctrl Pts',(-10.4434977547771,24.9353054545958,
4.87486985377003));
#105789=CARTESIAN_POINT('Ctrl Pts',(-9.98876603784026,24.9616969040622,
4.87113562005391));
#105790=CARTESIAN_POINT('Ctrl Pts',(-10.6359844254605,13.3031159881355,
2.17587845181322));
#105791=CARTESIAN_POINT('Ctrl Pts',(-11.0751492670415,13.3295086417492,
2.38680019546726));
#105792=CARTESIAN_POINT('Ctrl Pts',(-11.7195574691764,13.3822863805868,
3.27606933367556));
#105793=CARTESIAN_POINT('Ctrl Pts',(-11.1233266862871,13.4614492046484,
4.82309844324562));
#105794=CARTESIAN_POINT('Ctrl Pts',(-9.50288606725111,13.5406044603201,
5.16126118616049));
#105795=CARTESIAN_POINT('Ctrl Pts',(-8.33582623506433,13.6197597159919,
3.98889780012413));
#105796=CARTESIAN_POINT('Ctrl Pts',(-8.68356693638938,13.6989149716636,
2.37035894643987));
#105797=CARTESIAN_POINT('Ctrl Pts',(-10.2301031787562,13.7780702273355,
1.78087986024663));
#105798=CARTESIAN_POINT('Ctrl Pts',(-11.5670265056259,13.8572254830071,
2.75634502028094));
#105799=CARTESIAN_POINT('Ctrl Pts',(-11.4772577385584,13.9363807386789,
4.40904156727679));
#105800=CARTESIAN_POINT('Ctrl Pts',(-10.0424438384259,14.0155359943506,
5.2339958540866));
#105801=CARTESIAN_POINT('Ctrl Pts',(-8.56900094268083,14.0946912500225,
4.48021916945787));
#105802=CARTESIAN_POINT('Ctrl Pts',(-8.3984481082542,14.1738465056942,2.83395027585145));
#105803=CARTESIAN_POINT('Ctrl Pts',(-9.68608267864575,14.2530017613659,
1.79411815823003));
#105804=CARTESIAN_POINT('Ctrl Pts',(-11.2595309659728,14.3321570170378,
2.30745409065834));
#105805=CARTESIAN_POINT('Ctrl Pts',(-11.6862008437117,14.4113122727095,
3.90658387072663));
#105806=CARTESIAN_POINT('Ctrl Pts',(-10.5776155942583,14.4904675283814,
5.13552505049112));
#105807=CARTESIAN_POINT('Ctrl Pts',(-8.94312238632918,14.5696227840531,
4.87535186425462));
#105808=CARTESIAN_POINT('Ctrl Pts',(-8.27089644770011,14.6487780397248,
3.36294594215109));
#105809=CARTESIAN_POINT('Ctrl Pts',(-9.1729872488516,14.7279332953965,1.97532541135201));
#105810=CARTESIAN_POINT('Ctrl Pts',(-10.828057749799,14.8070885510684,1.97589265008151));
#105811=CARTESIAN_POINT('Ctrl Pts',(-11.7291970782439,14.8862438067401,
3.36413137104963));
#105812=CARTESIAN_POINT('Ctrl Pts',(-11.0559345849988,14.9653990624118,
4.87607592322209));
#105813=CARTESIAN_POINT('Ctrl Pts',(-9.42126327840329,15.0445543180837,
5.1351289320187));
#105814=CARTESIAN_POINT('Ctrl Pts',(-8.31352100020771,15.1237095737555,
3.90542742183816));
#105815=CARTESIAN_POINT('Ctrl Pts',(-8.74128651684992,15.2028648294271,
2.30659178162193));
#105816=CARTESIAN_POINT('Ctrl Pts',(-10.3150872711079,15.2820200850989,
1.79433214746349));
#105817=CARTESIAN_POINT('Ctrl Pts',(-11.602006920055,15.3611753407707,2.83505140153521));
#105818=CARTESIAN_POINT('Ctrl Pts',(-11.4303290346439,15.4403305964424,
4.48119399860425));
#105819=CARTESIAN_POINT('Ctrl Pts',(-9.95636313998825,15.5194858521142,
5.2339776916485));
#105820=CARTESIAN_POINT('Ctrl Pts',(-8.52212779550044,15.5986411077859,
4.40800691499187));
#105821=CARTESIAN_POINT('Ctrl Pts',(-8.43346763317752,15.6777963634578,
2.75531271382871));
#105822=CARTESIAN_POINT('Ctrl Pts',(-9.77110608338552,15.7569516191295,
1.78064244978428));
#105823=CARTESIAN_POINT('Ctrl Pts',(-11.3171481916453,15.8361068748012,
2.3714152881757));
#105824=CARTESIAN_POINT('Ctrl Pts',(-11.6639513450902,15.9152621304731,
3.98974353665035));
#105825=CARTESIAN_POINT('Ctrl Pts',(-10.4957577164001,15.9944173861447,
5.16216939484391));
#105826=CARTESIAN_POINT('Ctrl Pts',(-8.87618589850731,16.0735726418165,
4.82122090348578));
#105827=CARTESIAN_POINT('Ctrl Pts',(-8.27982593864574,16.1527278974884,
3.27732532886281));
#105828=CARTESIAN_POINT('Ctrl Pts',(-9.24965249941607,16.2318831531601,
1.93617090483314));
#105829=CARTESIAN_POINT('Ctrl Pts',(-10.9026565174023,16.3110384088318,
2.01885381473895));
#105830=CARTESIAN_POINT('Ctrl Pts',(-11.7338085483849,16.3901936645035,
3.45009280542587));
#105831=CARTESIAN_POINT('Ctrl Pts',(-10.9863601116336,16.4693489201754,
4.92677136945647));
#105832=CARTESIAN_POINT('Ctrl Pts',(-9.3408491206118,16.5485041758471,5.10440111216747));
#105833=CARTESIAN_POINT('Ctrl Pts',(-8.2954827577144,16.6276594315189,3.82125345332548));
#105834=CARTESIAN_POINT('Ctrl Pts',(-8.80204767260358,16.7068146871907,
2.24561049438064));
#105835=CARTESIAN_POINT('Ctrl Pts',(-10.3993259226603,16.7859699428624,
1.81206587272666));
#105836=CARTESIAN_POINT('Ctrl Pts',(-11.6330253399346,16.8651251985341,
2.91535391076835));
#105837=CARTESIAN_POINT('Ctrl Pts',(-11.3798855281354,16.944280454206,4.55095134985639));
#105838=CARTESIAN_POINT('Ctrl Pts',(-9.87038558236248,17.0234357098778,
5.22967711242965));
#105839=CARTESIAN_POINT('Ctrl Pts',(-8.47889715550738,17.1025909655494,
4.33356400294095));
#105840=CARTESIAN_POINT('Ctrl Pts',(-8.47234460523684,17.1817462212212,
2.67850635707057));
#105841=CARTESIAN_POINT('Ctrl Pts',(-9.85669390682044,17.2609014768931,
1.77140340906848));
#105842=CARTESIAN_POINT('Ctrl Pts',(-11.3715207435005,17.3400567325647,
2.43815553838126));
#105843=CARTESIAN_POINT('Ctrl Pts',(-11.6376034271924,17.4192119882365,
4.07169732006558));
#105844=CARTESIAN_POINT('Ctrl Pts',(-10.4126786184271,17.4983672439082,
5.18471931443062));
#105845=CARTESIAN_POINT('Ctrl Pts',(-8.81201759548772,17.5775224995801,
4.76383567645944));
#105846=CARTESIAN_POINT('Ctrl Pts',(-8.29299247817908,17.6566777552518,
3.19225313816505));
#105847=CARTESIAN_POINT('Ctrl Pts',(-9.32816599190252,17.7358330109235,
1.90086839938479));
#105848=CARTESIAN_POINT('Ctrl Pts',(-10.9750318867773,17.8149882665954,
2.06546326980104));
#105849=CARTESIAN_POINT('Ctrl Pts',(-11.7341493656255,17.8941435222671,
3.53617717820614));
#105850=CARTESIAN_POINT('Ctrl Pts',(-10.9143560689751,17.9732987779388,
4.97395243805591));
#105851=CARTESIAN_POINT('Ctrl Pts',(-9.26205856100099,18.0524540336107,
5.06972139028892));
#105852=CARTESIAN_POINT('Ctrl Pts',(-8.28164302168439,18.1316092892824,
3.73628818336193));
#105853=CARTESIAN_POINT('Ctrl Pts',(-8.86575958265614,18.2107645449541,
2.18771897591022));
#105854=CARTESIAN_POINT('Ctrl Pts',(-10.4825809685115,18.289919800626,1.83395725764526));
#105855=CARTESIAN_POINT('Ctrl Pts',(-11.6600213492834,18.3690750562978,
2.99709649986729));
#105856=CARTESIAN_POINT('Ctrl Pts',(-11.3260431360774,18.4482303119694,
4.61812003460476));
#105857=CARTESIAN_POINT('Ctrl Pts',(-9.7847272864311,18.5273855676412,5.22111605341277));
#105858=CARTESIAN_POINT('Ctrl Pts',(-8.43941324254747,18.6065408233129,
4.25706788532226));
#105859=CARTESIAN_POINT('Ctrl Pts',(-8.51498444435524,18.6856960789847,
2.60372347458188));
#105860=CARTESIAN_POINT('Ctrl Pts',(-9.94263471678268,18.7648513346564,
1.76642218668908));
#105861=CARTESIAN_POINT('Ctrl Pts',(-11.4225150136859,18.8440065903283,
2.50751128653242));
#105862=CARTESIAN_POINT('Ctrl Pts',(-11.6072218221122,18.9231618460001,
4.1522429187418));
#105863=CARTESIAN_POINT('Ctrl Pts',(-10.3285830249918,19.0023171016717,
5.20311949263982));
#105864=CARTESIAN_POINT('Ctrl Pts',(-8.75077548895581,19.0814723573435,
4.70333741383239));
#105865=CARTESIAN_POINT('Ctrl Pts',(-8.31036365861973,19.1606276130152,
3.10793897871686));
#105866=CARTESIAN_POINT('Ctrl Pts',(-9.40833432229519,19.2397828686871,
1.86950481866748));
#105867=CARTESIAN_POINT('Ctrl Pts',(-11.045005591892,19.3189381243588,2.11560622529692));
#105868=CARTESIAN_POINT('Ctrl Pts',(-11.7302186871239,19.3980933800307,
3.62217244063306));
#105869=CARTESIAN_POINT('Ctrl Pts',(-10.8400998165974,19.4772486357024,
5.01750291883593));
#105870=CARTESIAN_POINT('Ctrl Pts',(-9.18508567279581,19.5564038913741,
5.03117518587516));
#105871=CARTESIAN_POINT('Ctrl Pts',(-8.27203588214378,19.6355591470458,
3.65074089665331));
#105872=CARTESIAN_POINT('Ctrl Pts',(-8.93226531382342,19.7147144027176,
2.1330598219169));
#105873=CARTESIAN_POINT('Ctrl Pts',(-10.5646473378894,19.7938696583894,
1.85995238046668));
#105874=CARTESIAN_POINT('Ctrl Pts',(-11.682928452413,19.8730249140611,3.08007782318505));
#105875=CARTESIAN_POINT('Ctrl Pts',(-11.2689344811918,19.9521801697329,
4.6825346053984));
#105876=CARTESIAN_POINT('Ctrl Pts',(-9.6995992426785,20.0313354254047,5.20831560184972));
#105877=CARTESIAN_POINT('Ctrl Pts',(-8.40377331201639,20.1104906810765,
4.1787069847079));
#105878=CARTESIAN_POINT('Ctrl Pts',(-8.56128212157532,20.1896459367483,
2.53114826891643));
#105879=CARTESIAN_POINT('Ctrl Pts',(-10.0287168268935,20.2688011924199,
1.76571105222467));
#105880=CARTESIAN_POINT('Ctrl Pts',(-11.4700053949071,20.3479564480918,
2.57931169798544));
#105881=CARTESIAN_POINT('Ctrl Pts',(-11.5728813647517,20.4271117037635,
4.23118193559423));
#105882=CARTESIAN_POINT('Ctrl Pts',(-10.2436780774028,20.5062669594352,
5.21732460679853));
#105883=CARTESIAN_POINT('Ctrl Pts',(-8.6926104283152,20.5854222151071,4.63987513279845));
#105884=CARTESIAN_POINT('Ctrl Pts',(-8.33189669188675,20.6645774707789,
3.02459053019094));
#105885=CARTESIAN_POINT('Ctrl Pts',(-9.48996002278146,20.7437327264505,
1.84215741635058));
#105886=CARTESIAN_POINT('Ctrl Pts',(-11.1124052759767,20.8228879821223,
2.16915917086166));
#105887=CARTESIAN_POINT('Ctrl Pts',(-11.7220261947885,20.9020432377942,
3.70786677219993));
#105888=CARTESIAN_POINT('Ctrl Pts',(-10.7637742598904,20.9811984934658,
5.05731553978359));
#105889=CARTESIAN_POINT('Ctrl Pts',(-9.11012005290798,21.0603537491376,
4.98885744458157));
#105890=CARTESIAN_POINT('Ctrl Pts',(-8.26668500306089,21.1395090048093,
3.5648223102683));
#105891=CARTESIAN_POINT('Ctrl Pts',(-9.00140105152678,21.2186642604812,
2.08176766690691));
#105892=CARTESIAN_POINT('Ctrl Pts',(-10.6453228877982,21.2978195161528,
1.88998721091841));
#105893=CARTESIAN_POINT('Ctrl Pts',(-11.7016902253526,21.3769747718248,
3.16409348404373));
#105894=CARTESIAN_POINT('Ctrl Pts',(-11.2087002315096,21.4561300274965,
4.74403639853141));
#105895=CARTESIAN_POINT('Ctrl Pts',(-9.61521113550892,21.5352852831683,
5.19130728736269));
#105896=CARTESIAN_POINT('Ctrl Pts',(-8.37206515093778,21.6144405388399,
4.09867431691298));
#105897=CARTESIAN_POINT('Ctrl Pts',(-8.6111235980864,21.6935957945117,2.46095950476894));
#105898=CARTESIAN_POINT('Ctrl Pts',(-10.114728202726,21.7727510501836,1.76927175731667));
#105899=CARTESIAN_POINT('Ctrl Pts',(-11.5138749105269,21.8519063058552,
2.65337991649145));
#105900=CARTESIAN_POINT('Ctrl Pts',(-11.534666641318,21.9310615615271,4.3083199308122));
#105901=CARTESIAN_POINT('Ctrl Pts',(-10.1581729105416,22.0102168171988,
5.227299667369));
#105902=CARTESIAN_POINT('Ctrl Pts',(-8.63766568369801,22.0893720728705,
4.57360515141694));
#105903=CARTESIAN_POINT('Ctrl Pts',(-8.35753853856994,22.1685273285423,
2.94241309355486));
#105904=CARTESIAN_POINT('Ctrl Pts',(-9.57284203580558,22.2476825842141,
1.81889355359428));
#105905=CARTESIAN_POINT('Ctrl Pts',(-11.1770649224999,22.3268378398858,
2.22599019676199));
#105906=CARTESIAN_POINT('Ctrl Pts',(-11.7095920680774,22.4059930955575,
3.79304909364371));
#105907=CARTESIAN_POINT('Ctrl Pts',(-10.6855674012843,22.4851483512294,
5.09329223584824));
#105908=CARTESIAN_POINT('Ctrl Pts',(-9.03734635401123,22.5643036069012,
4.94287240198551));
#105909=CARTESIAN_POINT('Ctrl Pts',(-8.26560356454317,22.6434588625728,
3.47874405583843));
#105910=CARTESIAN_POINT('Ctrl Pts',(-9.07299650302853,22.7226141182447,
2.03396885193113));
#105911=CARTESIAN_POINT('Ctrl Pts',(-10.7244089010975,22.8017693739163,
1.92398776822735));
#105912=CARTESIAN_POINT('Ctrl Pts',(-11.7162604546908,22.8809246295881,
3.2489365380884));
#105913=CARTESIAN_POINT('Ctrl Pts',(-11.1454887540544,22.9600798852599,
4.80247392482133));
#105914=CARTESIAN_POINT('Ctrl Pts',(-9.53177082647642,23.0392351409316,
5.17013300447963));
#105915=CARTESIAN_POINT('Ctrl Pts',(-8.34436686224613,23.1183903966035,
4.01716701511935));
#105916=CARTESIAN_POINT('Ctrl Pts',(-8.66438610514347,23.1975456522753,
2.39333006953975));
#105917=CARTESIAN_POINT('Ctrl Pts',(-10.2004569859495,23.2767009079471,
1.77709552962646));
#105918=CARTESIAN_POINT('Ctrl Pts',(-11.5540154991171,23.3558561636188,
2.72953350314748));
#105919=CARTESIAN_POINT('Ctrl Pts',(-11.4926717878413,23.4350114192905,
4.38346689441255));
#105920=CARTESIAN_POINT('Ctrl Pts',(-10.0722781245547,23.5141666749622,
5.23302011638312));
#105921=CARTESIAN_POINT('Ctrl Pts',(-8.58607661834083,23.5933219306341,
4.50469068007444));
#105922=CARTESIAN_POINT('Ctrl Pts',(-8.3872259900886,23.6724771863059,2.8616091304668));
#105923=CARTESIAN_POINT('Ctrl Pts',(-9.6567763023233,23.7516324419776,1.79977044663367));
#105924=CARTESIAN_POINT('Ctrl Pts',(-11.2388250856492,23.8307876976494,
2.28595948474501));
#105925=CARTESIAN_POINT('Ctrl Pts',(-11.6929472766268,23.9099429533211,
3.87750926853712));
#105926=CARTESIAN_POINT('Ctrl Pts',(-10.6056712204232,23.9890982089928,
5.12534500118684));
#105927=CARTESIAN_POINT('Ctrl Pts',(-8.96694508963116,24.0682534646645,
4.89333215526286));
#105928=CARTESIAN_POINT('Ctrl Pts',(-8.26879181330697,24.1474087203365,
3.39272040585454));
#105929=CARTESIAN_POINT('Ctrl Pts',(-9.14687995385603,24.2265639760081,
1.98977680156594));
#105930=CARTESIAN_POINT('Ctrl Pts',(-10.8017016802907,24.30571923168,1.96187857526504));
#105931=CARTESIAN_POINT('Ctrl Pts',(-11.7266203171524,24.3848744873517,
3.33438213392181));
#105932=CARTESIAN_POINT('Ctrl Pts',(-11.0794230098339,24.4640297430234,
4.8577336867134));
#105933=CARTESIAN_POINT('Ctrl Pts',(-9.44954665220232,24.5431849986951,
5.1447865027649));
#105934=CARTESIAN_POINT('Ctrl Pts',(-8.320626162939,24.6223402543669,3.93449791282671));
#105935=CARTESIAN_POINT('Ctrl Pts',(-8.72116975574837,24.7014955100387,
2.32821137347482));
#105936=CARTESIAN_POINT('Ctrl Pts',(-10.2852471633496,24.7806507657105,
1.78957752394988));
#105937=CARTESIAN_POINT('Ctrl Pts',(-11.5911917825255,24.8598060213822,
2.80677489524165));
#105938=CARTESIAN_POINT('Ctrl Pts',(-11.4452397653807,24.9389676412965,
4.45826046824691));
#105939=CARTESIAN_POINT('Ctrl Pts',(-10.4751157426634,24.9917441759868,
4.97288752784733));
#105940=CARTESIAN_POINT('Ctrl Pts',(-9.98796514251294,25.0181356254532,
4.96888707191221));
#105941=CARTESIAN_POINT('Ctrl Pts',(-11.2893010323265,24.8491715501582,
2.80576613662465));
#105942=CARTESIAN_POINT('Ctrl Pts',(-11.2911828539987,24.8493085424027,
2.80954992823753));
#105943=CARTESIAN_POINT('Ctrl Pts',(-11.2930478994451,24.8494459706458,
2.8133420285908));
#105944=CARTESIAN_POINT('Ctrl Pts',(-11.2967488969198,24.8497221006906,
2.82095216262323));
#105945=CARTESIAN_POINT('Ctrl Pts',(-11.2985847475564,24.8498608035729,
2.82477020296673));
#105946=CARTESIAN_POINT('Ctrl Pts',(-11.3004035488554,24.85,2.82859635082591));
#105947=CARTESIAN_POINT('Ctrl Pts',(-10.6340070945752,13.3,2.18095972236309));
#105948=CARTESIAN_POINT('Ctrl Pts',(-10.7649118977414,13.3,2.2597766501823));
#105949=CARTESIAN_POINT('Ctrl Pts',(-10.8821009016869,13.3,2.36060058848546));
#105950=CARTESIAN_POINT('Ctrl Pts',(-11.0770809467795,13.3,2.58998815869127));
#105951=CARTESIAN_POINT('Ctrl Pts',(-11.1560983945165,13.3,2.71786393184818));
#105952=CARTESIAN_POINT('Ctrl Pts',(-11.2754706506363,13.3,3.00226080557722));
#105953=CARTESIAN_POINT('Ctrl Pts',(-11.3122290867249,13.3,3.16041690251937));
#105954=CARTESIAN_POINT('Ctrl Pts',(-11.3221189530405,13.3,3.47550855713216));
#105955=CARTESIAN_POINT('Ctrl Pts',(-11.2969289416632,13.3,3.63084327221525));
#105956=CARTESIAN_POINT('Ctrl Pts',(-11.1953388723352,13.3,3.92477402681276));
#105957=CARTESIAN_POINT('Ctrl Pts',(-11.1178102771856,13.3,4.06435062655608));
#105958=CARTESIAN_POINT('Ctrl Pts',(-10.9298861008457,13.3,4.29041448834001));
#105959=CARTESIAN_POINT('Ctrl Pts',(-10.817769113814,13.3,4.39034265231198));
#105960=CARTESIAN_POINT('Ctrl Pts',(-10.6730394577712,13.3,4.46649518921549));
#105961=CARTESIAN_POINT('Origin',(-10.,13.3,3.5));
#105962=CARTESIAN_POINT('',(-9.34259215682144,13.3,2.1924652288649));
#105963=CARTESIAN_POINT('',(-10.,13.3,4.9635));
#105964=CARTESIAN_POINT('Origin',(-10.,13.3,3.5));
#105965=CARTESIAN_POINT('Ctrl Pts',(-9.34259215682146,13.3,2.19246522886492));
#105966=CARTESIAN_POINT('Ctrl Pts',(-9.31521779133866,13.3,2.20945799843699));
#105967=CARTESIAN_POINT('Ctrl Pts',(-9.28848021785727,13.3,2.22740026541353));
#105968=CARTESIAN_POINT('Ctrl Pts',(-9.26243629817129,13.3,2.24629525384867));
#105969=CARTESIAN_POINT('Ctrl Pts',(-9.21594140958665,13.3,2.28002751814271));
#105970=CARTESIAN_POINT('Ctrl Pts',(-9.17165482603987,13.3,2.31679483974346));
#105971=CARTESIAN_POINT('Ctrl Pts',(-9.12972630031258,13.3,2.35628918066472));
#105972=CARTESIAN_POINT('Ctrl Pts',(-9.11328522426273,13.3,2.37177576053754));
#105973=CARTESIAN_POINT('Ctrl Pts',(-9.0972077460164,13.3,2.38768135360173));
#105974=CARTESIAN_POINT('Ctrl Pts',(-9.08150295565413,13.3,2.40399019950359));
#105975=CARTESIAN_POINT('Ctrl Pts',(-9.06902583680322,13.3,2.41694722751508));
#105976=CARTESIAN_POINT('Ctrl Pts',(-9.05678329388114,13.3,2.43016012005021));
#105977=CARTESIAN_POINT('Ctrl Pts',(-9.04480148606494,13.3,2.44359617390108));
#105978=CARTESIAN_POINT('Ctrl Pts',(-9.00650633540295,13.3,2.48653925180841));
#105979=CARTESIAN_POINT('Ctrl Pts',(-8.97082703665313,13.3,2.53180331423269));
#105980=CARTESIAN_POINT('Ctrl Pts',(-8.93791405473512,13.3,2.57907594938494));
#105981=CARTESIAN_POINT('Ctrl Pts',(-8.90697991548926,13.3,2.62350638968843));
#105982=CARTESIAN_POINT('Ctrl Pts',(-8.87848954676292,13.3,2.66971220198839));
#105983=CARTESIAN_POINT('Ctrl Pts',(-8.8526081156124,13.3,2.71744597458528));
#105984=CARTESIAN_POINT('Ctrl Pts',(-8.84707051117102,13.3,2.72765911734387));
#105985=CARTESIAN_POINT('Ctrl Pts',(-8.8416520475112,13.3,2.73794333779959));
#105986=CARTESIAN_POINT('Ctrl Pts',(-8.83636226986782,13.3,2.74828049613421));
#105987=CARTESIAN_POINT('Ctrl Pts',(-8.81074658205689,13.3,2.79833806728434));
#105988=CARTESIAN_POINT('Ctrl Pts',(-8.78809853079567,13.3,2.84971852311362));
#105989=CARTESIAN_POINT('Ctrl Pts',(-8.76856023990328,13.3,2.90213268419753));
#105990=CARTESIAN_POINT('Ctrl Pts',(-8.74946444936866,13.3,2.95335977701847));
#105991=CARTESIAN_POINT('Ctrl Pts',(-8.73333901424337,13.3,3.00557532995757));
#105992=CARTESIAN_POINT('Ctrl Pts',(-8.72036517763863,13.3,3.05851505090622));
#105993=CARTESIAN_POINT('Ctrl Pts',(-8.71286934006812,13.3,3.08910180495198));
#105994=CARTESIAN_POINT('Ctrl Pts',(-8.70642646300776,13.3,3.11993031884901));
#105995=CARTESIAN_POINT('Ctrl Pts',(-8.70107944044095,13.3,3.15094851201392));
#105996=CARTESIAN_POINT('Ctrl Pts',(-8.6978504963647,13.3,3.16967968619995));
#105997=CARTESIAN_POINT('Ctrl Pts',(-8.69502128966433,13.3,3.18848000645603));
#105998=CARTESIAN_POINT('Ctrl Pts',(-8.69260235178538,13.3,3.20733768073485));
#105999=CARTESIAN_POINT('Ctrl Pts',(-8.69053148333976,13.3,3.22348185829385));
#106000=CARTESIAN_POINT('Ctrl Pts',(-8.68876097039777,13.3,3.23967513535794));
#106001=CARTESIAN_POINT('Ctrl Pts',(-8.68730098700498,13.3,3.25586630701112));
#106002=CARTESIAN_POINT('Ctrl Pts',(-8.68271778980999,13.3,3.30669382523563));
#106003=CARTESIAN_POINT('Ctrl Pts',(-8.68117918886184,13.3,3.3575752015979));
#106004=CARTESIAN_POINT('Ctrl Pts',(-8.68282898128772,13.3,3.40828825099132));
#106005=CARTESIAN_POINT('Ctrl Pts',(-8.68319575405777,13.3,3.41956249695818));
#106006=CARTESIAN_POINT('Ctrl Pts',(-8.68372028641139,13.3,3.43082840054581));
#106007=CARTESIAN_POINT('Ctrl Pts',(-8.68440446650174,13.3,3.44208346590591));
#106008=CARTESIAN_POINT('Ctrl Pts',(-8.68766251977198,13.3,3.49567988448072));
#106009=CARTESIAN_POINT('Ctrl Pts',(-8.69453705507356,13.3,3.54903238816311));
#106010=CARTESIAN_POINT('Ctrl Pts',(-8.70486643643529,13.3,3.60185630631317));
#106011=CARTESIAN_POINT('Ctrl Pts',(-8.70971531879739,13.3,3.62665323809881));
#106012=CARTESIAN_POINT('Ctrl Pts',(-8.71532619270893,13.3,3.65133335363798));
#106013=CARTESIAN_POINT('Ctrl Pts',(-8.72168558588098,13.3,3.67586495389262));
#106014=CARTESIAN_POINT('Ctrl Pts',(-8.72619429323909,13.3,3.69325746345788));
#106015=CARTESIAN_POINT('Ctrl Pts',(-8.73107929177658,13.3,3.71057528883275));
#106016=CARTESIAN_POINT('Ctrl Pts',(-8.73633631363297,13.3,3.72780656509595));
#106017=CARTESIAN_POINT('Ctrl Pts',(-8.73933492736524,13.3,3.73763531282399));
#106018=CARTESIAN_POINT('Ctrl Pts',(-8.74245220717161,13.3,3.74742793277564));
#106019=CARTESIAN_POINT('Ctrl Pts',(-8.74568498220576,13.3,3.75717712187213));
#106020=CARTESIAN_POINT('Ctrl Pts',(-8.76222845779434,13.3,3.80706784118373));
#106021=CARTESIAN_POINT('Ctrl Pts',(-8.78180660508961,13.3,3.85586874502093));
#106022=CARTESIAN_POINT('Ctrl Pts',(-8.80424653825476,13.3,3.90332080785399));
#106023=CARTESIAN_POINT('Ctrl Pts',(-8.82645061601556,13.3,3.95027412475122));
#106024=CARTESIAN_POINT('Ctrl Pts',(-8.85145745690028,13.3,3.99590765632431));
#106025=CARTESIAN_POINT('Ctrl Pts',(-8.8791380940311,13.3,4.03993822048699));
#106026=CARTESIAN_POINT('Ctrl Pts',(-8.89317285365425,13.3,4.06226279275655));
#106027=CARTESIAN_POINT('Ctrl Pts',(-8.90789551638605,13.3,4.08417468939178));
#106028=CARTESIAN_POINT('Ctrl Pts',(-8.92329211937121,13.3,4.10563273885798));
#106029=CARTESIAN_POINT('Ctrl Pts',(-8.93455023908675,13.3,4.12132303690524));
#106030=CARTESIAN_POINT('Ctrl Pts',(-8.94616873015292,13.3,4.13677061829437));
#106031=CARTESIAN_POINT('Ctrl Pts',(-8.95814263522597,13.3,4.15195823856277));
#106032=CARTESIAN_POINT('Ctrl Pts',(-8.9639302347199,13.3,4.15929919064508));
#106033=CARTESIAN_POINT('Ctrl Pts',(-8.96980032039377,13.3,4.16657853776216));
#106034=CARTESIAN_POINT('Ctrl Pts',(-8.97574395339132,13.3,4.17378460022058));
#106035=CARTESIAN_POINT('Ctrl Pts',(-9.00783287843214,13.3,4.2126892227238));
#106036=CARTESIAN_POINT('Ctrl Pts',(-9.04212471772084,13.3,4.24954017180012));
#106037=CARTESIAN_POINT('Ctrl Pts',(-9.07848924761864,13.3,4.28408550552319));
#106038=CARTESIAN_POINT('Ctrl Pts',(-9.11411291247182,13.3,4.31792703720943));
#106039=CARTESIAN_POINT('Ctrl Pts',(-9.15172641996041,13.3,4.34955652077773));
#106040=CARTESIAN_POINT('Ctrl Pts',(-9.19123107437835,13.3,4.37869353424287));
#106041=CARTESIAN_POINT('Ctrl Pts',(-9.23073572879629,13.3,4.407830547708));
#106042=CARTESIAN_POINT('Ctrl Pts',(-9.27213215627179,13.3,4.43447577192636));
#106043=CARTESIAN_POINT('Ctrl Pts',(-9.31533557546055,13.3,4.45829519891842));
#106044=CARTESIAN_POINT('Origin',(-10.,13.3,3.5));
#106045=CARTESIAN_POINT('Ctrl Pts',(-9.14640484551624,13.1319226084129,
4.69534642251162));
#106046=CARTESIAN_POINT('Ctrl Pts',(-8.74996755407482,13.158314057538,4.41226235778059));
#106047=CARTESIAN_POINT('Ctrl Pts',(-8.26764348151547,13.2110905918871,
3.4257644765553));
#106048=CARTESIAN_POINT('Ctrl Pts',(-9.12022709537494,13.2902522114602,
2.00399222931921));
#106049=CARTESIAN_POINT('Ctrl Pts',(-10.7745379170022,13.3694074671319,
1.94868204332565));
#106050=CARTESIAN_POINT('Ctrl Pts',(-11.723237150978,13.4485627228037,3.30369389649766));
#106051=CARTESIAN_POINT('Ctrl Pts',(-11.1031746725215,13.5277179784755,
4.8385355444873));
#106052=CARTESIAN_POINT('Ctrl Pts',(-9.47858070734822,13.6068732341472,
5.1540948536134));
#106053=CARTESIAN_POINT('Ctrl Pts',(-8.32878742394358,13.686028489819,3.96392887501833));
#106054=CARTESIAN_POINT('Ctrl Pts',(-8.70057184656685,13.7651837454908,
2.35120927629056));
#106055=CARTESIAN_POINT('Ctrl Pts',(-10.2554772506561,13.8443390011625,
1.78452309056729));
#106056=CARTESIAN_POINT('Ctrl Pts',(-11.5777671320349,13.9234942568343,
2.77970463020884));
#106057=CARTESIAN_POINT('Ctrl Pts',(-11.4635336479878,14.0026495125061,
4.43072368178711));
#106058=CARTESIAN_POINT('Ctrl Pts',(-10.0167777334889,14.0818047681778,
5.23432466554119));
#106059=CARTESIAN_POINT('Ctrl Pts',(-8.55474717092323,14.1609600238496,
4.45886123527889));
#106060=CARTESIAN_POINT('Ctrl Pts',(-8.4085918471124,14.2401152795213,2.81036935499744));
#106061=CARTESIAN_POINT('Ctrl Pts',(-9.71138439389651,14.3192705351931,
1.78977498532776));
#106062=CARTESIAN_POINT('Ctrl Pts',(-11.2769559220394,14.3984257908649,
2.32630786842705));
#106063=CARTESIAN_POINT('Ctrl Pts',(-11.6798828962121,14.4775810465366,
3.93146607007081));
#106064=CARTESIAN_POINT('Ctrl Pts',(-10.5533076620495,14.5567363022084,
5.14378220205025));
#106065=CARTESIAN_POINT('Ctrl Pts',(-8.92295610591595,14.6358915578802,
4.85946530170135));
#106066=CARTESIAN_POINT('Ctrl Pts',(-8.27323299078649,14.7150468135519,
3.33738044165135));
#106067=CARTESIAN_POINT('Ctrl Pts',(-9.19569915917786,14.7942020692237,
1.96335770044252));
#106068=CARTESIAN_POINT('Ctrl Pts',(-10.8504662952567,14.8733573248955,
1.9884192039403));
#106069=CARTESIAN_POINT('Ctrl Pts',(-11.7308996735887,14.9525125805672,
3.38974694470339));
#106070=CARTESIAN_POINT('Ctrl Pts',(-11.0353810597377,15.031667836239,4.89145803910818));
#106071=CARTESIAN_POINT('Ctrl Pts',(-9.39716722968648,15.1108230919107,
5.1262724457309));
#106072=CARTESIAN_POINT('Ctrl Pts',(-8.30782143563832,15.1899783475825,
3.88039600672407));
#106073=CARTESIAN_POINT('Ctrl Pts',(-8.75917278251741,15.2691336032543,
2.28817607231548));
#106074=CARTESIAN_POINT('Ctrl Pts',(-10.3402742552705,15.348288858926,1.7992993070502));
#106075=CARTESIAN_POINT('Ctrl Pts',(-11.6115623412065,15.4274441145978,
2.85887892249356));
#106076=CARTESIAN_POINT('Ctrl Pts',(-11.4155528595928,15.5065993702696,
4.50218736636369));
#106077=CARTESIAN_POINT('Ctrl Pts',(-9.93070880145079,15.5857546259413,
5.23302283466301));
#106078=CARTESIAN_POINT('Ctrl Pts',(-8.5089530920962,15.6649098816131,4.38597321294798));
#106079=CARTESIAN_POINT('Ctrl Pts',(-8.44476788752832,15.7440651372849,
2.73226144295864));
#106080=CARTESIAN_POINT('Ctrl Pts',(-9.79659262388905,15.8232203929566,
1.77756136394283));
#106081=CARTESIAN_POINT('Ctrl Pts',(-11.3336159967253,15.9023756486284,
2.39110965875215));
#106082=CARTESIAN_POINT('Ctrl Pts',(-11.656406784211,15.9815309043001,4.01428200518281));
#106083=CARTESIAN_POINT('Ctrl Pts',(-10.4710699720557,16.0606861599719,
5.16921014167275));
#106084=CARTESIAN_POINT('Ctrl Pts',(-8.85683270320632,16.1398414156437,
4.80435345944898));
#106085=CARTESIAN_POINT('Ctrl Pts',(-8.28342801711096,16.2189966713154,
3.25190718834359));
#106086=CARTESIAN_POINT('Ctrl Pts',(-9.27293022613473,16.2981519269872,
1.92534481248533));
#106087=CARTESIAN_POINT('Ctrl Pts',(-10.9244159547161,16.3773071826589,
2.03247672648724));
#106088=CARTESIAN_POINT('Ctrl Pts',(-11.7342381329274,16.4564624383307,
3.47576131324842));
#106089=CARTESIAN_POINT('Ctrl Pts',(-10.9650687146612,16.5356176940025,
4.94111477392245));
#106090=CARTESIAN_POINT('Ctrl Pts',(-9.31722216345621,16.6147729496742,
5.09436001002277));
#106091=CARTESIAN_POINT('Ctrl Pts',(-8.29103214585774,16.693928205346,3.79597008150099));
#106092=CARTESIAN_POINT('Ctrl Pts',(-8.82082560544542,16.7730834610178,
2.228104893137));
#106093=CARTESIAN_POINT('Ctrl Pts',(-10.4242354412573,16.8522387166895,
1.8182765667279));
#106094=CARTESIAN_POINT('Ctrl Pts',(-11.6413867904435,16.9313939723613,
2.93962617852609));
#106095=CARTESIAN_POINT('Ctrl Pts',(-11.3640859652301,17.010549228033,4.57118574257565));
#106096=CARTESIAN_POINT('Ctrl Pts',(-9.84481021449978,17.0897044837048,
5.22745059151099));
#106097=CARTESIAN_POINT('Ctrl Pts',(-8.4668318799151,17.1688597393766,4.31090377431026));
#106098=CARTESIAN_POINT('Ctrl Pts',(-8.48477463115914,17.2480149950483,
2.65604413785062));
#106099=CARTESIAN_POINT('Ctrl Pts',(-9.88230192661505,17.3271702507201,
1.76959063249279));
#106100=CARTESIAN_POINT('Ctrl Pts',(-11.3869911309622,17.4063255063919,
2.45864270383911));
#106101=CARTESIAN_POINT('Ctrl Pts',(-11.6288506819897,17.4854807620636,
4.0958312440758));
#106102=CARTESIAN_POINT('Ctrl Pts',(-10.3876719524339,17.5646360177354,
5.19052650760978));
#106103=CARTESIAN_POINT('Ctrl Pts',(-8.79352511344672,17.6437912734072,
4.7460287973203));
#106104=CARTESIAN_POINT('Ctrl Pts',(-8.29785124138321,17.7229465290789,
3.16704501929752));
#106105=CARTESIAN_POINT('Ctrl Pts',(-9.35195218673424,17.8021017847507,
1.89121056463045));
#106106=CARTESIAN_POINT('Ctrl Pts',(-10.9960886248091,17.8812570404224,
2.08014899825329));
#106107=CARTESIAN_POINT('Ctrl Pts',(-11.7333048781308,17.9604122960942,
3.56183538698199));
#106108=CARTESIAN_POINT('Ctrl Pts',(-10.8923792461265,18.0395675517659,
4.98722180481529));
#106109=CARTESIAN_POINT('Ctrl Pts',(-9.23895889165499,18.1187228074378,
5.05852040315301));
#106110=CARTESIAN_POINT('Ctrl Pts',(-8.27845232556989,18.1978780631095,
3.71081513299456));
#106111=CARTESIAN_POINT('Ctrl Pts',(-8.8853829292997,18.2770333187813,2.1711666013609));
#106112=CARTESIAN_POINT('Ctrl Pts',(-10.5071516654119,18.356188574453,1.84139618838458));
#106113=CARTESIAN_POINT('Ctrl Pts',(-11.6671682334563,18.4353438301248,
3.02175372767848));
#106114=CARTESIAN_POINT('Ctrl Pts',(-11.3092591022783,18.5144990857966,
4.63754561171706));
#106115=CARTESIAN_POINT('Ctrl Pts',(-9.75929388557313,18.5936543414683,
5.21762335280841));
#106116=CARTESIAN_POINT('Ctrl Pts',(-8.42848711353859,18.6728095971401,
4.23383694600431));
#106117=CARTESIAN_POINT('Ctrl Pts',(-8.52851362464164,18.7519648528118,
2.58190563514964));
#106118=CARTESIAN_POINT('Ctrl Pts',(-9.96830113909682,18.8311201084836,
1.76588218455242));
#106119=CARTESIAN_POINT('Ctrl Pts',(-11.4369498774138,18.9102753641554,
2.5287407836031));
#106120=CARTESIAN_POINT('Ctrl Pts',(-11.597282452041,18.9894306198272,4.17591285239826));
#106121=CARTESIAN_POINT('Ctrl Pts',(-10.30331903289,19.0685858754989,5.20767882809444));
#106122=CARTESIAN_POINT('Ctrl Pts',(-8.73318927020649,19.1477411311707,
4.68463496086992));
#106123=CARTESIAN_POINT('Ctrl Pts',(-8.31646713862804,19.2268963868424,
3.08300297325283));
#106124=CARTESIAN_POINT('Ctrl Pts',(-9.43257039592116,19.3060516425142,
1.86103903034569));
#106125=CARTESIAN_POINT('Ctrl Pts',(-11.0653077644253,19.385206898186,2.13131859708315));
#106126=CARTESIAN_POINT('Ctrl Pts',(-11.7281022077035,19.4643621538577,
3.64775714996454));
#106127=CARTESIAN_POINT('Ctrl Pts',(-10.8174917004099,19.5435174095295,
5.02966556325107));
#106128=CARTESIAN_POINT('Ctrl Pts',(-9.16257018955271,19.6226726652012,
5.01884190362575));
#106129=CARTESIAN_POINT('Ctrl Pts',(-8.27011296098191,19.701827920873,3.62514091206507));
#106130=CARTESIAN_POINT('Ctrl Pts',(-8.95268573873123,19.7809831765448,
2.11750144528891));
#106131=CARTESIAN_POINT('Ctrl Pts',(-10.5888186914164,19.8601384322165,
1.86860122463147));
#106132=CARTESIAN_POINT('Ctrl Pts',(-11.6888431662962,19.9392936878883,
3.10505927623311));
#106133=CARTESIAN_POINT('Ctrl Pts',(-11.2512073183408,20.01844894356,4.70110351850519));
#106134=CARTESIAN_POINT('Ctrl Pts',(-9.67437045548402,20.0976041992318,
5.20356532465696));
#106135=CARTESIAN_POINT('Ctrl Pts',(-8.39401324244765,20.1767594549036,
4.15496255633562));
#106136=CARTESIAN_POINT('Ctrl Pts',(-8.57587713162465,20.2559147105753,
2.51002855020681));
#106137=CARTESIAN_POINT('Ctrl Pts',(-10.0543784310982,20.3350699662471,
1.76644515464131));
#106138=CARTESIAN_POINT('Ctrl Pts',(-11.4833691794522,20.4142252219189,
2.60123123491824));
#106139=CARTESIAN_POINT('Ctrl Pts',(-11.5617798521189,20.4933804775906,
4.25432957594862));
#106140=CARTESIAN_POINT('Ctrl Pts',(-10.2182189885692,20.5725357332624,
5.22062485413386));
#106141=CARTESIAN_POINT('Ctrl Pts',(-8.67597379061322,20.6516909889342,
4.62032317323714));
#106142=CARTESIAN_POINT('Ctrl Pts',(-8.33922985482189,20.7308462446059,
2.99998805962229));
#106143=CARTESIAN_POINT('Ctrl Pts',(-9.51458627775735,20.8100015002777,
1.83490452709347));
#106144=CARTESIAN_POINT('Ctrl Pts',(-11.1319028754137,20.8891567559494,
2.18585948382011));
#106145=CARTESIAN_POINT('Ctrl Pts',(-11.7186429366803,20.9683120116212,
3.73331496273064));
#106146=CARTESIAN_POINT('Ctrl Pts',(-10.740590537881,21.047467267293,5.0683415032564));
#106147=CARTESIAN_POINT('Ctrl Pts',(-9.08824421511444,21.1266225229647,
4.97542224612582));
#106148=CARTESIAN_POINT('Ctrl Pts',(-8.26603459332348,21.2057777786365,
3.53915844844108));
#106149=CARTESIAN_POINT('Ctrl Pts',(-9.02256825582621,21.2849330343083,
2.06724161104649));
#106150=CARTESIAN_POINT('Ctrl Pts',(-10.6690353599237,21.36408828998,1.8998246649798));
#106151=CARTESIAN_POINT('Ctrl Pts',(-11.7063582000309,21.4432435456518,
3.18933762889195));
#106152=CARTESIAN_POINT('Ctrl Pts',(-11.1900736045309,21.5223988013236,
4.76170290933883));
#106153=CARTESIAN_POINT('Ctrl Pts',(-9.59024910463943,21.6015540569953,
5.18531113429732));
#106154=CARTESIAN_POINT('Ctrl Pts',(-8.36349518146937,21.6807093126671,
4.07447488592744));
#106155=CARTESIAN_POINT('Ctrl Pts',(-8.62674848798312,21.7598645683389,
2.44058992813047));
#106156=CARTESIAN_POINT('Ctrl Pts',(-10.1403217800601,21.8390198240106,
1.77127815607141));
#106157=CARTESIAN_POINT('Ctrl Pts',(-11.526134698685,21.9181750796824,2.6759355018536));
#106158=CARTESIAN_POINT('Ctrl Pts',(-11.522430330979,21.9973303353541,4.33088826141085));
#106159=CARTESIAN_POINT('Ctrl Pts',(-10.1325814349091,22.0764855910259,
5.22933269753159));
#106160=CARTESIAN_POINT('Ctrl Pts',(-8.62201960582365,22.1556408466977,
4.55325184495658));
#106161=CARTESIAN_POINT('Ctrl Pts',(-8.36608332164426,22.2347961023694,
2.91820475782117));
#106162=CARTESIAN_POINT('Ctrl Pts',(-9.59779781360324,22.3139513580411,
1.81287142846536));
#106163=CARTESIAN_POINT('Ctrl Pts',(-11.1957099230445,22.393106613713,2.24363731526574));
#106164=CARTESIAN_POINT('Ctrl Pts',(-11.7049503647936,22.4722618693847,
3.81829808229183));
#106165=CARTESIAN_POINT('Ctrl Pts',(-10.6618651788015,22.5514171250564,
5.10315435960114));
#106166=CARTESIAN_POINT('Ctrl Pts',(-9.01616404542407,22.6305723807283,
4.92836838045495));
#106167=CARTESIAN_POINT('Ctrl Pts',(-8.26622726836883,22.7097276364,3.45307953105006));
#106168=CARTESIAN_POINT('Ctrl Pts',(-9.09485834826755,22.7888828920717,
2.0205108969932));
#106169=CARTESIAN_POINT('Ctrl Pts',(-10.7476040843601,22.8680381477436,
1.93498960075163));
#106170=CARTESIAN_POINT('Ctrl Pts',(-11.7196701916628,22.9471934034153,
3.27438119455899));
#106171=CARTESIAN_POINT('Ctrl Pts',(-11.1260085443793,23.0263486590871,
4.81919451720226));
#106172=CARTESIAN_POINT('Ctrl Pts',(-9.50713703565121,23.1055039147588,
5.16290574620378));
#106173=CARTESIAN_POINT('Ctrl Pts',(-8.33700810572673,23.1846591704306,
3.9925721865046));
#106174=CARTESIAN_POINT('Ctrl Pts',(-8.68100238130063,23.2638144261023,
2.37376081282388));
#106175=CARTESIAN_POINT('Ctrl Pts',(-10.2259195084625,23.3429696817741,
1.78036927452147));
#106176=CARTESIAN_POINT('Ctrl Pts',(-11.5651410675949,23.4221249374458,
2.75266959436419));
#106177=CARTESIAN_POINT('Ctrl Pts',(-11.4793308685935,23.5012801931177,
4.4054002959104));
#106178=CARTESIAN_POINT('Ctrl Pts',(-10.0466172046406,23.5804354487894,
5.23378097889537));
#106179=CARTESIAN_POINT('Ctrl Pts',(-8.57145981851902,23.6595907044612,
4.48358605052702));
#106180=CARTESIAN_POINT('Ctrl Pts',(-8.39696100206443,23.7387459601329,
2.83785476917708));
#106181=CARTESIAN_POINT('Ctrl Pts',(-9.68200079264003,23.8179012158047,
1.79499351538082));
#106182=CARTESIAN_POINT('Ctrl Pts',(-11.2565702958328,23.8970564714764,
2.30451071544906));
#106183=CARTESIAN_POINT('Ctrl Pts',(-11.68706098934,23.9762117271482,3.90249537746301));
#106184=CARTESIAN_POINT('Ctrl Pts',(-10.5815042229309,24.05536698282,5.13402184238338));
#106185=CARTESIAN_POINT('Ctrl Pts',(-8.94651741854107,24.1345222384917,
4.87778957136504));
#106186=CARTESIAN_POINT('Ctrl Pts',(-8.27067096015597,24.2136774941635,
3.36712891673609));
#106187=CARTESIAN_POINT('Ctrl Pts',(-9.16941545665505,24.2928327498353,
1.97739998955691));
#106188=CARTESIAN_POINT('Ctrl Pts',(-10.8242593981243,24.371988005507,1.97405625657309));
#106189=CARTESIAN_POINT('Ctrl Pts',(-11.7288843588558,24.4511432611788,
3.35989062967651));
#106190=CARTESIAN_POINT('Ctrl Pts',(-11.0589050694329,24.5302985168505,
4.87360926711793));
#106191=CARTESIAN_POINT('Ctrl Pts',(-9.42574840582899,24.6094537725223,
5.13607197096169));
#106192=CARTESIAN_POINT('Ctrl Pts',(-8.3136275442009,24.6886090281941,3.91010675923693));
#106193=CARTESIAN_POINT('Ctrl Pts',(-8.74057475057857,24.7677748232262,
2.30812637245377));
#106194=CARTESIAN_POINT('Ctrl Pts',(-9.78464073208413,24.8205555330345,
1.96751243971017));
#106195=CARTESIAN_POINT('Ctrl Pts',(-10.2639206363603,24.8469511576188,
2.05506967699429));
#106196=CARTESIAN_POINT('Ctrl Pts',(-9.20319421055138,13.1883418974182,
4.61582047396927));
#106197=CARTESIAN_POINT('Ctrl Pts',(-8.83313174321593,13.2147333465434,
4.3515698857443));
#106198=CARTESIAN_POINT('Ctrl Pts',(-8.38289651005301,13.2675098808925,
3.43070333804874));
#106199=CARTESIAN_POINT('Ctrl Pts',(-9.17875805629518,13.3466715004656,
2.10352106443306));
#106200=CARTESIAN_POINT('Ctrl Pts',(-10.7230082002845,13.4258267561374,
2.05189064434031));
#106201=CARTESIAN_POINT('Ctrl Pts',(-11.6085908305356,13.5049820118091,
3.31675406783516));
#106202=CARTESIAN_POINT('Ctrl Pts',(-11.0297808758882,13.5841372674809,
4.74948327743878));
#106203=CARTESIAN_POINT('Ctrl Pts',(-9.51327053705405,13.6632925231527,
5.04404854424627));
#106204=CARTESIAN_POINT('Ctrl Pts',(-8.43997256895578,13.7424477788244,
3.93306386120543));
#106205=CARTESIAN_POINT('Ctrl Pts',(-8.78702231357646,13.8216030344962,
2.42763789167694));
#106206=CARTESIAN_POINT('Ctrl Pts',(-10.2384804451219,13.9007582901679,
1.89865312505424));
#106207=CARTESIAN_POINT('Ctrl Pts',(-11.4727988773174,13.9799135458397,
2.82762561063302));
#106208=CARTESIAN_POINT('Ctrl Pts',(-11.3661653040601,14.0590688015115,
4.36880298479835));
#106209=CARTESIAN_POINT('Ctrl Pts',(-10.0156615171812,14.1382240571832,
5.11894069691916));
#106210=CARTESIAN_POINT('Ctrl Pts',(-8.65089929883466,14.217379312855,4.39506855742421));
#106211=CARTESIAN_POINT('Ctrl Pts',(-8.51446763382406,14.2965345685268,
2.85625022279848));
#106212=CARTESIAN_POINT('Ctrl Pts',(-9.73058588177254,14.3756898241985,
1.90355561322882));
#106213=CARTESIAN_POINT('Ctrl Pts',(-11.1920005241443,14.4548450798703,
2.40439316512615));
#106214=CARTESIAN_POINT('Ctrl Pts',(-11.5681209180563,14.534000335542,3.90276079447873));
#106215=CARTESIAN_POINT('Ctrl Pts',(-10.5164963111043,14.6131555912138,
5.03442198951837));
#106216=CARTESIAN_POINT('Ctrl Pts',(-8.99461143167394,14.6923108468856,
4.76902058576619));
#106217=CARTESIAN_POINT('Ctrl Pts',(-8.38811415137153,14.7714661025573,
3.34819945979173));
#106218=CARTESIAN_POINT('Ctrl Pts',(-9.249208992039,14.8506213582291,2.06558993550106));
#106219=CARTESIAN_POINT('Ctrl Pts',(-10.793885092051,14.9297766139009,2.08898410658372));
#106220=CARTESIAN_POINT('Ctrl Pts',(-11.6157435683949,15.0089318695726,
3.39708203906353));
#106221=CARTESIAN_POINT('Ctrl Pts',(-10.966497546701,15.0880871252444,4.79888485836913));
#106222=CARTESIAN_POINT('Ctrl Pts',(-9.43727346748395,15.1672423809162,
5.01807715071069));
#106223=CARTESIAN_POINT('Ctrl Pts',(-8.42040143997807,15.2463976365879,
3.85508840326556));
#106224=CARTESIAN_POINT('Ctrl Pts',(-8.84172455126754,15.3255528922597,
2.36879826308837));
#106225=CARTESIAN_POINT('Ctrl Pts',(-10.3176359368674,15.4047081479315,
1.91244628540419));
#106226=CARTESIAN_POINT('Ctrl Pts',(-11.5043457039156,15.4838634036032,
2.90153246698827));
#106227=CARTESIAN_POINT('Ctrl Pts',(-11.3213766594965,15.563018659275,4.43551221728033));
#106228=CARTESIAN_POINT('Ctrl Pts',(-9.93531871886594,15.6421739149467,
5.11772547636037));
#106229=CARTESIAN_POINT('Ctrl Pts',(-8.60815188287271,15.7213291706185,
4.32702974784375));
#106230=CARTESIAN_POINT('Ctrl Pts',(-8.54823689585808,15.8004844262903,
2.7833388008119));
#106231=CARTESIAN_POINT('Ctrl Pts',(-9.81012524022611,15.879639681962,1.89215455948744));
#106232=CARTESIAN_POINT('Ctrl Pts',(-11.2448910253417,15.9587949376338,
2.46488371667913));
#106233=CARTESIAN_POINT('Ctrl Pts',(-11.5462066629694,16.0379501933055,
3.98006701653167));
#106234=CARTESIAN_POINT('Ctrl Pts',(-10.439729863739,16.1171054489773,5.05815821786802));
#106235=CARTESIAN_POINT('Ctrl Pts',(-8.93288719411203,16.1962607046491,
4.71757531367999));
#106236=CARTESIAN_POINT('Ctrl Pts',(-8.39763090642369,16.2754159603208,
3.26841270992457));
#106237=CARTESIAN_POINT('Ctrl Pts',(-9.32130190511764,16.3545712159926,
2.03010603070281));
#106238=CARTESIAN_POINT('Ctrl Pts',(-10.8629149084403,16.4337264716644,
2.1301104987027));
#106239=CARTESIAN_POINT('Ctrl Pts',(-11.6188599212877,16.5128817273361,
3.47737390397444));
#106240=CARTESIAN_POINT('Ctrl Pts',(-10.9008630555346,16.5920369830079,
4.84523794926625));
#106241=CARTESIAN_POINT('Ctrl Pts',(-9.36264711648426,16.6711922386796,
4.98828783736456));
#106242=CARTESIAN_POINT('Ctrl Pts',(-8.4047291353409,16.7503474943514,3.77627930313895));
#106243=CARTESIAN_POINT('Ctrl Pts',(-8.89927563504166,16.8295027500232,
2.31272359689913));
#106244=CARTESIAN_POINT('Ctrl Pts',(-10.3960112166845,16.908658005695,1.930160995123));
#106245=CARTESIAN_POINT('Ctrl Pts',(-11.5321859437461,16.9878132613667,
2.97690763840396));
#106246=CARTESIAN_POINT('Ctrl Pts',(-11.2733338382859,17.0669685170385,
4.49992015743727));
#106247=CARTESIAN_POINT('Ctrl Pts',(-9.85513493264302,17.1461237727102,
5.11252395245242));
#106248=CARTESIAN_POINT('Ctrl Pts',(-8.56883297911816,17.225279028382,4.25695465076404));
#106249=CARTESIAN_POINT('Ctrl Pts',(-8.58558200586084,17.3044342840538,
2.71219220438708));
#106250=CARTESIAN_POINT('Ctrl Pts',(-9.89013233523239,17.3835895397255,
1.88471411780712));
#106251=CARTESIAN_POINT('Ctrl Pts',(-11.2947151319445,17.4627447953973,
2.52792381364047));
#106252=CARTESIAN_POINT('Ctrl Pts',(-11.5204838578795,17.541900051069,4.05619081518931));
#106253=CARTESIAN_POINT('Ctrl Pts',(-10.36188028304,17.6210553067408,5.07805641398524));
#106254=CARTESIAN_POINT('Ctrl Pts',(-8.87379143452213,17.7002105624126,
4.66313096941719));
#106255=CARTESIAN_POINT('Ctrl Pts',(-8.41109455900217,17.7793658180843,
3.18919638911266));
#106256=CARTESIAN_POINT('Ctrl Pts',(-9.39506656435745,17.8585210737561,
1.99824272153759));
#106257=CARTESIAN_POINT('Ctrl Pts',(-10.9298192227108,17.9376763294279,
2.17461115213288));
#106258=CARTESIAN_POINT('Ctrl Pts',(-11.6179887555821,18.0168315850996,
3.55772150191017));
#106259=CARTESIAN_POINT('Ctrl Pts',(-10.8330095900408,18.0959868407714,
4.88827749671063));
#106260=CARTESIAN_POINT('Ctrl Pts',(-9.2895906707619,18.1751420964431,4.95483262607923));
#106261=CARTESIAN_POINT('Ctrl Pts',(-8.39298624577207,18.2542973521149,
3.69678968137423));
#106262=CARTESIAN_POINT('Ctrl Pts',(-8.95953798438631,18.3334526077867,
2.25957338829005));
#106263=CARTESIAN_POINT('Ctrl Pts',(-10.4734110555877,18.4126078634584,
1.95174247703412));
#106264=CARTESIAN_POINT('Ctrl Pts',(-11.5562521570384,18.4917631191302,
3.05357127255664));
#106265=CARTESIAN_POINT('Ctrl Pts',(-11.2221545859343,18.5709183748019,
4.56186512940809));
#106266=CARTESIAN_POINT('Ctrl Pts',(-9.77530797296171,18.6500736304738,
5.10335051624982));
#106267=CARTESIAN_POINT('Ctrl Pts',(-8.53303927564717,18.7292288861455,
4.18501504960061));
#106268=CARTESIAN_POINT('Ctrl Pts',(-8.62641106053443,18.8083841418173,
2.6429861084259));
#106269=CARTESIAN_POINT('Ctrl Pts',(-9.97041005240727,18.887539397489,1.88125239151542));
#106270=CARTESIAN_POINT('Ctrl Pts',(-11.341350141758,18.9666946531608,2.59335829448514));
#106271=CARTESIAN_POINT('Ctrl Pts',(-11.4910158504129,19.0458499088325,
4.13094462418708));
#106272=CARTESIAN_POINT('Ctrl Pts',(-10.2831393315521,19.1250051645043,
5.09406759703012));
#106273=CARTESIAN_POINT('Ctrl Pts',(-8.81746971227177,19.2041604201761,
4.6058216418476));
#106274=CARTESIAN_POINT('Ctrl Pts',(-8.42847194759504,19.2833156758479,
3.11074562882687));
#106275=CARTESIAN_POINT('Ctrl Pts',(-9.47032127436574,19.3624709315196,
1.97007848809699));
#106276=CARTESIAN_POINT('Ctrl Pts',(-10.9944332389656,19.4416261871914,
2.22237645677081));
#106277=CARTESIAN_POINT('Ctrl Pts',(-11.6131322168643,19.5207814428631,
3.63792692227193));
#106278=CARTESIAN_POINT('Ctrl Pts',(-10.7631042846145,19.5999366985349,
4.92789748783868));
#106279=CARTESIAN_POINT('Ctrl Pts',(-9.21828408032049,19.6790919542066,
4.91779392222309));
#106280=CARTESIAN_POINT('Ctrl Pts',(-8.38520169597802,19.7582472098784,
3.61681533418571));
#106281=CARTESIAN_POINT('Ctrl Pts',(-9.02236316318391,19.8374024655502,
2.209478554896));
#106282=CARTESIAN_POINT('Ctrl Pts',(-10.5496448050245,19.9165577212219,
1.97713757243713));
#106283=CARTESIAN_POINT('Ctrl Pts',(-11.5764850647372,19.9957129768937,
3.13133453425377));
#106284=CARTESIAN_POINT('Ctrl Pts',(-11.1679649653791,20.0748682325655,
4.62119455252864));
#106285=CARTESIAN_POINT('Ctrl Pts',(-9.69603446678095,20.1540234882372,
5.09022776343139));
#106286=CARTESIAN_POINT('Ctrl Pts',(-8.50085893825222,20.233178743909,4.11138814345296));
#106287=CARTESIAN_POINT('Ctrl Pts',(-8.67062349118661,20.3123339995808,
2.57589097894878));
#106288=CARTESIAN_POINT('Ctrl Pts',(-10.0507606545005,20.3914892552525,
1.88177790741573));
#106289=CARTESIAN_POINT('Ctrl Pts',(-11.384681185066,20.4706445109243,2.66102598330019));
#106290=CARTESIAN_POINT('Ctrl Pts',(-11.4578752251296,20.549799766596,4.20414431257134));
#106291=CARTESIAN_POINT('Ctrl Pts',(-10.2037009612183,20.6289550222678,
5.10615232881938));
#106292=CARTESIAN_POINT('Ctrl Pts',(-8.76406075704688,20.7081102779396,
4.54578849329186));
#106293=CARTESIAN_POINT('Ctrl Pts',(-8.44972026882971,20.7872655336113,
3.03325366622149));
#106294=CARTESIAN_POINT('Ctrl Pts',(-9.54688067038685,20.8664207892831,
1.94568270353057));
#106295=CARTESIAN_POINT('Ctrl Pts',(-11.0565978022317,20.9455760449549,
2.27328875879759));
#106296=CARTESIAN_POINT('Ctrl Pts',(-11.6043022675897,21.0247313006266,
3.71779260588845));
#106297=CARTESIAN_POINT('Ctrl Pts',(-10.6913193275462,21.1038865562984,
4.96400033208134));
#106298=CARTESIAN_POINT('Ctrl Pts',(-9.14890298504629,21.1830418119701,
4.87726295822911));
#106299=CARTESIAN_POINT('Ctrl Pts',(-8.38139466058816,21.2621970676419,
3.5365532515734));
#106300=CARTESIAN_POINT('Ctrl Pts',(-9.08759642266299,21.3413523233137,
2.16256248854919));
#106301=CARTESIAN_POINT('Ctrl Pts',(-10.6245246887038,21.4205075789854,
2.00628372902598));
#106302=CARTESIAN_POINT('Ctrl Pts',(-11.5928348298557,21.4996628346572,
3.2100058797634));
#106303=CARTESIAN_POINT('Ctrl Pts',(-11.1108984545884,21.578818090329,4.67776228865001));
#106304=CARTESIAN_POINT('Ctrl Pts',(-9.61750967781382,21.6579733460008,
5.07318801750046));
#106305=CARTESIAN_POINT('Ctrl Pts',(-8.47237123240889,21.7371286016725,
4.03625528752755));
#106306=CARTESIAN_POINT('Ctrl Pts',(-8.71811039531279,21.8162838573443,
2.51107208231946));
#106307=CARTESIAN_POINT('Ctrl Pts',(-10.1309862247346,21.895439113016,1.88628937107586));
#106308=CARTESIAN_POINT('Ctrl Pts',(-11.4246015303662,21.9745943686878,
2.7307602034137));
#106309=CARTESIAN_POINT('Ctrl Pts',(-11.4211436128521,22.0537496243595,
4.27560957744361));
#106310=CARTESIAN_POINT('Ctrl Pts',(-10.1237608418393,22.1329048800313,
5.11428084266634));
#106311=CARTESIAN_POINT('Ctrl Pts',(-8.71369612390732,22.2120601357031,
4.4831793952912));
#106312=CARTESIAN_POINT('Ctrl Pts',(-8.47478718458996,22.2912153913748,
2.95691137677308));
#106313=CARTESIAN_POINT('Ctrl Pts',(-9.62455617400543,22.3703706470466,
1.92511545867901));
#106314=CARTESIAN_POINT('Ctrl Pts',(-11.1161597909483,22.4495259027183,
2.32722265281731));
#106315=CARTESIAN_POINT('Ctrl Pts',(-11.5915206573679,22.5286811583902,
3.79712183042311));
#106316=CARTESIAN_POINT('Ctrl Pts',(-10.6178315370386,22.6078364140618,
4.99649710216846));
#106317=CARTESIAN_POINT('Ctrl Pts',(-9.08161828197361,22.6869916697337,
4.83333956856887));
#106318=CARTESIAN_POINT('Ctrl Pts',(-8.3815745170351,22.7661469254054,3.45620113222694));
#106319=CARTESIAN_POINT('Ctrl Pts',(-9.15507708240484,22.8453021810772,
2.11894075135078));
#106320=CARTESIAN_POINT('Ctrl Pts',(-10.6978662654123,22.9244574367489,
2.03910915482813));
#106321=CARTESIAN_POINT('Ctrl Pts',(-11.605261179684,23.0036126924207,3.28939152894722));
#106322=CARTESIAN_POINT('Ctrl Pts',(-11.0510956188272,23.0827679480924,
4.73142900143493));
#106323=CARTESIAN_POINT('Ctrl Pts',(-9.53992702356022,23.1619232037643,
5.0522732514618));
#106324=CARTESIAN_POINT('Ctrl Pts',(-8.4476463318674,23.2410784594359,3.95980154393634));
#106325=CARTESIAN_POINT('Ctrl Pts',(-8.76875479748452,23.3202337151078,
2.4486890829546));
#106326=CARTESIAN_POINT('Ctrl Pts',(-10.2108891684152,23.3993889707795,
1.89477566082987));
#106327=CARTESIAN_POINT('Ctrl Pts',(-11.4610128202023,23.4785442264513,
2.80238920556933));
#106328=CARTESIAN_POINT('Ctrl Pts',(-11.3809115415121,23.5576994821231,
4.34516435427308));
#106329=CARTESIAN_POINT('Ctrl Pts',(-10.0435157795242,23.6368547377948,
5.1184331815417));
#106330=CARTESIAN_POINT('Ctrl Pts',(-8.66650006026283,23.7160099934666,
4.41814844));
#106331=CARTESIAN_POINT('Ctrl Pts',(-8.50361058452884,23.7951652491383,
2.8819070426957));
#106332=CARTESIAN_POINT('Ctrl Pts',(-9.70315716047176,23.8743205048101,
1.90842695643741));
#106333=CARTESIAN_POINT('Ctrl Pts',(-11.1729711459929,23.9534757604818,
2.38404616854922));
#106334=CARTESIAN_POINT('Ctrl Pts',(-11.5748214553443,24.0326310161536,
3.87571751116932));
#106335=CARTESIAN_POINT('Ctrl Pts',(-10.5428169653803,24.1117862718254,
5.02531098291438));
#106336=CARTESIAN_POINT('Ctrl Pts',(-9.01660521901929,24.1909415274972,
4.78612574865134));
#106337=CARTESIAN_POINT('Ctrl Pts',(-8.38572257167664,24.2700967831689,
3.375968780002));
#106338=CARTESIAN_POINT('Ctrl Pts',(-9.22467393437342,24.3492520388406,
2.07869799639465));
#106339=CARTESIAN_POINT('Ctrl Pts',(-10.7694217299418,24.4284072945125,
2.07557672071041));
#106340=CARTESIAN_POINT('Ctrl Pts',(-11.6138623317943,24.5075625501842,
3.36921205346196));
#106341=CARTESIAN_POINT('Ctrl Pts',(-10.9884565128663,24.586717805856,4.78222355847577));
#106342=CARTESIAN_POINT('Ctrl Pts',(-9.46395314871217,24.6658730615277,
5.02722471720835));
#106343=CARTESIAN_POINT('Ctrl Pts',(-8.42582127031864,24.7450283171995,
3.8828225105725));
#106344=CARTESIAN_POINT('Ctrl Pts',(-8.82436383940853,24.8241941122316,
2.38742127725138));
#106345=CARTESIAN_POINT('Ctrl Pts',(-9.79896850329409,24.8769748220399,
2.06946826152566));
#106346=CARTESIAN_POINT('Ctrl Pts',(-10.2463620955464,24.9033704466242,
2.15120034869797));
#106347=CARTESIAN_POINT('Ctrl Pts',(-9.25998357558652,13.2447611864237,
4.53629452542694));
#106348=CARTESIAN_POINT('Ctrl Pts',(-8.91629593235703,13.2711526355489,
4.290877413708));
#106349=CARTESIAN_POINT('Ctrl Pts',(-8.49814953859056,13.323929169898,3.43564219954219));
#106350=CARTESIAN_POINT('Ctrl Pts',(-9.23728901721539,13.4030907894711,
2.20304989954692));
#106351=CARTESIAN_POINT('Ctrl Pts',(-10.6714784835667,13.4822460451429,
2.15509924535495));
#106352=CARTESIAN_POINT('Ctrl Pts',(-11.4939445100931,13.5614013008146,
3.32981423917266));
#106353=CARTESIAN_POINT('Ctrl Pts',(-10.9563870792549,13.6405565564864,
4.66043101039028));
#106354=CARTESIAN_POINT('Ctrl Pts',(-9.54796036675987,13.7197118121582,
4.93400223487913));
#106355=CARTESIAN_POINT('Ctrl Pts',(-8.55115771396801,13.7988670678299,
3.90219884739254));
#106356=CARTESIAN_POINT('Ctrl Pts',(-8.87347278058603,13.8780223235017,
2.50406650706332));
#106357=CARTESIAN_POINT('Ctrl Pts',(-10.2214836395877,13.9571775791735,
2.0127831595412));
#106358=CARTESIAN_POINT('Ctrl Pts',(-11.3678306225998,14.0363328348452,
2.87554659105721));
#106359=CARTESIAN_POINT('Ctrl Pts',(-11.2687969601324,14.115488090517,4.30688228780959));
#106360=CARTESIAN_POINT('Ctrl Pts',(-10.0145453008736,14.1946433461887,
5.00355672829712));
#106361=CARTESIAN_POINT('Ctrl Pts',(-8.74705142674612,14.2737986018605,
4.33127587956952));
#106362=CARTESIAN_POINT('Ctrl Pts',(-8.62034342053574,14.3529538575323,
2.90213109059951));
#106363=CARTESIAN_POINT('Ctrl Pts',(-9.74978736964855,14.432109113204,2.01733624112986));
#106364=CARTESIAN_POINT('Ctrl Pts',(-11.1070451262493,14.5112643688758,
2.48247846182523));
#106365=CARTESIAN_POINT('Ctrl Pts',(-11.4563589399006,14.5904196245476,
3.87405551888664));
#106366=CARTESIAN_POINT('Ctrl Pts',(-10.479684960159,14.6695748802193,4.92506177698652));
#106367=CARTESIAN_POINT('Ctrl Pts',(-9.06626675743199,14.7487301358911,
4.678575869831));
#106368=CARTESIAN_POINT('Ctrl Pts',(-8.50299531195658,14.8278853915628,
3.35901847793213));
#106369=CARTESIAN_POINT('Ctrl Pts',(-9.30271882490017,14.9070406472346,
2.16782217055959));
#106370=CARTESIAN_POINT('Ctrl Pts',(-10.737303888845,14.9861959029064,2.18954900922713));
#106371=CARTESIAN_POINT('Ctrl Pts',(-11.5005874632012,15.0653511585781,
3.40441713342364));
#106372=CARTESIAN_POINT('Ctrl Pts',(-10.8976140336643,15.1445064142499,
4.70631167763009));
#106373=CARTESIAN_POINT('Ctrl Pts',(-9.4773797052814,15.2236616699217,4.90988185569045));
#106374=CARTESIAN_POINT('Ctrl Pts',(-8.53298144431783,15.3028169255934,
3.82978079980707));
#106375=CARTESIAN_POINT('Ctrl Pts',(-8.92427632001765,15.3819721812652,
2.44942045386124));
#106376=CARTESIAN_POINT('Ctrl Pts',(-10.2949976184642,15.4611274369369,
2.02559326375819));
#106377=CARTESIAN_POINT('Ctrl Pts',(-11.3971290666245,15.5402826926087,
2.94418601148299));
#106378=CARTESIAN_POINT('Ctrl Pts',(-11.2272004594,15.6194379482805,4.36883706819697));
#106379=CARTESIAN_POINT('Ctrl Pts',(-9.93992863628107,15.6985932039522,
5.00242811805772));
#106380=CARTESIAN_POINT('Ctrl Pts',(-8.7073506736492,15.777748459624,4.26808628273949));
#106381=CARTESIAN_POINT('Ctrl Pts',(-8.65170590418785,15.8569037152958,
2.83441615866517));
#106382=CARTESIAN_POINT('Ctrl Pts',(-9.82365785656318,15.9360589709675,
2.00674775503204));
#106383=CARTESIAN_POINT('Ctrl Pts',(-11.1561660539582,16.0152142266393,
2.5386577746061));
#106384=CARTESIAN_POINT('Ctrl Pts',(-11.436006541728,16.094369482311,3.94585202788052));
#106385=CARTESIAN_POINT('Ctrl Pts',(-10.4083897554222,16.1735247379828,
4.94710629406329));
#106386=CARTESIAN_POINT('Ctrl Pts',(-9.00894168501776,16.2526799936546,
4.63079716791098));
#106387=CARTESIAN_POINT('Ctrl Pts',(-8.51183379573641,16.3318352493264,
3.28491823150556));
#106388=CARTESIAN_POINT('Ctrl Pts',(-9.36967358410055,16.4109905049981,
2.13486724892028));
#106389=CARTESIAN_POINT('Ctrl Pts',(-10.8014138621645,16.4901457606699,
2.22774427091815));
#106390=CARTESIAN_POINT('Ctrl Pts',(-11.503481709648,16.5693010163416,3.47898649470048));
#106391=CARTESIAN_POINT('Ctrl Pts',(-10.836657396408,16.6484562720134,4.74936112461004));
#106392=CARTESIAN_POINT('Ctrl Pts',(-9.40807206951228,16.7276115276852,
4.88221566470634));
#106393=CARTESIAN_POINT('Ctrl Pts',(-8.51842612482407,16.8067667833569,
3.75658852477692));
#106394=CARTESIAN_POINT('Ctrl Pts',(-8.97772566463787,16.8859220390287,
2.39734230066127));
#106395=CARTESIAN_POINT('Ctrl Pts',(-10.3677869921117,16.9650772947004,
2.0420454235181));
#106396=CARTESIAN_POINT('Ctrl Pts',(-11.4229850970487,17.0442325503722,
3.01418909828181));
#106397=CARTESIAN_POINT('Ctrl Pts',(-11.1825817113415,17.123387806044,4.4286545722989));
#106398=CARTESIAN_POINT('Ctrl Pts',(-9.8654596507863,17.2025430617157,4.99759731339386));
#106399=CARTESIAN_POINT('Ctrl Pts',(-8.6708340783212,17.2816983173875,4.20300552721785));
#106400=CARTESIAN_POINT('Ctrl Pts',(-8.68638938056257,17.3608535730592,
2.76834027092352));
#106401=CARTESIAN_POINT('Ctrl Pts',(-9.89796274384974,17.440008828731,1.99983760312146));
#106402=CARTESIAN_POINT('Ctrl Pts',(-11.2024391329266,17.5191640844028,
2.59720492344182));
#106403=CARTESIAN_POINT('Ctrl Pts',(-11.4121170337693,17.5983193400746,
4.01655038630282));
#106404=CARTESIAN_POINT('Ctrl Pts',(-10.3360886136461,17.6774745957463,
4.96558632036072));
#106405=CARTESIAN_POINT('Ctrl Pts',(-8.95405775559752,17.7566298514181,
4.58023314151408));
#106406=CARTESIAN_POINT('Ctrl Pts',(-8.52433787662112,17.8357851070898,
3.2113477589278));
#106407=CARTESIAN_POINT('Ctrl Pts',(-9.43818094198068,17.9149403627616,
2.10527487844473));
#106408=CARTESIAN_POINT('Ctrl Pts',(-10.8635498206126,17.9940956184334,
2.26907330601246));
#106409=CARTESIAN_POINT('Ctrl Pts',(-11.5026726330335,18.0732508741052,
3.55360761683835));
#106410=CARTESIAN_POINT('Ctrl Pts',(-10.7736399339552,18.1524061297769,
4.78933318860598));
#106411=CARTESIAN_POINT('Ctrl Pts',(-9.34022244986883,18.2315613854487,
4.85114484900545));
#106412=CARTESIAN_POINT('Ctrl Pts',(-8.50752016597425,18.3107166411204,
3.68276422975389));
#106413=CARTESIAN_POINT('Ctrl Pts',(-9.03369303947292,18.3898718967922,
2.34798017521921));
#106414=CARTESIAN_POINT('Ctrl Pts',(-10.4396704457635,18.469027152464,2.06208876568365));
#106415=CARTESIAN_POINT('Ctrl Pts',(-11.4453360806203,18.5481824081357,
3.08538881743479));
#106416=CARTESIAN_POINT('Ctrl Pts',(-11.1350500695903,18.6273376638075,
4.48618464709913));
#106417=CARTESIAN_POINT('Ctrl Pts',(-9.7913220603503,18.7064929194792,4.98907767969123));
#106418=CARTESIAN_POINT('Ctrl Pts',(-8.63759143775575,18.785648175151,4.13619315319688));
#106419=CARTESIAN_POINT('Ctrl Pts',(-8.72430849642721,18.8648034308228,
2.70406658170217));
#106420=CARTESIAN_POINT('Ctrl Pts',(-9.97251896571771,18.9439586864945,
1.9966225984784));
#106421=CARTESIAN_POINT('Ctrl Pts',(-11.2457504061023,19.0231139421663,
2.65797580536718));
#106422=CARTESIAN_POINT('Ctrl Pts',(-11.3847492487849,19.1022691978381,
4.08597639597589));
#106423=CARTESIAN_POINT('Ctrl Pts',(-10.2629596302143,19.1814244535098,
4.98045636596579));
#106424=CARTESIAN_POINT('Ctrl Pts',(-8.90175015433707,19.2605797091816,
4.52700832282528));
#106425=CARTESIAN_POINT('Ctrl Pts',(-8.54047675656204,19.3397349648533,
3.13848828440091));
#106426=CARTESIAN_POINT('Ctrl Pts',(-9.5080721528103,19.4188902205251,2.07911794584829));
#106427=CARTESIAN_POINT('Ctrl Pts',(-10.9235587135059,19.4980454761969,
2.31343431645849));
#106428=CARTESIAN_POINT('Ctrl Pts',(-11.4981622260253,19.5772007318686,
3.62809669457932));
#106429=CARTESIAN_POINT('Ctrl Pts',(-10.7087168688192,19.6563559875404,
4.82612941242628));
#106430=CARTESIAN_POINT('Ctrl Pts',(-9.27399797108825,19.7355112432122,
4.81674594082043));
#106431=CARTESIAN_POINT('Ctrl Pts',(-8.50029043097417,19.8146664988839,
3.60848975630635));
#106432=CARTESIAN_POINT('Ctrl Pts',(-9.09204058763656,19.8938217545557,
2.30145566450311));
#106433=CARTESIAN_POINT('Ctrl Pts',(-10.5104709186327,19.9729770102274,
2.08567392024281));
#106434=CARTESIAN_POINT('Ctrl Pts',(-11.464126963178,20.0521322658992,3.15760979227444));
#106435=CARTESIAN_POINT('Ctrl Pts',(-11.0847226124176,20.131287521571,4.5412855865521));
#106436=CARTESIAN_POINT('Ctrl Pts',(-9.71769847807786,20.2104427772427,
4.97689020220581));
#106437=CARTESIAN_POINT('Ctrl Pts',(-8.60770463405684,20.2895980329145,
4.06781373057032));
#106438=CARTESIAN_POINT('Ctrl Pts',(-8.76536985074856,20.3687532885863,
2.64175340769075));
#106439=CARTESIAN_POINT('Ctrl Pts',(-10.0471428779031,20.447908544258,1.99711066019015));
#106440=CARTESIAN_POINT('Ctrl Pts',(-11.2859931906797,20.5270637999298,
2.72082073168215));
#106441=CARTESIAN_POINT('Ctrl Pts',(-11.3539705981402,20.6062190556016,
4.15395904919404));
#106442=CARTESIAN_POINT('Ctrl Pts',(-10.1891829338672,20.6853743112733,
4.99167980350491));
#106443=CARTESIAN_POINT('Ctrl Pts',(-8.85214772348058,20.7645295669451,
4.47125381334657));
#106444=CARTESIAN_POINT('Ctrl Pts',(-8.56021068283754,20.8436848226168,
3.06651927282067));
#106445=CARTESIAN_POINT('Ctrl Pts',(-9.57917506301629,20.9228400782886,
2.05646087996767));
#106446=CARTESIAN_POINT('Ctrl Pts',(-10.9812927290496,21.0019953339603,
2.36071803377508));
#106447=CARTESIAN_POINT('Ctrl Pts',(-11.4899615984991,21.0811505896321,
3.70227024904624));
#106448=CARTESIAN_POINT('Ctrl Pts',(-10.6420481172114,21.1603058453039,
4.85965916090628));
#106449=CARTESIAN_POINT('Ctrl Pts',(-9.20956175497811,21.2394611009757,
4.77910367033238));
#106450=CARTESIAN_POINT('Ctrl Pts',(-8.49675472785286,21.3186163566474,
3.53394805470571));
#106451=CARTESIAN_POINT('Ctrl Pts',(-9.15262458949975,21.3977716123192,
2.25788336605189));
#106452=CARTESIAN_POINT('Ctrl Pts',(-10.5800140174839,21.4769268679909,
2.11274279307217));
#106453=CARTESIAN_POINT('Ctrl Pts',(-11.4793114596804,21.5560821236627,
3.23067413063488));
#106454=CARTESIAN_POINT('Ctrl Pts',(-11.0317233046461,21.6352373793345,
4.59382166796118));
#106455=CARTESIAN_POINT('Ctrl Pts',(-9.64477025098822,21.7143926350062,
4.96106490070361));
#106456=CARTESIAN_POINT('Ctrl Pts',(-8.58124728334842,21.793547890678,3.99803568912767));
#106457=CARTESIAN_POINT('Ctrl Pts',(-8.80947230264245,21.8727031463497,
2.58155423650846));
#106458=CARTESIAN_POINT('Ctrl Pts',(-10.1216506694092,21.9518584020216,
2.0013005860803));
#106459=CARTESIAN_POINT('Ctrl Pts',(-11.3230683620472,22.0310136576933,
2.78558490497384));
#106460=CARTESIAN_POINT('Ctrl Pts',(-11.3198568947254,22.1101689133651,
4.22033089347637));
#106461=CARTESIAN_POINT('Ctrl Pts',(-10.1149402487698,22.1893241690368,
4.99922898780111));
#106462=CARTESIAN_POINT('Ctrl Pts',(-8.80537264199095,22.2684794247086,
4.41310694562581));
#106463=CARTESIAN_POINT('Ctrl Pts',(-8.58349104753574,22.3476346803803,
2.99561799572498));
#106464=CARTESIAN_POINT('Ctrl Pts',(-9.65131453440758,22.4267899360521,
2.03735948889266));
#106465=CARTESIAN_POINT('Ctrl Pts',(-11.036609658852,22.5059451917238,2.41080799036886));
#106466=CARTESIAN_POINT('Ctrl Pts',(-11.4780909499422,22.5851004473957,
3.77594557855443));
#106467=CARTESIAN_POINT('Ctrl Pts',(-10.5737978952759,22.6642557030673,
4.88983984473576));
#106468=CARTESIAN_POINT('Ctrl Pts',(-9.1470725185231,22.7434109587392,4.73831075668277));
#106469=CARTESIAN_POINT('Ctrl Pts',(-8.49692176570142,22.8225662144109,
3.45932273340382));
#106470=CARTESIAN_POINT('Ctrl Pts',(-9.21529581654213,22.9017214700827,
2.21737060570834));
#106471=CARTESIAN_POINT('Ctrl Pts',(-10.6481284464643,22.9808767257544,
2.14322870890463));
#106472=CARTESIAN_POINT('Ctrl Pts',(-11.4908521677052,23.0600319814262,
3.30440186333547));
#106473=CARTESIAN_POINT('Ctrl Pts',(-10.9761826932751,23.139187237098,4.64366348566761));
#106474=CARTESIAN_POINT('Ctrl Pts',(-9.5727170114692,23.2183424927698,4.94164075671982));
#106475=CARTESIAN_POINT('Ctrl Pts',(-8.55828455800811,23.2974977484415,
3.92703090136812));
#106476=CARTESIAN_POINT('Ctrl Pts',(-8.8565072136684,23.3766530041133,2.52361735308531));
#106477=CARTESIAN_POINT('Ctrl Pts',(-10.1958588283679,23.455808259785,2.00918204713828));
#106478=CARTESIAN_POINT('Ctrl Pts',(-11.3568845728098,23.5349635154568,
2.85210881677446));
#106479=CARTESIAN_POINT('Ctrl Pts',(-11.2824922144306,23.6141187711285,
4.28492841263576));
#106480=CARTESIAN_POINT('Ctrl Pts',(-10.0404143544081,23.6932740268003,
5.00308538418801));
#106481=CARTESIAN_POINT('Ctrl Pts',(-8.76154030200664,23.772429282472,4.35271082947298));
#106482=CARTESIAN_POINT('Ctrl Pts',(-8.61026016699327,23.8515845381438,
2.92595931621431));
#106483=CARTESIAN_POINT('Ctrl Pts',(-9.72431352830351,23.9307397938156,
2.021860397494));
#106484=CARTESIAN_POINT('Ctrl Pts',(-11.0893719961529,24.0098950494874,
2.46358162164939));
#106485=CARTESIAN_POINT('Ctrl Pts',(-11.4625819213487,24.0890503051591,
3.84893964487562));
#106486=CARTESIAN_POINT('Ctrl Pts',(-10.5041297078297,24.1682055608308,
4.91660012344537));
#106487=CARTESIAN_POINT('Ctrl Pts',(-9.08669301949751,24.2473608165027,
4.69446192593765));
#106488=CARTESIAN_POINT('Ctrl Pts',(-8.50077418319726,24.3265160721744,
3.38480864326793));
#106489=CARTESIAN_POINT('Ctrl Pts',(-9.27993241209184,24.4056713278462,
2.1799960032324));
#106490=CARTESIAN_POINT('Ctrl Pts',(-10.7145840617594,24.4848265835179,
2.17709718484775));
#106491=CARTESIAN_POINT('Ctrl Pts',(-11.4988403047328,24.5639818391897,
3.3785334772474));
#106492=CARTESIAN_POINT('Ctrl Pts',(-10.9180079562998,24.6431370948615,
4.69083784983361));
#106493=CARTESIAN_POINT('Ctrl Pts',(-9.50215789159537,24.7222923505332,
4.91837746345501));
#106494=CARTESIAN_POINT('Ctrl Pts',(-8.5380149964364,24.801447606205,3.85553826190807));
#106495=CARTESIAN_POINT('Ctrl Pts',(-8.90815292823849,24.8806134012371,
2.46671618204897));
#106496=CARTESIAN_POINT('Ctrl Pts',(-9.81329627450407,24.9333941110454,
2.17142408334115));
#106497=CARTESIAN_POINT('Ctrl Pts',(-10.2288035547324,24.9597897356297,
2.24733102040164));
#106498=CARTESIAN_POINT('Ctrl Pts',(-9.31677294062166,13.3011804754291,
4.45676857688459));
#106499=CARTESIAN_POINT('Ctrl Pts',(-8.99946012149813,13.3275719245543,
4.2301849416717));
#106500=CARTESIAN_POINT('Ctrl Pts',(-8.61340256712811,13.3803484589035,
3.44058106103564));
#106501=CARTESIAN_POINT('Ctrl Pts',(-9.29581997813561,13.4595100784765,
2.30257873466078));
#106502=CARTESIAN_POINT('Ctrl Pts',(-10.6199487668489,13.5386653341483,
2.25830784636961));
#106503=CARTESIAN_POINT('Ctrl Pts',(-11.3792981896508,13.6178205898201,
3.34287441051017));
#106504=CARTESIAN_POINT('Ctrl Pts',(-10.8829932826216,13.6969758454918,
4.57137874334175));
#106505=CARTESIAN_POINT('Ctrl Pts',(-9.5826501964657,13.7761311011636,4.82395592551201));
#106506=CARTESIAN_POINT('Ctrl Pts',(-8.6623428589802,13.8552863568353,3.87133383357965));
#106507=CARTESIAN_POINT('Ctrl Pts',(-8.95992324759565,13.9344416125071,
2.58049512244971));
#106508=CARTESIAN_POINT('Ctrl Pts',(-10.2044868340536,14.0135968681788,
2.12691319402816));
#106509=CARTESIAN_POINT('Ctrl Pts',(-11.2628623678821,14.0927521238507,
2.9234675714814));
#106510=CARTESIAN_POINT('Ctrl Pts',(-11.1714286162047,14.1719073795224,
4.24496159082084));
#106511=CARTESIAN_POINT('Ctrl Pts',(-10.0134290845659,14.2510626351942,
4.88817275967509));
#106512=CARTESIAN_POINT('Ctrl Pts',(-8.84320355465755,14.3302178908659,
4.26748320171483));
#106513=CARTESIAN_POINT('Ctrl Pts',(-8.72621920724741,14.4093731465377,
2.94801195840054));
#106514=CARTESIAN_POINT('Ctrl Pts',(-9.76898885752458,14.4885284022094,
2.13111686903091));
#106515=CARTESIAN_POINT('Ctrl Pts',(-11.0220897283542,14.5676836578812,
2.56056375852433));
#106516=CARTESIAN_POINT('Ctrl Pts',(-11.3445969617449,14.646838913553,3.84535024329455));
#106517=CARTESIAN_POINT('Ctrl Pts',(-10.4428736092137,14.7259941692247,
4.81570156445467));
#106518=CARTESIAN_POINT('Ctrl Pts',(-9.13792208319002,14.8051494248965,
4.58813115389582));
#106519=CARTESIAN_POINT('Ctrl Pts',(-8.61787647254162,14.8843046805683,
3.36983749607252));
#106520=CARTESIAN_POINT('Ctrl Pts',(-9.35622865776133,14.96345993624,2.27005440561813));
#106521=CARTESIAN_POINT('Ctrl Pts',(-10.680722685639,15.0426151919118,2.29011391187054));
#106522=CARTESIAN_POINT('Ctrl Pts',(-11.3854313580073,15.1217704475836,
3.41175222778377));
#106523=CARTESIAN_POINT('Ctrl Pts',(-10.8287305206277,15.2009257032553,
4.61373849689104));
#106524=CARTESIAN_POINT('Ctrl Pts',(-9.51748594307886,15.2800809589271,
4.80168656067022));
#106525=CARTESIAN_POINT('Ctrl Pts',(-8.64556144865758,15.3592362145988,
3.80447319634858));
#106526=CARTESIAN_POINT('Ctrl Pts',(-9.00682808876778,15.4383914702706,
2.53004264463413));
#106527=CARTESIAN_POINT('Ctrl Pts',(-10.2723593000609,15.5175467259424,
2.13874024211219));
#106528=CARTESIAN_POINT('Ctrl Pts',(-11.2899124293335,15.5967019816141,
2.98683955597768));
#106529=CARTESIAN_POINT('Ctrl Pts',(-11.1330242593036,15.6758572372859,
4.30216191911361));
#106530=CARTESIAN_POINT('Ctrl Pts',(-9.94453855369621,15.7550124929577,
4.88713075975507));
#106531=CARTESIAN_POINT('Ctrl Pts',(-8.80654946442569,15.8341677486294,
4.20914281763525));
#106532=CARTESIAN_POINT('Ctrl Pts',(-8.75517491251764,15.9133230043012,
2.88549351651843));
#106533=CARTESIAN_POINT('Ctrl Pts',(-9.83719047290022,15.9924782599729,
2.12134095057665));
#106534=CARTESIAN_POINT('Ctrl Pts',(-11.0674410825746,16.0716335156447,
2.61243183253307));
#106535=CARTESIAN_POINT('Ctrl Pts',(-11.3258064204865,16.1507887713165,
3.91163703922939));
#106536=CARTESIAN_POINT('Ctrl Pts',(-10.3770496471056,16.2299440269882,
4.83605437025856));
#106537=CARTESIAN_POINT('Ctrl Pts',(-9.08499617592348,16.30909928266,4.54401902214198));
#106538=CARTESIAN_POINT('Ctrl Pts',(-8.62603668504912,16.3882545383318,
3.30142375308653));
#106539=CARTESIAN_POINT('Ctrl Pts',(-9.41804526308345,16.4674097940035,
2.23962846713776));
#106540=CARTESIAN_POINT('Ctrl Pts',(-10.7399128158888,16.5465650496753,
2.32537804313361));
#106541=CARTESIAN_POINT('Ctrl Pts',(-11.3881034980083,16.625720305347,3.48059908542653));
#106542=CARTESIAN_POINT('Ctrl Pts',(-10.7724517372814,16.7048755610188,
4.65348429995384));
#106543=CARTESIAN_POINT('Ctrl Pts',(-9.45349702254033,16.7840308166906,
4.77614349204813));
#106544=CARTESIAN_POINT('Ctrl Pts',(-8.6321231143072,16.8631860723623,3.73689774641489));
#106545=CARTESIAN_POINT('Ctrl Pts',(-9.05617569423413,16.9423413280341,
2.4819610044234));
#106546=CARTESIAN_POINT('Ctrl Pts',(-10.3395627675389,17.0214965837059,
2.15392985191321));
#106547=CARTESIAN_POINT('Ctrl Pts',(-11.3137842503515,17.1006518393776,
3.05147055815968));
#106548=CARTESIAN_POINT('Ctrl Pts',(-11.0918295843972,17.1798070950494,
4.35738898716052));
#106549=CARTESIAN_POINT('Ctrl Pts',(-9.87578436892954,17.2589623507211,
4.88267067433529));
#106550=CARTESIAN_POINT('Ctrl Pts',(-8.77283517752426,17.3381176063929,
4.14905640367165));
#106551=CARTESIAN_POINT('Ctrl Pts',(-8.78719675526428,17.4172728620647,
2.82448833745998));
#106552=CARTESIAN_POINT('Ctrl Pts',(-9.90579315246707,17.4964281177364,
2.11496108843579));
#106553=CARTESIAN_POINT('Ctrl Pts',(-11.1101631339089,17.5755833734082,
2.66648603324317));
#106554=CARTESIAN_POINT('Ctrl Pts',(-11.3037502096591,17.6547386290799,
3.97690995741632));
#106555=CARTESIAN_POINT('Ctrl Pts',(-10.3102969442523,17.7338938847517,
4.85311622673618));
#106556=CARTESIAN_POINT('Ctrl Pts',(-9.03432407667294,17.8130491404235,
4.49733531361096));
#106557=CARTESIAN_POINT('Ctrl Pts',(-8.63758119424006,17.8922043960953,
3.23349912874295));
#106558=CARTESIAN_POINT('Ctrl Pts',(-9.48129531960395,17.971359651767,2.21230703535186));
#106559=CARTESIAN_POINT('Ctrl Pts',(-10.7972804185142,18.0505149074388,
2.36353545989204));
#106560=CARTESIAN_POINT('Ctrl Pts',(-11.387356510485,18.1296701631105,3.54949373176654));
#106561=CARTESIAN_POINT('Ctrl Pts',(-10.7142702778696,18.2088254187823,
4.69038888050132));
#106562=CARTESIAN_POINT('Ctrl Pts',(-9.39085422897575,18.2879806744541,
4.74745707193165));
#106563=CARTESIAN_POINT('Ctrl Pts',(-8.62205408617643,18.3671359301258,
3.66873877813356));
#106564=CARTESIAN_POINT('Ctrl Pts',(-9.10784809455951,18.4462911857976,
2.43638696214837));
#106565=CARTESIAN_POINT('Ctrl Pts',(-10.4059298359393,18.5254464414694,
2.17243505433318));
#106566=CARTESIAN_POINT('Ctrl Pts',(-11.3344200042023,18.6046016971411,
3.11720636231295));
#106567=CARTESIAN_POINT('Ctrl Pts',(-11.0479455532464,18.6837569528129,
4.41050416479016));
#106568=CARTESIAN_POINT('Ctrl Pts',(-9.80733614773888,18.7629122084847,
4.87480484313264));
#106569=CARTESIAN_POINT('Ctrl Pts',(-8.74214359986434,18.8420674641564,
4.08737125679317));
#106570=CARTESIAN_POINT('Ctrl Pts',(-8.82220593232,18.9212227198282,2.76514705497843));
#106571=CARTESIAN_POINT('Ctrl Pts',(-9.97462787902816,19.0003779754999,
2.11199280544139));
#106572=CARTESIAN_POINT('Ctrl Pts',(-11.1501506704466,19.0795332311717,
2.72259331624922));
#106573=CARTESIAN_POINT('Ctrl Pts',(-11.2784826471567,19.1586884868435,
4.0410081677647));
#106574=CARTESIAN_POINT('Ctrl Pts',(-10.2427799288765,19.2378437425152,
4.86684513490147));
#106575=CARTESIAN_POINT('Ctrl Pts',(-8.98603059640236,19.316998998187,4.44819500380294));
#106576=CARTESIAN_POINT('Ctrl Pts',(-8.65248156552903,19.3961542538588,
3.16623093997496));
#106577=CARTESIAN_POINT('Ctrl Pts',(-9.54582303125486,19.4753095095305,
2.18815740359959));
#106578=CARTESIAN_POINT('Ctrl Pts',(-10.8526841880462,19.5544647652023,
2.40449217614617));
#106579=CARTESIAN_POINT('Ctrl Pts',(-11.3831922351862,19.6336200208741,
3.6182664668867));
#106580=CARTESIAN_POINT('Ctrl Pts',(-10.6543294530239,19.7127752765458,
4.7243613370139));
#106581=CARTESIAN_POINT('Ctrl Pts',(-9.32971186185602,19.7919305322176,
4.71569795941777));
#106582=CARTESIAN_POINT('Ctrl Pts',(-8.61537916597029,19.8710857878893,
3.60016417842699));
#106583=CARTESIAN_POINT('Ctrl Pts',(-9.16171801208923,19.9502410435611,
2.39343277411021));
#106584=CARTESIAN_POINT('Ctrl Pts',(-10.4712970322408,20.0293962992329,
2.19421026804849));
#106585=CARTESIAN_POINT('Ctrl Pts',(-11.3517688616188,20.1085515549046,
3.18388505029508));
#106586=CARTESIAN_POINT('Ctrl Pts',(-11.0014802594559,20.1877068105764,
4.46137662057556));
#106587=CARTESIAN_POINT('Ctrl Pts',(-9.73936248937481,20.2668620662481,
4.86355264098023));
#106588=CARTESIAN_POINT('Ctrl Pts',(-8.71455032986141,20.34601732192,4.02423931768769));
#106589=CARTESIAN_POINT('Ctrl Pts',(-8.86011621031052,20.4251725775915,
2.70761583643271));
#106590=CARTESIAN_POINT('Ctrl Pts',(-10.0435251013056,20.5043278332634,
2.11244341296457));
#106591=CARTESIAN_POINT('Ctrl Pts',(-11.1873051962935,20.5834830889351,
2.78061548006411));
#106592=CARTESIAN_POINT('Ctrl Pts',(-11.250065971151,20.6626383446069,4.10377378581674));
#106593=CARTESIAN_POINT('Ctrl Pts',(-10.1746649065162,20.7417936002788,
4.87720727819045));
#106594=CARTESIAN_POINT('Ctrl Pts',(-8.94023468991426,20.8209488559505,
4.39671913340127));
#106595=CARTESIAN_POINT('Ctrl Pts',(-8.67070109684536,20.9001041116222,
3.09978487941987));
#106596=CARTESIAN_POINT('Ctrl Pts',(-9.61146945564575,20.979259367294,2.16723905640477));
#106597=CARTESIAN_POINT('Ctrl Pts',(-10.9059876558676,21.0584146229658,
2.44814730875257));
#106598=CARTESIAN_POINT('Ctrl Pts',(-11.3756209294084,21.1375698786376,
3.68674789220404));
#106599=CARTESIAN_POINT('Ctrl Pts',(-10.5927769068766,21.2167251343092,
4.75531798973122));
#106600=CARTESIAN_POINT('Ctrl Pts',(-9.27022052490997,21.2958803899811,
4.68094438243568));
#106601=CARTESIAN_POINT('Ctrl Pts',(-8.61211479511756,21.3750356456528,
3.53134285783803));
#106602=CARTESIAN_POINT('Ctrl Pts',(-9.2176527563365,21.4541909013246,2.35320424355459));
#106603=CARTESIAN_POINT('Ctrl Pts',(-10.5355033462641,21.5333461569963,
2.21920185711835));
#106604=CARTESIAN_POINT('Ctrl Pts',(-11.3657880895052,21.6125014126681,
3.25134238150634));
#106605=CARTESIAN_POINT('Ctrl Pts',(-10.9525481547035,21.6916566683399,
4.50988104727235));
#106606=CARTESIAN_POINT('Ctrl Pts',(-9.67203082416259,21.7708119240117,
4.84894178390677));
#106607=CARTESIAN_POINT('Ctrl Pts',(-8.69012333428795,21.8499671796834,
3.95981609072778));
#106608=CARTESIAN_POINT('Ctrl Pts',(-8.90083420997211,21.9291224353551,
2.65203639069745));
#106609=CARTESIAN_POINT('Ctrl Pts',(-10.1123151140836,22.0082776910269,
2.11631180108475));
#106610=CARTESIAN_POINT('Ctrl Pts',(-11.2215351937282,22.0874329466986,
2.84040960653396));
#106611=CARTESIAN_POINT('Ctrl Pts',(-11.2185701765987,22.1665882023705,
4.16505220950913));
#106612=CARTESIAN_POINT('Ctrl Pts',(-10.1061196557001,22.2457434580421,
4.88417713293588));
#106613=CARTESIAN_POINT('Ctrl Pts',(-8.89704916007462,22.324898713714,4.34303449596042));
#106614=CARTESIAN_POINT('Ctrl Pts',(-8.69219491048146,22.4040539693857,
3.0343246146769));
#106615=CARTESIAN_POINT('Ctrl Pts',(-9.67807289480975,22.4832092250576,
2.14960351910631));
#106616=CARTESIAN_POINT('Ctrl Pts',(-10.9570595267557,22.5623644807292,
2.49439332792044));
#106617=CARTESIAN_POINT('Ctrl Pts',(-11.3646612425165,22.6415197364011,
3.7547693266857));
#106618=CARTESIAN_POINT('Ctrl Pts',(-10.5297642535131,22.7206749920728,
4.78318258730308));
#106619=CARTESIAN_POINT('Ctrl Pts',(-9.21252675507264,22.7998302477446,
4.64328194479669));
#106620=CARTESIAN_POINT('Ctrl Pts',(-8.6122690143677,22.8789855034163,3.4624443345807));
#106621=CARTESIAN_POINT('Ctrl Pts',(-9.27551455067946,22.958140759088,2.31580046006593));
#106622=CARTESIAN_POINT('Ctrl Pts',(-10.5983906275165,23.0372960147598,
2.24734826298114));
#106623=CARTESIAN_POINT('Ctrl Pts',(-11.3764431557264,23.1164512704317,
3.3194121977237));
#106624=CARTESIAN_POINT('Ctrl Pts',(-10.9012697677231,23.1956065261034,
4.55589796990028));
#106625=CARTESIAN_POINT('Ctrl Pts',(-9.60550699937822,23.2747617817751,
4.83100826197783));
#106626=CARTESIAN_POINT('Ctrl Pts',(-8.66892278414878,23.3539170374469,
3.89426025879988));
#106627=CARTESIAN_POINT('Ctrl Pts',(-8.94425962985228,23.4330722931186,
2.59854562321601));
#106628=CARTESIAN_POINT('Ctrl Pts',(-10.1808284883205,23.5122275487905,
2.12358843344668));
#106629=CARTESIAN_POINT('Ctrl Pts',(-11.2527563254173,23.591382804462,2.90182842797959));
#106630=CARTESIAN_POINT('Ctrl Pts',(-11.1840728873491,23.670538060134,4.22469247099844));
#106631=CARTESIAN_POINT('Ctrl Pts',(-10.0373129292917,23.7496933158057,
4.88773758683433));
#106632=CARTESIAN_POINT('Ctrl Pts',(-8.85658054375048,23.8288485714775,
4.28727321894597));
#106633=CARTESIAN_POINT('Ctrl Pts',(-8.71690974945766,23.9080038271492,
2.97001158973293));
#106634=CARTESIAN_POINT('Ctrl Pts',(-9.74546989613527,23.9871590828211,
2.13529383855059));
#106635=CARTESIAN_POINT('Ctrl Pts',(-11.0057728463129,24.0663143384927,
2.54311707474954));
#106636=CARTESIAN_POINT('Ctrl Pts',(-11.3503423873531,24.1454695941646,
3.82216177858194));
#106637=CARTESIAN_POINT('Ctrl Pts',(-10.465442450279,24.2246248498363,4.80788926397637));
#106638=CARTESIAN_POINT('Ctrl Pts',(-9.15678081997574,24.3037801055081,
4.60279810322396));
#106639=CARTESIAN_POINT('Ctrl Pts',(-8.61582579471792,24.3829353611798,
3.39364850653384));
#106640=CARTESIAN_POINT('Ctrl Pts',(-9.33519088981022,24.4620906168515,
2.28129401007015));
#106641=CARTESIAN_POINT('Ctrl Pts',(-10.6597463935769,24.5412458725233,
2.27861764898507));
#106642=CARTESIAN_POINT('Ctrl Pts',(-11.3838182776712,24.620401128195,3.38785490103285));
#106643=CARTESIAN_POINT('Ctrl Pts',(-10.8475593997332,24.6995563838669,
4.59945214119144));
#106644=CARTESIAN_POINT('Ctrl Pts',(-9.54036263447855,24.7787116395386,
4.80953020970168));
#106645=CARTESIAN_POINT('Ctrl Pts',(-8.65020872255413,24.8578668952104,
3.82825401324364));
#106646=CARTESIAN_POINT('Ctrl Pts',(-8.99194201706846,24.9370326902426,
2.54601108684658));
#106647=CARTESIAN_POINT('Ctrl Pts',(-9.82762404571402,24.9898134000508,
2.27337990515665));
#106648=CARTESIAN_POINT('Ctrl Pts',(-10.2112450139185,25.0162090246351,
2.3434616921053));
#106649=CARTESIAN_POINT('Ctrl Pts',(-9.36563614293035,13.3013173138078,
2.18112163397617));
#106650=CARTESIAN_POINT('Ctrl Pts',(-9.36179253662721,13.301100711406,2.18297352663203));
#106651=CARTESIAN_POINT('Ctrl Pts',(-9.35795682031215,13.3008830480983,
2.18484156183112));
#106652=CARTESIAN_POINT('Ctrl Pts',(-9.35027234948581,13.3004438276433,
2.18862405105439));
#106653=CARTESIAN_POINT('Ctrl Pts',(-9.34643267341032,13.3002227704914,
2.19053427774748));
#106654=CARTESIAN_POINT('Ctrl Pts',(-9.34259215682144,13.3,2.1924652288649));
#106655=CARTESIAN_POINT('Origin',(-10.,13.3,3.5));
#106656=CARTESIAN_POINT('',(-10.,13.2,5.0635));
#106657=CARTESIAN_POINT('Origin',(-10.,13.2,3.5));
#106658=CARTESIAN_POINT('Origin',(-10.,13.3,5.0635));
#106659=CARTESIAN_POINT('Origin',(-10.,13.2,3.5));
#106660=CARTESIAN_POINT('',(-10.,13.2,0.95));
#106661=CARTESIAN_POINT('Origin',(-10.,13.2,3.5));
#106662=CARTESIAN_POINT('Origin',(-10.,25.025,3.5));
#106663=CARTESIAN_POINT('',(-11.1135,25.2,3.5));
#106664=CARTESIAN_POINT('',(-11.2885,25.025,3.5));
#106665=CARTESIAN_POINT('Origin',(-10.,25.2,3.5));
#106666=CARTESIAN_POINT('Origin',(-10.,25.2,3.5));
#106667=CARTESIAN_POINT('Origin',(-7.21791809774051,12.6,3.99055610190908));
#106668=CARTESIAN_POINT('',(-7.30151407930766,12.6,4.02978650022929));
#106669=CARTESIAN_POINT('',(-7.28305503829031,12.6,3.92510007650003));
#106670=CARTESIAN_POINT('Origin',(-10.,12.6,3.5));
#106671=CARTESIAN_POINT('',(-7.43949984216826,12.6,3.95148526193402));
#106672=CARTESIAN_POINT('',(-7.02412006173947,12.6,4.18719618236609));
#106673=CARTESIAN_POINT('',(-7.43949984216826,12.6,3.95148526193402));
#106674=CARTESIAN_POINT('Origin',(-6.96855264488606,10.2,3.87205770140218));
#106675=CARTESIAN_POINT('',(-7.28305503829031,10.5,3.92510007650003));
#106676=CARTESIAN_POINT('',(-7.28305503829031,13.2,3.92510007650003));
#106677=CARTESIAN_POINT('',(-7.43949984216826,10.35,3.95148526193402));
#106678=CARTESIAN_POINT('',(-7.43949984216826,10.2,3.95148526193402));
#106679=CARTESIAN_POINT('Ctrl Pts',(-7.28305503829031,10.5,3.92510007650003));
#106680=CARTESIAN_POINT('Ctrl Pts',(-7.36347059168573,10.422647555638,3.93866255499417));
#106681=CARTESIAN_POINT('Ctrl Pts',(-7.43949984216826,10.35,3.95148526193402));
#106682=CARTESIAN_POINT('Origin',(-7.43949984216826,10.2,3.95148526193402));
#106683=CARTESIAN_POINT('',(-7.30151407930766,10.5,4.02978650022929));
#106684=CARTESIAN_POINT('',(-7.30151407930766,13.2,4.02978650022929));
#106685=CARTESIAN_POINT('Ctrl Pts',(-7.43949984216826,10.35,3.95148526193402));
#106686=CARTESIAN_POINT('Ctrl Pts',(-7.37244134059122,10.4226475556382,
3.98953820017093));
#106687=CARTESIAN_POINT('Ctrl Pts',(-7.30151407930766,10.5,4.0297865002293));
#106688=CARTESIAN_POINT('Origin',(-10.,13.2,3.5));
#106689=CARTESIAN_POINT('',(-12.7494863164095,12.6,3.44684930972108));
#106690=CARTESIAN_POINT('',(-12.75,12.6,3.5));
#106691=CARTESIAN_POINT('Origin',(-10.,12.6,3.5));
#106692=CARTESIAN_POINT('',(-12.75,13.,3.5));
#106693=CARTESIAN_POINT('',(-12.75,13.2,3.5));
#106694=CARTESIAN_POINT('',(-10.,13.,0.75));
#106695=CARTESIAN_POINT('Origin',(-10.,13.,3.5));
#106696=CARTESIAN_POINT('Origin',(-10.,13.,3.5));
#106697=CARTESIAN_POINT('',(-12.7494863164095,12.6,3.55315069027892));
#106698=CARTESIAN_POINT('Origin',(-10.,12.6,3.5));
#106699=CARTESIAN_POINT('',(-12.7494863164095,10.5,3.55315069027892));
#106700=CARTESIAN_POINT('',(-12.7494863164095,13.2,3.55315069027892));
#106701=CARTESIAN_POINT('',(-12.7169449617097,10.5,3.92510007650003));
#106702=CARTESIAN_POINT('Origin',(-10.,10.5,3.5));
#106703=CARTESIAN_POINT('',(-12.7169449617097,12.6,3.92510007650003));
#106704=CARTESIAN_POINT('',(-12.7169449617097,13.2,3.92510007650003));
#106705=CARTESIAN_POINT('',(-12.6984859206923,12.6,4.0297865002293));
#106706=CARTESIAN_POINT('Origin',(-10.,12.6,3.5));
#106707=CARTESIAN_POINT('',(-12.6984859206923,10.5,4.02978650022929));
#106708=CARTESIAN_POINT('',(-12.6984859206923,13.2,4.02978650022929));
#106709=CARTESIAN_POINT('',(-12.6018506091889,10.5,4.39043439256555));
#106710=CARTESIAN_POINT('Origin',(-10.,10.5,3.5));
#106711=CARTESIAN_POINT('',(-12.6018506091889,12.6,4.39043439256555));
#106712=CARTESIAN_POINT('',(-12.6018506091889,13.2,4.39043439256555));
#106713=CARTESIAN_POINT('',(-12.5654933957747,12.6,4.49032501545511));
#106714=CARTESIAN_POINT('Origin',(-10.,12.6,3.5));
#106715=CARTESIAN_POINT('',(-12.5654933957747,10.5,4.49032501545511));
#106716=CARTESIAN_POINT('',(-12.5654933957747,13.2,4.49032501545511));
#106717=CARTESIAN_POINT('',(-12.4077003425078,10.5,4.82871331019451));
#106718=CARTESIAN_POINT('Origin',(-10.,10.5,3.5));
#106719=CARTESIAN_POINT('',(-12.4077003425078,12.6,4.82871331019451));
#106720=CARTESIAN_POINT('',(-12.4077003425078,13.2,4.82871331019451));
#106721=CARTESIAN_POINT('',(-12.3545496522288,12.6,4.92077300621495));
#106722=CARTESIAN_POINT('Origin',(-10.,12.6,3.5));
#106723=CARTESIAN_POINT('',(-12.3545496522288,10.5,4.92077300621495));
#106724=CARTESIAN_POINT('',(-12.3545496522288,13.2,4.92077300621495));
#106725=CARTESIAN_POINT('',(-12.1403933192747,10.5,5.22661994625458));
#106726=CARTESIAN_POINT('Origin',(-10.,10.5,3.5));
#106727=CARTESIAN_POINT('',(-12.1403933192747,12.6,5.22661994625458));
#106728=CARTESIAN_POINT('',(-12.1403933192747,13.2,5.22661994625458));
#106729=CARTESIAN_POINT('',(-12.0720641089596,12.6,5.30805152812679));
#106730=CARTESIAN_POINT('Origin',(-10.,12.6,3.5));
#106731=CARTESIAN_POINT('',(-12.0720641089596,10.5,5.30805152812679));
#106732=CARTESIAN_POINT('',(-12.0720641089596,13.2,5.30805152812679));
#106733=CARTESIAN_POINT('',(-11.8080515281268,10.5,5.57206410895956));
#106734=CARTESIAN_POINT('Origin',(-10.,10.5,3.5));
#106735=CARTESIAN_POINT('',(-11.8080515281268,12.6,5.57206410895956));
#106736=CARTESIAN_POINT('',(-11.8080515281268,13.2,5.57206410895956));
#106737=CARTESIAN_POINT('',(-11.7266199462546,12.6,5.64039331927471));
#106738=CARTESIAN_POINT('Origin',(-10.,12.6,3.5));
#106739=CARTESIAN_POINT('',(-11.7266199462546,10.5,5.64039331927471));
#106740=CARTESIAN_POINT('',(-11.7266199462546,13.2,5.64039331927471));
#106741=CARTESIAN_POINT('',(-11.420773006215,10.5,5.85454965222883));
#106742=CARTESIAN_POINT('Origin',(-10.,10.5,3.5));
#106743=CARTESIAN_POINT('',(-11.420773006215,12.6,5.85454965222883));
#106744=CARTESIAN_POINT('',(-11.420773006215,13.2,5.85454965222883));
#106745=CARTESIAN_POINT('',(-11.3287133101945,12.6,5.90770034250775));
#106746=CARTESIAN_POINT('Origin',(-10.,12.6,3.5));
#106747=CARTESIAN_POINT('',(-11.3287133101945,10.5,5.90770034250775));
#106748=CARTESIAN_POINT('',(-11.3287133101945,13.2,5.90770034250775));
#106749=CARTESIAN_POINT('',(-10.9903250154551,10.5,6.06549339577475));
#106750=CARTESIAN_POINT('Origin',(-10.,10.5,3.5));
#106751=CARTESIAN_POINT('',(-10.9903250154551,12.6,6.06549339577475));
#106752=CARTESIAN_POINT('',(-10.9903250154551,13.2,6.06549339577475));
#106753=CARTESIAN_POINT('',(-10.8904343925656,12.6,6.10185060918885));
#106754=CARTESIAN_POINT('Origin',(-10.,12.6,3.5));
#106755=CARTESIAN_POINT('',(-10.8904343925656,10.5,6.10185060918885));
#106756=CARTESIAN_POINT('',(-10.8904343925656,13.2,6.10185060918885));
#106757=CARTESIAN_POINT('',(-10.5297865002293,10.5,6.19848592069234));
#106758=CARTESIAN_POINT('Origin',(-10.,10.5,3.5));
#106759=CARTESIAN_POINT('',(-10.5297865002293,12.6,6.19848592069234));
#106760=CARTESIAN_POINT('',(-10.5297865002293,13.2,6.19848592069234));
#106761=CARTESIAN_POINT('',(-10.4251000765,12.6,6.21694496170969));
#106762=CARTESIAN_POINT('Origin',(-10.,12.6,3.5));
#106763=CARTESIAN_POINT('',(-10.4251000765,10.5,6.21694496170969));
#106764=CARTESIAN_POINT('',(-10.4251000765,13.2,6.21694496170969));
#106765=CARTESIAN_POINT('',(-10.0531506902789,10.5,6.24948631640946));
#106766=CARTESIAN_POINT('Origin',(-10.,10.5,3.5));
#106767=CARTESIAN_POINT('',(-10.0531506902789,12.6,6.24948631640946));
#106768=CARTESIAN_POINT('',(-10.0531506902789,13.2,6.24948631640946));
#106769=CARTESIAN_POINT('',(-9.94684930972108,12.6,6.24948631640946));
#106770=CARTESIAN_POINT('Origin',(-10.,12.6,3.5));
#106771=CARTESIAN_POINT('',(-9.94684930972108,10.5,6.24948631640946));
#106772=CARTESIAN_POINT('',(-9.94684930972108,13.2,6.24948631640946));
#106773=CARTESIAN_POINT('',(-9.57489992349997,10.5,6.21694496170969));
#106774=CARTESIAN_POINT('Origin',(-10.,10.5,3.5));
#106775=CARTESIAN_POINT('',(-9.57489992349997,12.6,6.21694496170969));
#106776=CARTESIAN_POINT('',(-9.57489992349997,13.2,6.21694496170969));
#106777=CARTESIAN_POINT('',(-9.47021349977071,12.6,6.19848592069234));
#106778=CARTESIAN_POINT('Origin',(-10.,12.6,3.5));
#106779=CARTESIAN_POINT('',(-9.47021349977071,10.5,6.19848592069234));
#106780=CARTESIAN_POINT('',(-9.47021349977071,13.2,6.19848592069234));
#106781=CARTESIAN_POINT('',(-9.10956560743445,10.5,6.10185060918886));
#106782=CARTESIAN_POINT('Origin',(-10.,10.5,3.5));
#106783=CARTESIAN_POINT('',(-9.10956560743445,12.6,6.10185060918886));
#106784=CARTESIAN_POINT('',(-9.10956560743445,13.2,6.10185060918886));
#106785=CARTESIAN_POINT('',(-9.0096749845449,12.6,6.06549339577475));
#106786=CARTESIAN_POINT('Origin',(-10.,12.6,3.5));
#106787=CARTESIAN_POINT('',(-9.0096749845449,10.5,6.06549339577475));
#106788=CARTESIAN_POINT('',(-9.0096749845449,13.2,6.06549339577475));
#106789=CARTESIAN_POINT('',(-8.67128668980549,10.5,5.90770034250775));
#106790=CARTESIAN_POINT('Origin',(-10.,10.5,3.5));
#106791=CARTESIAN_POINT('',(-8.67128668980549,12.6,5.90770034250775));
#106792=CARTESIAN_POINT('',(-8.67128668980549,13.2,5.90770034250775));
#106793=CARTESIAN_POINT('',(-8.57922699378505,12.6,5.85454965222883));
#106794=CARTESIAN_POINT('Origin',(-10.,12.6,3.5));
#106795=CARTESIAN_POINT('',(-8.57922699378505,10.5,5.85454965222883));
#106796=CARTESIAN_POINT('',(-8.57922699378505,13.2,5.85454965222883));
#106797=CARTESIAN_POINT('',(-8.27338005374542,10.5,5.64039331927471));
#106798=CARTESIAN_POINT('Origin',(-10.,10.5,3.5));
#106799=CARTESIAN_POINT('',(-8.27338005374542,12.6,5.64039331927471));
#106800=CARTESIAN_POINT('',(-8.27338005374542,13.2,5.64039331927471));
#106801=CARTESIAN_POINT('',(-8.19194847187321,12.6,5.57206410895956));
#106802=CARTESIAN_POINT('Origin',(-10.,12.6,3.5));
#106803=CARTESIAN_POINT('',(-8.19194847187321,10.5,5.57206410895956));
#106804=CARTESIAN_POINT('',(-8.19194847187321,13.2,5.57206410895956));
#106805=CARTESIAN_POINT('',(-7.92793589104044,10.5,5.30805152812679));
#106806=CARTESIAN_POINT('Origin',(-10.,10.5,3.5));
#106807=CARTESIAN_POINT('',(-7.92793589104044,12.6,5.30805152812679));
#106808=CARTESIAN_POINT('',(-7.92793589104044,13.2,5.30805152812679));
#106809=CARTESIAN_POINT('',(-7.85960668072529,12.6,5.22661994625458));
#106810=CARTESIAN_POINT('Origin',(-10.,12.6,3.5));
#106811=CARTESIAN_POINT('',(-7.85960668072529,10.5,5.22661994625458));
#106812=CARTESIAN_POINT('',(-7.85960668072529,13.2,5.22661994625458));
#106813=CARTESIAN_POINT('',(-7.64545034777117,10.5,4.92077300621495));
#106814=CARTESIAN_POINT('Origin',(-10.,10.5,3.5));
#106815=CARTESIAN_POINT('',(-7.64545034777117,12.6,4.92077300621495));
#106816=CARTESIAN_POINT('',(-7.64545034777117,13.2,4.92077300621495));
#106817=CARTESIAN_POINT('',(-7.59229965749225,12.6,4.82871331019451));
#106818=CARTESIAN_POINT('Origin',(-10.,12.6,3.5));
#106819=CARTESIAN_POINT('',(-7.59229965749225,10.5,4.82871331019451));
#106820=CARTESIAN_POINT('',(-7.59229965749225,13.2,4.82871331019451));
#106821=CARTESIAN_POINT('',(-7.43450660422526,10.5,4.49032501545511));
#106822=CARTESIAN_POINT('Origin',(-10.,10.5,3.5));
#106823=CARTESIAN_POINT('',(-7.43450660422526,12.6,4.49032501545511));
#106824=CARTESIAN_POINT('',(-7.43450660422526,13.2,4.49032501545511));
#106825=CARTESIAN_POINT('',(-7.39814939081115,12.6,4.39043439256555));
#106826=CARTESIAN_POINT('Origin',(-10.,12.6,3.5));
#106827=CARTESIAN_POINT('',(-7.39814939081115,10.5,4.39043439256555));
#106828=CARTESIAN_POINT('',(-7.39814939081115,13.2,4.39043439256555));
#106829=CARTESIAN_POINT('Origin',(-10.,10.5,3.5));
#106830=CARTESIAN_POINT('',(-7.25051368359054,10.5,3.55315069027892));
#106831=CARTESIAN_POINT('Origin',(-10.,10.5,3.5));
#106832=CARTESIAN_POINT('',(-7.25051368359054,12.6,3.55315069027892));
#106833=CARTESIAN_POINT('',(-7.25051368359054,13.2,3.55315069027892));
#106834=CARTESIAN_POINT('',(-7.25051368359054,12.6,3.44684930972108));
#106835=CARTESIAN_POINT('Origin',(-10.,12.6,3.5));
#106836=CARTESIAN_POINT('',(-7.25051368359054,10.5,3.44684930972108));
#106837=CARTESIAN_POINT('',(-7.25051368359054,13.2,3.44684930972108));
#106838=CARTESIAN_POINT('',(-7.28305503829031,10.5,3.07489992349997));
#106839=CARTESIAN_POINT('Origin',(-10.,10.5,3.5));
#106840=CARTESIAN_POINT('',(-7.28305503829031,12.6,3.07489992349997));
#106841=CARTESIAN_POINT('',(-7.28305503829031,13.2,3.07489992349997));
#106842=CARTESIAN_POINT('',(-7.30151407930766,12.6,2.9702134997707));
#106843=CARTESIAN_POINT('Origin',(-10.,12.6,3.5));
#106844=CARTESIAN_POINT('',(-7.30151407930766,10.5,2.9702134997707));
#106845=CARTESIAN_POINT('',(-7.30151407930766,13.2,2.9702134997707));
#106846=CARTESIAN_POINT('',(-7.39814939081114,10.5,2.60956560743445));
#106847=CARTESIAN_POINT('Origin',(-10.,10.5,3.5));
#106848=CARTESIAN_POINT('',(-7.39814939081114,12.6,2.60956560743445));
#106849=CARTESIAN_POINT('',(-7.39814939081114,13.2,2.60956560743445));
#106850=CARTESIAN_POINT('',(-7.43450660422525,12.6,2.50967498454489));
#106851=CARTESIAN_POINT('Origin',(-10.,12.6,3.5));
#106852=CARTESIAN_POINT('',(-7.43450660422525,10.5,2.50967498454489));
#106853=CARTESIAN_POINT('',(-7.43450660422525,13.2,2.50967498454489));
#106854=CARTESIAN_POINT('',(-7.59229965749225,10.5,2.17128668980549));
#106855=CARTESIAN_POINT('Origin',(-10.,10.5,3.5));
#106856=CARTESIAN_POINT('',(-7.59229965749225,12.6,2.17128668980549));
#106857=CARTESIAN_POINT('',(-7.59229965749225,13.2,2.17128668980549));
#106858=CARTESIAN_POINT('',(-7.64545034777117,12.6,2.07922699378505));
#106859=CARTESIAN_POINT('Origin',(-10.,12.6,3.5));
#106860=CARTESIAN_POINT('',(-7.64545034777117,10.5,2.07922699378505));
#106861=CARTESIAN_POINT('',(-7.64545034777117,13.2,2.07922699378505));
#106862=CARTESIAN_POINT('',(-7.85960668072529,10.5,1.77338005374542));
#106863=CARTESIAN_POINT('Origin',(-10.,10.5,3.5));
#106864=CARTESIAN_POINT('',(-7.85960668072529,12.6,1.77338005374542));
#106865=CARTESIAN_POINT('',(-7.85960668072529,13.2,1.77338005374542));
#106866=CARTESIAN_POINT('',(-7.92793589104044,12.6,1.69194847187321));
#106867=CARTESIAN_POINT('Origin',(-10.,12.6,3.5));
#106868=CARTESIAN_POINT('',(-7.92793589104044,10.5,1.69194847187321));
#106869=CARTESIAN_POINT('',(-7.92793589104044,13.2,1.69194847187321));
#106870=CARTESIAN_POINT('',(-8.19194847187321,10.5,1.42793589104044));
#106871=CARTESIAN_POINT('Origin',(-10.,10.5,3.5));
#106872=CARTESIAN_POINT('',(-8.19194847187321,12.6,1.42793589104044));
#106873=CARTESIAN_POINT('',(-8.19194847187321,13.2,1.42793589104044));
#106874=CARTESIAN_POINT('',(-8.27338005374542,12.6,1.35960668072529));
#106875=CARTESIAN_POINT('Origin',(-10.,12.6,3.5));
#106876=CARTESIAN_POINT('',(-8.27338005374542,10.5,1.35960668072529));
#106877=CARTESIAN_POINT('',(-8.27338005374542,13.2,1.35960668072529));
#106878=CARTESIAN_POINT('',(-8.57922699378505,10.5,1.14545034777117));
#106879=CARTESIAN_POINT('Origin',(-10.,10.5,3.5));
#106880=CARTESIAN_POINT('',(-8.57922699378505,12.6,1.14545034777117));
#106881=CARTESIAN_POINT('',(-8.57922699378505,13.2,1.14545034777117));
#106882=CARTESIAN_POINT('',(-8.67128668980549,12.6,1.09229965749225));
#106883=CARTESIAN_POINT('Origin',(-10.,12.6,3.5));
#106884=CARTESIAN_POINT('',(-8.67128668980549,10.5,1.09229965749225));
#106885=CARTESIAN_POINT('',(-8.67128668980549,13.2,1.09229965749225));
#106886=CARTESIAN_POINT('',(-9.00967498454489,10.5,0.934506604225252));
#106887=CARTESIAN_POINT('Origin',(-10.,10.5,3.5));
#106888=CARTESIAN_POINT('',(-9.00967498454489,12.6,0.934506604225254));
#106889=CARTESIAN_POINT('',(-9.00967498454489,13.2,0.934506604225252));
#106890=CARTESIAN_POINT('',(-9.10956560743445,12.6,0.898149390811144));
#106891=CARTESIAN_POINT('Origin',(-10.,12.6,3.5));
#106892=CARTESIAN_POINT('',(-9.10956560743445,10.5,0.898149390811144));
#106893=CARTESIAN_POINT('',(-9.10956560743445,13.2,0.898149390811144));
#106894=CARTESIAN_POINT('',(-9.47021349977071,10.5,0.801514079307658));
#106895=CARTESIAN_POINT('Origin',(-10.,10.5,3.5));
#106896=CARTESIAN_POINT('',(-9.4702134997707,12.6,0.801514079307658));
#106897=CARTESIAN_POINT('',(-9.47021349977071,13.2,0.801514079307658));
#106898=CARTESIAN_POINT('',(-9.57489992349997,12.6,0.783055038290311));
#106899=CARTESIAN_POINT('Origin',(-10.,12.6,3.5));
#106900=CARTESIAN_POINT('',(-9.57489992349997,10.5,0.783055038290311));
#106901=CARTESIAN_POINT('',(-9.57489992349997,13.2,0.783055038290311));
#106902=CARTESIAN_POINT('',(-9.94684930972108,10.5,0.750513683590538));
#106903=CARTESIAN_POINT('Origin',(-10.,10.5,3.5));
#106904=CARTESIAN_POINT('',(-9.94684930972108,12.6,0.750513683590538));
#106905=CARTESIAN_POINT('',(-9.94684930972108,13.2,0.750513683590538));
#106906=CARTESIAN_POINT('',(-10.0531506902789,12.6,0.750513683590537));
#106907=CARTESIAN_POINT('Origin',(-10.,12.6,3.5));
#106908=CARTESIAN_POINT('',(-10.0531506902789,10.5,0.750513683590537));
#106909=CARTESIAN_POINT('',(-10.0531506902789,13.2,0.750513683590537));
#106910=CARTESIAN_POINT('',(-10.4251000765,10.5,0.783055038290311));
#106911=CARTESIAN_POINT('Origin',(-10.,10.5,3.5));
#106912=CARTESIAN_POINT('',(-10.4251000765,12.6,0.78305503829031));
#106913=CARTESIAN_POINT('',(-10.4251000765,13.2,0.783055038290311));
#106914=CARTESIAN_POINT('',(-10.5297865002293,12.6,0.801514079307658));
#106915=CARTESIAN_POINT('Origin',(-10.,12.6,3.5));
#106916=CARTESIAN_POINT('',(-10.5297865002293,10.5,0.801514079307658));
#106917=CARTESIAN_POINT('',(-10.5297865002293,13.2,0.801514079307658));
#106918=CARTESIAN_POINT('',(-10.8904343925655,10.5,0.898149390811144));
#106919=CARTESIAN_POINT('Origin',(-10.,10.5,3.5));
#106920=CARTESIAN_POINT('',(-10.8904343925656,12.6,0.898149390811144));
#106921=CARTESIAN_POINT('',(-10.8904343925655,13.2,0.898149390811144));
#106922=CARTESIAN_POINT('',(-10.9903250154551,12.6,0.934506604225253));
#106923=CARTESIAN_POINT('Origin',(-10.,12.6,3.5));
#106924=CARTESIAN_POINT('',(-10.9903250154551,10.5,0.934506604225253));
#106925=CARTESIAN_POINT('',(-10.9903250154551,13.2,0.934506604225253));
#106926=CARTESIAN_POINT('',(-11.3287133101945,10.5,1.09229965749225));
#106927=CARTESIAN_POINT('Origin',(-10.,10.5,3.5));
#106928=CARTESIAN_POINT('',(-11.3287133101945,12.6,1.09229965749225));
#106929=CARTESIAN_POINT('',(-11.3287133101945,13.2,1.09229965749225));
#106930=CARTESIAN_POINT('',(-11.420773006215,12.6,1.14545034777117));
#106931=CARTESIAN_POINT('Origin',(-10.,12.6,3.5));
#106932=CARTESIAN_POINT('',(-11.420773006215,10.5,1.14545034777117));
#106933=CARTESIAN_POINT('',(-11.420773006215,13.2,1.14545034777117));
#106934=CARTESIAN_POINT('',(-11.7266199462546,10.5,1.35960668072529));
#106935=CARTESIAN_POINT('Origin',(-10.,10.5,3.5));
#106936=CARTESIAN_POINT('',(-11.7266199462546,12.6,1.35960668072529));
#106937=CARTESIAN_POINT('',(-11.7266199462546,13.2,1.35960668072529));
#106938=CARTESIAN_POINT('',(-11.8080515281268,12.6,1.42793589104044));
#106939=CARTESIAN_POINT('Origin',(-10.,12.6,3.5));
#106940=CARTESIAN_POINT('',(-11.8080515281268,10.5,1.42793589104044));
#106941=CARTESIAN_POINT('',(-11.8080515281268,13.2,1.42793589104044));
#106942=CARTESIAN_POINT('',(-12.0720641089596,10.5,1.69194847187321));
#106943=CARTESIAN_POINT('Origin',(-10.,10.5,3.5));
#106944=CARTESIAN_POINT('',(-12.0720641089596,12.6,1.69194847187321));
#106945=CARTESIAN_POINT('',(-12.0720641089596,13.2,1.69194847187321));
#106946=CARTESIAN_POINT('',(-12.1403933192747,12.6,1.77338005374542));
#106947=CARTESIAN_POINT('Origin',(-10.,12.6,3.5));
#106948=CARTESIAN_POINT('',(-12.1403933192747,10.5,1.77338005374542));
#106949=CARTESIAN_POINT('',(-12.1403933192747,13.2,1.77338005374542));
#106950=CARTESIAN_POINT('',(-12.3545496522288,10.5,2.07922699378504));
#106951=CARTESIAN_POINT('Origin',(-10.,10.5,3.5));
#106952=CARTESIAN_POINT('',(-12.3545496522288,12.6,2.07922699378504));
#106953=CARTESIAN_POINT('',(-12.3545496522288,13.2,2.07922699378504));
#106954=CARTESIAN_POINT('',(-12.4077003425078,12.6,2.17128668980549));
#106955=CARTESIAN_POINT('Origin',(-10.,12.6,3.5));
#106956=CARTESIAN_POINT('',(-12.4077003425078,10.5,2.17128668980549));
#106957=CARTESIAN_POINT('',(-12.4077003425078,13.2,2.17128668980549));
#106958=CARTESIAN_POINT('',(-12.5654933957747,10.5,2.50967498454489));
#106959=CARTESIAN_POINT('Origin',(-10.,10.5,3.5));
#106960=CARTESIAN_POINT('',(-12.5654933957747,12.6,2.50967498454489));
#106961=CARTESIAN_POINT('',(-12.5654933957747,13.2,2.50967498454489));
#106962=CARTESIAN_POINT('',(-12.6018506091889,12.6,2.60956560743445));
#106963=CARTESIAN_POINT('Origin',(-10.,12.6,3.5));
#106964=CARTESIAN_POINT('',(-12.6018506091889,10.5,2.60956560743445));
#106965=CARTESIAN_POINT('',(-12.6018506091889,13.2,2.60956560743445));
#106966=CARTESIAN_POINT('',(-12.6984859206923,10.5,2.9702134997707));
#106967=CARTESIAN_POINT('Origin',(-10.,10.5,3.5));
#106968=CARTESIAN_POINT('',(-12.6984859206923,12.6,2.9702134997707));
#106969=CARTESIAN_POINT('',(-12.6984859206923,13.2,2.9702134997707));
#106970=CARTESIAN_POINT('',(-12.7169449617097,12.6,3.07489992349997));
#106971=CARTESIAN_POINT('Origin',(-10.,12.6,3.5));
#106972=CARTESIAN_POINT('',(-12.7169449617097,10.5,3.07489992349997));
#106973=CARTESIAN_POINT('',(-12.7169449617097,13.2,3.07489992349997));
#106974=CARTESIAN_POINT('',(-12.7494863164095,10.5,3.44684930972108));
#106975=CARTESIAN_POINT('Origin',(-10.,10.5,3.5));
#106976=CARTESIAN_POINT('',(-12.7494863164095,13.2,3.44684930972108));
#106977=CARTESIAN_POINT('Origin',(-7.07921428367087,10.2,4.39281061781755));
#106978=CARTESIAN_POINT('',(-7.55679918595664,12.6,4.38925237264674));
#106979=CARTESIAN_POINT('',(-7.55679918595664,12.6,4.38925237264674));
#106980=CARTESIAN_POINT('',(-7.55679918595664,10.35,4.38925237264674));
#106981=CARTESIAN_POINT('',(-7.55679918595664,10.2,4.38925237264674));
#106982=CARTESIAN_POINT('Ctrl Pts',(-7.39814939081114,10.5,4.39043439256555));
#106983=CARTESIAN_POINT('Ctrl Pts',(-7.47969835093245,10.4226475556384,
4.38982681223345));
#106984=CARTESIAN_POINT('Ctrl Pts',(-7.55679918595664,10.35,4.38925237264674));
#106985=CARTESIAN_POINT('Origin',(-7.55679918595664,10.2,4.38925237264674));
#106986=CARTESIAN_POINT('Ctrl Pts',(-7.55679918595664,10.35,4.38925237264674));
#106987=CARTESIAN_POINT('Ctrl Pts',(-7.49736727707808,10.4226475556379,
4.43837178784313));
#106988=CARTESIAN_POINT('Ctrl Pts',(-7.43450660422525,10.5,4.49032501545511));
#106989=CARTESIAN_POINT('',(-7.18866072953509,12.6,4.69351225646904));
#106990=CARTESIAN_POINT('Origin',(-7.34536834627981,12.6,4.46620690489502));
#106991=CARTESIAN_POINT('Origin',(-10.,10.35,3.5));
#106992=CARTESIAN_POINT('',(-12.6,10.35,3.5));
#106993=CARTESIAN_POINT('Ctrl Pts',(-12.6,10.35,3.5));
#106994=CARTESIAN_POINT('Ctrl Pts',(-12.6726475556384,10.4226475556384,
3.47416975799524));
#106995=CARTESIAN_POINT('Ctrl Pts',(-12.7494863164095,10.5,3.44684930972108));
#106996=CARTESIAN_POINT('',(-12.5605001578317,10.35,3.04851473806598));
#106997=CARTESIAN_POINT('Ctrl Pts',(-12.7169449617097,10.5,3.07489992349997));
#106998=CARTESIAN_POINT('Ctrl Pts',(-12.6365294083145,10.4226475556383,
3.06133744500587));
#106999=CARTESIAN_POINT('Ctrl Pts',(-12.5605001578317,10.35,3.04851473806598));
#107000=CARTESIAN_POINT('Ctrl Pts',(-12.5605001578317,10.35,3.04851473806598));
#107001=CARTESIAN_POINT('Ctrl Pts',(-12.627558659409,10.4226475556384,3.01046179982895));
#107002=CARTESIAN_POINT('Ctrl Pts',(-12.6984859206923,10.5,2.9702134997707));
#107003=CARTESIAN_POINT('',(-12.4432008140434,10.35,2.61074762735326));
#107004=CARTESIAN_POINT('Ctrl Pts',(-12.6018506091889,10.5,2.60956560743445));
#107005=CARTESIAN_POINT('Ctrl Pts',(-12.5203016490671,10.422647555638,2.61017318776655));
#107006=CARTESIAN_POINT('Ctrl Pts',(-12.4432008140434,10.35,2.61074762735326));
#107007=CARTESIAN_POINT('Ctrl Pts',(-12.4432008140434,10.35,2.61074762735326));
#107008=CARTESIAN_POINT('Ctrl Pts',(-12.5026327229221,10.4226475556382,
2.56162821215673));
#107009=CARTESIAN_POINT('Ctrl Pts',(-12.5654933957747,10.5,2.50967498454489));
#107010=CARTESIAN_POINT('',(-12.2516660498395,10.35,2.2));
#107011=CARTESIAN_POINT('Ctrl Pts',(-12.4077003425078,10.5,2.17128668980549));
#107012=CARTESIAN_POINT('Ctrl Pts',(-12.3274957995478,10.4226475556385,
2.1860458679428));
#107013=CARTESIAN_POINT('Ctrl Pts',(-12.2516660498395,10.35,2.2));
#107014=CARTESIAN_POINT('Ctrl Pts',(-12.2516660498395,10.35,2.2));
#107015=CARTESIAN_POINT('Ctrl Pts',(-12.3016655575428,10.4226475556383,
2.14130657641884));
#107016=CARTESIAN_POINT('Ctrl Pts',(-12.3545496522288,10.5,2.07922699378504));
#107017=CARTESIAN_POINT('',(-11.9917155521093,10.35,1.828752214815));
#107018=CARTESIAN_POINT('Ctrl Pts',(-12.1403933192747,10.5,1.77338005374542));
#107019=CARTESIAN_POINT('Ctrl Pts',(-12.063970167928,10.4226475556382,1.80184237952885));
#107020=CARTESIAN_POINT('Ctrl Pts',(-11.9917155521093,10.35,1.828752214815));
#107021=CARTESIAN_POINT('Ctrl Pts',(-11.9917155521093,10.35,1.828752214815));
#107022=CARTESIAN_POINT('Ctrl Pts',(-12.0307634488964,10.4226475556383,
1.76226815282458));
#107023=CARTESIAN_POINT('Ctrl Pts',(-12.0720641089596,10.5,1.69194847187321));
#107024=CARTESIAN_POINT('',(-11.671247785185,10.35,1.50828444789066));
#107025=CARTESIAN_POINT('Ctrl Pts',(-11.8080515281268,10.5,1.42793589104044));
#107026=CARTESIAN_POINT('Ctrl Pts',(-11.7377318471755,10.4226475556384,
1.46923655110355));
#107027=CARTESIAN_POINT('Ctrl Pts',(-11.671247785185,10.35,1.50828444789066));
#107028=CARTESIAN_POINT('Ctrl Pts',(-11.671247785185,10.35,1.50828444789066));
#107029=CARTESIAN_POINT('Ctrl Pts',(-11.6981576204711,10.4226475556381,
1.43602983207208));
#107030=CARTESIAN_POINT('Ctrl Pts',(-11.7266199462546,10.5,1.35960668072529));
#107031=CARTESIAN_POINT('',(-11.3,10.35,1.24833395016046));
#107032=CARTESIAN_POINT('Ctrl Pts',(-11.420773006215,10.5,1.14545034777117));
#107033=CARTESIAN_POINT('Ctrl Pts',(-11.3586934235811,10.4226475556382,
1.19833444245727));
#107034=CARTESIAN_POINT('Ctrl Pts',(-11.3,10.35,1.24833395016046));
#107035=CARTESIAN_POINT('Ctrl Pts',(-11.3,10.35,1.24833395016046));
#107036=CARTESIAN_POINT('Ctrl Pts',(-11.3139541320571,10.4226475556381,
1.17250420045271));
#107037=CARTESIAN_POINT('Ctrl Pts',(-11.3287133101945,10.5,1.09229965749225));
#107038=CARTESIAN_POINT('',(-10.8892523726467,10.35,1.05679918595664));
#107039=CARTESIAN_POINT('Ctrl Pts',(-10.9903250154551,10.5,0.934506604225252));
#107040=CARTESIAN_POINT('Ctrl Pts',(-10.9383717878433,10.4226475556382,
0.997367277077879));
#107041=CARTESIAN_POINT('Ctrl Pts',(-10.8892523726467,10.35,1.05679918595664));
#107042=CARTESIAN_POINT('Ctrl Pts',(-10.8892523726467,10.35,1.05679918595664));
#107043=CARTESIAN_POINT('Ctrl Pts',(-10.8898268122334,10.4226475556381,
0.9796983509328));
#107044=CARTESIAN_POINT('Ctrl Pts',(-10.8904343925655,10.5,0.898149390811143));
#107045=CARTESIAN_POINT('',(-10.451485261934,10.35,0.939499842168259));
#107046=CARTESIAN_POINT('Ctrl Pts',(-10.5297865002293,10.5,0.801514079307656));
#107047=CARTESIAN_POINT('Ctrl Pts',(-10.4895382001709,10.4226475556381,
0.87244134059127));
#107048=CARTESIAN_POINT('Ctrl Pts',(-10.451485261934,10.35,0.939499842168259));
#107049=CARTESIAN_POINT('Ctrl Pts',(-10.451485261934,10.35,0.939499842168259));
#107050=CARTESIAN_POINT('Ctrl Pts',(-10.4386625549941,10.4226475556383,
0.863470591685507));
#107051=CARTESIAN_POINT('Ctrl Pts',(-10.4251000765,10.5,0.783055038290308));
#107052=CARTESIAN_POINT('',(-10.,10.35,0.9));
#107053=CARTESIAN_POINT('Ctrl Pts',(-10.0531506902789,10.5,0.750513683590536));
#107054=CARTESIAN_POINT('Ctrl Pts',(-10.0258302420047,10.4226475556382,
0.827352444361817));
#107055=CARTESIAN_POINT('Ctrl Pts',(-10.,10.35,0.9));
#107056=CARTESIAN_POINT('Ctrl Pts',(-10.,10.35,0.9));
#107057=CARTESIAN_POINT('Ctrl Pts',(-9.97416975799534,10.4226475556381,
0.827352444361882));
#107058=CARTESIAN_POINT('Ctrl Pts',(-9.94684930972108,10.5,0.750513683590536));
#107059=CARTESIAN_POINT('',(-9.54851473806598,10.35,0.939499842168258));
#107060=CARTESIAN_POINT('Ctrl Pts',(-9.57489992349997,10.5,0.783055038290309));
#107061=CARTESIAN_POINT('Ctrl Pts',(-9.56133744500588,10.4226475556384,
0.863470591685391));
#107062=CARTESIAN_POINT('Ctrl Pts',(-9.54851473806598,10.35,0.939499842168258));
#107063=CARTESIAN_POINT('Ctrl Pts',(-9.54851473806598,10.35,0.939499842168258));
#107064=CARTESIAN_POINT('Ctrl Pts',(-9.51046179982901,10.4226475556383,
0.87244134059112));
#107065=CARTESIAN_POINT('Ctrl Pts',(-9.4702134997707,10.5,0.801514079307657));
#107066=CARTESIAN_POINT('',(-9.11074762735326,10.35,1.05679918595664));
#107067=CARTESIAN_POINT('Ctrl Pts',(-9.10956560743445,10.5,0.898149390811143));
#107068=CARTESIAN_POINT('Ctrl Pts',(-9.11017318776655,10.4226475556384,
0.979698350932521));
#107069=CARTESIAN_POINT('Ctrl Pts',(-9.11074762735326,10.35,1.05679918595664));
#107070=CARTESIAN_POINT('Ctrl Pts',(-9.11074762735326,10.35,1.05679918595664));
#107071=CARTESIAN_POINT('Ctrl Pts',(-9.06162821215675,10.4226475556381,
0.997367277077925));
#107072=CARTESIAN_POINT('Ctrl Pts',(-9.00967498454489,10.5,0.934506604225251));
#107073=CARTESIAN_POINT('',(-8.7,10.35,1.24833395016046));
#107074=CARTESIAN_POINT('Ctrl Pts',(-8.67128668980549,10.5,1.09229965749225));
#107075=CARTESIAN_POINT('Ctrl Pts',(-8.6860458679429,10.422647555638,1.17250420045278));
#107076=CARTESIAN_POINT('Ctrl Pts',(-8.7,10.35,1.24833395016046));
#107077=CARTESIAN_POINT('Ctrl Pts',(-8.7,10.35,1.24833395016046));
#107078=CARTESIAN_POINT('Ctrl Pts',(-8.64130657641881,10.4226475556384,
1.19833444245718));
#107079=CARTESIAN_POINT('Ctrl Pts',(-8.57922699378504,10.5,1.14545034777116));
#107080=CARTESIAN_POINT('',(-8.328752214815,10.35,1.50828444789066));
#107081=CARTESIAN_POINT('Ctrl Pts',(-8.27338005374542,10.5,1.35960668072529));
#107082=CARTESIAN_POINT('Ctrl Pts',(-8.30184237952875,10.4226475556385,
1.43602983207171));
#107083=CARTESIAN_POINT('Ctrl Pts',(-8.328752214815,10.35,1.50828444789066));
#107084=CARTESIAN_POINT('Ctrl Pts',(-8.328752214815,10.35,1.50828444789066));
#107085=CARTESIAN_POINT('Ctrl Pts',(-8.26226815282446,10.4226475556384,
1.46923655110356));
#107086=CARTESIAN_POINT('Ctrl Pts',(-8.19194847187321,10.5,1.42793589104044));
#107087=CARTESIAN_POINT('',(-8.00828444789066,10.35,1.828752214815));
#107088=CARTESIAN_POINT('Ctrl Pts',(-7.92793589104044,10.5,1.69194847187321));
#107089=CARTESIAN_POINT('Ctrl Pts',(-7.96923655110352,10.4226475556385,
1.76226815282441));
#107090=CARTESIAN_POINT('Ctrl Pts',(-8.00828444789066,10.35,1.828752214815));
#107091=CARTESIAN_POINT('Ctrl Pts',(-8.00828444789066,10.35,1.828752214815));
#107092=CARTESIAN_POINT('Ctrl Pts',(-7.93602983207183,10.4226475556384,
1.8018423795288));
#107093=CARTESIAN_POINT('Ctrl Pts',(-7.85960668072529,10.5,1.77338005374542));
#107094=CARTESIAN_POINT('',(-7.74833395016046,10.35,2.2));
#107095=CARTESIAN_POINT('Ctrl Pts',(-7.64545034777117,10.5,2.07922699378504));
#107096=CARTESIAN_POINT('Ctrl Pts',(-7.69833444245728,10.4226475556382,
2.14130657641894));
#107097=CARTESIAN_POINT('Ctrl Pts',(-7.74833395016046,10.35,2.2));
#107098=CARTESIAN_POINT('Ctrl Pts',(-7.74833395016046,10.35,2.2));
#107099=CARTESIAN_POINT('Ctrl Pts',(-7.67250420045245,10.4226475556383,
2.18604586794284));
#107100=CARTESIAN_POINT('Ctrl Pts',(-7.59229965749225,10.5,2.17128668980549));
#107101=CARTESIAN_POINT('',(-7.55679918595664,10.35,2.61074762735326));
#107102=CARTESIAN_POINT('Ctrl Pts',(-7.43450660422525,10.5,2.50967498454489));
#107103=CARTESIAN_POINT('Ctrl Pts',(-7.49736727707784,10.4226475556382,
2.56162821215668));
#107104=CARTESIAN_POINT('Ctrl Pts',(-7.55679918595664,10.35,2.61074762735326));
#107105=CARTESIAN_POINT('Ctrl Pts',(-7.55679918595664,10.35,2.61074762735326));
#107106=CARTESIAN_POINT('Ctrl Pts',(-7.47969835093274,10.4226475556382,
2.61017318776655));
#107107=CARTESIAN_POINT('Ctrl Pts',(-7.39814939081114,10.5,2.60956560743445));
#107108=CARTESIAN_POINT('',(-7.43949984216826,10.35,3.04851473806598));
#107109=CARTESIAN_POINT('Ctrl Pts',(-7.30151407930766,10.5,2.9702134997707));
#107110=CARTESIAN_POINT('Ctrl Pts',(-7.37244134059122,10.4226475556382,
3.01046179982907));
#107111=CARTESIAN_POINT('Ctrl Pts',(-7.43949984216826,10.35,3.04851473806598));
#107112=CARTESIAN_POINT('Ctrl Pts',(-7.43949984216826,10.35,3.04851473806598));
#107113=CARTESIAN_POINT('Ctrl Pts',(-7.36347059168553,10.4226475556382,
3.06133744500586));
#107114=CARTESIAN_POINT('Ctrl Pts',(-7.28305503829031,10.5,3.07489992349997));
#107115=CARTESIAN_POINT('',(-7.4,10.35,3.5));
#107116=CARTESIAN_POINT('Ctrl Pts',(-7.25051368359054,10.5,3.44684930972108));
#107117=CARTESIAN_POINT('Ctrl Pts',(-7.32735244436168,10.4226475556383,
3.47416975799527));
#107118=CARTESIAN_POINT('Ctrl Pts',(-7.4,10.35,3.5));
#107119=CARTESIAN_POINT('Ctrl Pts',(-7.4,10.35,3.5));
#107120=CARTESIAN_POINT('Ctrl Pts',(-7.32735244436169,10.4226475556383,
3.52583024200473));
#107121=CARTESIAN_POINT('Ctrl Pts',(-7.25051368359054,10.5,3.55315069027892));
#107122=CARTESIAN_POINT('',(-7.74833395016046,10.35,4.8));
#107123=CARTESIAN_POINT('Ctrl Pts',(-7.59229965749225,10.5,4.82871331019451));
#107124=CARTESIAN_POINT('Ctrl Pts',(-7.67250420045251,10.4226475556383,
4.81395413205715));
#107125=CARTESIAN_POINT('Ctrl Pts',(-7.74833395016046,10.35,4.8));
#107126=CARTESIAN_POINT('Ctrl Pts',(-7.74833395016046,10.35,4.8));
#107127=CARTESIAN_POINT('Ctrl Pts',(-7.6983344424572,10.4226475556383,4.85869342358116));
#107128=CARTESIAN_POINT('Ctrl Pts',(-7.64545034777117,10.5,4.92077300621496));
#107129=CARTESIAN_POINT('',(-8.00828444789066,10.35,5.171247785185));
#107130=CARTESIAN_POINT('Ctrl Pts',(-7.85960668072529,10.5,5.22661994625458));
#107131=CARTESIAN_POINT('Ctrl Pts',(-7.93602983207187,10.4226475556384,
5.19815762047119));
#107132=CARTESIAN_POINT('Ctrl Pts',(-8.00828444789066,10.35,5.171247785185));
#107133=CARTESIAN_POINT('Ctrl Pts',(-8.00828444789066,10.35,5.171247785185));
#107134=CARTESIAN_POINT('Ctrl Pts',(-7.96923655110368,10.4226475556382,
5.23773184717532));
#107135=CARTESIAN_POINT('Ctrl Pts',(-7.92793589104044,10.5,5.30805152812679));
#107136=CARTESIAN_POINT('',(-8.328752214815,10.35,5.49171555210934));
#107137=CARTESIAN_POINT('Ctrl Pts',(-8.19194847187321,10.5,5.57206410895956));
#107138=CARTESIAN_POINT('Ctrl Pts',(-8.26226815282441,10.4226475556384,
5.53076344889647));
#107139=CARTESIAN_POINT('Ctrl Pts',(-8.328752214815,10.35,5.49171555210934));
#107140=CARTESIAN_POINT('Ctrl Pts',(-8.328752214815,10.35,5.49171555210934));
#107141=CARTESIAN_POINT('Ctrl Pts',(-8.3018423795289,10.4226475556381,5.56397016792788));
#107142=CARTESIAN_POINT('Ctrl Pts',(-8.27338005374542,10.5,5.64039331927471));
#107143=CARTESIAN_POINT('',(-8.7,10.35,5.75166604983954));
#107144=CARTESIAN_POINT('Ctrl Pts',(-8.57922699378504,10.5,5.85454965222883));
#107145=CARTESIAN_POINT('Ctrl Pts',(-8.64130657641894,10.4226475556382,
5.80166555754271));
#107146=CARTESIAN_POINT('Ctrl Pts',(-8.7,10.35,5.75166604983954));
#107147=CARTESIAN_POINT('Ctrl Pts',(-8.7,10.35,5.75166604983954));
#107148=CARTESIAN_POINT('Ctrl Pts',(-8.68604586794282,10.4226475556384,
5.82749579954766));
#107149=CARTESIAN_POINT('Ctrl Pts',(-8.67128668980549,10.5,5.90770034250775));
#107150=CARTESIAN_POINT('',(-9.11074762735326,10.35,5.94320081404336));
#107151=CARTESIAN_POINT('Ctrl Pts',(-9.00967498454489,10.5,6.06549339577475));
#107152=CARTESIAN_POINT('Ctrl Pts',(-9.06162821215668,10.4226475556382,
6.00263272292216));
#107153=CARTESIAN_POINT('Ctrl Pts',(-9.11074762735326,10.35,5.94320081404336));
#107154=CARTESIAN_POINT('Ctrl Pts',(-9.11074762735326,10.35,5.94320081404336));
#107155=CARTESIAN_POINT('Ctrl Pts',(-9.11017318776655,10.4226475556383,
6.02030164906735));
#107156=CARTESIAN_POINT('Ctrl Pts',(-9.10956560743445,10.5,6.10185060918886));
#107157=CARTESIAN_POINT('',(-9.54851473806598,10.35,6.06050015783174));
#107158=CARTESIAN_POINT('Ctrl Pts',(-9.4702134997707,10.5,6.19848592069234));
#107159=CARTESIAN_POINT('Ctrl Pts',(-9.5104617998291,10.4226475556381,6.12755865940872));
#107160=CARTESIAN_POINT('Ctrl Pts',(-9.54851473806598,10.35,6.06050015783174));
#107161=CARTESIAN_POINT('Ctrl Pts',(-9.54851473806598,10.35,6.06050015783174));
#107162=CARTESIAN_POINT('Ctrl Pts',(-9.56133744500587,10.4226475556383,
6.13652940831454));
#107163=CARTESIAN_POINT('Ctrl Pts',(-9.57489992349997,10.5,6.21694496170969));
#107164=CARTESIAN_POINT('',(-10.,10.35,6.1));
#107165=CARTESIAN_POINT('Ctrl Pts',(-9.94684930972108,10.5,6.24948631640946));
#107166=CARTESIAN_POINT('Ctrl Pts',(-9.97416975799534,10.4226475556381,
6.17264755563811));
#107167=CARTESIAN_POINT('Ctrl Pts',(-10.,10.35,6.1));
#107168=CARTESIAN_POINT('Ctrl Pts',(-10.,10.35,6.1));
#107169=CARTESIAN_POINT('Ctrl Pts',(-10.0258302420047,10.4226475556382,
6.17264755563824));
#107170=CARTESIAN_POINT('Ctrl Pts',(-10.0531506902789,10.5,6.24948631640946));
#107171=CARTESIAN_POINT('',(-10.451485261934,10.35,6.06050015783174));
#107172=CARTESIAN_POINT('Ctrl Pts',(-10.4251000765,10.5,6.21694496170969));
#107173=CARTESIAN_POINT('Ctrl Pts',(-10.4386625549941,10.4226475556383,
6.13652940831459));
#107174=CARTESIAN_POINT('Ctrl Pts',(-10.451485261934,10.35,6.06050015783174));
#107175=CARTESIAN_POINT('Ctrl Pts',(-10.451485261934,10.35,6.06050015783174));
#107176=CARTESIAN_POINT('Ctrl Pts',(-10.4895382001709,10.4226475556381,
6.12755865940872));
#107177=CARTESIAN_POINT('Ctrl Pts',(-10.5297865002293,10.5,6.19848592069234));
#107178=CARTESIAN_POINT('',(-10.8892523726467,10.35,5.94320081404336));
#107179=CARTESIAN_POINT('Ctrl Pts',(-10.8904343925656,10.5,6.10185060918886));
#107180=CARTESIAN_POINT('Ctrl Pts',(-10.8898268122335,10.4226475556381,
6.02030164906721));
#107181=CARTESIAN_POINT('Ctrl Pts',(-10.8892523726467,10.35,5.94320081404336));
#107182=CARTESIAN_POINT('Ctrl Pts',(-10.8892523726467,10.35,5.94320081404336));
#107183=CARTESIAN_POINT('Ctrl Pts',(-10.9383717878434,10.4226475556383,
6.00263272292223));
#107184=CARTESIAN_POINT('Ctrl Pts',(-10.9903250154551,10.5,6.06549339577475));
#107185=CARTESIAN_POINT('',(-11.3,10.35,5.75166604983954));
#107186=CARTESIAN_POINT('Ctrl Pts',(-11.3287133101945,10.5,5.90770034250776));
#107187=CARTESIAN_POINT('Ctrl Pts',(-11.3139541320571,10.4226475556383,
5.8274957995475));
#107188=CARTESIAN_POINT('Ctrl Pts',(-11.3,10.35,5.75166604983954));
#107189=CARTESIAN_POINT('Ctrl Pts',(-11.3,10.35,5.75166604983954));
#107190=CARTESIAN_POINT('Ctrl Pts',(-11.358693423581,10.4226475556382,5.8016655575427));
#107191=CARTESIAN_POINT('Ctrl Pts',(-11.420773006215,10.5,5.85454965222883));
#107192=CARTESIAN_POINT('',(-11.671247785185,10.35,5.49171555210934));
#107193=CARTESIAN_POINT('Ctrl Pts',(-11.7266199462546,10.5,5.64039331927471));
#107194=CARTESIAN_POINT('Ctrl Pts',(-11.6981576204711,10.4226475556381,
5.56397016792789));
#107195=CARTESIAN_POINT('Ctrl Pts',(-11.671247785185,10.35,5.49171555210934));
#107196=CARTESIAN_POINT('Ctrl Pts',(-11.671247785185,10.35,5.49171555210934));
#107197=CARTESIAN_POINT('Ctrl Pts',(-11.7377318471755,10.4226475556384,
5.53076344889643));
#107198=CARTESIAN_POINT('Ctrl Pts',(-11.8080515281268,10.5,5.57206410895956));
#107199=CARTESIAN_POINT('',(-11.9917155521093,10.35,5.171247785185));
#107200=CARTESIAN_POINT('Ctrl Pts',(-12.0720641089596,10.5,5.30805152812679));
#107201=CARTESIAN_POINT('Ctrl Pts',(-12.0307634488963,10.4226475556381,
5.23773184717531));
#107202=CARTESIAN_POINT('Ctrl Pts',(-11.9917155521093,10.35,5.171247785185));
#107203=CARTESIAN_POINT('Ctrl Pts',(-11.9917155521093,10.35,5.171247785185));
#107204=CARTESIAN_POINT('Ctrl Pts',(-12.0639701679281,10.4226475556383,
5.19815762047119));
#107205=CARTESIAN_POINT('Ctrl Pts',(-12.1403933192747,10.5,5.22661994625458));
#107206=CARTESIAN_POINT('',(-12.2516660498395,10.35,4.8));
#107207=CARTESIAN_POINT('Ctrl Pts',(-12.3545496522288,10.5,4.92077300621495));
#107208=CARTESIAN_POINT('Ctrl Pts',(-12.3016655575427,10.4226475556382,
4.85869342358103));
#107209=CARTESIAN_POINT('Ctrl Pts',(-12.2516660498395,10.35,4.8));
#107210=CARTESIAN_POINT('Ctrl Pts',(-12.2516660498395,10.35,4.8));
#107211=CARTESIAN_POINT('Ctrl Pts',(-12.3274957995474,10.4226475556382,
4.81395413205714));
#107212=CARTESIAN_POINT('Ctrl Pts',(-12.4077003425078,10.5,4.82871331019451));
#107213=CARTESIAN_POINT('',(-12.4432008140434,10.35,4.38925237264674));
#107214=CARTESIAN_POINT('Ctrl Pts',(-12.5654933957747,10.5,4.49032501545511));
#107215=CARTESIAN_POINT('Ctrl Pts',(-12.5026327229219,10.4226475556379,
4.43837178784312));
#107216=CARTESIAN_POINT('Ctrl Pts',(-12.4432008140434,10.35,4.38925237264674));
#107217=CARTESIAN_POINT('Ctrl Pts',(-12.4432008140434,10.35,4.38925237264674));
#107218=CARTESIAN_POINT('Ctrl Pts',(-12.5203016490672,10.4226475556381,
4.38982681223345));
#107219=CARTESIAN_POINT('Ctrl Pts',(-12.6018506091889,10.5,4.39043439256555));
#107220=CARTESIAN_POINT('',(-12.5605001578317,10.35,3.95148526193402));
#107221=CARTESIAN_POINT('Ctrl Pts',(-12.6984859206923,10.5,4.0297865002293));
#107222=CARTESIAN_POINT('Ctrl Pts',(-12.6275586594092,10.4226475556386,
3.98953820017117));
#107223=CARTESIAN_POINT('Ctrl Pts',(-12.5605001578317,10.35,3.95148526193402));
#107224=CARTESIAN_POINT('Ctrl Pts',(-12.5605001578317,10.35,3.95148526193402));
#107225=CARTESIAN_POINT('Ctrl Pts',(-12.6365294083143,10.4226475556381,
3.93866255499416));
#107226=CARTESIAN_POINT('Ctrl Pts',(-12.7169449617097,10.5,3.92510007650003));
#107227=CARTESIAN_POINT('Ctrl Pts',(-12.7494863164095,10.5,3.55315069027892));
#107228=CARTESIAN_POINT('Ctrl Pts',(-12.6726475556383,10.4226475556383,
3.52583024200474));
#107229=CARTESIAN_POINT('Ctrl Pts',(-12.6,10.35,3.5));
#107230=CARTESIAN_POINT('',(-12.45,10.2,3.5));
#107231=CARTESIAN_POINT('',(-12.6,10.35,3.5));
#107232=CARTESIAN_POINT('Origin',(-10.,10.2,3.5));
#107233=CARTESIAN_POINT('Origin',(-7.55347823430896,12.6,4.9125));
#107234=CARTESIAN_POINT('',(-7.74833395016046,12.6,4.8));
#107235=CARTESIAN_POINT('',(-7.43862251845746,12.6,5.16356406460551));
#107236=CARTESIAN_POINT('',(-7.74833395016046,12.6,4.8));
#107237=CARTESIAN_POINT('Origin',(-7.27862251845746,10.2,4.88643593539449));
#107238=CARTESIAN_POINT('',(-7.74833395016046,10.2,4.8));
#107239=CARTESIAN_POINT('Origin',(-7.74833395016046,10.2,4.8));
#107240=CARTESIAN_POINT('Origin',(-7.56071843093727,10.2,5.33793509864491));
#107241=CARTESIAN_POINT('',(-8.00828444789066,12.6,5.171247785185));
#107242=CARTESIAN_POINT('',(-8.00828444789066,12.6,5.171247785185));
#107243=CARTESIAN_POINT('',(-8.00828444789066,10.2,5.171247785185));
#107244=CARTESIAN_POINT('Origin',(-8.00828444789066,10.2,5.171247785185));
#107245=CARTESIAN_POINT('',(-7.76641046603697,12.6,5.58306932044298));
#107246=CARTESIAN_POINT('Origin',(-7.83592444818889,12.6,5.31587499736447));
#107247=CARTESIAN_POINT('Origin',(-8.18412500263553,12.6,5.66407555181111));
#107248=CARTESIAN_POINT('',(-8.328752214815,12.6,5.49171555210934));
#107249=CARTESIAN_POINT('',(-8.16206490135509,12.6,5.93928156906273));
#107250=CARTESIAN_POINT('',(-8.328752214815,12.6,5.49171555210934));
#107251=CARTESIAN_POINT('Origin',(-7.91693067955702,10.2,5.73358953396304));
#107252=CARTESIAN_POINT('',(-8.328752214815,10.2,5.49171555210934));
#107253=CARTESIAN_POINT('Origin',(-8.328752214815,10.2,5.49171555210934));
#107254=CARTESIAN_POINT('Origin',(-8.33643593539449,10.2,6.06137748154254));
#107255=CARTESIAN_POINT('',(-8.7,12.6,5.75166604983954));
#107256=CARTESIAN_POINT('',(-8.7,12.6,5.75166604983954));
#107257=CARTESIAN_POINT('',(-8.7,10.2,5.75166604983954));
#107258=CARTESIAN_POINT('Origin',(-8.7,10.2,5.75166604983954));
#107259=CARTESIAN_POINT('',(-8.61356406460551,12.6,6.22137748154254));
#107260=CARTESIAN_POINT('Origin',(-8.5875,12.6,5.94652176569104));
#107261=CARTESIAN_POINT('Origin',(-9.03379309510499,12.6,6.15463165372019));
#107262=CARTESIAN_POINT('',(-9.11074762735326,12.6,5.94320081404336));
#107263=CARTESIAN_POINT('',(-9.10718938218246,12.6,6.42078571632913));
#107264=CARTESIAN_POINT('',(-9.11074762735326,12.6,5.94320081404336));
#107265=CARTESIAN_POINT('Origin',(-8.80648774353097,10.2,6.31133927046491));
#107266=CARTESIAN_POINT('',(-9.11074762735326,10.2,5.94320081404336));
#107267=CARTESIAN_POINT('Origin',(-9.11074762735326,10.2,5.94320081404336));
#107268=CARTESIAN_POINT('Origin',(-9.31280381763391,10.2,6.47587993826052));
#107269=CARTESIAN_POINT('',(-9.54851473806598,12.6,6.06050015783174));
#107270=CARTESIAN_POINT('',(-9.54851473806598,12.6,6.06050015783174));
#107271=CARTESIAN_POINT('',(-9.54851473806598,10.2,6.06050015783174));
#107272=CARTESIAN_POINT('Origin',(-9.54851473806598,10.2,6.06050015783174));
#107273=CARTESIAN_POINT('',(-9.62794229859782,12.6,6.53144735511394));
#107274=CARTESIAN_POINT('Origin',(-9.50944389809092,12.6,6.28208190225949));
#107275=CARTESIAN_POINT('Origin',(-10.,12.6,6.325));
#107276=CARTESIAN_POINT('',(-10.,12.6,6.1));
#107277=CARTESIAN_POINT('',(-10.16,12.6,6.55));
#107278=CARTESIAN_POINT('',(-10.,12.6,6.1));
#107279=CARTESIAN_POINT('Origin',(-9.84,10.2,6.55));
#107280=CARTESIAN_POINT('',(-10.,10.2,6.1));
#107281=CARTESIAN_POINT('Origin',(-10.,10.2,6.1));
#107282=CARTESIAN_POINT('Origin',(-10.3720577014022,10.2,6.53144735511395));
#107283=CARTESIAN_POINT('',(-10.451485261934,12.6,6.06050015783174));
#107284=CARTESIAN_POINT('',(-10.451485261934,12.6,6.06050015783174));
#107285=CARTESIAN_POINT('',(-10.451485261934,10.2,6.06050015783174));
#107286=CARTESIAN_POINT('Origin',(-10.451485261934,10.2,6.06050015783174));
#107287=CARTESIAN_POINT('',(-10.6871961823661,12.6,6.47587993826053));
#107288=CARTESIAN_POINT('Origin',(-10.4905561019091,12.6,6.28208190225949));
#107289=CARTESIAN_POINT('Origin',(-10.966206904895,12.6,6.15463165372019));
#107290=CARTESIAN_POINT('',(-10.8892523726467,12.6,5.94320081404336));
#107291=CARTESIAN_POINT('',(-11.193512256469,12.6,6.31133927046491));
#107292=CARTESIAN_POINT('',(-10.8892523726467,12.6,5.94320081404336));
#107293=CARTESIAN_POINT('Origin',(-10.8928106178175,10.2,6.42078571632913));
#107294=CARTESIAN_POINT('',(-10.8892523726467,10.2,5.94320081404336));
#107295=CARTESIAN_POINT('Origin',(-10.8892523726467,10.2,5.94320081404336));
#107296=CARTESIAN_POINT('Origin',(-11.3864359353945,10.2,6.22137748154254));
#107297=CARTESIAN_POINT('',(-11.3,12.6,5.75166604983954));
#107298=CARTESIAN_POINT('',(-11.3,12.6,5.75166604983954));
#107299=CARTESIAN_POINT('',(-11.3,10.2,5.75166604983954));
#107300=CARTESIAN_POINT('Origin',(-11.3,10.2,5.75166604983954));
#107301=CARTESIAN_POINT('',(-11.6635640646055,12.6,6.06137748154254));
#107302=CARTESIAN_POINT('Origin',(-11.4125,12.6,5.94652176569104));
#107303=CARTESIAN_POINT('Origin',(-11.8158749973645,12.6,5.66407555181111));
#107304=CARTESIAN_POINT('',(-11.671247785185,12.6,5.49171555210934));
#107305=CARTESIAN_POINT('',(-12.083069320443,12.6,5.73358953396303));
#107306=CARTESIAN_POINT('',(-11.671247785185,12.6,5.49171555210934));
#107307=CARTESIAN_POINT('Origin',(-11.8379350986449,10.2,5.93928156906273));
#107308=CARTESIAN_POINT('',(-11.671247785185,10.2,5.49171555210934));
#107309=CARTESIAN_POINT('Origin',(-11.671247785185,10.2,5.49171555210934));
#107310=CARTESIAN_POINT('Origin',(-12.233589533963,10.2,5.58306932044298));
#107311=CARTESIAN_POINT('',(-11.9917155521093,12.6,5.171247785185));
#107312=CARTESIAN_POINT('',(-11.9917155521093,12.6,5.171247785185));
#107313=CARTESIAN_POINT('',(-11.9917155521093,10.2,5.171247785185));
#107314=CARTESIAN_POINT('Origin',(-11.9917155521093,10.2,5.171247785185));
#107315=CARTESIAN_POINT('',(-12.4392815690627,12.6,5.33793509864491));
#107316=CARTESIAN_POINT('Origin',(-12.1640755518111,12.6,5.31587499736447));
#107317=CARTESIAN_POINT('Origin',(-12.446521765691,12.6,4.9125));
#107318=CARTESIAN_POINT('',(-12.2516660498395,12.6,4.8));
#107319=CARTESIAN_POINT('',(-12.7213774815425,12.6,4.88643593539449));
#107320=CARTESIAN_POINT('',(-12.2516660498395,12.6,4.8));
#107321=CARTESIAN_POINT('Origin',(-12.5613774815425,10.2,5.16356406460551));
#107322=CARTESIAN_POINT('',(-12.2516660498395,10.2,4.8));
#107323=CARTESIAN_POINT('Origin',(-12.2516660498395,10.2,4.8));
#107324=CARTESIAN_POINT('Origin',(-12.8113392704649,10.2,4.69351225646903));
#107325=CARTESIAN_POINT('',(-12.4432008140434,12.6,4.38925237264674));
#107326=CARTESIAN_POINT('',(-12.4432008140434,12.6,4.38925237264674));
#107327=CARTESIAN_POINT('',(-12.4432008140434,10.2,4.38925237264674));
#107328=CARTESIAN_POINT('Origin',(-12.4432008140434,10.2,4.38925237264674));
#107329=CARTESIAN_POINT('',(-12.9207857163291,12.6,4.39281061781754));
#107330=CARTESIAN_POINT('Origin',(-12.6546316537202,12.6,4.46620690489501));
#107331=CARTESIAN_POINT('Origin',(-12.7820819022595,12.6,3.99055610190908));
#107332=CARTESIAN_POINT('',(-12.5605001578317,12.6,3.95148526193402));
#107333=CARTESIAN_POINT('',(-13.0314473551139,12.6,3.87205770140218));
#107334=CARTESIAN_POINT('',(-12.5605001578317,12.6,3.95148526193402));
#107335=CARTESIAN_POINT('Origin',(-12.9758799382605,10.2,4.18719618236609));
#107336=CARTESIAN_POINT('',(-12.5605001578317,10.2,3.95148526193402));
#107337=CARTESIAN_POINT('Origin',(-12.5605001578317,10.2,3.95148526193402));
#107338=CARTESIAN_POINT('Origin',(-13.05,10.2,3.66));
#107339=CARTESIAN_POINT('',(-12.6,12.6,3.5));
#107340=CARTESIAN_POINT('',(-12.6,12.6,3.5));
#107341=CARTESIAN_POINT('',(-12.6,10.2,3.5));
#107342=CARTESIAN_POINT('Origin',(-12.6,10.2,3.5));
#107343=CARTESIAN_POINT('',(-13.05,12.6,3.34));
#107344=CARTESIAN_POINT('Origin',(-12.825,12.6,3.5));
#107345=CARTESIAN_POINT('Origin',(-12.7820819022595,12.6,3.00944389809092));
#107346=CARTESIAN_POINT('',(-12.5605001578317,12.6,3.04851473806598));
#107347=CARTESIAN_POINT('',(-12.9758799382605,12.6,2.81280381763391));
#107348=CARTESIAN_POINT('',(-12.5605001578317,12.6,3.04851473806598));
#107349=CARTESIAN_POINT('Origin',(-13.0314473551139,10.2,3.12794229859781));
#107350=CARTESIAN_POINT('',(-12.5605001578317,10.2,3.04851473806598));
#107351=CARTESIAN_POINT('Origin',(-12.5605001578317,10.2,3.04851473806598));
#107352=CARTESIAN_POINT('Origin',(-12.9207857163291,10.2,2.60718938218245));
#107353=CARTESIAN_POINT('',(-12.4432008140434,12.6,2.61074762735326));
#107354=CARTESIAN_POINT('',(-12.4432008140434,12.6,2.61074762735326));
#107355=CARTESIAN_POINT('',(-12.4432008140434,10.2,2.61074762735326));
#107356=CARTESIAN_POINT('Origin',(-12.4432008140434,10.2,2.61074762735326));
#107357=CARTESIAN_POINT('',(-12.8113392704649,12.6,2.30648774353096));
#107358=CARTESIAN_POINT('Origin',(-12.6546316537202,12.6,2.53379309510498));
#107359=CARTESIAN_POINT('Origin',(-12.446521765691,12.6,2.0875));
#107360=CARTESIAN_POINT('',(-12.2516660498395,12.6,2.2));
#107361=CARTESIAN_POINT('',(-12.5613774815425,12.6,1.83643593539449));
#107362=CARTESIAN_POINT('',(-12.2516660498395,12.6,2.2));
#107363=CARTESIAN_POINT('Origin',(-12.7213774815425,10.2,2.11356406460551));
#107364=CARTESIAN_POINT('',(-12.2516660498395,10.2,2.2));
#107365=CARTESIAN_POINT('Origin',(-12.2516660498395,10.2,2.2));
#107366=CARTESIAN_POINT('Origin',(-12.4392815690627,10.2,1.66206490135509));
#107367=CARTESIAN_POINT('',(-11.9917155521093,12.6,1.828752214815));
#107368=CARTESIAN_POINT('',(-11.9917155521093,12.6,1.828752214815));
#107369=CARTESIAN_POINT('',(-11.9917155521093,10.2,1.828752214815));
#107370=CARTESIAN_POINT('Origin',(-11.9917155521093,10.2,1.828752214815));
#107371=CARTESIAN_POINT('',(-12.233589533963,12.6,1.41693067955702));
#107372=CARTESIAN_POINT('Origin',(-12.1640755518111,12.6,1.68412500263553));
#107373=CARTESIAN_POINT('Origin',(-11.8158749973645,12.6,1.33592444818889));
#107374=CARTESIAN_POINT('',(-11.671247785185,12.6,1.50828444789066));
#107375=CARTESIAN_POINT('',(-11.8379350986449,12.6,1.06071843093727));
#107376=CARTESIAN_POINT('',(-11.671247785185,12.6,1.50828444789066));
#107377=CARTESIAN_POINT('Origin',(-12.083069320443,10.2,1.26641046603696));
#107378=CARTESIAN_POINT('',(-11.671247785185,10.2,1.50828444789066));
#107379=CARTESIAN_POINT('Origin',(-11.671247785185,10.2,1.50828444789066));
#107380=CARTESIAN_POINT('Origin',(-11.6635640646055,10.2,0.938622518457461));
#107381=CARTESIAN_POINT('',(-11.3,12.6,1.24833395016046));
#107382=CARTESIAN_POINT('',(-11.3,12.6,1.24833395016046));
#107383=CARTESIAN_POINT('',(-11.3,10.2,1.24833395016046));
#107384=CARTESIAN_POINT('Origin',(-11.3,10.2,1.24833395016046));
#107385=CARTESIAN_POINT('',(-11.3864359353945,12.6,0.778622518457461));
#107386=CARTESIAN_POINT('Origin',(-11.4125,12.6,1.05347823430896));
#107387=CARTESIAN_POINT('Origin',(-10.966206904895,12.6,0.845368346279809));
#107388=CARTESIAN_POINT('',(-10.8892523726467,12.6,1.05679918595664));
#107389=CARTESIAN_POINT('',(-10.8928106178175,12.6,0.579214283670874));
#107390=CARTESIAN_POINT('',(-10.8892523726467,12.6,1.05679918595664));
#107391=CARTESIAN_POINT('Origin',(-11.193512256469,10.2,0.688660729535087));
#107392=CARTESIAN_POINT('',(-10.8892523726467,10.2,1.05679918595664));
#107393=CARTESIAN_POINT('Origin',(-10.8892523726467,10.2,1.05679918595664));
#107394=CARTESIAN_POINT('Origin',(-10.6871961823661,10.2,0.524120061739474));
#107395=CARTESIAN_POINT('',(-10.451485261934,12.6,0.939499842168259));
#107396=CARTESIAN_POINT('',(-10.451485261934,12.6,0.939499842168259));
#107397=CARTESIAN_POINT('',(-10.451485261934,10.2,0.939499842168259));
#107398=CARTESIAN_POINT('Origin',(-10.451485261934,10.2,0.939499842168259));
#107399=CARTESIAN_POINT('',(-10.3720577014022,12.6,0.468552644886056));
#107400=CARTESIAN_POINT('Origin',(-10.4905561019091,12.6,0.717918097740512));
#107401=CARTESIAN_POINT('Origin',(-10.,12.6,0.675));
#107402=CARTESIAN_POINT('',(-10.,12.6,0.9));
#107403=CARTESIAN_POINT('',(-9.84,12.6,0.45));
#107404=CARTESIAN_POINT('',(-10.,12.6,0.9));
#107405=CARTESIAN_POINT('Origin',(-10.16,10.2,0.45));
#107406=CARTESIAN_POINT('',(-10.,10.2,0.9));
#107407=CARTESIAN_POINT('Origin',(-10.,10.2,0.9));
#107408=CARTESIAN_POINT('Origin',(-9.62794229859782,10.2,0.468552644886056));
#107409=CARTESIAN_POINT('',(-9.54851473806598,12.6,0.939499842168258));
#107410=CARTESIAN_POINT('',(-9.54851473806598,12.6,0.939499842168258));
#107411=CARTESIAN_POINT('',(-9.54851473806598,10.2,0.939499842168258));
#107412=CARTESIAN_POINT('Origin',(-9.54851473806598,10.2,0.939499842168258));
#107413=CARTESIAN_POINT('',(-9.31280381763391,12.6,0.524120061739474));
#107414=CARTESIAN_POINT('Origin',(-9.50944389809092,12.6,0.717918097740512));
#107415=CARTESIAN_POINT('Origin',(-9.03379309510498,12.6,0.845368346279809));
#107416=CARTESIAN_POINT('',(-9.11074762735326,12.6,1.05679918595664));
#107417=CARTESIAN_POINT('',(-8.80648774353096,12.6,0.688660729535087));
#107418=CARTESIAN_POINT('',(-9.11074762735326,12.6,1.05679918595664));
#107419=CARTESIAN_POINT('Origin',(-9.10718938218246,10.2,0.579214283670872));
#107420=CARTESIAN_POINT('',(-9.11074762735326,10.2,1.05679918595664));
#107421=CARTESIAN_POINT('Origin',(-9.11074762735326,10.2,1.05679918595664));
#107422=CARTESIAN_POINT('Origin',(-8.61356406460551,10.2,0.778622518457462));
#107423=CARTESIAN_POINT('',(-8.7,12.6,1.24833395016046));
#107424=CARTESIAN_POINT('',(-8.7,12.6,1.24833395016046));
#107425=CARTESIAN_POINT('',(-8.7,10.2,1.24833395016046));
#107426=CARTESIAN_POINT('Origin',(-8.7,10.2,1.24833395016046));
#107427=CARTESIAN_POINT('',(-8.33643593539449,12.6,0.938622518457463));
#107428=CARTESIAN_POINT('Origin',(-8.5875,12.6,1.05347823430896));
#107429=CARTESIAN_POINT('Origin',(-8.18412500263553,12.6,1.33592444818889));
#107430=CARTESIAN_POINT('',(-8.328752214815,12.6,1.50828444789066));
#107431=CARTESIAN_POINT('',(-7.91693067955702,12.6,1.26641046603696));
#107432=CARTESIAN_POINT('',(-8.328752214815,12.6,1.50828444789066));
#107433=CARTESIAN_POINT('Origin',(-8.16206490135509,10.2,1.06071843093727));
#107434=CARTESIAN_POINT('',(-8.328752214815,10.2,1.50828444789066));
#107435=CARTESIAN_POINT('Origin',(-8.328752214815,10.2,1.50828444789066));
#107436=CARTESIAN_POINT('Origin',(-7.76641046603696,10.2,1.41693067955702));
#107437=CARTESIAN_POINT('',(-8.00828444789066,12.6,1.828752214815));
#107438=CARTESIAN_POINT('',(-8.00828444789066,12.6,1.828752214815));
#107439=CARTESIAN_POINT('',(-8.00828444789066,10.2,1.828752214815));
#107440=CARTESIAN_POINT('Origin',(-8.00828444789066,10.2,1.828752214815));
#107441=CARTESIAN_POINT('',(-7.56071843093727,12.6,1.66206490135509));
#107442=CARTESIAN_POINT('Origin',(-7.83592444818889,12.6,1.68412500263553));
#107443=CARTESIAN_POINT('Origin',(-7.55347823430896,12.6,2.0875));
#107444=CARTESIAN_POINT('',(-7.74833395016046,12.6,2.2));
#107445=CARTESIAN_POINT('',(-7.27862251845746,12.6,2.11356406460551));
#107446=CARTESIAN_POINT('',(-7.74833395016046,12.6,2.2));
#107447=CARTESIAN_POINT('Origin',(-7.43862251845746,10.2,1.83643593539449));
#107448=CARTESIAN_POINT('',(-7.74833395016046,10.2,2.2));
#107449=CARTESIAN_POINT('Origin',(-7.74833395016046,10.2,2.2));
#107450=CARTESIAN_POINT('Origin',(-7.18866072953509,10.2,2.30648774353096));
#107451=CARTESIAN_POINT('',(-7.55679918595664,12.6,2.61074762735326));
#107452=CARTESIAN_POINT('',(-7.55679918595664,12.6,2.61074762735326));
#107453=CARTESIAN_POINT('',(-7.55679918595664,10.2,2.61074762735326));
#107454=CARTESIAN_POINT('Origin',(-7.55679918595664,10.2,2.61074762735326));
#107455=CARTESIAN_POINT('',(-7.07921428367087,12.6,2.60718938218246));
#107456=CARTESIAN_POINT('Origin',(-7.34536834627981,12.6,2.53379309510498));
#107457=CARTESIAN_POINT('Origin',(-7.21791809774051,12.6,3.00944389809092));
#107458=CARTESIAN_POINT('',(-7.43949984216826,12.6,3.04851473806598));
#107459=CARTESIAN_POINT('',(-6.96855264488606,12.6,3.12794229859781));
#107460=CARTESIAN_POINT('',(-7.43949984216826,12.6,3.04851473806598));
#107461=CARTESIAN_POINT('Origin',(-7.02412006173947,10.2,2.81280381763391));
#107462=CARTESIAN_POINT('',(-7.43949984216826,10.2,3.04851473806598));
#107463=CARTESIAN_POINT('Origin',(-7.43949984216826,10.2,3.04851473806598));
#107464=CARTESIAN_POINT('Origin',(-6.95,10.2,3.34));
#107465=CARTESIAN_POINT('',(-7.4,12.6,3.5));
#107466=CARTESIAN_POINT('',(-7.4,12.6,3.5));
#107467=CARTESIAN_POINT('',(-7.4,10.2,3.5));
#107468=CARTESIAN_POINT('Origin',(-7.4,10.2,3.5));
#107469=CARTESIAN_POINT('',(-6.95,12.6,3.66));
#107470=CARTESIAN_POINT('Origin',(-7.175,12.6,3.5));
#107471=CARTESIAN_POINT('Origin',(-10.,13.,3.5));
#107472=CARTESIAN_POINT('Origin',(-10.,13.,0.95));
#107473=CARTESIAN_POINT('Origin',(-10.,10.2,3.5));
#107474=CARTESIAN_POINT('',(-11.5933756729741,10.2,3.5));
#107475=CARTESIAN_POINT('Origin',(-10.,10.2,3.5));
#107476=CARTESIAN_POINT('Origin',(-10.,10.3,3.5));
#107477=CARTESIAN_POINT('',(-11.3903449147952,10.4,3.5918519675297));
#107478=CARTESIAN_POINT('',(-11.4433756729741,10.35,3.5));
#107479=CARTESIAN_POINT('Ctrl Pts',(-11.3903449147952,10.4,3.59185196752971));
#107480=CARTESIAN_POINT('Ctrl Pts',(-11.4163929392269,10.3769827337472,
3.54673546577726));
#107481=CARTESIAN_POINT('Ctrl Pts',(-11.4433756729741,10.35,3.5));
#107482=CARTESIAN_POINT('',(-10.7747185946659,10.4,4.65814803247029));
#107483=CARTESIAN_POINT('Origin',(-10.,10.4,3.5));
#107484=CARTESIAN_POINT('',(-10.721687836487,10.35,4.75));
#107485=CARTESIAN_POINT('Ctrl Pts',(-10.721687836487,10.35,4.75));
#107486=CARTESIAN_POINT('Ctrl Pts',(-10.7486705702342,10.3769827337472,
4.70326453422273));
#107487=CARTESIAN_POINT('Ctrl Pts',(-10.7747185946659,10.4,4.65814803247029));
#107488=CARTESIAN_POINT('',(-10.6156263201293,10.4,4.75));
#107489=CARTESIAN_POINT('Ctrl Pts',(-10.6156263201293,10.4,4.75));
#107490=CARTESIAN_POINT('Ctrl Pts',(-10.6677223689926,10.3769827337472,
4.75));
#107491=CARTESIAN_POINT('Ctrl Pts',(-10.721687836487,10.35,4.75));
#107492=CARTESIAN_POINT('',(-9.38437367987071,10.4,4.75));
#107493=CARTESIAN_POINT('Origin',(-10.,10.4,3.5));
#107494=CARTESIAN_POINT('',(-9.27831216351297,10.35,4.75));
#107495=CARTESIAN_POINT('Ctrl Pts',(-9.27831216351297,10.35,4.75));
#107496=CARTESIAN_POINT('Ctrl Pts',(-9.33227763100738,10.3769827337472,
4.75));
#107497=CARTESIAN_POINT('Ctrl Pts',(-9.38437367987072,10.4,4.75));
#107498=CARTESIAN_POINT('',(-9.2252814053341,10.4,4.65814803247029));
#107499=CARTESIAN_POINT('Ctrl Pts',(-9.22528140533409,10.4,4.65814803247029));
#107500=CARTESIAN_POINT('Ctrl Pts',(-9.25132942976576,10.3769827337472,
4.70326453422274));
#107501=CARTESIAN_POINT('Ctrl Pts',(-9.27831216351297,10.35,4.75));
#107502=CARTESIAN_POINT('',(-8.60965508520481,10.4,3.5918519675297));
#107503=CARTESIAN_POINT('Origin',(-10.,10.4,3.5));
#107504=CARTESIAN_POINT('',(-8.55662432702594,10.35,3.5));
#107505=CARTESIAN_POINT('Ctrl Pts',(-8.55662432702594,10.35,3.5));
#107506=CARTESIAN_POINT('Ctrl Pts',(-8.58360706077314,10.3769827337472,
3.54673546577726));
#107507=CARTESIAN_POINT('Ctrl Pts',(-8.60965508520481,10.4,3.59185196752971));
#107508=CARTESIAN_POINT('',(-8.60965508520481,10.4,3.4081480324703));
#107509=CARTESIAN_POINT('Ctrl Pts',(-8.60965508520481,10.4,3.40814803247029));
#107510=CARTESIAN_POINT('Ctrl Pts',(-8.58360706077314,10.3769827337472,
3.45326453422273));
#107511=CARTESIAN_POINT('Ctrl Pts',(-8.55662432702594,10.35,3.5));
#107512=CARTESIAN_POINT('',(-9.2252814053341,10.4,2.34185196752971));
#107513=CARTESIAN_POINT('Origin',(-10.,10.4,3.5));
#107514=CARTESIAN_POINT('',(-9.27831216351297,10.35,2.25));
#107515=CARTESIAN_POINT('Ctrl Pts',(-9.27831216351297,10.35,2.25));
#107516=CARTESIAN_POINT('Ctrl Pts',(-9.25132942976577,10.3769827337472,
2.29673546577726));
#107517=CARTESIAN_POINT('Ctrl Pts',(-9.22528140533409,10.4,2.34185196752971));
#107518=CARTESIAN_POINT('',(-9.38437367987071,10.4,2.25));
#107519=CARTESIAN_POINT('Ctrl Pts',(-9.38437367987072,10.4,2.25));
#107520=CARTESIAN_POINT('Ctrl Pts',(-9.33227763100738,10.3769827337472,
2.25));
#107521=CARTESIAN_POINT('Ctrl Pts',(-9.27831216351297,10.35,2.25));
#107522=CARTESIAN_POINT('',(-10.6156263201293,10.4,2.25));
#107523=CARTESIAN_POINT('Origin',(-10.,10.4,3.5));
#107524=CARTESIAN_POINT('',(-10.721687836487,10.35,2.25));
#107525=CARTESIAN_POINT('Ctrl Pts',(-10.721687836487,10.35,2.25));
#107526=CARTESIAN_POINT('Ctrl Pts',(-10.6677223689926,10.3769827337472,
2.25));
#107527=CARTESIAN_POINT('Ctrl Pts',(-10.6156263201293,10.4,2.25));
#107528=CARTESIAN_POINT('',(-10.7747185946659,10.4,2.34185196752971));
#107529=CARTESIAN_POINT('Ctrl Pts',(-10.7747185946659,10.4,2.34185196752971));
#107530=CARTESIAN_POINT('Ctrl Pts',(-10.7486705702342,10.3769827337472,
2.29673546577727));
#107531=CARTESIAN_POINT('Ctrl Pts',(-10.721687836487,10.35,2.25));
#107532=CARTESIAN_POINT('',(-11.3903449147952,10.4,3.4081480324703));
#107533=CARTESIAN_POINT('Origin',(-10.,10.4,3.5));
#107534=CARTESIAN_POINT('Ctrl Pts',(-11.4433756729741,10.35,3.5));
#107535=CARTESIAN_POINT('Ctrl Pts',(-11.4163929392269,10.3769827337472,
3.45326453422274));
#107536=CARTESIAN_POINT('Ctrl Pts',(-11.3903449147952,10.4,3.40814803247029));
#107537=CARTESIAN_POINT('',(-11.4933756729741,10.3,3.5));
#107538=CARTESIAN_POINT('Origin',(-10.,10.3,3.5));
#107539=CARTESIAN_POINT('',(-11.3903449147952,10.2,3.4081480324703));
#107540=CARTESIAN_POINT('',(-11.3903449147952,10.3,3.4081480324703));
#107541=CARTESIAN_POINT('',(-10.7747185946659,10.2,2.34185196752971));
#107542=CARTESIAN_POINT('',(-10.7747185946659,10.3,2.34185196752971));
#107543=CARTESIAN_POINT('Origin',(-10.,10.2,3.5));
#107544=CARTESIAN_POINT('Origin',(-10.,10.3,3.5));
#107545=CARTESIAN_POINT('',(-9.38437367987071,10.2,2.25));
#107546=CARTESIAN_POINT('',(-9.38437367987071,10.3,2.25));
#107547=CARTESIAN_POINT('',(-10.6156263201293,10.2,2.25));
#107548=CARTESIAN_POINT('Origin',(-10.,10.2,3.5));
#107549=CARTESIAN_POINT('',(-10.6156263201293,10.3,2.25));
#107550=CARTESIAN_POINT('Origin',(-10.,10.3,3.5));
#107551=CARTESIAN_POINT('',(-10.7747185946659,10.2,4.65814803247029));
#107552=CARTESIAN_POINT('',(-10.7747185946659,10.3,4.65814803247029));
#107553=CARTESIAN_POINT('',(-11.3903449147952,10.2,3.5918519675297));
#107554=CARTESIAN_POINT('',(-11.3903449147952,10.3,3.5918519675297));
#107555=CARTESIAN_POINT('Origin',(-10.,10.2,3.5));
#107556=CARTESIAN_POINT('Origin',(-10.,10.3,3.5));
#107557=CARTESIAN_POINT('',(-8.60965508520481,10.2,3.4081480324703));
#107558=CARTESIAN_POINT('',(-8.60965508520481,10.3,3.4081480324703));
#107559=CARTESIAN_POINT('',(-9.2252814053341,10.2,2.34185196752971));
#107560=CARTESIAN_POINT('Origin',(-10.,10.2,3.5));
#107561=CARTESIAN_POINT('',(-9.2252814053341,10.3,2.34185196752971));
#107562=CARTESIAN_POINT('Origin',(-10.,10.3,3.5));
#107563=CARTESIAN_POINT('',(-9.38437367987071,10.2,4.75));
#107564=CARTESIAN_POINT('',(-9.38437367987071,10.3,4.75));
#107565=CARTESIAN_POINT('',(-10.6156263201293,10.2,4.75));
#107566=CARTESIAN_POINT('',(-10.6156263201293,10.3,4.75));
#107567=CARTESIAN_POINT('Origin',(-10.,10.2,3.5));
#107568=CARTESIAN_POINT('Origin',(-10.,10.3,3.5));
#107569=CARTESIAN_POINT('',(-9.2252814053341,10.2,4.65814803247029));
#107570=CARTESIAN_POINT('',(-9.2252814053341,10.3,4.65814803247029));
#107571=CARTESIAN_POINT('',(-8.60965508520481,10.2,3.5918519675297));
#107572=CARTESIAN_POINT('Origin',(-10.,10.2,3.5));
#107573=CARTESIAN_POINT('',(-8.60965508520481,10.3,3.5918519675297));
#107574=CARTESIAN_POINT('Origin',(-10.721687836487,10.2,4.75));
#107575=CARTESIAN_POINT('',(-10.3608439182435,10.2,4.75));
#107576=CARTESIAN_POINT('',(-10.721687836487,11.5,4.75));
#107577=CARTESIAN_POINT('',(-10.721687836487,10.2,4.75));
#107578=CARTESIAN_POINT('',(-9.27831216351297,11.5,4.75));
#107579=CARTESIAN_POINT('',(-9.27831216351297,11.5,4.75));
#107580=CARTESIAN_POINT('',(-9.27831216351297,10.2,4.75));
#107581=CARTESIAN_POINT('Origin',(-11.4433756729741,10.2,3.5));
#107582=CARTESIAN_POINT('',(-11.2629537138523,10.2,3.8125));
#107583=CARTESIAN_POINT('',(-11.4433756729741,11.5,3.5));
#107584=CARTESIAN_POINT('',(-11.4433756729741,10.2,3.5));
#107585=CARTESIAN_POINT('',(-10.721687836487,11.5,4.75));
#107586=CARTESIAN_POINT('Origin',(-10.721687836487,10.2,2.25));
#107587=CARTESIAN_POINT('',(-10.9021097956088,10.2,2.5625));
#107588=CARTESIAN_POINT('',(-10.721687836487,11.5,2.25));
#107589=CARTESIAN_POINT('',(-10.721687836487,10.2,2.25));
#107590=CARTESIAN_POINT('',(-11.4433756729741,11.5,3.5));
#107591=CARTESIAN_POINT('Origin',(-10.,10.2,3.5));
#107592=CARTESIAN_POINT('Origin',(-10.,10.2,3.5));
#107593=CARTESIAN_POINT('Origin',(-10.,10.2,3.5));
#107594=CARTESIAN_POINT('',(-9.63915608175648,10.2,2.25));
#107595=CARTESIAN_POINT('Origin',(-10.,10.2,3.5));
#107596=CARTESIAN_POINT('Origin',(-10.,10.2,3.5));
#107597=CARTESIAN_POINT('',(-8.7370462861477,10.2,3.1875));
#107598=CARTESIAN_POINT('Origin',(-10.,10.2,3.5));
#107599=CARTESIAN_POINT('',(-9.09789020439121,10.2,4.4375));
#107600=CARTESIAN_POINT('Origin',(-10.,11.5,3.5));
#107601=CARTESIAN_POINT('',(-8.55662432702594,11.5,3.5));
#107602=CARTESIAN_POINT('',(-9.27831216351297,11.5,2.25));
#107603=CARTESIAN_POINT('',(-9.27831216351297,11.5,2.25));
#107604=CARTESIAN_POINT('Origin',(-10.,11.5,3.5));
#107605=CARTESIAN_POINT('Origin',(-10.,11.5,3.5));
#107606=CARTESIAN_POINT('',(-10.721687836487,11.5,2.25));
#107607=CARTESIAN_POINT('Origin',(-10.,11.5,3.5));
#107608=CARTESIAN_POINT('Origin',(-10.,11.5,3.5));
#107609=CARTESIAN_POINT('Origin',(-10.,11.5,3.5));
#107610=CARTESIAN_POINT('Origin',(-10.,11.5,3.5));
#107611=CARTESIAN_POINT('Origin',(-10.,11.5,3.5));
#107612=CARTESIAN_POINT('Origin',(-10.,11.5,3.5));
#107613=CARTESIAN_POINT('Origin',(-10.,11.5,3.5));
#107614=CARTESIAN_POINT('Origin',(-10.,11.5,3.5));
#107615=CARTESIAN_POINT('',(-8.55662432702594,11.5,3.5));
#107616=CARTESIAN_POINT('Origin',(-10.,11.5,3.5));
#107617=CARTESIAN_POINT('Origin',(-10.,11.9336338001763,3.5));
#107618=CARTESIAN_POINT('',(-10.,12.3672676003525,3.5));
#107619=CARTESIAN_POINT('',(-10.721687836487,11.9336338001763,3.5));
#107620=CARTESIAN_POINT('Origin',(-8.55662432702594,10.2,3.5));
#107621=CARTESIAN_POINT('',(-8.55662432702594,10.2,3.5));
#107622=CARTESIAN_POINT('',(-9.27831216351297,10.2,2.25));
#107623=CARTESIAN_POINT('Origin',(-9.27831216351297,10.2,4.75));
#107624=CARTESIAN_POINT('Origin',(-9.27831216351297,10.2,2.25));
#107625=CARTESIAN_POINT('',(0.,0.,0.));
#107626=CARTESIAN_POINT('Origin',(-10.,3.5,11.));
#107627=CARTESIAN_POINT('',(-11.4635,3.76156981780296,11.0000000019885));
#107628=CARTESIAN_POINT('',(-11.4634991533828,3.68934495415709,10.9984258183648));
#107629=CARTESIAN_POINT('',(-11.4635,3.5,11.));
#107630=CARTESIAN_POINT('',(-9.36565826844269,3.60066707712968,9.6811206205771));
#107631=CARTESIAN_POINT('Ctrl Pts',(-11.4635,3.76156981780296,11.0000000019885));
#107632=CARTESIAN_POINT('Ctrl Pts',(-11.4635000000624,3.75928323455344,
10.9540845300718));
#107633=CARTESIAN_POINT('Ctrl Pts',(-11.4613391785855,3.7569468082902,10.9081937237433));
#107634=CARTESIAN_POINT('Ctrl Pts',(-11.4562760707715,3.75407978255904,
10.8545499913958));
#107635=CARTESIAN_POINT('Ctrl Pts',(-11.4554628663213,3.75365277919035,
10.8466261482596));
#107636=CARTESIAN_POINT('Ctrl Pts',(-11.4541266745868,3.75299753308779,
10.8345758123366));
#107637=CARTESIAN_POINT('Ctrl Pts',(-11.453650698948,3.75277181702621,10.8304441325523));
#107638=CARTESIAN_POINT('Ctrl Pts',(-11.4527573751666,3.75236150731869,
10.8229700458294));
#107639=CARTESIAN_POINT('Ctrl Pts',(-11.4523460931523,3.7521772514568,10.8196269951759));
#107640=CARTESIAN_POINT('Ctrl Pts',(-11.4514092663413,3.75176756419203,
10.8122231170571));
#107641=CARTESIAN_POINT('Ctrl Pts',(-11.4508782205965,3.75154183540335,
10.8081630787565));
#107642=CARTESIAN_POINT('Ctrl Pts',(-11.4492828561814,3.75088213419359,
10.796351600552));
#107643=CARTESIAN_POINT('Ctrl Pts',(-11.4481734220193,3.75044577390274,
10.7886065230668));
#107644=CARTESIAN_POINT('Ctrl Pts',(-11.4386008915863,3.74685556954419,
10.7253950659656));
#107645=CARTESIAN_POINT('Ctrl Pts',(-11.4270172341977,3.74355475161639,
10.6704533723633));
#107646=CARTESIAN_POINT('Ctrl Pts',(-11.3745844567709,3.73160803816701,
10.4774514069699));
#107647=CARTESIAN_POINT('Ctrl Pts',(-11.3165714936372,3.7228421766896,10.3448701326712));
#107648=CARTESIAN_POINT('Ctrl Pts',(-11.230883367043,3.71380732535996,10.2081277259522));
#107649=CARTESIAN_POINT('Ctrl Pts',(-11.2213726482237,3.71284163789666,
10.1935358331985));
#107650=CARTESIAN_POINT('Ctrl Pts',(-11.2071489353362,3.71144945541935,
10.1725419843163));
#107651=CARTESIAN_POINT('Ctrl Pts',(-11.2026409287824,3.71101545406395,
10.1660035253833));
#107652=CARTESIAN_POINT('Ctrl Pts',(-11.1945597899482,3.71025002039912,
10.1544843431643));
#107653=CARTESIAN_POINT('Ctrl Pts',(-11.1910081967787,3.70991779345025,
10.149488804016));
#107654=CARTESIAN_POINT('Ctrl Pts',(-11.183551393156,3.70922881005415,10.1391386469318));
#107655=CARTESIAN_POINT('Ctrl Pts',(-11.1796409781286,3.70887226102982,
10.1337879392841));
#107656=CARTESIAN_POINT('Ctrl Pts',(-11.1693867808877,3.70794942744629,
10.1199551197653));
#107657=CARTESIAN_POINT('Ctrl Pts',(-11.1629869634305,3.70738529574889,
10.1115149043245));
#107658=CARTESIAN_POINT('Ctrl Pts',(-11.1341557265686,3.70489468741467,
10.0743369878939));
#107659=CARTESIAN_POINT('Ctrl Pts',(-11.1107459145355,3.70300644783047,
10.0463727059592));
#107660=CARTESIAN_POINT('Ctrl Pts',(-11.0423592439328,3.69781349960447,
9.97062045404308));
#107661=CARTESIAN_POINT('Ctrl Pts',(-10.9951780407876,3.69459183261759,
9.92493885221194));
#107662=CARTESIAN_POINT('Ctrl Pts',(-10.8670877841723,3.68640728329733,
9.81660338351391));
#107663=CARTESIAN_POINT('Ctrl Pts',(-10.7824025313501,3.68150410237404,
9.75898836082052));
#107664=CARTESIAN_POINT('Ctrl Pts',(-10.6828185260105,3.67553997822639,
9.70550783553445));
#107665=CARTESIAN_POINT('Ctrl Pts',(-10.6731568845148,3.67495926161974,
9.70045742720849));
#107666=CARTESIAN_POINT('Ctrl Pts',(-10.6591947605846,3.6741158372041,9.69335651332966));
#107667=CARTESIAN_POINT('Ctrl Pts',(-10.6549390623499,3.67385820065167,
9.69121821643585));
#107668=CARTESIAN_POINT('Ctrl Pts',(-10.6476190029936,3.67341396908673,
9.68758485905051));
#107669=CARTESIAN_POINT('Ctrl Pts',(-10.6445597469403,3.67322798585676,
9.68607967989761));
#107670=CARTESIAN_POINT('Ctrl Pts',(-10.6412433593453,3.6730260062026,9.68446235986725));
#107671=CARTESIAN_POINT('Ctrl Pts',(-10.6409914789954,3.67301066358095,
9.68433961359115));
#107672=CARTESIAN_POINT('Ctrl Pts',(-10.6406699375262,3.67299107491475,
9.68418303432902));
#107673=CARTESIAN_POINT('Ctrl Pts',(-10.6406003087526,3.67298683288301,
9.68414913442919));
#107674=CARTESIAN_POINT('Ctrl Pts',(-10.6404706537734,3.67297893352799,
9.68408602252596));
#107675=CARTESIAN_POINT('Ctrl Pts',(-10.6404106282497,3.67297527628957,
9.684056809098));
#107676=CARTESIAN_POINT('Ctrl Pts',(-10.6402987106879,3.67296845713685,
9.68400235014591));
#107677=CARTESIAN_POINT('Ctrl Pts',(-10.6402468191287,3.67296529528336,
9.68397710357088));
#107678=CARTESIAN_POINT('Ctrl Pts',(-10.6401499589466,3.67295939322996,
9.68392998569179));
#107679=CARTESIAN_POINT('Ctrl Pts',(-10.6401049906925,3.6729566530758,9.6839081136216));
#107680=CARTESIAN_POINT('Ctrl Pts',(-10.6400209719959,3.67295153324019,
9.68386725316521));
#107681=CARTESIAN_POINT('Ctrl Pts',(-10.639981921824,3.67294915359248,9.68384826420967));
#107682=CARTESIAN_POINT('Ctrl Pts',(-10.6399088988077,3.67294470360158,
9.68381275927257));
#107683=CARTESIAN_POINT('Ctrl Pts',(-10.6398749262358,3.67294263328786,
9.68379624290097));
#107684=CARTESIAN_POINT('Ctrl Pts',(-10.639802862946,3.67293824161285,9.683761211497));
#107685=CARTESIAN_POINT('Ctrl Pts',(-10.6397647720017,3.67293592022751,
9.68374269677266));
#107686=CARTESIAN_POINT('Ctrl Pts',(-10.6396897405693,3.67293134747059,
9.68370623054835));
#107687=CARTESIAN_POINT('Ctrl Pts',(-10.6396528001962,3.672929096109,9.6836882789825));
#107688=CARTESIAN_POINT('Ctrl Pts',(-10.6395800200727,3.67292466037136,
9.68365291449727));
#107689=CARTESIAN_POINT('Ctrl Pts',(-10.6395441803077,3.67292247599718,
9.68363550145781));
#107690=CARTESIAN_POINT('Ctrl Pts',(-10.6394735542032,3.67291817136605,
9.68360119075929));
#107691=CARTESIAN_POINT('Ctrl Pts',(-10.6394387678749,3.67291605111234,
9.68358429300076));
#107692=CARTESIAN_POINT('Ctrl Pts',(-10.6393702040009,3.67291187200881,
9.68355099086755));
#107693=CARTESIAN_POINT('Ctrl Pts',(-10.639336426533,3.67290981316611,9.68353458643304));
#107694=CARTESIAN_POINT('Ctrl Pts',(-10.6392698382736,3.67290575432521,
9.6835022502093));
#107695=CARTESIAN_POINT('Ctrl Pts',(-10.6392370275452,3.67290375433308,
9.68348631835994));
#107696=CARTESIAN_POINT('Ctrl Pts',(-10.6391723331431,3.67289981078479,
9.68345490779823));
#107697=CARTESIAN_POINT('Ctrl Pts',(-10.6391404494302,3.67289786722832,
9.68343942898236));
#107698=CARTESIAN_POINT('Ctrl Pts',(-10.6390775712215,3.67289403425102,
9.68340890586767));
#107699=CARTESIAN_POINT('Ctrl Pts',(-10.6390465768076,3.67289214483712,
9.68339386152979));
#107700=CARTESIAN_POINT('Ctrl Pts',(-10.6389854416086,3.67288841798128,
9.68336418986316));
#107701=CARTESIAN_POINT('Ctrl Pts',(-10.6389553008488,3.67288658054267,
9.68334956247316));
#107702=CARTESIAN_POINT('Ctrl Pts',(-10.6388958392237,3.67288295558627,
9.68332070811273));
#107703=CARTESIAN_POINT('Ctrl Pts',(-10.6388665183607,3.6728811680703,9.68330648107476));
#107704=CARTESIAN_POINT('Ctrl Pts',(-10.6388086643959,3.67287764100519,
9.68327841162284));
#107705=CARTESIAN_POINT('Ctrl Pts',(-10.6387801313542,3.67287590146129,
9.68326456917388));
#107706=CARTESIAN_POINT('Ctrl Pts',(-10.638723822775,3.67287246850038,9.6832372540307));
#107707=CARTESIAN_POINT('Ctrl Pts',(-10.6386960472265,3.67287077508415,
9.68322378127099));
#107708=CARTESIAN_POINT('Ctrl Pts',(-10.6386412245604,3.67286743261041,
9.68319719122579));
#107709=CARTESIAN_POINT('Ctrl Pts',(-10.6386141775498,3.6728657835608,9.68318407393591));
#107710=CARTESIAN_POINT('Ctrl Pts',(-10.6385607848509,3.67286252817158,
9.68315818151615));
#107711=CARTESIAN_POINT('Ctrl Pts',(-10.6385344390814,3.6728609218283,9.68314540629411));
#107712=CARTESIAN_POINT('Ctrl Pts',(-10.6384824225997,3.67285775025418,
9.68312018511746));
#107713=CARTESIAN_POINT('Ctrl Pts',(-10.6384567519562,3.67285618502872,
9.68310773914664));
#107714=CARTESIAN_POINT('Ctrl Pts',(-10.6384060609823,3.67285309418509,
9.68308316432884));
#107715=CARTESIAN_POINT('Ctrl Pts',(-10.6383810406905,3.67285156857039,
9.68307103545405));
#107716=CARTESIAN_POINT('Ctrl Pts',(-10.6383316268515,3.67284855551457,
9.68304708326534));
#107717=CARTESIAN_POINT('Ctrl Pts',(-10.638307233336,3.67284706807643,9.68303525992313));
#107718=CARTESIAN_POINT('Ctrl Pts',(-10.6382590505208,3.67284413000316,
9.68301190775047));
#107719=CARTESIAN_POINT('Ctrl Pts',(-10.6382352612765,3.67284267937239,
9.68300037890587));
#107720=CARTESIAN_POINT('Ctrl Pts',(-10.6381882657558,3.67283981362117,
9.68297760530938));
#107721=CARTESIAN_POINT('Ctrl Pts',(-10.6381650594227,3.67283839849819,
9.68296636049148));
#107722=CARTESIAN_POINT('Ctrl Pts',(-10.6381192093571,3.67283560252335,
9.6829441449648));
#107723=CARTESIAN_POINT('Ctrl Pts',(-10.6380965655761,3.6728342216694,9.68293317419612));
#107724=CARTESIAN_POINT('Ctrl Pts',(-10.6380518209419,3.67283149303557,
9.68291149712869));
#107725=CARTESIAN_POINT('Ctrl Pts',(-10.6380297201757,3.67283014526182,
9.68290079083785));
#107726=CARTESIAN_POINT('Ctrl Pts',(-10.6379860431233,3.67282748166586,
9.68287963368769));
#107727=CARTESIAN_POINT('Ctrl Pts',(-10.6379644668303,3.67282616584401,
9.68286918279287));
#107728=CARTESIAN_POINT('Ctrl Pts',(-10.6379218210235,3.67282356507472,
9.68284852776526));
#107729=CARTESIAN_POINT('Ctrl Pts',(-10.637900751503,3.67282228012761,9.68283832359883));
#107730=CARTESIAN_POINT('Ctrl Pts',(-10.6340957948628,3.67259022807093,
9.68099566011124));
#107731=CARTESIAN_POINT('Ctrl Pts',(-10.630304075875,3.67235849603446,9.67917953651132));
#107732=CARTESIAN_POINT('Ctrl Pts',(-10.6223412854083,3.67187091114326,
9.67540768643617));
#107733=CARTESIAN_POINT('Ctrl Pts',(-10.6181687044318,3.67161487634773,
9.67345526858665));
#107734=CARTESIAN_POINT('Ctrl Pts',(-10.5939129155798,3.67012370939006,
9.66224488605167));
#107735=CARTESIAN_POINT('Ctrl Pts',(-10.5736321125373,3.66886583557573,
9.65342382575651));
#107736=CARTESIAN_POINT('Ctrl Pts',(-10.5151047183265,3.66522010217662,
9.62952964509481));
#107737=CARTESIAN_POINT('Ctrl Pts',(-10.4764133352891,3.66279159045909,
9.61560416173461));
#107738=CARTESIAN_POINT('Ctrl Pts',(-10.394635829856,3.65768531922315,9.59000600742252));
#107739=CARTESIAN_POINT('Ctrl Pts',(-10.3514957064976,3.65500670078497,
9.57863753186562));
#107740=CARTESIAN_POINT('Ctrl Pts',(-10.2157524381356,3.64671647490178,
9.54942482909924));
#107741=CARTESIAN_POINT('Ctrl Pts',(-10.1218888162979,3.64119769998302,
9.5385399617413));
#107742=CARTESIAN_POINT('Ctrl Pts',(-10.0155701495009,3.63528987767549,
9.53653321439832));
#107743=CARTESIAN_POINT('Ctrl Pts',(-10.0035193113381,3.6346248433307,9.53645461687845));
#107744=CARTESIAN_POINT('Ctrl Pts',(-9.98376715523786,3.63354214859706,
9.53656976272105));
#107745=CARTESIAN_POINT('Ctrl Pts',(-9.97606606332483,3.6331218491377,9.53667545144304));
#107746=CARTESIAN_POINT('Ctrl Pts',(-9.96222203785887,3.63236949464247,
9.5369747636302));
#107747=CARTESIAN_POINT('Ctrl Pts',(-9.95607884911573,3.63203677767909,
9.53714629892512));
#107748=CARTESIAN_POINT('Ctrl Pts',(-9.94297929968529,3.6313296623974,9.53759466833822));
#107749=CARTESIAN_POINT('Ctrl Pts',(-9.93602345000046,3.63095560527962,
9.53788245423457));
#107750=CARTESIAN_POINT('Ctrl Pts',(-9.91719855108318,3.629946993374,9.53879589745609));
#107751=CARTESIAN_POINT('Ctrl Pts',(-9.90533450443742,3.62931533774236,
9.53951653070841));
#107752=CARTESIAN_POINT('Ctrl Pts',(-9.84203160136382,3.6259648265879,9.54413623488598));
#107753=CARTESIAN_POINT('Ctrl Pts',(-9.79081467319214,3.62332573743453,
9.55060856387685));
#107754=CARTESIAN_POINT('Ctrl Pts',(-9.61033444665143,3.61414547291448,
9.5831847917179));
#107755=CARTESIAN_POINT('Ctrl Pts',(-9.48440197132043,3.60801057640892,
9.62400730170195));
#107756=CARTESIAN_POINT('Ctrl Pts',(-9.36564806195114,3.60128744213858,
9.68112552959212));
#107757=CARTESIAN_POINT('',(-10.6340070945752,3.6,9.68095972236316));
#107758=CARTESIAN_POINT('Origin',(-10.,3.6,11.));
#107759=CARTESIAN_POINT('Ctrl Pts',(-10.6340070945752,3.6,9.68095972236315));
#107760=CARTESIAN_POINT('Ctrl Pts',(-10.6850513968777,3.60307949391912,
9.70549456814919));
#107761=CARTESIAN_POINT('Ctrl Pts',(-10.7347103886682,3.60615898783824,
9.7330158864931));
#107762=CARTESIAN_POINT('Ctrl Pts',(-10.7826290695724,3.60923848175736,
9.76334160357025));
#107763=CARTESIAN_POINT('Ctrl Pts',(-10.8305243595235,3.61231647245693,
9.79365251749729));
#107764=CARTESIAN_POINT('Ctrl Pts',(-10.8766806071727,3.6153944631565,9.82676485276805));
#107765=CARTESIAN_POINT('Ctrl Pts',(-10.9207691913895,3.61847245385607,
9.86245160710065));
#107766=CARTESIAN_POINT('Ctrl Pts',(-10.9648471405381,3.62154970208133,
9.89812975305819));
#107767=CARTESIAN_POINT('Ctrl Pts',(-11.0068580336482,3.62462695030659,
9.93638077499454));
#107768=CARTESIAN_POINT('Ctrl Pts',(-11.0465054999892,3.62770419853185,
9.97693671334934));
#107769=CARTESIAN_POINT('Ctrl Pts',(-11.0861557437108,3.63078166232422,
10.017495492725));
#107770=CARTESIAN_POINT('Ctrl Pts',(-11.1234418877901,3.63385912611659,
10.0603591562058));
#107771=CARTESIAN_POINT('Ctrl Pts',(-11.158105019341,3.63693658990896,10.1052234836691));
#107772=CARTESIAN_POINT('Ctrl Pts',(-11.1927813699806,3.64001522731909,
10.1501049205366));
#107773=CARTESIAN_POINT('Ctrl Pts',(-11.2248324210782,3.64309386472922,
10.1969881460308));
#107774=CARTESIAN_POINT('Ctrl Pts',(-11.2540412311563,3.64617250213935,
10.2455380456511));
#107775=CARTESIAN_POINT('Ctrl Pts',(-11.2832941999661,3.64925579392338,
10.2941613444267));
#107776=CARTESIAN_POINT('Ctrl Pts',(-11.3096960963109,3.65233908570741,
10.3444559234168));
#107777=CARTESIAN_POINT('Ctrl Pts',(-11.3330752825907,3.65542237749143,
10.3960608135369));
#107778=CARTESIAN_POINT('Ctrl Pts',(-11.3564733874392,3.65850816429248,
10.4477074626237));
#107779=CARTESIAN_POINT('Ctrl Pts',(-11.376843732178,3.66159395109352,10.5006660748198));
#107780=CARTESIAN_POINT('Ctrl Pts',(-11.3940634951727,3.66467973789456,
10.5545572748076));
#107781=CARTESIAN_POINT('Ctrl Pts',(-11.4113186639751,3.66777186942717,
10.6085592812834));
#107782=CARTESIAN_POINT('Ctrl Pts',(-11.4254101882224,3.67086400095979,
10.6634972277376));
#107783=CARTESIAN_POINT('Ctrl Pts',(-11.4362657981855,3.6739561324924,10.718978991955));
#107784=CARTESIAN_POINT('Ctrl Pts',(-11.4421490956222,3.67563194155163,
10.7490478432044));
#107785=CARTESIAN_POINT('Ctrl Pts',(-11.447082837701,3.67730775061086,10.7792762882384));
#107786=CARTESIAN_POINT('Ctrl Pts',(-11.4510618967054,3.67898355967009,
10.8096014130053));
#107787=CARTESIAN_POINT('Ctrl Pts',(-11.4592626321064,3.68243735783242,
10.8721006933471));
#107788=CARTESIAN_POINT('Ctrl Pts',(-11.4634311218865,3.68589115599475,
10.9351776930672));
#107789=CARTESIAN_POINT('Ctrl Pts',(-11.4634991533828,3.68934495415709,
10.9984258183648));
#107790=CARTESIAN_POINT('Origin',(-10.,3.5,11.));
#107791=CARTESIAN_POINT('',(-11.4635,4.25936781471288,11.0000000001943));
#107792=CARTESIAN_POINT('',(-11.4634999508678,4.19066505394721,10.9996207769711));
#107793=CARTESIAN_POINT('',(-11.4635,3.5,11.));
#107794=CARTESIAN_POINT('Ctrl Pts',(-11.4635,4.25936781471288,11.0000000001943));
#107795=CARTESIAN_POINT('Ctrl Pts',(-11.4635000000009,4.25902532594864,
10.9934975786898));
#107796=CARTESIAN_POINT('Ctrl Pts',(-11.4634566640214,4.25868411486387,
10.9869950464565));
#107797=CARTESIAN_POINT('Ctrl Pts',(-11.4624819664045,4.25486105431314,
10.9138761111745));
#107798=CARTESIAN_POINT('Ctrl Pts',(-11.4570462164854,4.25151849227137,
10.8473945935954));
#107799=CARTESIAN_POINT('Ctrl Pts',(-11.4349561851339,4.24423808160547,
10.7010888593856));
#107800=CARTESIAN_POINT('Ctrl Pts',(-11.4161317145643,4.24034623495184,
10.6218235698782));
#107801=CARTESIAN_POINT('Ctrl Pts',(-11.3748965878244,4.23377647577659,
10.4959068745586));
#107802=CARTESIAN_POINT('Ctrl Pts',(-11.3564340745739,4.23118570966055,
10.4481520862128));
#107803=CARTESIAN_POINT('Ctrl Pts',(-11.3325366186803,4.22807649401993,
10.394829516972));
#107804=CARTESIAN_POINT('Ctrl Pts',(-11.3295125724275,4.22768684870793,
10.3882145235923));
#107805=CARTESIAN_POINT('Ctrl Pts',(-11.3245933241023,4.22705857471218,
10.3776625798055));
#107806=CARTESIAN_POINT('Ctrl Pts',(-11.3227295443383,4.22682177218674,
10.373711016886));
#107807=CARTESIAN_POINT('Ctrl Pts',(-11.319386514376,4.2263990950339,10.3667046537964));
#107808=CARTESIAN_POINT('Ctrl Pts',(-11.3179142970722,4.22621364818248,
10.3636465799442));
#107809=CARTESIAN_POINT('Ctrl Pts',(-11.3147296349514,4.22581394181117,
10.3570898904234));
#107810=CARTESIAN_POINT('Ctrl Pts',(-11.3130138844915,4.22559948891633,
10.3535930380753));
#107811=CARTESIAN_POINT('Ctrl Pts',(-11.3082188104421,4.22500268554567,
10.3439181110308));
#107812=CARTESIAN_POINT('Ctrl Pts',(-11.3051097448193,4.22461857645875,
10.3377549915668));
#107813=CARTESIAN_POINT('Ctrl Pts',(-11.2869922682685,4.22239740661244,
10.3024637258214));
#107814=CARTESIAN_POINT('Ctrl Pts',(-11.2710535368334,4.22050982010397,
10.2738260923971));
#107815=CARTESIAN_POINT('Ctrl Pts',(-11.2144743116127,4.21407730220086,
10.1797460725453));
#107816=CARTESIAN_POINT('Ctrl Pts',(-11.1696328919382,4.20940319389579,
10.1169809133202));
#107817=CARTESIAN_POINT('Ctrl Pts',(-11.0577195639985,4.19897244948248,
9.98390776972589));
#107818=CARTESIAN_POINT('Ctrl Pts',(-10.9881634055467,4.19328350564014,
9.91613991937271));
#107819=CARTESIAN_POINT('Ctrl Pts',(-10.902996436888,4.18722905409278,9.84822978531838));
#107820=CARTESIAN_POINT('Ctrl Pts',(-10.8934909156783,4.18656443193835,
9.84084030945967));
#107821=CARTESIAN_POINT('Ctrl Pts',(-10.8778119624781,4.18548594264641,
9.82895915447156));
#107822=CARTESIAN_POINT('Ctrl Pts',(-10.8716927900577,4.18506936017406,
9.82439709671948));
#107823=CARTESIAN_POINT('Ctrl Pts',(-10.8606614008153,4.18432599134863,
9.81630629857245));
#107824=CARTESIAN_POINT('Ctrl Pts',(-10.8557625012729,4.18399852730871,
9.81275976795615));
#107825=CARTESIAN_POINT('Ctrl Pts',(-10.8453055400798,4.18330509621986,
9.80528786251275));
#107826=CARTESIAN_POINT('Ctrl Pts',(-10.8397417909755,4.18293944414606,
9.80137066856863));
#107827=CARTESIAN_POINT('Ctrl Pts',(-10.8247039285546,4.18195984130277,
9.79093926206517));
#107828=CARTESIAN_POINT('Ctrl Pts',(-10.8151799319174,4.18134860991019,
9.78449758273484));
#107829=CARTESIAN_POINT('Ctrl Pts',(-10.7657127214036,4.17821941567478,
9.75188273989734));
#107830=CARTESIAN_POINT('Ctrl Pts',(-10.7245799218045,4.17576991415896,
9.72756250009926));
#107831=CARTESIAN_POINT('Ctrl Pts',(-10.5860427122453,4.16790447436724,
9.65455133606497));
#107832=CARTESIAN_POINT('Ctrl Pts',(-10.4844024470744,4.16275036782057,
9.61470892577944));
#107833=CARTESIAN_POINT('Ctrl Pts',(-10.3296849698857,4.15480856973996,
9.57319322343475));
#107834=CARTESIAN_POINT('Ctrl Pts',(-10.2794212567143,4.15220878469236,
9.56250477510039));
#107835=CARTESIAN_POINT('Ctrl Pts',(-10.22151324667,4.1490892384097,9.55334276700885));
#107836=CARTESIAN_POINT('Ctrl Pts',(-10.2143130980492,4.14869917941742,
9.55225860045987));
#107837=CARTESIAN_POINT('Ctrl Pts',(-10.2027772842615,4.14807033150747,
9.55060952895859));
#107838=CARTESIAN_POINT('Ctrl Pts',(-10.1984465687697,4.14783337280801,
9.55001023351723));
#107839=CARTESIAN_POINT('Ctrl Pts',(-10.1907474716124,4.14741044648355,
9.54897995063021));
#107840=CARTESIAN_POINT('Ctrl Pts',(-10.1873801946584,4.14722490719728,
9.54854127029223));
#107841=CARTESIAN_POINT('Ctrl Pts',(-10.1801450014133,4.14682499289747,
9.5476242850908));
#107842=CARTESIAN_POINT('Ctrl Pts',(-10.1762767539655,4.14661042436716,
9.54714971725238));
#107843=CARTESIAN_POINT('Ctrl Pts',(-10.1655501883383,4.14601342115145,
9.54587722026402));
#107844=CARTESIAN_POINT('Ctrl Pts',(-10.158688138685,4.14562922905592,9.54511237745438));
#107845=CARTESIAN_POINT('Ctrl Pts',(-10.1192591053765,4.14340963137147,
9.54099988621677));
#107846=CARTESIAN_POINT('Ctrl Pts',(-10.0865946246977,4.14152384108607,
9.53869745653475));
#107847=CARTESIAN_POINT('Ctrl Pts',(-9.97703812012236,4.13510086996666,
9.53466107879946));
#107848=CARTESIAN_POINT('Ctrl Pts',(-9.90009195140336,4.13043505181022,
9.53789082686124));
#107849=CARTESIAN_POINT('Ctrl Pts',(-9.72760709132496,4.12001305109543,
9.55881457973886));
#107850=CARTESIAN_POINT('Ctrl Pts',(-9.63283846661595,4.11432459966961,
9.57999605338088));
#107851=CARTESIAN_POINT('Ctrl Pts',(-9.5294153479113,4.10827049964071,9.61416910888153));
#107852=CARTESIAN_POINT('Ctrl Pts',(-9.51803155698666,4.1076059269297,9.61808697610765));
#107853=CARTESIAN_POINT('Ctrl Pts',(-9.49951013454301,4.10652741164867,
9.62471805842435));
#107854=CARTESIAN_POINT('Ctrl Pts',(-9.49234325988269,4.1061107562891,9.62734739954439));
#107855=CARTESIAN_POINT('Ctrl Pts',(-9.47953373417776,4.1053671883899,9.63216093048103));
#107856=CARTESIAN_POINT('Ctrl Pts',(-9.47388347253239,4.10503959868816,
9.63432424968306));
#107857=CARTESIAN_POINT('Ctrl Pts',(-9.46190380532984,4.10434582774548,
9.63899629416874));
#107858=CARTESIAN_POINT('Ctrl Pts',(-9.45557814944251,4.10397996220359,
9.64151427951083));
#107859=CARTESIAN_POINT('Ctrl Pts',(-9.43860860061271,4.10299960445534,
9.64840672941961));
#107860=CARTESIAN_POINT('Ctrl Pts',(-9.42799823294832,4.10238783645299,
9.6528627906235));
#107861=CARTESIAN_POINT('Ctrl Pts',(-9.37354193673367,4.09925284569418,
9.67649232937693));
#107862=CARTESIAN_POINT('Ctrl Pts',(-9.33060098972898,4.09679837199659,
9.69768367318154));
#107863=CARTESIAN_POINT('Ctrl Pts',(-9.19321779772954,4.08890377083662,
9.77407641669106));
#107864=CARTESIAN_POINT('Ctrl Pts',(-9.10392339858117,4.08372818152984,
9.8377471299721));
#107865=CARTESIAN_POINT('Ctrl Pts',(-8.98472230561747,4.07578415129803,
9.94471464098695));
#107866=CARTESIAN_POINT('Ctrl Pts',(-8.94868865692762,4.07320954238742,
9.98060828185785));
#107867=CARTESIAN_POINT('Ctrl Pts',(-8.90972642669894,4.07011876376522,
10.0236862493227));
#107868=CARTESIAN_POINT('Ctrl Pts',(-8.90489459937282,4.06972965837293,
10.0291090886872));
#107869=CARTESIAN_POINT('Ctrl Pts',(-8.89722285460441,4.06910205929221,
10.0378493436846));
#107870=CARTESIAN_POINT('Ctrl Pts',(-8.894357013495,4.06886538443477,10.0411439611423));
#107871=CARTESIAN_POINT('Ctrl Pts',(-8.88929047445153,4.06844288072918,
10.0470214514402));
#107872=CARTESIAN_POINT('Ctrl Pts',(-8.8870839602853,4.06825747885049,10.0495992147901));
#107873=CARTESIAN_POINT('Ctrl Pts',(-8.88236472824535,4.06785789790903,
10.0551514355703));
#107874=CARTESIAN_POINT('Ctrl Pts',(-8.87985495103988,4.06764352568938,
10.0581282046149));
#107875=CARTESIAN_POINT('Ctrl Pts',(-8.87292647403023,4.06704661440199,
10.0664127173652));
#107876=CARTESIAN_POINT('Ctrl Pts',(-8.86853347967118,4.06666231205731,
10.0717417079311));
#107877=CARTESIAN_POINT('Ctrl Pts',(-8.84343365158452,4.06443367406926,
10.1026323475469));
#107878=CARTESIAN_POINT('Ctrl Pts',(-8.82355702798911,4.06253835793603,
10.1288536075467));
#107879=CARTESIAN_POINT('Ctrl Pts',(-8.75979856923863,4.05606133986969,
10.2191293539086));
#107880=CARTESIAN_POINT('Ctrl Pts',(-8.72013237741204,4.0513485978988,10.2859993770333));
#107881=CARTESIAN_POINT('Ctrl Pts',(-8.64362129402592,4.04092436659841,
10.4420422886716));
#107882=CARTESIAN_POINT('Ctrl Pts',(-8.60989244312836,4.03527841007388,
10.5323608541549));
#107883=CARTESIAN_POINT('Ctrl Pts',(-8.5821864869836,4.02926290781066,10.6369822019807));
#107884=CARTESIAN_POINT('Ctrl Pts',(-8.57924924226182,4.02859855366428,
10.6486534817777));
#107885=CARTESIAN_POINT('Ctrl Pts',(-8.57468616676362,4.02752062677492,
10.667778838211));
#107886=CARTESIAN_POINT('Ctrl Pts',(-8.57297410343424,4.02710433720996,
10.6752115809375));
#107887=CARTESIAN_POINT('Ctrl Pts',(-8.57001003934691,4.02636157421692,
10.688555832201));
#107888=CARTESIAN_POINT('Ctrl Pts',(-8.56873640419713,4.02603442281965,
10.6944623131808));
#107889=CARTESIAN_POINT('Ctrl Pts',(-8.56610798219057,4.02534174409984,
10.707028807842));
#107890=CARTESIAN_POINT('Ctrl Pts',(-8.56476293228192,4.02497653071097,
10.713690727108));
#107891=CARTESIAN_POINT('Ctrl Pts',(-8.56127089511812,4.0239983324744,10.7316297529902));
#107892=CARTESIAN_POINT('Ctrl Pts',(-8.55921007983556,4.02338805989919,
10.7429232748398));
#107893=CARTESIAN_POINT('Ctrl Pts',(-8.54928908673348,4.02026797403415,
10.8011638252084));
#107894=CARTESIAN_POINT('Ctrl Pts',(-8.54358942585577,4.01782622003179,
10.8484519850405));
#107895=CARTESIAN_POINT('Ctrl Pts',(-8.5325229658762,4.01000866402875,11.0036926808674));
#107896=CARTESIAN_POINT('Ctrl Pts',(-8.53679592890457,4.00489055417382,
11.1119614298076));
#107897=CARTESIAN_POINT('Ctrl Pts',(-8.55704725225737,3.99818067615685,
11.2459127323938));
#107898=CARTESIAN_POINT('Ctrl Pts',(-8.56191310014219,3.996805822727,11.2729315930196));
#107899=CARTESIAN_POINT('Ctrl Pts',(-8.57308492715497,3.99402019825296,
11.3263119500431));
#107900=CARTESIAN_POINT('Ctrl Pts',(-8.57936908408791,3.99261066355084,
11.3526666056775));
#107901=CARTESIAN_POINT('Ctrl Pts',(-8.58812228222338,3.99080398171295,
11.3853295179107));
#107902=CARTESIAN_POINT('Ctrl Pts',(-8.58990882809027,3.99044217328389,
11.3918168076613));
#107903=CARTESIAN_POINT('Ctrl Pts',(-8.59279987395277,3.98986703356222,
11.4020388310042));
#107904=CARTESIAN_POINT('Ctrl Pts',(-8.59387467687242,3.9896553567237,11.4057819504665));
#107905=CARTESIAN_POINT('Ctrl Pts',(-8.5958184862173,3.98927622996159,11.4124510184772));
#107906=CARTESIAN_POINT('Ctrl Pts',(-8.59668172021969,3.98910911245706,
11.4153785880219));
#107907=CARTESIAN_POINT('Ctrl Pts',(-8.59876944473903,3.98870791238855,
11.4223781019532));
#107908=CARTESIAN_POINT('Ctrl Pts',(-8.60000252178603,3.98847334163494,
11.4264474059822));
#107909=CARTESIAN_POINT('Ctrl Pts',(-8.60378642450302,3.98776077456913,
11.4387414441541));
#107910=CARTESIAN_POINT('Ctrl Pts',(-8.60639207964714,3.9872797837346,11.4469489459745));
#107911=CARTESIAN_POINT('Ctrl Pts',(-8.63462513418686,3.98217099433124,
11.5332319088467));
#107912=CARTESIAN_POINT('Ctrl Pts',(-8.66671036991323,3.97723783834088,
11.6090328708078));
#107913=CARTESIAN_POINT('Ctrl Pts',(-8.75845258664613,3.96538526579975,
11.78330611747));
#107914=CARTESIAN_POINT('Ctrl Pts',(-8.82369721348791,3.9585232195873,11.8782531834745));
#107915=CARTESIAN_POINT('Ctrl Pts',(-8.9111459972959,3.95109034780991,11.9780326845613));
#107916=CARTESIAN_POINT('Ctrl Pts',(-8.92315794942276,3.95010006756871,
11.9912427597698));
#107917=CARTESIAN_POINT('Ctrl Pts',(-8.940897279623,3.94868066041328,12.0100483405166));
#107918=CARTESIAN_POINT('Ctrl Pts',(-8.9464332485259,3.94824354657535,12.0158215031291));
#107919=CARTESIAN_POINT('Ctrl Pts',(-8.95628511663903,3.94747578526157,
12.0259283076081));
#107920=CARTESIAN_POINT('Ctrl Pts',(-8.96058133922653,3.94714430608266,
12.0302807866332));
#107921=CARTESIAN_POINT('Ctrl Pts',(-8.96953945878527,3.94645992398107,
12.0392431400338));
#107922=CARTESIAN_POINT('Ctrl Pts',(-8.97420530939773,3.94610720486851,
12.0438488807047));
#107923=CARTESIAN_POINT('Ctrl Pts',(-8.9863210046459,3.94520078887457,12.0556488032474));
#107924=CARTESIAN_POINT('Ctrl Pts',(-8.99381661482084,3.94464912917223,
12.0627956078895));
#107925=CARTESIAN_POINT('Ctrl Pts',(-9.02653713770173,3.94227909849936,
12.0933370319047));
#107926=CARTESIAN_POINT('Ctrl Pts',(-9.05250769171143,3.94049470240947,
12.1159186232665));
#107927=CARTESIAN_POINT('Ctrl Pts',(-9.12576854130143,3.93568956595658,
12.1752161718429));
#107928=CARTESIAN_POINT('Ctrl Pts',(-9.17455328394296,3.93273692379298,
12.2099802036993));
#107929=CARTESIAN_POINT('Ctrl Pts',(-9.30341362858846,3.92531926392359,
12.2903757537293));
#107930=CARTESIAN_POINT('Ctrl Pts',(-9.38590987885403,3.9209171720759,12.3316128621035));
#107931=CARTESIAN_POINT('Ctrl Pts',(-9.49601912626406,3.91487561606458,
12.374232236855));
#107932=CARTESIAN_POINT('Ctrl Pts',(-9.52056010450624,3.91351825491526,
12.38298524485));
#107933=CARTESIAN_POINT('Ctrl Pts',(-9.55164247914391,3.9117706456984,12.393144653948));
#107934=CARTESIAN_POINT('Ctrl Pts',(-9.55797878562638,3.91141292060233,
12.3951679956314));
#107935=CARTESIAN_POINT('Ctrl Pts',(-9.56803441446307,3.91084258175971,
12.3983036336196));
#107936=CARTESIAN_POINT('Ctrl Pts',(-9.57174482424624,3.91063156799455,
12.3994444692852));
#107937=CARTESIAN_POINT('Ctrl Pts',(-9.57839588900365,3.91025223444002,
12.4014605370903));
#107938=CARTESIAN_POINT('Ctrl Pts',(-9.58133480962992,3.91008423502295,
12.4023412998281));
#107939=CARTESIAN_POINT('Ctrl Pts',(-9.58840476613533,3.90967919080898,
12.4044358840081));
#107940=CARTESIAN_POINT('Ctrl Pts',(-9.59253839710264,3.9094416391885,12.4056407186875));
#107941=CARTESIAN_POINT('Ctrl Pts',(-9.60515815376641,3.90871430699387,
12.4092586718527));
#107942=CARTESIAN_POINT('Ctrl Pts',(-9.61366068163934,3.90822138155659,
12.4116132654143));
#107943=CARTESIAN_POINT('Ctrl Pts',(-9.69076257099488,3.90372869431454,
12.4322162328003));
#107944=CARTESIAN_POINT('Ctrl Pts',(-9.76057753616558,3.89950218620623,
12.4455262284206));
#107945=CARTESIAN_POINT('Ctrl Pts',(-9.95691335943876,3.88763480977903,
12.4683409039926));
#107946=CARTESIAN_POINT('Ctrl Pts',(-10.0841446359608,3.88001851236018,
12.4665648414931));
#107947=CARTESIAN_POINT('Ctrl Pts',(-10.2258664341384,3.87201545602908,
12.4460593981653));
#107948=CARTESIAN_POINT('Ctrl Pts',(-10.2421237150076,3.87110352171542,
12.4434263287684));
#107949=CARTESIAN_POINT('Ctrl Pts',(-10.2660498092042,3.86977004226315,
12.4391355753332));
#107950=CARTESIAN_POINT('Ctrl Pts',(-10.2737549047943,3.86934193695376,
12.4376897998497));
#107951=CARTESIAN_POINT('Ctrl Pts',(-10.2874192760727,3.86858499270221,
12.4350119977767));
#107952=CARTESIAN_POINT('Ctrl Pts',(-10.2933831394414,3.86825539129264,
12.4338045923533));
#107953=CARTESIAN_POINT('Ctrl Pts',(-10.3059135382311,3.86756444081787,
12.4311863135084));
#107954=CARTESIAN_POINT('Ctrl Pts',(-10.3124782529998,3.86720335429075,
12.4297673588015));
#107955=CARTESIAN_POINT('Ctrl Pts',(-10.3298118674834,3.86625220851928,
12.4258956349346));
#107956=CARTESIAN_POINT('Ctrl Pts',(-10.3405632804195,3.86566457962419,
12.4233660423615));
#107957=CARTESIAN_POINT('Ctrl Pts',(-10.3916863954531,3.86288038728586,
12.4107253678329));
#107958=CARTESIAN_POINT('Ctrl Pts',(-10.4316450224197,3.86073480563761,
12.3990165384748));
#107959=CARTESIAN_POINT('Ctrl Pts',(-10.5453478444627,3.85466331358175,
12.3603623278659));
#107960=CARTESIAN_POINT('Ctrl Pts',(-10.6174939661687,3.8508592225807,12.329169638352));
#107961=CARTESIAN_POINT('Ctrl Pts',(-10.7599315977409,3.84300715496183,
12.2534737244739));
#107962=CARTESIAN_POINT('Ctrl Pts',(-10.829631671141,3.83896904898374,12.2084703806387));
#107963=CARTESIAN_POINT('Ctrl Pts',(-10.9046129472499,3.83398200278471,
12.1505002974353));
#107964=CARTESIAN_POINT('Ctrl Pts',(-10.9139919238802,3.83334560005462,
12.143063543176));
#107965=CARTESIAN_POINT('Ctrl Pts',(-10.9267722504251,3.83245928562767,
12.1326719401305));
#107966=CARTESIAN_POINT('Ctrl Pts',(-10.9302529952138,3.83221591042099,
12.1298149812878));
#107967=CARTESIAN_POINT('Ctrl Pts',(-10.9361927939819,3.83179707565793,
12.1248935998925));
#107968=CARTESIAN_POINT('Ctrl Pts',(-10.9386583627342,3.83162217119824,
12.1228370479482));
#107969=CARTESIAN_POINT('Ctrl Pts',(-10.9437637601388,3.83125776928576,
12.1185500251627));
#107970=CARTESIAN_POINT('Ctrl Pts',(-10.9464024512624,3.83106817517489,
12.1163183206741));
#107971=CARTESIAN_POINT('Ctrl Pts',(-10.9527964197624,3.83060573594224,
12.110871581779));
#107972=CARTESIAN_POINT('Ctrl Pts',(-10.9565433359189,3.83033219467308,
12.1076468452401));
#107973=CARTESIAN_POINT('Ctrl Pts',(-10.9698358896328,3.82935289191924,
12.0960890278877));
#107974=CARTESIAN_POINT('Ctrl Pts',(-10.9792892852846,3.82863997268335,
12.0876512691742));
#107975=CARTESIAN_POINT('Ctrl Pts',(-11.0024848172464,3.82685202884115,
12.0664002238586));
#107976=CARTESIAN_POINT('Ctrl Pts',(-11.0160917886559,3.82576853830024,
12.0534432420865));
#107977=CARTESIAN_POINT('Ctrl Pts',(-11.0729656139498,3.82110377664866,
11.9971589985293));
#107978=CARTESIAN_POINT('Ctrl Pts',(-11.1137383944983,3.81741652752482,
11.951402828134));
#107979=CARTESIAN_POINT('Ctrl Pts',(-11.2201695803576,3.80702796518297,
11.8157142820872));
#107980=CARTESIAN_POINT('Ctrl Pts',(-11.2786261614965,3.80038812963448,
11.7206431311604));
#107981=CARTESIAN_POINT('Ctrl Pts',(-11.3334206405127,3.79313696006048,
11.6034481191542));
#107982=CARTESIAN_POINT('Ctrl Pts',(-11.3407862042801,3.79213211684076,
11.586900871452));
#107983=CARTESIAN_POINT('Ctrl Pts',(-11.3509633628391,3.79069792132813,
11.562844899132));
#107984=CARTESIAN_POINT('Ctrl Pts',(-11.3540231980191,3.79026023683922,
11.5554435804096));
#107985=CARTESIAN_POINT('Ctrl Pts',(-11.3592993561836,3.78949379697774,
11.5423785510346));
#107986=CARTESIAN_POINT('Ctrl Pts',(-11.3615413983233,3.78916418528113,
11.5367254927325));
#107987=CARTESIAN_POINT('Ctrl Pts',(-11.3660988510201,3.7884858883677,11.5250220419829));
#107988=CARTESIAN_POINT('Ctrl Pts',(-11.3684094582083,3.78813736897251,
11.5189699142211));
#107989=CARTESIAN_POINT('Ctrl Pts',(-11.3742353039344,3.78724644782813,
11.5034009356227));
#107990=CARTESIAN_POINT('Ctrl Pts',(-11.3776919402571,3.78670599183501,
11.4938624274722));
#107991=CARTESIAN_POINT('Ctrl Pts',(-11.3919194069026,3.78442904277287,
11.4532898603045));
#107992=CARTESIAN_POINT('Ctrl Pts',(-11.4017433432576,3.78272355128406,
11.4219326286449));
#107993=CARTESIAN_POINT('Ctrl Pts',(-11.4254024569034,3.7781939191404,11.3364243790323));
#107994=CARTESIAN_POINT('Ctrl Pts',(-11.4372059870598,3.77542855920324,
11.2817677902986));
#107995=CARTESIAN_POINT('Ctrl Pts',(-11.4563573860184,3.76937853245025,
11.1595518662736));
#107996=CARTESIAN_POINT('Ctrl Pts',(-11.4621865884358,3.76611769224654,
11.0918890488679));
#107997=CARTESIAN_POINT('Ctrl Pts',(-11.4634340406339,3.76236728451616,
11.0160449865655));
#107998=CARTESIAN_POINT('Ctrl Pts',(-11.4634999999891,3.76196931788923,
11.0080221175165));
#107999=CARTESIAN_POINT('Ctrl Pts',(-11.4635,3.76156981780296,11.0000000019885));
#108000=CARTESIAN_POINT('Ctrl Pts',(-11.463499196434,3.68866743805058,10.9984663647852));
#108001=CARTESIAN_POINT('Ctrl Pts',(-11.463621240977,3.6956372676389,11.1149295816248));
#108002=CARTESIAN_POINT('Ctrl Pts',(-11.4498399904823,3.70278005779937,
11.2310163054424));
#108003=CARTESIAN_POINT('Ctrl Pts',(-11.4129076953229,3.71185718108644,
11.3836211223003));
#108004=CARTESIAN_POINT('Ctrl Pts',(-11.4017475418727,3.71415130090118,
11.4225844559022));
#108005=CARTESIAN_POINT('Ctrl Pts',(-11.3856556268055,3.71697531498198,
11.4710651396683));
#108006=CARTESIAN_POINT('Ctrl Pts',(-11.3822186554584,3.71755570624248,
11.4810566277026));
#108007=CARTESIAN_POINT('Ctrl Pts',(-11.3765347233692,3.71848032778269,
11.4970161484804));
#108008=CARTESIAN_POINT('Ctrl Pts',(-11.3743564835665,3.71882691806274,
11.5030081057587));
#108009=CARTESIAN_POINT('Ctrl Pts',(-11.3701427470647,3.71948297752731,
11.5143676246052));
#108010=CARTESIAN_POINT('Ctrl Pts',(-11.3681146947118,3.71979269826478,
11.5197378031813));
#108011=CARTESIAN_POINT('Ctrl Pts',(-11.3634213391418,3.72049597253914,
11.5319477278626));
#108012=CARTESIAN_POINT('Ctrl Pts',(-11.3607360545594,3.72088881792799,
11.5387796635389));
#108013=CARTESIAN_POINT('Ctrl Pts',(-11.3536159952689,3.72190629038651,
11.556501790686));
#108014=CARTESIAN_POINT('Ctrl Pts',(-11.3491011302877,3.72252809222464,
11.5673593721522));
#108015=CARTESIAN_POINT('Ctrl Pts',(-11.3051046072282,3.72837529935472,
11.6696687992457));
#108016=CARTESIAN_POINT('Ctrl Pts',(-11.256513512871,3.73324548612767,11.7569223344702));
#108017=CARTESIAN_POINT('Ctrl Pts',(-11.1685222763326,3.74064261708535,
11.8827781795316));
#108018=CARTESIAN_POINT('Ctrl Pts',(-11.135196436116,3.74321973909345,11.9252407374178));
#108019=CARTESIAN_POINT('Ctrl Pts',(-11.0728646023674,3.74783544669981,
11.9962106531898));
#108020=CARTESIAN_POINT('Ctrl Pts',(-11.0448741788817,3.749847015431,12.0255299351027));
#108021=CARTESIAN_POINT('Ctrl Pts',(-11.0001720952386,3.7530384120377,12.0686222624175));
#108022=CARTESIAN_POINT('Ctrl Pts',(-10.9843102853539,3.75416713610228,
12.0832501643586));
#108023=CARTESIAN_POINT('Ctrl Pts',(-10.963839295049,3.75562816907438,12.1013077803014));
#108024=CARTESIAN_POINT('Ctrl Pts',(-10.9595246345129,3.75593634644207,
12.1050689965284));
#108025=CARTESIAN_POINT('Ctrl Pts',(-10.9528290768421,3.75641514750095,
12.1108369345323));
#108026=CARTESIAN_POINT('Ctrl Pts',(-10.9504636472347,3.75658441330433,
12.1128615365692));
#108027=CARTESIAN_POINT('Ctrl Pts',(-10.9455282033141,3.75693781611274,
12.1170586337432));
#108028=CARTESIAN_POINT('Ctrl Pts',(-10.9429571554539,3.75712204125014,
12.1192298141948));
#108029=CARTESIAN_POINT('Ctrl Pts',(-10.9370783850132,3.7575435147962,12.1241596423967));
#108030=CARTESIAN_POINT('Ctrl Pts',(-10.9337659419453,3.75778116799584,
12.1269125813249));
#108031=CARTESIAN_POINT('Ctrl Pts',(-10.9251148130383,3.75840217944588,
12.1340381184093));
#108032=CARTESIAN_POINT('Ctrl Pts',(-10.9197573273043,3.75878708573071,
12.138387599381));
#108033=CARTESIAN_POINT('Ctrl Pts',(-10.8830815549875,3.76142306602123,
12.1677349648958));
#108034=CARTESIAN_POINT('Ctrl Pts',(-10.8507811116043,3.7637492708968,12.1914734371027));
#108035=CARTESIAN_POINT('Ctrl Pts',(-10.8097879617422,3.76666827161838,
12.2190829739189));
#108036=CARTESIAN_POINT('Ctrl Pts',(-10.8019755757595,3.76722316004374,
12.2242365016237));
#108037=CARTESIAN_POINT('Ctrl Pts',(-10.69121846531,3.77506507994747,12.2957835330226));
#108038=CARTESIAN_POINT('Ctrl Pts',(-10.5803652448107,3.78255814372612,
12.3490815733773));
#108039=CARTESIAN_POINT('Ctrl Pts',(-10.4266191962654,3.79189938242241,
12.4004983582289));
#108040=CARTESIAN_POINT('Ctrl Pts',(-10.3885772971929,3.7941370682623,12.4115267224502));
#108041=CARTESIAN_POINT('Ctrl Pts',(-10.3394813975757,3.79693295931095,
12.4236238825763));
#108042=CARTESIAN_POINT('Ctrl Pts',(-10.3288011646216,3.79753574982269,
12.4261284589795));
#108043=CARTESIAN_POINT('Ctrl Pts',(-10.3114929758665,3.79850408520259,
12.4299825538055));
#108044=CARTESIAN_POINT('Ctrl Pts',(-10.3048821937036,3.79887193584947,
12.4314065908261));
#108045=CARTESIAN_POINT('Ctrl Pts',(-10.2922034062061,3.7995736842926,12.4340459242474));
#108046=CARTESIAN_POINT('Ctrl Pts',(-10.2861371111975,3.79990780552745,
12.4352686503338));
#108047=CARTESIAN_POINT('Ctrl Pts',(-10.2722813720362,3.8006673057545,12.4379700841435));
#108048=CARTESIAN_POINT('Ctrl Pts',(-10.2644872656801,3.80109191475134,
12.439424050798));
#108049=CARTESIAN_POINT('Ctrl Pts',(-10.239905312291,3.80242311536301,12.4438033343177));
#108050=CARTESIAN_POINT('Ctrl Pts',(-10.2230776622916,3.80332268643314,
12.4464988816223));
#108051=CARTESIAN_POINT('Ctrl Pts',(-10.0901368362225,3.81034577827223,
12.4654189154367));
#108052=CARTESIAN_POINT('Ctrl Pts',(-9.97250560790931,3.8160138269401,12.4679316482423));
#108053=CARTESIAN_POINT('Ctrl Pts',(-9.78201139466121,3.82540972126106,
12.4490740294538));
#108054=CARTESIAN_POINT('Ctrl Pts',(-9.70886459319882,3.82908485480946,
12.436165848386));
#108055=CARTESIAN_POINT('Ctrl Pts',(-9.62826925642121,3.83350188429057,
12.415531739621));
#108056=CARTESIAN_POINT('Ctrl Pts',(-9.61953928920874,3.83398532889747,
12.4132103492714));
#108057=CARTESIAN_POINT('Ctrl Pts',(-9.60657894204175,3.83471124576169,
12.4096352656766));
#108058=CARTESIAN_POINT('Ctrl Pts',(-9.60233168046534,3.83495045552813,
12.4084429763839));
#108059=CARTESIAN_POINT('Ctrl Pts',(-9.59475888137071,3.83537942334854,
12.4062801594041));
#108060=CARTESIAN_POINT('Ctrl Pts',(-9.59143124362136,3.83556877251293,
12.4053169827976));
#108061=CARTESIAN_POINT('Ctrl Pts',(-9.58420765318586,3.83598171672622,
12.4031983066168));
#108062=CARTESIAN_POINT('Ctrl Pts',(-9.58031308018908,3.83620555537564,
12.4020383917323));
#108063=CARTESIAN_POINT('Ctrl Pts',(-9.5693876366974,3.83683676838281,12.398734882277));
#108064=CARTESIAN_POINT('Ctrl Pts',(-9.56236810983725,3.83724614241533,
12.3965545469196));
#108065=CARTESIAN_POINT('Ctrl Pts',(-9.52167520326802,3.83964038914278,
12.3835780042865));
#108066=CARTESIAN_POINT('Ctrl Pts',(-9.4883878354657,3.84168281737915,12.3716177748839));
#108067=CARTESIAN_POINT('Ctrl Pts',(-9.37697068751281,3.84873355475861,
12.3269652007139));
#108068=CARTESIAN_POINT('Ctrl Pts',(-9.3012557911328,3.85388244858191,12.2887042258911));
#108069=CARTESIAN_POINT('Ctrl Pts',(-9.16775115568061,3.86325361129794,
12.2059982852506));
#108070=CARTESIAN_POINT('Ctrl Pts',(-9.10913407821677,3.86749056508258,
12.1633701473067));
#108071=CARTESIAN_POINT('Ctrl Pts',(-9.03744416317425,3.87278480940935,
12.1026259900027));
#108072=CARTESIAN_POINT('Ctrl Pts',(-9.02129202632319,3.87398641071349,
12.0883145611338));
#108073=CARTESIAN_POINT('Ctrl Pts',(-8.99905040742021,3.87565425777772,
12.0677118228095));
#108074=CARTESIAN_POINT('Ctrl Pts',(-8.99269240572417,3.87613261406625,
12.0617156109641));
#108075=CARTESIAN_POINT('Ctrl Pts',(-8.98188559552157,3.87694853633377,
12.0513392776563));
#108076=CARTESIAN_POINT('Ctrl Pts',(-8.97741045390739,3.87728726918689,
12.0469870291625));
#108077=CARTESIAN_POINT('Ctrl Pts',(-8.96893285390491,3.87793065615391,
12.0386360271323));
#108078=CARTESIAN_POINT('Ctrl Pts',(-8.96492547785753,3.87823552324564,
12.0346424461863));
#108079=CARTESIAN_POINT('Ctrl Pts',(-8.95462702312118,3.87902097647494,
12.024259725397));
#108080=CARTESIAN_POINT('Ctrl Pts',(-8.94837127075439,3.87950003373344,
12.0178357757858));
#108081=CARTESIAN_POINT('Ctrl Pts',(-8.93066024863424,3.88086225438437,
11.9993109539905));
#108082=CARTESIAN_POINT('Ctrl Pts',(-8.91935187918126,3.88173924583813,
11.9870712004773));
#108083=CARTESIAN_POINT('Ctrl Pts',(-8.83809280218324,3.88810205326599,
11.8960487144789));
#108084=CARTESIAN_POINT('Ctrl Pts',(-8.77662140943615,3.89322482133122,
11.8101104680997));
#108085=CARTESIAN_POINT('Ctrl Pts',(-8.68360118630223,3.9024459828006,11.6449873227817));
#108086=CARTESIAN_POINT('Ctrl Pts',(-8.64870170330079,3.90653652346817,
11.5682467422017));
#108087=CARTESIAN_POINT('Ctrl Pts',(-8.61596075125646,3.91167409351744,
11.4758778841439));
#108088=CARTESIAN_POINT('Ctrl Pts',(-8.61151562744227,3.91240937872692,
11.4627477955098));
#108089=CARTESIAN_POINT('Ctrl Pts',(-8.60567595994616,3.91343178394463,
11.4446563174431));
#108090=CARTESIAN_POINT('Ctrl Pts',(-8.60411998255951,3.91371013400223,
11.439747364546));
#108091=CARTESIAN_POINT('Ctrl Pts',(-8.60154577770961,3.91418093506458,
11.4314746681681));
#108092=CARTESIAN_POINT('Ctrl Pts',(-8.60051368832493,3.91437259543914,
11.4281152461787));
#108093=CARTESIAN_POINT('Ctrl Pts',(-8.59857652184909,3.91473795727468,
11.4217279597367));
#108094=CARTESIAN_POINT('Ctrl Pts',(-8.59766913271872,3.91491152229669,
11.4187008183829));
#108095=CARTESIAN_POINT('Ctrl Pts',(-8.59553592826119,3.91532534752545,
11.4114995111017));
#108096=CARTESIAN_POINT('Ctrl Pts',(-8.594318911974,3.91556610414029,11.4073227887311));
#108097=CARTESIAN_POINT('Ctrl Pts',(-8.59008618251765,3.91642001660049,
11.3925514217248));
#108098=CARTESIAN_POINT('Ctrl Pts',(-8.58717155649628,3.91703856224464,
11.3819284826828));
#108099=CARTESIAN_POINT('Ctrl Pts',(-8.55848488315195,3.92344567725704,
11.2725496680797));
#108100=CARTESIAN_POINT('Ctrl Pts',(-8.5429925246425,3.92966933800374,11.1713942574521));
#108101=CARTESIAN_POINT('Ctrl Pts',(-8.53555432041782,3.93907835791392,
11.0148450370401));
#108102=CARTESIAN_POINT('Ctrl Pts',(-8.53602172434667,3.94233009204437,
10.9601267404747));
#108103=CARTESIAN_POINT('Ctrl Pts',(-8.54255641551234,3.94821150146611,
10.8590726087786));
#108104=CARTESIAN_POINT('Ctrl Pts',(-8.54778053460093,3.95085910693208,
10.8127524802944));
#108105=CARTESIAN_POINT('Ctrl Pts',(-8.5570171799708,3.95406748731553,10.755537359413));
#108106=CARTESIAN_POINT('Ctrl Pts',(-8.55895903372659,3.95469251157409,
10.7443393942694));
#108107=CARTESIAN_POINT('Ctrl Pts',(-8.56226119614032,3.95568201495197,
10.7265317302962));
#108108=CARTESIAN_POINT('Ctrl Pts',(-8.56353709283855,3.95604914069399,
10.7199070134034));
#108109=CARTESIAN_POINT('Ctrl Pts',(-8.56603587246791,3.95674049784029,
10.7073991913873));
#108110=CARTESIAN_POINT('Ctrl Pts',(-8.5672492641077,3.95706502196616,10.701514351197));
#108111=CARTESIAN_POINT('Ctrl Pts',(-8.57007916288314,3.95779735714886,
10.6882045715526));
#108112=CARTESIAN_POINT('Ctrl Pts',(-8.57171733135342,3.9582044711808,10.6807843815936));
#108113=CARTESIAN_POINT('Ctrl Pts',(-8.57609484049765,3.95925065853,10.6616647843114));
#108114=CARTESIAN_POINT('Ctrl Pts',(-8.57892063142789,3.95988697663107,
10.6499856274233));
#108115=CARTESIAN_POINT('Ctrl Pts',(-8.60544254377412,3.96553144806429,
10.5459895131117));
#108116=CARTESIAN_POINT('Ctrl Pts',(-8.63796046277498,3.97023393713507,
10.456155233466));
#108117=CARTESIAN_POINT('Ctrl Pts',(-8.70853018395964,3.97821463661005,
10.3081550364451));
#108118=CARTESIAN_POINT('Ctrl Pts',(-8.74239373723112,3.98151936158128,
10.2483555113975));
#108119=CARTESIAN_POINT('Ctrl Pts',(-8.80393878236052,3.98708753192422,
10.1555504170636));
#108120=CARTESIAN_POINT('Ctrl Pts',(-8.82909687958725,3.98927145510715,
10.1209989820992));
#108121=CARTESIAN_POINT('Ctrl Pts',(-8.86031214068976,3.9919410486122,10.0818508238769));
#108122=CARTESIAN_POINT('Ctrl Pts',(-8.86493985477081,3.99233586806212,
10.0761359469759));
#108123=CARTESIAN_POINT('Ctrl Pts',(-8.87213436590156,3.99294864472083,
10.0673869220076));
#108124=CARTESIAN_POINT('Ctrl Pts',(-8.87467084891018,3.99316449014423,
10.0643278657751));
#108125=CARTESIAN_POINT('Ctrl Pts',(-8.87938298240759,3.99356519843441,
10.0586918016619));
#108126=CARTESIAN_POINT('Ctrl Pts',(-8.88155511353874,3.99374981059857,
10.0561119454562));
#108127=CARTESIAN_POINT('Ctrl Pts',(-8.88650834740058,3.99417053990146,
10.0502700568117));
#108128=CARTESIAN_POINT('Ctrl Pts',(-8.88929488574262,3.99440704605749,
10.0470127106798));
#108129=CARTESIAN_POINT('Ctrl Pts',(-8.89656081382891,3.99502315628839,
10.0385943030978));
#108130=CARTESIAN_POINT('Ctrl Pts',(-8.9010620644707,3.99540426977056,10.033452348914));
#108131=CARTESIAN_POINT('Ctrl Pts',(-8.93137626248471,3.997966037854,9.99930875767027));
#108132=CARTESIAN_POINT('Ctrl Pts',(-8.95829661271478,4.00021727456717,
9.97131481010969));
#108133=CARTESIAN_POINT('Ctrl Pts',(-9.01476431686176,4.00483553466987,
9.91708687833304));
#108134=CARTESIAN_POINT('Ctrl Pts',(-9.04432665826587,4.00720196757216,
9.89091098341901));
#108135=CARTESIAN_POINT('Ctrl Pts',(-9.14238211038541,4.01481228537688,
9.81092229343975));
#108136=CARTESIAN_POINT('Ctrl Pts',(-9.21463854369616,4.02005723328906,
9.76200797819362));
#108137=CARTESIAN_POINT('Ctrl Pts',(-9.31630753092358,4.02678853680713,
9.70568712541951));
#108138=CARTESIAN_POINT('Ctrl Pts',(-9.34221204166076,4.028453545645,9.69233170412443));
#108139=CARTESIAN_POINT('Ctrl Pts',(-9.38713387223544,4.03125533436954,
9.67084460889202));
#108140=CARTESIAN_POINT('Ctrl Pts',(-9.40595567378044,4.03240451475936,
9.66232651833249));
#108141=CARTESIAN_POINT('Ctrl Pts',(-9.4328413834886,4.03401203140198,9.65083842456283));
#108142=CARTESIAN_POINT('Ctrl Pts',(-9.44076017347881,4.03448140244391,
9.64753681243631));
#108143=CARTESIAN_POINT('Ctrl Pts',(-9.45445269465086,4.03528607529179,
9.64196875920419));
#108144=CARTESIAN_POINT('Ctrl Pts',(-9.46021258359201,4.0356224761713,9.63966906229667));
#108145=CARTESIAN_POINT('Ctrl Pts',(-9.47126711829713,4.03626416858958,
9.63533668920751));
#108146=CARTESIAN_POINT('Ctrl Pts',(-9.47655929078084,4.03656965277777,
9.63329804376216));
#108147=CARTESIAN_POINT('Ctrl Pts',(-9.48901175725161,4.03728450134231,
9.62858405639713));
#108148=CARTESIAN_POINT('Ctrl Pts',(-9.49618146244723,4.03769303320538,
9.62593393216179));
#108149=CARTESIAN_POINT('Ctrl Pts',(-9.51744230244507,4.03889570352381,
9.61826411138814));
#108150=CARTESIAN_POINT('Ctrl Pts',(-9.53159022115626,4.03968466774092,
9.61340406110895));
#108151=CARTESIAN_POINT('Ctrl Pts',(-9.66522824689856,4.0470375110941,9.56977603257737));
#108152=CARTESIAN_POINT('Ctrl Pts',(-9.78916358041345,4.05305366763034,
9.54632788019479));
#108153=CARTESIAN_POINT('Ctrl Pts',(-9.98626834889587,4.06271385989675,
9.53480347257085));
#108154=CARTESIAN_POINT('Ctrl Pts',(-10.0581630668327,4.06627188786413,
9.53589475367225));
#108155=CARTESIAN_POINT('Ctrl Pts',(-10.13849097072,4.07055353624185,9.54304056907519));
#108156=CARTESIAN_POINT('Ctrl Pts',(-10.1472963951161,4.07102708668872,
9.54390443420741));
#108157=CARTESIAN_POINT('Ctrl Pts',(-10.1603799693482,4.07173767184036,
9.54530790095667));
#108158=CARTESIAN_POINT('Ctrl Pts',(-10.1646646012093,4.07197148761062,
9.54578667117222));
#108159=CARTESIAN_POINT('Ctrl Pts',(-10.1723173902641,4.07239119254161,
9.54667605814397));
#108160=CARTESIAN_POINT('Ctrl Pts',(-10.1756863076899,4.07257668293792,
9.5470794639753));
#108161=CARTESIAN_POINT('Ctrl Pts',(-10.1830333490986,4.07298282061103,
9.54798515154535));
#108162=CARTESIAN_POINT('Ctrl Pts',(-10.1870107608459,4.07320371222326,
9.54849205942315));
#108163=CARTESIAN_POINT('Ctrl Pts',(-10.1981330115468,4.07382417329191,
9.54995602666162));
#108164=CARTESIAN_POINT('Ctrl Pts',(-10.2052728377477,4.07422567425499,
9.55094952722314));
#108165=CARTESIAN_POINT('Ctrl Pts',(-10.245732920231,4.07651796416436,9.55688453663883));
#108166=CARTESIAN_POINT('Ctrl Pts',(-10.2788798819815,4.07846148918611,
9.56292220646131));
#108167=CARTESIAN_POINT('Ctrl Pts',(-10.3248256160433,4.08122089493624,
9.57294055013334));
#108168=CARTESIAN_POINT('Ctrl Pts',(-10.3378250692537,4.08200905211992,
9.57596188145257));
#108169=CARTESIAN_POINT('Ctrl Pts',(-10.359423469749,4.08332920311354,9.58129415943564));
#108170=CARTESIAN_POINT('Ctrl Pts',(-10.3680460893823,4.08385909095779,
9.58350659526353));
#108171=CARTESIAN_POINT('Ctrl Pts',(-10.4580812322691,4.08941878995923,
9.60748586870029));
#108172=CARTESIAN_POINT('Ctrl Pts',(-10.5374941053354,4.09454000816576,
9.63616891079823));
#108173=CARTESIAN_POINT('Ctrl Pts',(-10.6695066184319,4.10313123968146,
9.69718279713107));
#108174=CARTESIAN_POINT('Ctrl Pts',(-10.7233582545682,4.10666334508523,
9.72629436327319));
#108175=CARTESIAN_POINT('Ctrl Pts',(-10.7888688175068,4.11097741989449,
9.76720780475711));
#108176=CARTESIAN_POINT('Ctrl Pts',(-10.8023611620632,4.11186716641689,
9.77594640547207));
#108177=CARTESIAN_POINT('Ctrl Pts',(-10.8221460892521,4.11317413300904,
9.78922826210136));
#108178=CARTESIAN_POINT('Ctrl Pts',(-10.8285506048574,4.11359756888372,
9.79360193477379));
#108179=CARTESIAN_POINT('Ctrl Pts',(-10.8399010241364,4.1143487416071,9.80148621226924));
#108180=CARTESIAN_POINT('Ctrl Pts',(-10.8448604049933,4.11467720897415,
9.80497701807492));
#108181=CARTESIAN_POINT('Ctrl Pts',(-10.855285330716,4.11536826922182,9.81241224298774));
#108182=CARTESIAN_POINT('Ctrl Pts',(-10.8607456251433,4.11573058121202,
9.81636380234019));
#108183=CARTESIAN_POINT('Ctrl Pts',(-10.8751987505641,4.11669067126526,
9.82697628744257));
#108184=CARTESIAN_POINT('Ctrl Pts',(-10.8841429056887,4.11728592215926,
9.83370294746339));
#108185=CARTESIAN_POINT('Ctrl Pts',(-10.9235781566369,4.11991652789749,
9.86407552476082));
#108186=CARTESIAN_POINT('Ctrl Pts',(-10.9532054970541,4.12190881011942,
9.88882016212099));
#108187=CARTESIAN_POINT('Ctrl Pts',(-11.0869203946385,4.13104799140508,
10.0097869329715));
#108188=CARTESIAN_POINT('Ctrl Pts',(-11.177637315422,4.13761157382644,10.1196129677356));
#108189=CARTESIAN_POINT('Ctrl Pts',(-11.261835914936,4.14586013438316,10.2583621581496));
#108190=CARTESIAN_POINT('Ctrl Pts',(-11.2721489751241,4.14692115500028,
10.2761951376949));
#108191=CARTESIAN_POINT('Ctrl Pts',(-11.2886352955542,4.148714180465,10.3061441044475));
#108192=CARTESIAN_POINT('Ctrl Pts',(-11.2950224275119,4.14943522350565,
10.3181394461627));
#108193=CARTESIAN_POINT('Ctrl Pts',(-11.3035781319548,4.15044067137346,
10.3347614152334));
#108194=CARTESIAN_POINT('Ctrl Pts',(-11.3058910894315,4.15071665862096,
10.3393134012605));
#108195=CARTESIAN_POINT('Ctrl Pts',(-11.3097505403178,4.15118443888823,
10.3470083906919));
#108196=CARTESIAN_POINT('Ctrl Pts',(-11.3113096791728,4.15137546105613,
10.3501450587294));
#108197=CARTESIAN_POINT('Ctrl Pts',(-11.3142636463107,4.15174136690262,
10.3561417522695));
#108198=CARTESIAN_POINT('Ctrl Pts',(-11.3156604320297,4.15191612230184,
10.3590007781777));
#108199=CARTESIAN_POINT('Ctrl Pts',(-11.3189671380646,4.15233395755997,
10.3658254867663));
#108200=CARTESIAN_POINT('Ctrl Pts',(-11.3208685018215,4.15257754800281,
10.3697952519955));
#108201=CARTESIAN_POINT('Ctrl Pts',(-11.3275701156708,4.15344792844247,
10.3839507887112));
#108202=CARTESIAN_POINT('Ctrl Pts',(-11.332270563974,4.1540803382153,10.3941830544954));
#108203=CARTESIAN_POINT('Ctrl Pts',(-11.3771424094568,4.16033032924802,
10.4949115674403));
#108204=CARTESIAN_POINT('Ctrl Pts',(-11.4081476016286,4.16635450413496,
10.5892038508825));
#108205=CARTESIAN_POINT('Ctrl Pts',(-11.4440125546357,4.17638952254871,
10.7524149019133));
#108206=CARTESIAN_POINT('Ctrl Pts',(-11.4539698137171,4.18043414813969,
10.8198779079293));
#108207=CARTESIAN_POINT('Ctrl Pts',(-11.4620531741787,4.18649632257071,
10.9249991086533));
#108208=CARTESIAN_POINT('Ctrl Pts',(-11.463490280705,4.18860247107709,10.9623016056446));
#108209=CARTESIAN_POINT('Ctrl Pts',(-11.4634999508678,4.1906650539568,10.9996207771448));
#108210=CARTESIAN_POINT('Origin',(-10.,3.5,11.));
#108211=CARTESIAN_POINT('',(-11.4635,4.76071734372175,11.0000000323785));
#108212=CARTESIAN_POINT('',(-11.4635,4.68907309470234,10.9999999999272));
#108213=CARTESIAN_POINT('',(-11.4635,3.5,11.));
#108214=CARTESIAN_POINT('Ctrl Pts',(-11.4635,4.76071734372175,11.0000000323785));
#108215=CARTESIAN_POINT('Ctrl Pts',(-11.4635000002391,4.76006698159341,
10.9891917017201));
#108216=CARTESIAN_POINT('Ctrl Pts',(-11.4633802669752,4.75941670604928,
10.9783811577407));
#108217=CARTESIAN_POINT('Ctrl Pts',(-11.4608690620626,4.752607847583,10.8650820461834));
#108218=CARTESIAN_POINT('Ctrl Pts',(-11.4478351442589,4.74656325652258,
10.7631010660844));
#108219=CARTESIAN_POINT('Ctrl Pts',(-11.4211108031141,4.74010366942665,
10.6500546192025));
#108220=CARTESIAN_POINT('Ctrl Pts',(-11.4177930959355,4.73935224505105,
10.6368465353151));
#108221=CARTESIAN_POINT('Ctrl Pts',(-11.412424909794,4.73820923513488,10.6166713970486));
#108222=CARTESIAN_POINT('Ctrl Pts',(-11.4105061850128,4.73781348121368,
10.6096703337811));
#108223=CARTESIAN_POINT('Ctrl Pts',(-11.406915733191,4.7370955043669,10.5969417364871));
#108224=CARTESIAN_POINT('Ctrl Pts',(-11.4052609281689,4.73677274802698,
10.5912096267016));
#108225=CARTESIAN_POINT('Ctrl Pts',(-11.4015712498716,4.73607046762362,
10.5787160860028));
#108226=CARTESIAN_POINT('Ctrl Pts',(-11.3995223967472,4.73569140208005,
10.5719589178161));
#108227=CARTESIAN_POINT('Ctrl Pts',(-11.3937591309399,4.73465421774199,
10.5534353657643));
#108228=CARTESIAN_POINT('Ctrl Pts',(-11.3899446512638,4.73399933662033,
10.5417005713136));
#108229=CARTESIAN_POINT('Ctrl Pts',(-11.3681989230111,4.7304306400058,10.4775725621268));
#108230=CARTESIAN_POINT('Ctrl Pts',(-11.347452685443,4.72761013312772,10.4261787380737));
#108231=CARTESIAN_POINT('Ctrl Pts',(-11.2796825450749,4.71968911358206,
10.2823830850725));
#108232=CARTESIAN_POINT('Ctrl Pts',(-11.2257038705031,4.71477976942153,
10.1936439323859));
#108233=CARTESIAN_POINT('Ctrl Pts',(-11.1336575211577,4.70723622624622,
10.073200018029));
#108234=CARTESIAN_POINT('Ctrl Pts',(-11.1026458974866,4.70479473939584,
10.0365121891736));
#108235=CARTESIAN_POINT('Ctrl Pts',(-11.0647150253019,4.7018322776016,9.99587266438407));
#108236=CARTESIAN_POINT('Ctrl Pts',(-11.0594962623898,4.70142515934709,
9.99036766280083));
#108237=CARTESIAN_POINT('Ctrl Pts',(-11.0514314465998,4.70079628440902,
9.98199189525893));
#108238=CARTESIAN_POINT('Ctrl Pts',(-11.0486158245668,4.70057677771146,
9.97909185531299));
#108239=CARTESIAN_POINT('Ctrl Pts',(-11.0434249600661,4.70017210252978,
9.97378948767722));
#108240=CARTESIAN_POINT('Ctrl Pts',(-11.0410533824669,4.69998721224627,
9.97138368808151));
#108241=CARTESIAN_POINT('Ctrl Pts',(-11.0356859204814,4.69956875410312,
9.96597635021488));
#108242=CARTESIAN_POINT('Ctrl Pts',(-11.0326853259841,4.69933482551563,
9.96297962856517));
#108243=CARTESIAN_POINT('Ctrl Pts',(-11.024919562509,4.69872951547363,9.95529101603052));
#108244=CARTESIAN_POINT('Ctrl Pts',(-11.0201352341605,4.6983567066261,9.95061871972146));
#108245=CARTESIAN_POINT('Ctrl Pts',(-10.9894467185593,4.69596707211208,
9.92105702099918));
#108246=CARTESIAN_POINT('Ctrl Pts',(-10.962667327796,4.69388972184353,9.897097475539));
#108247=CARTESIAN_POINT('Ctrl Pts',(-10.9281680873675,4.6912517443498,9.8684453375328));
#108248=CARTESIAN_POINT('Ctrl Pts',(-10.921248221818,4.69072443692526,9.86280447493264));
#108249=CARTESIAN_POINT('Ctrl Pts',(-10.8383863882249,4.68443548817276,
9.79651071882984));
#108250=CARTESIAN_POINT('Ctrl Pts',(-10.7566352107316,4.67850216854922,
9.74350370590314));
#108251=CARTESIAN_POINT('Ctrl Pts',(-10.6172501684215,4.66925078563945,
9.67169804983092));
#108252=CARTESIAN_POINT('Ctrl Pts',(-10.5626498788265,4.66581263197997,
9.64766487386264));
#108253=CARTESIAN_POINT('Ctrl Pts',(-10.4918509223742,4.66159898933973,
9.6215347379253));
#108254=CARTESIAN_POINT('Ctrl Pts',(-10.4768827225729,4.66072126629397,
9.61628517924777));
#108255=CARTESIAN_POINT('Ctrl Pts',(-10.4545148306403,4.65942861226279,
9.60884653020689));
#108256=CARTESIAN_POINT('Ctrl Pts',(-10.4471787314659,4.65900765322553,
9.60647106485552));
#108257=CARTESIAN_POINT('Ctrl Pts',(-10.4340480977753,4.65825944463588,
9.60233366879131));
#108258=CARTESIAN_POINT('Ctrl Pts',(-10.4282607947573,4.65793148252047,
9.6005495300752));
#108259=CARTESIAN_POINT('Ctrl Pts',(-10.4159929889272,4.65724003472574,
9.59685077673134));
#108260=CARTESIAN_POINT('Ctrl Pts',(-10.4095099511158,4.65687684069734,
9.59494501473441));
#108261=CARTESIAN_POINT('Ctrl Pts',(-10.3921672217811,4.65591102019841,
9.58997715490186));
#108262=CARTESIAN_POINT('Ctrl Pts',(-10.3812848112144,4.65531097944266,
9.5869955924605));
#108263=CARTESIAN_POINT('Ctrl Pts',(-10.3320399407606,4.65262149741239,
9.57411383494212));
#108264=CARTESIAN_POINT('Ctrl Pts',(-10.2933179613259,4.65057764995032,
9.56564760151899));
#108265=CARTESIAN_POINT('Ctrl Pts',(-10.1396706078471,4.64267910493585,
9.53853744075819));
#108266=CARTESIAN_POINT('Ctrl Pts',(-10.0230472469863,4.63717882680453,
9.53205979938233));
#108267=CARTESIAN_POINT('Ctrl Pts',(-9.85404747007822,4.62879073839662,
9.54283364612742));
#108268=CARTESIAN_POINT('Ctrl Pts',(-9.80143167727726,4.62611251383239,
9.54906738447881));
#108269=CARTESIAN_POINT('Ctrl Pts',(-9.74165540250956,4.62288071416184,
9.55946186045097));
#108270=CARTESIAN_POINT('Ctrl Pts',(-9.73404667231101,4.62246578347306,
9.56084716417637));
#108271=CARTESIAN_POINT('Ctrl Pts',(-9.72244795156883,4.6218273316654,9.5630540364959));
#108272=CARTESIAN_POINT('Ctrl Pts',(-9.71844970297724,4.62160616826766,
9.56383208814206));
#108273=CARTESIAN_POINT('Ctrl Pts',(-9.71114276646304,4.6211999236078,9.56528568964215));
#108274=CARTESIAN_POINT('Ctrl Pts',(-9.70783312258723,4.62101513547982,
9.56595600873118));
#108275=CARTESIAN_POINT('Ctrl Pts',(-9.70040759446,4.62059878870618,9.56748671178977));
#108276=CARTESIAN_POINT('Ctrl Pts',(-9.69629311219602,4.62036688624542,
9.56835337608942));
#108277=CARTESIAN_POINT('Ctrl Pts',(-9.68425279616956,4.6196848482562,9.57094375773924));
#108278=CARTESIAN_POINT('Ctrl Pts',(-9.6763376186338,4.6192321402102,9.57271562150901));
#108279=CARTESIAN_POINT('Ctrl Pts',(-9.60885389582452,4.61533765066677,
9.58841249154717));
#108280=CARTESIAN_POINT('Ctrl Pts',(-9.55020314037553,4.61172316716515,
9.60599286747066));
#108281=CARTESIAN_POINT('Ctrl Pts',(-9.43666180945782,4.60447625328042,
9.64793939549272));
#108282=CARTESIAN_POINT('Ctrl Pts',(-9.38181816847751,4.60085288924654,
9.67211852207918));
#108283=CARTESIAN_POINT('Ctrl Pts',(-9.26481640147025,4.59299486197849,
9.73252544513172));
#108284=CARTESIAN_POINT('Ctrl Pts',(-9.20352680122065,4.58879503422589,
9.77011411323021));
#108285=CARTESIAN_POINT('Ctrl Pts',(-9.12825352236983,4.58357504836204,
9.8242754797133));
#108286=CARTESIAN_POINT('Ctrl Pts',(-9.11153256352299,4.58241063860529,
9.83685953277936));
#108287=CARTESIAN_POINT('Ctrl Pts',(-9.08832142522019,4.58078663799147,
9.85512073914929));
#108288=CARTESIAN_POINT('Ctrl Pts',(-9.08160326408213,4.58031565453016,
9.86050283654933));
#108289=CARTESIAN_POINT('Ctrl Pts',(-9.0701335027491,4.57950982044025,9.86985889911455));
#108290=CARTESIAN_POINT('Ctrl Pts',(-9.06535897941183,4.57917384902404,
9.87380429103717));
#108291=CARTESIAN_POINT('Ctrl Pts',(-9.05628205722691,4.57853405959313,
9.88140242061531));
#108292=CARTESIAN_POINT('Ctrl Pts',(-9.05197546924879,4.57823004168493,
9.88504996056674));
#108293=CARTESIAN_POINT('Ctrl Pts',(-9.04084887665433,4.57744328819505,
9.89458489986472));
#108294=CARTESIAN_POINT('Ctrl Pts',(-9.03406188954293,4.57696211743715,
9.90051057637646));
#108295=CARTESIAN_POINT('Ctrl Pts',(-9.01097518708037,4.57532054962892,
9.92104621064389));
#108296=CARTESIAN_POINT('Ctrl Pts',(-8.99494833670773,4.57417267339318,
9.93595931486271));
#108297=CARTESIAN_POINT('Ctrl Pts',(-8.87064410368156,4.56518419476819,
10.0569407878142));
#108298=CARTESIAN_POINT('Ctrl Pts',(-8.77912095313951,4.55815464699216,
10.1788699898861));
#108299=CARTESIAN_POINT('Ctrl Pts',(-8.68864390469351,4.54849552282197,
10.3489498082288));
#108300=CARTESIAN_POINT('Ctrl Pts',(-8.67088137798294,4.54638986834393,
10.386025823709));
#108301=CARTESIAN_POINT('Ctrl Pts',(-8.6518199071518,4.54380766849645,10.4305297735395));
#108302=CARTESIAN_POINT('Ctrl Pts',(-8.64898669464144,4.54341430415586,
10.4372843116696));
#108303=CARTESIAN_POINT('Ctrl Pts',(-8.64468998516335,4.54280231069275,
10.4477474251766));
#108304=CARTESIAN_POINT('Ctrl Pts',(-8.64319069908793,4.54258574736916,
10.4514412858155));
#108305=CARTESIAN_POINT('Ctrl Pts',(-8.64044728142347,4.5421837665463,10.4582804267795));
#108306=CARTESIAN_POINT('Ctrl Pts',(-8.63919894571175,4.54199860030833,
10.4614239324142));
#108307=CARTESIAN_POINT('Ctrl Pts',(-8.63638449297455,4.5415759715976,10.468583421798));
#108308=CARTESIAN_POINT('Ctrl Pts',(-8.63482522089789,4.54133811583802,
10.4726019983709));
#108309=CARTESIAN_POINT('Ctrl Pts',(-8.63080962526865,4.54071590388535,
10.4830881784182));
#108310=CARTESIAN_POINT('Ctrl Pts',(-8.6283813980002,4.54032998820244,10.4895663408298));
#108311=CARTESIAN_POINT('Ctrl Pts',(-8.61200965341005,4.53766157520196,
10.5342042929301));
#108312=CARTESIAN_POINT('Ctrl Pts',(-8.59961554425191,4.5353018501579,10.5729102311699));
#108313=CARTESIAN_POINT('Ctrl Pts',(-8.56636470243833,4.52788959179638,
10.6938674780609));
#108314=CARTESIAN_POINT('Ctrl Pts',(-8.5510342191019,4.52272421054177,10.7774562479718));
#108315=CARTESIAN_POINT('Ctrl Pts',(-8.53613052030939,4.51331459876314,
10.9346951991438));
#108316=CARTESIAN_POINT('Ctrl Pts',(-8.53469512208989,4.50905315354574,
11.007909207974));
#108317=CARTESIAN_POINT('Ctrl Pts',(-8.53971172793616,4.50397343010813,
11.0984860436277));
#108318=CARTESIAN_POINT('Ctrl Pts',(-8.54100021829184,4.50299854921395,
11.1160216054971));
#108319=CARTESIAN_POINT('Ctrl Pts',(-8.54333744580792,4.50159234978565,
11.1415309200178));
#108320=CARTESIAN_POINT('Ctrl Pts',(-8.54413636693365,4.50115336236033,
11.1495255282902));
#108321=CARTESIAN_POINT('Ctrl Pts',(-8.54565738394172,4.50038478772996,
11.1635756343457));
#108322=CARTESIAN_POINT('Ctrl Pts',(-8.54635156481252,4.50005434347198,
11.1696339042389));
#108323=CARTESIAN_POINT('Ctrl Pts',(-8.547875307817,4.49936895495072,11.1822350761924));
#108324=CARTESIAN_POINT('Ctrl Pts',(-8.54871127520404,4.49901421769615,
11.1887770745228));
#108325=CARTESIAN_POINT('Ctrl Pts',(-8.55099855944523,4.49809590150956,
11.2057625900771));
#108326=CARTESIAN_POINT('Ctrl Pts',(-8.55251857745293,4.49753446808652,
11.2161965710375));
#108327=CARTESIAN_POINT('Ctrl Pts',(-8.55923042448646,4.49524038417566,
11.2590197917275));
#108328=CARTESIAN_POINT('Ctrl Pts',(-8.5653978762397,4.49353813545569,11.2912476205234));
#108329=CARTESIAN_POINT('Ctrl Pts',(-8.57825573472954,4.49056676660924,
11.3480246231672));
#108330=CARTESIAN_POINT('Ctrl Pts',(-8.58451252818077,4.48928696024296,
11.3726569293875));
#108331=CARTESIAN_POINT('Ctrl Pts',(-8.61968510283551,4.48282390277454,
11.4974164339687));
#108332=CARTESIAN_POINT('Ctrl Pts',(-8.65859282370361,4.47788582042177,
11.594405370506));
#108333=CARTESIAN_POINT('Ctrl Pts',(-8.73006742722019,4.47030391446386,
11.7289889325994));
#108334=CARTESIAN_POINT('Ctrl Pts',(-8.7547514087074,4.46785440218498,11.7703951560246));
#108335=CARTESIAN_POINT('Ctrl Pts',(-8.78563341847975,4.46488283143444,
11.8168253661177));
#108336=CARTESIAN_POINT('Ctrl Pts',(-8.78988642461653,4.46447542905982,
11.8231129951655));
#108337=CARTESIAN_POINT('Ctrl Pts',(-8.79647932256232,4.46384620767094,
11.8326983704181));
#108338=CARTESIAN_POINT('Ctrl Pts',(-8.79878435103489,4.46362664257924,
11.8360200721278));
#108339=CARTESIAN_POINT('Ctrl Pts',(-8.8030405039941,4.46322191608363,11.8420995350851));
#108340=CARTESIAN_POINT('Ctrl Pts',(-8.80498743780961,4.46303703343914,
11.8448601290615));
#108341=CARTESIAN_POINT('Ctrl Pts',(-8.80939919697607,4.46261866491626,
11.8510698852408));
#108342=CARTESIAN_POINT('Ctrl Pts',(-8.81186944573324,4.46238481897063,
11.854515071148));
#108343=CARTESIAN_POINT('Ctrl Pts',(-8.8182721689715,4.46177985643482,11.8633633308517));
#108344=CARTESIAN_POINT('Ctrl Pts',(-8.82222670286482,4.46140731505097,
11.8687502315531));
#108345=CARTESIAN_POINT('Ctrl Pts',(-8.84761937332365,4.45902312630088,
11.9028483084829));
#108346=CARTESIAN_POINT('Ctrl Pts',(-8.87006748617596,4.45695125976555,
11.9307890713788));
#108347=CARTESIAN_POINT('Ctrl Pts',(-8.90011803659311,4.45425074797896,
11.9655017641984));
#108348=CARTESIAN_POINT('Ctrl Pts',(-8.90679840846839,4.4536547185935,11.9730592296928));
#108349=CARTESIAN_POINT('Ctrl Pts',(-8.91986679995594,4.45249787000394,
11.9875389773571));
#108350=CARTESIAN_POINT('Ctrl Pts',(-8.92624461799343,4.45193735657752,
11.9944698776333));
#108351=CARTESIAN_POINT('Ctrl Pts',(-8.98375394072611,4.44692228004805,
12.0557681631929));
#108352=CARTESIAN_POINT('Ctrl Pts',(-9.03890816475989,4.44239233869295,
12.1062122084702));
#108353=CARTESIAN_POINT('Ctrl Pts',(-9.13786892075807,4.43492025791827,
12.1837098897234));
#108354=CARTESIAN_POINT('Ctrl Pts',(-9.17968930443782,4.43193188163528,
12.2130664512608));
#108355=CARTESIAN_POINT('Ctrl Pts',(-9.24872740868775,4.42728275583539,
12.2563224986996));
#108356=CARTESIAN_POINT('Ctrl Pts',(-9.27499100648203,4.42557472228268,
12.2716598909955));
#108357=CARTESIAN_POINT('Ctrl Pts',(-9.31072379647752,4.42332952796018,
12.2910598941398));
#108358=CARTESIAN_POINT('Ctrl Pts',(-9.31978407134148,4.42276679088924,
12.2958563318792));
#108359=CARTESIAN_POINT('Ctrl Pts',(-9.3346982753956,4.421850959482,12.3035522709367));
#108360=CARTESIAN_POINT('Ctrl Pts',(-9.34052243956966,4.42149590429826,
12.306508422106));
#108361=CARTESIAN_POINT('Ctrl Pts',(-9.35184348905517,4.42081067609336,
12.3121596178073));
#108362=CARTESIAN_POINT('Ctrl Pts',(-9.35733787023911,4.42048034632237,
12.3148593513447));
#108363=CARTESIAN_POINT('Ctrl Pts',(-9.37022258487034,4.4197108169443,12.3210903605723));
#108364=CARTESIAN_POINT('Ctrl Pts',(-9.37762598433645,4.41927256146422,
12.3245942479525));
#108365=CARTESIAN_POINT('Ctrl Pts',(-9.40180256049737,4.4178537538849,12.3357891112053));
#108366=CARTESIAN_POINT('Ctrl Pts',(-9.41869219883564,4.4168818188004,12.3432252255225));
#108367=CARTESIAN_POINT('Ctrl Pts',(-9.45893437620366,4.41460800038661,
12.3600416678689));
#108368=CARTESIAN_POINT('Ctrl Pts',(-9.4823973497858,4.4133150597027,12.3691431381006));
#108369=CARTESIAN_POINT('Ctrl Pts',(-9.57210490072127,4.40847764844481,
12.4013054761191));
#108370=CARTESIAN_POINT('Ctrl Pts',(-9.63974446153239,4.40505063387864,
12.4201999940375));
#108371=CARTESIAN_POINT('Ctrl Pts',(-9.80253993073046,4.39696478013528,
12.4532909300598));
#108372=CARTESIAN_POINT('Ctrl Pts',(-9.89824112606891,4.39233986708645,
12.4631082288743));
#108373=CARTESIAN_POINT('Ctrl Pts',(-10.0055896289308,4.3866834839278,12.4635336432352));
#108374=CARTESIAN_POINT('Ctrl Pts',(-10.0169787531758,4.38607733689636,
12.4634458223974));
#108375=CARTESIAN_POINT('Ctrl Pts',(-10.0327886102945,4.38522613525996,
12.4631393404871));
#108376=CARTESIAN_POINT('Ctrl Pts',(-10.0372114085697,4.3849869492825,12.4630335377909));
#108377=CARTESIAN_POINT('Ctrl Pts',(-10.0448213691902,4.38457346982709,
12.4628169622198));
#108378=CARTESIAN_POINT('Ctrl Pts',(-10.0480088006151,4.38439970082249,
12.4627158215997));
#108379=CARTESIAN_POINT('Ctrl Pts',(-10.0546920904973,4.38403407879386,
12.4624818849986));
#108380=CARTESIAN_POINT('Ctrl Pts',(-10.0581878259649,4.38384210577452,
12.4623469714208));
#108381=CARTESIAN_POINT('Ctrl Pts',(-10.0667602993354,4.38336959491487,
12.4619853410258));
#108382=CARTESIAN_POINT('Ctrl Pts',(-10.0718363817969,4.38308830523951,
12.4617447135627));
#108383=CARTESIAN_POINT('Ctrl Pts',(-10.0903169807852,4.3820590050995,12.4607721623199));
#108384=CARTESIAN_POINT('Ctrl Pts',(-10.1037121135729,4.38130297595579,
12.4598822687781));
#108385=CARTESIAN_POINT('Ctrl Pts',(-10.1372907698024,4.37938590431397,
12.4571870465033));
#108386=CARTESIAN_POINT('Ctrl Pts',(-10.1574522302599,4.37821498034552,
12.4551465795295));
#108387=CARTESIAN_POINT('Ctrl Pts',(-10.2470186685465,4.37294292897814,
12.4441987617279));
#108388=CARTESIAN_POINT('Ctrl Pts',(-10.315772420299,4.36871200208075,12.4307394415528));
#108389=CARTESIAN_POINT('Ctrl Pts',(-10.4782865807458,4.35858787967845,
12.3866368580609));
#108390=CARTESIAN_POINT('Ctrl Pts',(-10.5704465860408,4.35275828229026,
12.3513385778554));
#108391=CARTESIAN_POINT('Ctrl Pts',(-10.6749533804014,4.34619544065918,
12.2986973359208));
#108392=CARTESIAN_POINT('Ctrl Pts',(-10.6913720895069,4.34516497975277,
12.2900315942557));
#108393=CARTESIAN_POINT('Ctrl Pts',(-10.7140910824816,4.3437394343945,12.2774822085547));
#108394=CARTESIAN_POINT('Ctrl Pts',(-10.7205330482661,4.34333525461376,
12.2738598809937));
#108395=CARTESIAN_POINT('Ctrl Pts',(-10.7322933918196,4.34259737620842,
12.267129266984));
#108396=CARTESIAN_POINT('Ctrl Pts',(-10.7376200867129,4.34226315801337,
12.2640359173036));
#108397=CARTESIAN_POINT('Ctrl Pts',(-10.7483921359397,4.34158720515927,
12.2576890295778));
#108398=CARTESIAN_POINT('Ctrl Pts',(-10.7538361872963,4.34124555015794,
12.2544335329991));
#108399=CARTESIAN_POINT('Ctrl Pts',(-10.767266193376,4.34040253110171,12.2462835015279));
#108400=CARTESIAN_POINT('Ctrl Pts',(-10.7752267137763,4.33990267595804,
12.2413474636006));
#108401=CARTESIAN_POINT('Ctrl Pts',(-10.8051513274522,4.33802249945004,
12.2223921321279));
#108402=CARTESIAN_POINT('Ctrl Pts',(-10.8267877255677,4.33666080295548,
12.207863133798));
#108403=CARTESIAN_POINT('Ctrl Pts',(-10.8805507232855,4.33326098006719,
12.1696389640808));
#108404=CARTESIAN_POINT('Ctrl Pts',(-10.9121177413857,4.33124982275521,
12.145192735519));
#108405=CARTESIAN_POINT('Ctrl Pts',(-10.9921859330042,4.32605204862986,
12.0777724094825));
#108406=CARTESIAN_POINT('Ctrl Pts',(-11.0389018818581,4.32292138961851,
12.032816249364));
#108407=CARTESIAN_POINT('Ctrl Pts',(-11.1331478777198,4.3160944600365,11.9292335494198));
#108408=CARTESIAN_POINT('Ctrl Pts',(-11.1794325066448,4.31239862987386,
11.8697331038137));
#108409=CARTESIAN_POINT('Ctrl Pts',(-11.2275618969624,4.30780627260153,
11.7969119597719));
#108410=CARTESIAN_POINT('Ctrl Pts',(-11.234068844469,4.30716691251265,11.7867979100659));
#108411=CARTESIAN_POINT('Ctrl Pts',(-11.2431077156103,4.30625040892505,
11.772360367902));
#108412=CARTESIAN_POINT('Ctrl Pts',(-11.2457433860401,4.30597962197698,
11.7681020408617));
#108413=CARTESIAN_POINT('Ctrl Pts',(-11.2501573060547,4.30551996480853,
11.7608882026661));
#108414=CARTESIAN_POINT('Ctrl Pts',(-11.2519470852066,4.30533183135619,
11.7579397353729));
#108415=CARTESIAN_POINT('Ctrl Pts',(-11.255602759857,4.30494389355082,11.7518691299748));
#108416=CARTESIAN_POINT('Ctrl Pts',(-11.2574674582387,4.30474401929378,
11.7487463322423));
#108417=CARTESIAN_POINT('Ctrl Pts',(-11.2622426092817,4.30422707498271,
11.7406812689536));
#108418=CARTESIAN_POINT('Ctrl Pts',(-11.2651356557008,4.30390892658485,
11.7357288340929));
#108419=CARTESIAN_POINT('Ctrl Pts',(-11.277239274818,4.30255716276801,11.7147268760488));
#108420=CARTESIAN_POINT('Ctrl Pts',(-11.28617374447,4.30150777462773,11.6985210852964));
#108421=CARTESIAN_POINT('Ctrl Pts',(-11.309560960176,4.29862514904188,11.6541295645834));
#108422=CARTESIAN_POINT('Ctrl Pts',(-11.3234094925998,4.29676644455017,
11.6256376684137));
#108423=CARTESIAN_POINT('Ctrl Pts',(-11.3763842363113,4.28905422820884,
11.5070037375033));
#108424=CARTESIAN_POINT('Ctrl Pts',(-11.4073107495677,4.28305745858354,
11.4134788135742));
#108425=CARTESIAN_POINT('Ctrl Pts',(-11.4350097033341,4.27554249598131,
11.2888652974904));
#108426=CARTESIAN_POINT('Ctrl Pts',(-11.4405213853676,4.27383108191672,
11.259989026018));
#108427=CARTESIAN_POINT('Ctrl Pts',(-11.4507711367393,4.2701016011383,11.1958558255877));
#108428=CARTESIAN_POINT('Ctrl Pts',(-11.4551013009719,4.26809586376428,
11.1605518728364));
#108429=CARTESIAN_POINT('Ctrl Pts',(-11.459069417551,4.2655294348156,11.1143087612984));
#108430=CARTESIAN_POINT('Ctrl Pts',(-11.4598770673208,4.26493298247324,
11.1034843723839));
#108431=CARTESIAN_POINT('Ctrl Pts',(-11.4609860347905,4.26397641895943,
11.0860025924325));
#108432=CARTESIAN_POINT('Ctrl Pts',(-11.4613624250568,4.26361400115722,
11.0793505162485));
#108433=CARTESIAN_POINT('Ctrl Pts',(-11.4619952223012,4.26292372639437,
11.0666269105991));
#108434=CARTESIAN_POINT('Ctrl Pts',(-11.4622592649713,4.26259564050504,
11.0605559145251));
#108435=CARTESIAN_POINT('Ctrl Pts',(-11.4627790706779,4.2618444537934,11.0466028848607));
#108436=CARTESIAN_POINT('Ctrl Pts',(-11.4630089543204,4.26142215982443,
11.0387200381982));
#108437=CARTESIAN_POINT('Ctrl Pts',(-11.4633916991168,4.26045385918552,
11.0205584834817));
#108438=CARTESIAN_POINT('Ctrl Pts',(-11.4634999999986,4.25990923949891,
11.0102793802479));
#108439=CARTESIAN_POINT('Ctrl Pts',(-11.4635,4.25936781471288,11.0000000001943));
#108440=CARTESIAN_POINT('Ctrl Pts',(-11.4634999508678,4.1906650539568,10.9996207771448));
#108441=CARTESIAN_POINT('Ctrl Pts',(-11.4635027073645,4.19125299678564,
11.0102586717368));
#108442=CARTESIAN_POINT('Ctrl Pts',(-11.4633894767784,4.19183736043388,
11.0208964674618));
#108443=CARTESIAN_POINT('Ctrl Pts',(-11.4630177869332,4.19277917313937,
11.038143611353));
#108444=CARTESIAN_POINT('Ctrl Pts',(-11.4628304973372,4.19313880559912,
11.0447539721701));
#108445=CARTESIAN_POINT('Ctrl Pts',(-11.4623847929826,4.19382678807775,
11.0574457460763));
#108446=CARTESIAN_POINT('Ctrl Pts',(-11.462133231498,4.19415534252685,11.0635272490928));
#108447=CARTESIAN_POINT('Ctrl Pts',(-11.4614642418366,4.1949118984824,11.0775769476081));
#108448=CARTESIAN_POINT('Ctrl Pts',(-11.4610195731432,4.19533904961798,
11.0855436921553));
#108449=CARTESIAN_POINT('Ctrl Pts',(-11.4594046954425,4.19668585455684,
11.1107670124031));
#108450=CARTESIAN_POINT('Ctrl Pts',(-11.4579937014578,4.19759807587921,
11.1280070143655));
#108451=CARTESIAN_POINT('Ctrl Pts',(-11.4492537410059,4.20219873302817,
11.2156529495561));
#108452=CARTESIAN_POINT('Ctrl Pts',(-11.4371292417829,4.20573662907436,
11.2854883125994));
#108453=CARTESIAN_POINT('Ctrl Pts',(-11.4075844070937,4.21172667476086,
11.4039416860583));
#108454=CARTESIAN_POINT('Ctrl Pts',(-11.3925649089516,4.21420695202438,
11.453018478542));
#108455=CARTESIAN_POINT('Ctrl Pts',(-11.3632979534051,4.21837900901593,
11.5333090216644));
#108456=CARTESIAN_POINT('Ctrl Pts',(-11.3504754216913,4.22005673416179,
11.564991872712));
#108457=CARTESIAN_POINT('Ctrl Pts',(-11.330810666419,4.22247075492003,11.6090764668431));
#108458=CARTESIAN_POINT('Ctrl Pts',(-11.3248792541956,4.22318125671054,
11.6218730715134));
#108459=CARTESIAN_POINT('Ctrl Pts',(-11.3058385451146,4.22541460586849,
11.6614427630739));
#108460=CARTESIAN_POINT('Ctrl Pts',(-11.2920963094104,4.22696038963874,
11.6879009581243));
#108461=CARTESIAN_POINT('Ctrl Pts',(-11.274168729513,4.22892237210212,11.719982317872));
#108462=CARTESIAN_POINT('Ctrl Pts',(-11.2707375725481,4.22929560577588,
11.7260210101884));
#108463=CARTESIAN_POINT('Ctrl Pts',(-11.2652907127421,4.22988494870316,
11.7354503516548));
#108464=CARTESIAN_POINT('Ctrl Pts',(-11.2633040191641,4.23009926539293,
11.738857741328));
#108465=CARTESIAN_POINT('Ctrl Pts',(-11.2595859380812,4.23049925262188,
11.7451758076356));
#108466=CARTESIAN_POINT('Ctrl Pts',(-11.2578582013422,4.23068469251387,
11.7480885403933));
#108467=CARTESIAN_POINT('Ctrl Pts',(-11.2538796788197,4.23111072076019,
11.7547430475418));
#108468=CARTESIAN_POINT('Ctrl Pts',(-11.2516222499169,4.23135172895555,
11.7584807573541));
#108469=CARTESIAN_POINT('Ctrl Pts',(-11.2445633976118,4.23210298617417,
11.7700510388611));
#108470=CARTESIAN_POINT('Ctrl Pts',(-11.2397050161034,4.23261670820045,
11.7778483897551));
#108471=CARTESIAN_POINT('Ctrl Pts',(-11.2281639899435,4.23382838740645,
11.7959881152876));
#108472=CARTESIAN_POINT('Ctrl Pts',(-11.2214236564232,4.23452949560012,
11.8062928121524));
#108473=CARTESIAN_POINT('Ctrl Pts',(-11.19712487554,4.23703087890603,11.8424370801194));
#108474=CARTESIAN_POINT('Ctrl Pts',(-11.1788706641113,4.2388632731865,11.8677971810766));
#108475=CARTESIAN_POINT('Ctrl Pts',(-11.1018566529653,4.24635550263498,
11.9678724344192));
#108476=CARTESIAN_POINT('Ctrl Pts',(-11.0366934559322,4.25215340792624,
12.0373684494402));
#108477=CARTESIAN_POINT('Ctrl Pts',(-10.9163831261478,4.26160123827869,
12.1429350258821));
#108478=CARTESIAN_POINT('Ctrl Pts',(-10.8647109117015,4.26534512552799,
12.1825122853686));
#108479=CARTESIAN_POINT('Ctrl Pts',(-10.8008733870488,4.26960309813988,
12.2249774492004));
#108480=CARTESIAN_POINT('Ctrl Pts',(-10.7910980123733,4.27024573145171,
12.2313130710421));
#108481=CARTESIAN_POINT('Ctrl Pts',(-10.7748918506384,4.27129600320372,
12.2415439454792));
#108482=CARTESIAN_POINT('Ctrl Pts',(-10.7685049666905,4.27170612109958,
12.2455074740235));
#108483=CARTESIAN_POINT('Ctrl Pts',(-10.7569303214436,4.27244262711917,
12.2525674566509));
#108484=CARTESIAN_POINT('Ctrl Pts',(-10.751753416213,4.27276963983353,12.2556813081762));
#108485=CARTESIAN_POINT('Ctrl Pts',(-10.7406324770407,4.27346707039785,
12.2622770043287));
#108486=CARTESIAN_POINT('Ctrl Pts',(-10.7346828267279,4.27383713431826,
12.2657491252309));
#108487=CARTESIAN_POINT('Ctrl Pts',(-10.7184151731367,4.27484081446469,
12.2750893216377));
#108488=CARTESIAN_POINT('Ctrl Pts',(-10.7080498214554,4.27547147499225,
12.2808741548062));
#108489=CARTESIAN_POINT('Ctrl Pts',(-10.6506813350237,4.27891528209451,
12.3119818981885));
#108490=CARTESIAN_POINT('Ctrl Pts',(-10.6023877125966,4.28164167132618,
12.3348455088745));
#108491=CARTESIAN_POINT('Ctrl Pts',(-10.4875609921858,4.28783735645884,
12.3817033197719));
#108492=CARTESIAN_POINT('Ctrl Pts',(-10.420325975879,4.29125219786606,12.403618980909));
#108493=CARTESIAN_POINT('Ctrl Pts',(-10.2771246201473,4.29844200637088,
12.4390788668867));
#108494=CARTESIAN_POINT('Ctrl Pts',(-10.2011447474074,4.30221214224991,
12.4516488240615));
#108495=CARTESIAN_POINT('Ctrl Pts',(-10.112576159206,4.30688909545454,12.459213147033));
#108496=CARTESIAN_POINT('Ctrl Pts',(-10.100601713755,4.30752741606844,12.4600875580106));
#108497=CARTESIAN_POINT('Ctrl Pts',(-10.0841151733023,4.30841612886615,
12.4610876907105));
#108498=CARTESIAN_POINT('Ctrl Pts',(-10.0796109167686,4.30865994437959,
12.461340036809));
#108499=CARTESIAN_POINT('Ctrl Pts',(-10.0718959075772,4.30907939793572,
12.4617364871842));
#108500=CARTESIAN_POINT('Ctrl Pts',(-10.0686856869701,4.30925447807271,
12.4618908493761));
#108501=CARTESIAN_POINT('Ctrl Pts',(-10.0619979617401,4.30962039834609,
12.4621903490625));
#108502=CARTESIAN_POINT('Ctrl Pts',(-10.0585204327042,4.30981134273063,
12.4623336562643));
#108503=CARTESIAN_POINT('Ctrl Pts',(-10.0500617043155,4.31027737588285,
12.4626520157003));
#108504=CARTESIAN_POINT('Ctrl Pts',(-10.0450800768072,4.31055316982355,
12.4628140273009));
#108505=CARTESIAN_POINT('Ctrl Pts',(-10.0273307201407,4.31154032086842,
12.4633005167618));
#108506=CARTESIAN_POINT('Ctrl Pts',(-10.0145600471893,4.31225888096742,
12.4634832944315));
#108507=CARTESIAN_POINT('Ctrl Pts',(-9.98283890601908,4.31406163315034,
12.4635220723229));
#108508=CARTESIAN_POINT('Ctrl Pts',(-9.96389084247117,4.31515434596721,
12.4631771691707));
#108509=CARTESIAN_POINT('Ctrl Pts',(-9.88297682892465,4.31987390022469,
12.4601317210455));
#108510=CARTESIAN_POINT('Ctrl Pts',(-9.82121186205631,4.32360756779023,
12.4538614626365));
#108511=CARTESIAN_POINT('Ctrl Pts',(-9.65239117560432,4.33390627374144,
12.4258006583493));
#108512=CARTESIAN_POINT('Ctrl Pts',(-9.54706966550362,4.34040884773393,
12.395922924126));
#108513=CARTESIAN_POINT('Ctrl Pts',(-9.42919808313093,4.34754690018117,
12.3477197155518));
#108514=CARTESIAN_POINT('Ctrl Pts',(-9.4124875137565,4.34855645308008,12.3405194441713));
#108515=CARTESIAN_POINT('Ctrl Pts',(-9.38857552538606,4.34999809638388,
12.3296831549033));
#108516=CARTESIAN_POINT('Ctrl Pts',(-9.38126354408988,4.35043852947603,
12.3262964911135));
#108517=CARTESIAN_POINT('Ctrl Pts',(-9.36844373688849,4.3512101073188,12.3202296952608));
#108518=CARTESIAN_POINT('Ctrl Pts',(-9.36292411481005,4.3515421107202,12.3175750755878));
#108519=CARTESIAN_POINT('Ctrl Pts',(-9.35155387096724,4.35222566786066,
12.3120184891237));
#108520=CARTESIAN_POINT('Ctrl Pts',(-9.34570567568064,4.35257705179822,
12.3091118504968));
#108521=CARTESIAN_POINT('Ctrl Pts',(-9.33073637664173,4.35347606570667,
12.3015465206673));
#108522=CARTESIAN_POINT('Ctrl Pts',(-9.32164428256312,4.35402172131619,
12.2968310108645));
#108523=CARTESIAN_POINT('Ctrl Pts',(-9.28318524384873,4.35632895778256,
12.2763695257117));
#108524=CARTESIAN_POINT('Ctrl Pts',(-9.25431004452896,4.35805879535214,
12.2597179324156));
#108525=CARTESIAN_POINT('Ctrl Pts',(-9.17768256559356,4.36266759721873,
12.2119698606601));
#108526=CARTESIAN_POINT('Ctrl Pts',(-9.13113600827753,4.36548558557964,
12.1790474537085));
#108527=CARTESIAN_POINT('Ctrl Pts',(-9.06792739507211,4.36944187511943,
12.1285590632618));
#108528=CARTESIAN_POINT('Ctrl Pts',(-9.04959881169916,4.37060630122378,
12.1131677744841));
#108529=CARTESIAN_POINT('Ctrl Pts',(-8.96385440927159,4.37617070434543,
12.037502478922));
#108530=CARTESIAN_POINT('Ctrl Pts',(-8.90175186074244,4.38054913836327,
11.971522668923));
#108531=CARTESIAN_POINT('Ctrl Pts',(-8.83894846368413,4.38592479157026,
11.8910265424341));
#108532=CARTESIAN_POINT('Ctrl Pts',(-8.8318668714319,4.38654675365553,11.881722148035));
#108533=CARTESIAN_POINT('Ctrl Pts',(-8.82223408834294,4.3874164853401,11.8687460372733));
#108534=CARTESIAN_POINT('Ctrl Pts',(-8.81958691330211,4.3876580410826,11.8651457470532));
#108535=CARTESIAN_POINT('Ctrl Pts',(-8.81507186845236,4.38807454162844,
11.8589457609359));
#108536=CARTESIAN_POINT('Ctrl Pts',(-8.81319594684265,4.38824894444864,
11.8563519347607));
#108537=CARTESIAN_POINT('Ctrl Pts',(-8.80929378889067,4.38861461406567,
11.8509189944278));
#108538=CARTESIAN_POINT('Ctrl Pts',(-8.80726918133989,4.38880599259048,
11.8480787756091));
#108539=CARTESIAN_POINT('Ctrl Pts',(-8.80235086006076,4.38927490761548,
11.8411266665044));
#108540=CARTESIAN_POINT('Ctrl Pts',(-8.79946815837098,4.38955317055933,
11.8370070652155));
#108541=CARTESIAN_POINT('Ctrl Pts',(-8.7891719422427,4.39055921897083,11.8221303669832));
#108542=CARTESIAN_POINT('Ctrl Pts',(-8.78188153140228,4.39129456988115,
11.8112892814181));
#108543=CARTESIAN_POINT('Ctrl Pts',(-8.76405427341029,4.39314834541059,
11.7839974664613));
#108544=CARTESIAN_POINT('Ctrl Pts',(-8.753700028478,4.39427588787582,11.767430897717));
#108545=CARTESIAN_POINT('Ctrl Pts',(-8.71010388074995,4.39923549520253,
11.6944678142483));
#108546=CARTESIAN_POINT('Ctrl Pts',(-8.68033651541236,4.40318424201987,
11.6360857662842));
#108547=CARTESIAN_POINT('Ctrl Pts',(-8.61349356452003,4.41340422112537,
11.4799295966039));
#108548=CARTESIAN_POINT('Ctrl Pts',(-8.58279132160847,4.41960936200771,
11.3798137658191));
#108549=CARTESIAN_POINT('Ctrl Pts',(-8.55986463368865,4.42639467067139,
11.2609927101217));
#108550=CARTESIAN_POINT('Ctrl Pts',(-8.55700059874931,4.42731571203824,
11.2446626811821));
#108551=CARTESIAN_POINT('Ctrl Pts',(-8.55302306296479,4.42871907721364,
11.2194756706173));
#108552=CARTESIAN_POINT('Ctrl Pts',(-8.55171214278256,4.42920750387156,
11.2106516410122));
#108553=CARTESIAN_POINT('Ctrl Pts',(-8.54970580714675,4.4299999942246,11.1962413903572));
#108554=CARTESIAN_POINT('Ctrl Pts',(-8.54896180845184,4.43030556452011,
11.1906622590033));
#108555=CARTESIAN_POINT('Ctrl Pts',(-8.5474646733417,4.43094616816877,11.1789188044287));
#108556=CARTESIAN_POINT('Ctrl Pts',(-8.54671854818662,4.43128097748929,
11.1727536894348));
#108557=CARTESIAN_POINT('Ctrl Pts',(-8.54502222741896,4.43208153777317,
11.1579477573861));
#108558=CARTESIAN_POINT('Ctrl Pts',(-8.54410972596326,4.4325461109285,11.1493028034469));
#108559=CARTESIAN_POINT('Ctrl Pts',(-8.54121285508634,4.43414892854893,
11.1192996527263));
#108560=CARTESIAN_POINT('Ctrl Pts',(-8.53962098862819,4.43527505851465,
11.0979058031575));
#108561=CARTESIAN_POINT('Ctrl Pts',(-8.53509199129682,4.43977162261828,
11.0113630567045));
#108562=CARTESIAN_POINT('Ctrl Pts',(-8.53604006145651,4.44302476659197,
10.9460835370252));
#108563=CARTESIAN_POINT('Ctrl Pts',(-8.54680819821287,4.44952643021242,
10.8140017619516));
#108564=CARTESIAN_POINT('Ctrl Pts',(-8.55689734880188,4.45276409907855,
10.7473812312367));
#108565=CARTESIAN_POINT('Ctrl Pts',(-8.5845086068357,4.45901648981022,10.6234704505779));
#108566=CARTESIAN_POINT('Ctrl Pts',(-8.60102853696015,4.46201036422626,
10.5661016692836));
#108567=CARTESIAN_POINT('Ctrl Pts',(-8.62370958719293,4.4656129085021,10.5022827863349));
#108568=CARTESIAN_POINT('Ctrl Pts',(-8.62648242959269,4.46604654272255,
10.4946810877714));
#108569=CARTESIAN_POINT('Ctrl Pts',(-8.63079036824818,4.46671071561686,
10.4831684197133));
#108570=CARTESIAN_POINT('Ctrl Pts',(-8.6322795489361,4.46693865547146,10.4792403002204));
#108571=CARTESIAN_POINT('Ctrl Pts',(-8.63499649072198,4.46735166425808,
10.4721656723265));
#108572=CARTESIAN_POINT('Ctrl Pts',(-8.63621825226574,4.4675363803055,10.469016947591));
#108573=CARTESIAN_POINT('Ctrl Pts',(-8.63893946360308,4.46794560473289,
10.4620751900769));
#108574=CARTESIAN_POINT('Ctrl Pts',(-8.6404438572736,4.46817039661519,10.4582842269078));
#108575=CARTESIAN_POINT('Ctrl Pts',(-8.64485485056415,4.46882525345754,
10.4473029554661));
#108576=CARTESIAN_POINT('Ctrl Pts',(-8.6478027395085,4.46925765648791,10.4401295127875));
#108577=CARTESIAN_POINT('Ctrl Pts',(-8.67161106243556,4.47270724495156,
10.3834789321));
#108578=CARTESIAN_POINT('Ctrl Pts',(-8.69512131459534,4.47585912464434,
10.335164750206));
#108579=CARTESIAN_POINT('Ctrl Pts',(-8.78022628121704,4.48629403921791,
10.1822589838222));
#108580=CARTESIAN_POINT('Ctrl Pts',(-8.85218456131881,4.49369470354615,
10.0839894264824));
#108581=CARTESIAN_POINT('Ctrl Pts',(-8.95939012754774,4.50265881845623,
9.97034933335254));
#108582=CARTESIAN_POINT('Ctrl Pts',(-8.98423156756091,4.50462588743857,
9.94583484148541));
#108583=CARTESIAN_POINT('Ctrl Pts',(-9.01786948140973,4.50715121315438,
9.91493400650963));
#108584=CARTESIAN_POINT('Ctrl Pts',(-9.02589244845073,4.50774380653366,
9.90772574300453));
#108585=CARTESIAN_POINT('Ctrl Pts',(-9.03898964353153,4.50869581524709,
9.89621761201574));
#108586=CARTESIAN_POINT('Ctrl Pts',(-9.04401468049101,4.50905749535994,
9.89186258245043));
#108587=CARTESIAN_POINT('Ctrl Pts',(-9.05369392921946,4.50974741740859,
9.88358874728664));
#108588=CARTESIAN_POINT('Ctrl Pts',(-9.05834322823138,4.51007587987322,
9.87966442951265));
#108589=CARTESIAN_POINT('Ctrl Pts',(-9.06910340430252,4.51082941860507,
9.87069642864418));
#108590=CARTESIAN_POINT('Ctrl Pts',(-9.07523106938769,4.51125367234545,
9.86567312626953));
#108591=CARTESIAN_POINT('Ctrl Pts',(-9.09460976853472,4.51258043315257,
9.85004837179759));
#108592=CARTESIAN_POINT('Ctrl Pts',(-9.10800482151908,4.51347583936298,
9.83962727915443));
#108593=CARTESIAN_POINT('Ctrl Pts',(-9.17604020212013,4.51792154576474,
9.78857154048586));
#108594=CARTESIAN_POINT('Ctrl Pts',(-9.23329027237463,4.52133336940978,
9.75155049149914));
#108595=CARTESIAN_POINT('Ctrl Pts',(-9.37140400765338,4.52908766400374,
9.67533560828199));
#108596=CARTESIAN_POINT('Ctrl Pts',(-9.45370185317432,4.53336269262486,
9.63932898951885));
#108597=CARTESIAN_POINT('Ctrl Pts',(-9.57831253845299,4.53993716880449,
9.5979487231896));
#108598=CARTESIAN_POINT('Ctrl Pts',(-9.6183924081122,4.54206851476162,9.58651382446483));
#108599=CARTESIAN_POINT('Ctrl Pts',(-9.66567293564811,4.54465834111858,
9.5751820656132));
#108600=CARTESIAN_POINT('Ctrl Pts',(-9.67245545022669,4.54503165386277,
9.57360759387172));
#108601=CARTESIAN_POINT('Ctrl Pts',(-9.68346842367236,4.54564109254178,
9.57113376597176));
#108602=CARTESIAN_POINT('Ctrl Pts',(-9.68769216435107,4.54587560621555,
9.5702046410822));
#108603=CARTESIAN_POINT('Ctrl Pts',(-9.69522856534511,4.54629553421421,
9.56858179505312));
#108604=CARTESIAN_POINT('Ctrl Pts',(-9.69853958525993,4.5464805387279,9.56788082797028));
#108605=CARTESIAN_POINT('Ctrl Pts',(-9.70574813404548,4.54688446053319,
9.56638083234857));
#108606=CARTESIAN_POINT('Ctrl Pts',(-9.70964644350608,4.54710361226988,
9.56558622080727));
#108607=CARTESIAN_POINT('Ctrl Pts',(-9.7206908268142,4.5477264225081,9.56338185666804));
#108608=CARTESIAN_POINT('Ctrl Pts',(-9.72784415191331,4.54813208929254,
9.56200956405307));
#108609=CARTESIAN_POINT('Ctrl Pts',(-9.7744704762348,4.55078976391258,9.55342514274144));
#108610=CARTESIAN_POINT('Ctrl Pts',(-9.81421268169529,4.55311748327766,
9.54778620047079));
#108611=CARTESIAN_POINT('Ctrl Pts',(-9.99026490805148,4.56356191432461,
9.53015123061777));
#108612=CARTESIAN_POINT('Ctrl Pts',(-10.12766917171,4.57198130819257,9.53567044634369));
#108613=CARTESIAN_POINT('Ctrl Pts',(-10.2957513812052,4.58177402193593,
9.56629179590992));
#108614=CARTESIAN_POINT('Ctrl Pts',(-10.3289777944741,4.58368954345081,
9.57354916964442));
#108615=CARTESIAN_POINT('Ctrl Pts',(-10.3722756687432,4.58615952588042,
9.58459997551297));
#108616=CARTESIAN_POINT('Ctrl Pts',(-10.3825989798174,4.58674648353971,
9.5873555181993));
#108617=CARTESIAN_POINT('Ctrl Pts',(-10.399275183982,4.58769166096452,9.59200302004895));
#108618=CARTESIAN_POINT('Ctrl Pts',(-10.4056468954956,4.58805208702374,
9.59382548512793));
#108619=CARTESIAN_POINT('Ctrl Pts',(-10.4178497370601,4.58874105931627,
9.59740564135852));
#108620=CARTESIAN_POINT('Ctrl Pts',(-10.4236826931945,4.58906981439859,
9.59915657024715));
#108621=CARTESIAN_POINT('Ctrl Pts',(-10.4371230409777,4.58982608123282,
9.60328270304028));
#108622=CARTESIAN_POINT('Ctrl Pts',(-10.4447223382625,4.59025274953959,
9.60568374970993));
#108623=CARTESIAN_POINT('Ctrl Pts',(-10.468678635121,4.59159510281259,9.61346867616115));
#108624=CARTESIAN_POINT('Ctrl Pts',(-10.4849607406408,4.59250344029012,
9.61907933331101));
#108625=CARTESIAN_POINT('Ctrl Pts',(-10.5670173406499,4.59706606919631,
9.64898564152315));
#108626=CARTESIAN_POINT('Ctrl Pts',(-10.6310866773151,4.60057298233745,
9.6776991751375));
#108627=CARTESIAN_POINT('Ctrl Pts',(-10.7843200184807,4.60911327662862,
9.76005778247237));
#108628=CARTESIAN_POINT('Ctrl Pts',(-10.8702841163474,4.61403648628601,
9.81880710697756));
#108629=CARTESIAN_POINT('Ctrl Pts',(-10.9696661131851,4.6207100064064,9.9035074692363));
#108630=CARTESIAN_POINT('Ctrl Pts',(-10.9895502016247,4.62210286893229,
9.92141830819711));
#108631=CARTESIAN_POINT('Ctrl Pts',(-11.0137888928878,4.62389076601552,
9.94448623635616));
#108632=CARTESIAN_POINT('Ctrl Pts',(-11.0186149126043,4.62425138369602,
9.9491427875409));
#108633=CARTESIAN_POINT('Ctrl Pts',(-11.026190752231,4.62482518483648,9.95655381693644));
#108634=CARTESIAN_POINT('Ctrl Pts',(-11.0289619389371,4.62503673070563,
9.95928643497953));
#108635=CARTESIAN_POINT('Ctrl Pts',(-11.0338893927735,4.62541591633545,
9.96418422925124));
#108636=CARTESIAN_POINT('Ctrl Pts',(-11.0360498150024,4.62558322626069,
9.96634514091118));
#108637=CARTESIAN_POINT('Ctrl Pts',(-11.0412093646059,4.62598532784425,
9.97153828552069));
#108638=CARTESIAN_POINT('Ctrl Pts',(-11.044202001053,4.62622061221306,9.97457685848739));
#108639=CARTESIAN_POINT('Ctrl Pts',(-11.0521202808657,4.62684853915885,
9.98268728974459));
#108640=CARTESIAN_POINT('Ctrl Pts',(-11.057022465169,4.62724287806036,9.98778177256818));
#108641=CARTESIAN_POINT('Ctrl Pts',(-11.0970331405352,4.63050618427771,
10.029969557));
#108642=CARTESIAN_POINT('Ctrl Pts',(-11.1302117223681,4.63349764678874,
10.0688387602574));
#108643=CARTESIAN_POINT('Ctrl Pts',(-11.2000881254833,4.64033335998983,
10.1599490224313));
#108644=CARTESIAN_POINT('Ctrl Pts',(-11.2355408333677,4.64419583671292,
10.2130209581761));
#108645=CARTESIAN_POINT('Ctrl Pts',(-11.3125525732878,4.65341506154098,
10.3464056780626));
#108646=CARTESIAN_POINT('Ctrl Pts',(-11.3503623881414,4.65869589762568,
10.4285932223123));
#108647=CARTESIAN_POINT('Ctrl Pts',(-11.3843846726457,4.6643883727835,10.5251758135023));
#108648=CARTESIAN_POINT('Ctrl Pts',(-11.3882667257769,4.66505704095535,
10.5366486857993));
#108649=CARTESIAN_POINT('Ctrl Pts',(-11.3943693745582,4.66614079482623,
10.5554497808251));
#108650=CARTESIAN_POINT('Ctrl Pts',(-11.3966756164454,4.66655863937244,
10.5627494132611));
#108651=CARTESIAN_POINT('Ctrl Pts',(-11.4007022320805,4.6673034707351,10.575851292));
#108652=CARTESIAN_POINT('Ctrl Pts',(-11.4024440793121,4.66763114480397,
10.5816467098561));
#108653=CARTESIAN_POINT('Ctrl Pts',(-11.4060649000288,4.66832420622651,
10.5939705737451));
#108654=CARTESIAN_POINT('Ctrl Pts',(-11.4079344685314,4.66868928470783,
10.6005016489165));
#108655=CARTESIAN_POINT('Ctrl Pts',(-11.4128307836232,4.66966540194885,
10.6180676096622));
#108656=CARTESIAN_POINT('Ctrl Pts',(-11.4157737390103,4.67027375629095,
10.6291254879061));
#108657=CARTESIAN_POINT('Ctrl Pts',(-11.4219591890349,4.67160270119403,
10.653514067914));
#108658=CARTESIAN_POINT('Ctrl Pts',(-11.4251445537587,4.67232148261649,
10.6668582082903));
#108659=CARTESIAN_POINT('Ctrl Pts',(-11.4516421134135,4.67862788827222,
10.7852060970909));
#108660=CARTESIAN_POINT('Ctrl Pts',(-11.4634999999947,4.68383528789043,
10.8924348128952));
#108661=CARTESIAN_POINT('Ctrl Pts',(-11.4635,4.68907309470234,10.9999999999272));
#108662=CARTESIAN_POINT('Origin',(-10.,3.5,11.));
#108663=CARTESIAN_POINT('',(-11.4634997956549,5.26158527077303,10.9993582019504));
#108664=CARTESIAN_POINT('',(-11.4634997007504,5.18934561127431,10.9990641028533));
#108665=CARTESIAN_POINT('',(-11.4635,3.5,11.));
#108666=CARTESIAN_POINT('Ctrl Pts',(-11.4634997029717,5.26158526069413,
10.9990675828864));
#108667=CARTESIAN_POINT('Ctrl Pts',(-11.4634755855665,5.25968973270024,
10.9612134778287));
#108668=CARTESIAN_POINT('Ctrl Pts',(-11.4619828030479,5.25775673629656,
10.9233772234463));
#108669=CARTESIAN_POINT('Ctrl Pts',(-11.4584757697762,5.25538245818981,
10.8786321633612));
#108670=CARTESIAN_POINT('Ctrl Pts',(-11.4578756337479,5.25500801283252,
10.8716241626151));
#108671=CARTESIAN_POINT('Ctrl Pts',(-11.4568187498724,5.25439557666695,
10.8602478310136));
#108672=CARTESIAN_POINT('Ctrl Pts',(-11.4563928059141,5.25415915729695,
10.8558766756243));
#108673=CARTESIAN_POINT('Ctrl Pts',(-11.4556084282691,5.25374115395404,
10.8481859647311));
#108674=CARTESIAN_POINT('Ctrl Pts',(-11.4552582955775,5.25356001426152,
10.8448655729414));
#108675=CARTESIAN_POINT('Ctrl Pts',(-11.4545393244097,5.2531984936987,10.8382640875099));
#108676=CARTESIAN_POINT('Ctrl Pts',(-11.4541707448213,5.25301812810379,
10.8349830420699));
#108677=CARTESIAN_POINT('Ctrl Pts',(-11.4533491675055,5.25262647843925,
10.8278860456633));
#108678=CARTESIAN_POINT('Ctrl Pts',(-11.4528922506856,5.25241498772293,
10.8240706870113));
#108679=CARTESIAN_POINT('Ctrl Pts',(-11.4516020577256,5.25183460390441,
10.8136452198963));
#108680=CARTESIAN_POINT('Ctrl Pts',(-11.450738671356,5.25146410332905,10.8070390141617));
#108681=CARTESIAN_POINT('Ctrl Pts',(-11.4463740830346,5.24967334045397,
10.7753298421207));
#108682=CARTESIAN_POINT('Ctrl Pts',(-11.4422664340985,5.24822337335784,
10.7503161085175));
#108683=CARTESIAN_POINT('Ctrl Pts',(-11.432208964507,5.2451094017854,10.6976615065569));
#108684=CARTESIAN_POINT('Ctrl Pts',(-11.4261033503335,5.24344063725012,
10.6700603364372));
#108685=CARTESIAN_POINT('Ctrl Pts',(-11.4020201583697,5.23756598700445,
10.5744135924869));
#108686=CARTESIAN_POINT('Ctrl Pts',(-11.3799380833125,5.23329688406164,
10.5075008576346));
#108687=CARTESIAN_POINT('Ctrl Pts',(-11.3262091045415,5.22488178422601,
10.3771084134679));
#108688=CARTESIAN_POINT('Ctrl Pts',(-11.2945926722418,5.22074794160887,
10.3138102291102));
#108689=CARTESIAN_POINT('Ctrl Pts',(-11.2475274387565,5.21555244173908,
10.2345121605794));
#108690=CARTESIAN_POINT('Ctrl Pts',(-11.2361240249181,5.21435285740232,
10.2162310245885));
#108691=CARTESIAN_POINT('Ctrl Pts',(-11.2195507175855,5.21268894207907,
10.1909239206587));
#108692=CARTESIAN_POINT('Ctrl Pts',(-11.2147157502599,5.21221245147419,
10.183682840087));
#108693=CARTESIAN_POINT('Ctrl Pts',(-11.2063209485273,5.21140011377993,
10.1713501304063));
#108694=CARTESIAN_POINT('Ctrl Pts',(-11.2027928244289,5.21106309918862,
10.1662372877235));
#108695=CARTESIAN_POINT('Ctrl Pts',(-11.1960082256191,5.21042325002653,
10.1565379607346));
#108696=CARTESIAN_POINT('Ctrl Pts',(-11.1927576607588,5.2101202016491,10.1519474949386));
#108697=CARTESIAN_POINT('Ctrl Pts',(-11.185112366485,5.20941549545192,10.1412816819709));
#108698=CARTESIAN_POINT('Ctrl Pts',(-11.1806972297308,5.20901461968196,
10.1352211118231));
#108699=CARTESIAN_POINT('Ctrl Pts',(-11.1652488632197,5.2076325935004,10.1143543133129));
#108700=CARTESIAN_POINT('Ctrl Pts',(-11.1539819002871,5.20666040374123,
10.099722815278));
#108701=CARTESIAN_POINT('Ctrl Pts',(-11.0845615281312,5.20087216071541,
10.0130174974246));
#108702=CARTESIAN_POINT('Ctrl Pts',(-11.0199504829938,5.1963264719403,9.94638174895592));
#108703=CARTESIAN_POINT('Ctrl Pts',(-10.8776070953851,5.187219542736,9.82502956587028));
#108704=CARTESIAN_POINT('Ctrl Pts',(-10.7999921545526,5.18267587510986,
9.77087090758914));
#108705=CARTESIAN_POINT('Ctrl Pts',(-10.7091215358131,5.17721887130485,
9.71973592940985));
#108706=CARTESIAN_POINT('Ctrl Pts',(-10.7004813714721,5.17669861591017,
9.71498821730293));
#108707=CARTESIAN_POINT('Ctrl Pts',(-10.6869305407729,5.17587949513585,
9.70771940247305));
#108708=CARTESIAN_POINT('Ctrl Pts',(-10.6820523209375,5.17558398153923,
9.7051380999356));
#108709=CARTESIAN_POINT('Ctrl Pts',(-10.6729084221052,5.17502866328178,
9.70036562752736));
#108710=CARTESIAN_POINT('Ctrl Pts',(-10.6686463321352,5.17476925925277,
9.69816770362909));
#108711=CARTESIAN_POINT('Ctrl Pts',(-10.6613358253865,5.17432322927632,
9.6944431075811));
#108712=CARTESIAN_POINT('Ctrl Pts',(-10.6582926921947,5.17413723934396,
9.6929060460299));
#108713=CARTESIAN_POINT('Ctrl Pts',(-10.6523737345066,5.1737748122666,9.68994234247756));
#108714=CARTESIAN_POINT('Ctrl Pts',(-10.6494985542266,5.17359845765963,
9.68851451279253));
#108715=CARTESIAN_POINT('Ctrl Pts',(-10.6425777975542,5.17317327613372,
9.68510596848749));
#108716=CARTESIAN_POINT('Ctrl Pts',(-10.6385277540514,5.17292389951705,
9.6831344615964));
#108717=CARTESIAN_POINT('Ctrl Pts',(-10.623679497607,5.17200777221127,9.67599113149921));
#108718=CARTESIAN_POINT('Ctrl Pts',(-10.6128273229477,5.17133461093226,
9.670933314999));
#108719=CARTESIAN_POINT('Ctrl Pts',(-10.5279299822661,5.16604763741605,
9.63262648224487));
#108720=CARTESIAN_POINT('Ctrl Pts',(-10.4513021691369,5.16116135257995,
9.60545897853463));
#108721=CARTESIAN_POINT('Ctrl Pts',(-10.2950371137817,5.15143650110048,
9.56429241358354));
#108722=CARTESIAN_POINT('Ctrl Pts',(-10.2156849653794,5.146616058383,9.55024642308321));
#108723=CARTESIAN_POINT('Ctrl Pts',(-10.1084849545359,5.14039966155635,
9.54027280730143));
#108724=CARTESIAN_POINT('Ctrl Pts',(-10.0813289834433,5.13884880970364,
9.53850823091632));
#108725=CARTESIAN_POINT('Ctrl Pts',(-10.0345590566641,5.13621966845268,
9.53677691553001));
#108726=CARTESIAN_POINT('Ctrl Pts',(-10.0149665836054,5.13513084938983,
9.53644536257446));
#108727=CARTESIAN_POINT('Ctrl Pts',(-9.98698501833215,5.13359315332902,
9.53653383584459));
#108728=CARTESIAN_POINT('Ctrl Pts',(-9.97859763327772,5.13313445152896,
9.5366324637465));
#108729=CARTESIAN_POINT('Ctrl Pts',(-9.96405831972226,5.13234304401249,
9.53692846308017));
#108730=CARTESIAN_POINT('Ctrl Pts',(-9.95790599179437,5.13200932014684,
9.53709254475892));
#108731=CARTESIAN_POINT('Ctrl Pts',(-9.94529709641476,5.1313276891745,9.53750843084473));
#108732=CARTESIAN_POINT('Ctrl Pts',(-9.93884078912077,5.13097991180341,
9.53776419471243));
#108733=CARTESIAN_POINT('Ctrl Pts',(-9.92246994645456,5.13010113859548,
9.53852133593707));
#108734=CARTESIAN_POINT('Ctrl Pts',(-9.91255834330463,5.12957194529207,
9.53908085169949));
#108735=CARTESIAN_POINT('Ctrl Pts',(-9.87482127681209,5.12756733489161,
9.54159656254414));
#108736=CARTESIAN_POINT('Ctrl Pts',(-9.8470472076702,5.12611330053042,9.54424731715029));
#108737=CARTESIAN_POINT('Ctrl Pts',(-9.70587784545216,5.11880542912622,
9.56180568138952));
#108738=CARTESIAN_POINT('Ctrl Pts',(-9.59444050458146,5.11334769004883,
9.58917291230778));
#108739=CARTESIAN_POINT('Ctrl Pts',(-9.42362480176881,5.10441388646958,
9.65305945564372));
#108740=CARTESIAN_POINT('Ctrl Pts',(-9.36167182601259,5.101031704483,9.68129142481616));
#108741=CARTESIAN_POINT('Ctrl Pts',(-9.29435299519216,5.09696263609527,
9.71782663053099));
#108742=CARTESIAN_POINT('Ctrl Pts',(-9.28682914321674,5.09650202379302,
9.72199625713897));
#108743=CARTESIAN_POINT('Ctrl Pts',(-9.27564287051461,5.09580778722608,
9.72832509301882));
#108744=CARTESIAN_POINT('Ctrl Pts',(-9.27195225977204,5.09557719671801,
9.73043440220299));
#108745=CARTESIAN_POINT('Ctrl Pts',(-9.26562649824601,5.09517920826371,
9.734086442988));
#108746=CARTESIAN_POINT('Ctrl Pts',(-9.26298691447873,5.09501230575518,
9.73562138364736));
#108747=CARTESIAN_POINT('Ctrl Pts',(-9.25698700810334,5.09463101081404,
9.73913555350665));
#108748=CARTESIAN_POINT('Ctrl Pts',(-9.25362983904458,5.09441629474183,
9.74111992601837));
#108749=CARTESIAN_POINT('Ctrl Pts',(-9.24448934092962,5.09382803741676,
9.74657215320588));
#108750=CARTESIAN_POINT('Ctrl Pts',(-9.23872205751056,5.09345285803131,
9.75006655624689));
#108751=CARTESIAN_POINT('Ctrl Pts',(-9.20979566049898,5.09155163031159,
9.76786754949988));
#108752=CARTESIAN_POINT('Ctrl Pts',(-9.18701607253434,5.08999118940386,
9.7827776626815));
#108753=CARTESIAN_POINT('Ctrl Pts',(-9.14213434512544,5.08680802435196,
9.81397646491837));
#108754=CARTESIAN_POINT('Ctrl Pts',(-9.12004753578345,5.08518550233335,
9.83026975367048));
#108755=CARTESIAN_POINT('Ctrl Pts',(-9.01346194010103,5.07711991938126,
9.91362495883535));
#108756=CARTESIAN_POINT('Ctrl Pts',(-8.93608773617328,5.07054206553634,
9.98927607798419));
#108757=CARTESIAN_POINT('Ctrl Pts',(-8.83758630149709,5.06150619392063,
10.1095561121911));
#108758=CARTESIAN_POINT('Ctrl Pts',(-8.80925235217324,5.05880050826366,
10.1478165229008));
#108759=CARTESIAN_POINT('Ctrl Pts',(-8.77645351344813,5.0555296940229,10.1969444928169));
#108760=CARTESIAN_POINT('Ctrl Pts',(-8.77018908075466,5.05489792044144,
10.2065711967732));
#108761=CARTESIAN_POINT('Ctrl Pts',(-8.76039619594998,5.05389864445903,
10.2220148338608));
#108762=CARTESIAN_POINT('Ctrl Pts',(-8.75679394712738,5.05352845164113,
10.2277842127883));
#108763=CARTESIAN_POINT('Ctrl Pts',(-8.75006465730026,5.05283183558244,
10.2387310140819));
#108764=CARTESIAN_POINT('Ctrl Pts',(-8.74692924692391,5.05250511342552,
10.2439031020124));
#108765=CARTESIAN_POINT('Ctrl Pts',(-8.73990769015482,5.05176846833726,
10.2556493174005));
#108766=CARTESIAN_POINT('Ctrl Pts',(-8.73604074017696,5.05135924068338,
10.2622347524337));
#108767=CARTESIAN_POINT('Ctrl Pts',(-8.72620367741579,5.05030878366628,
10.2792916925588));
#108768=CARTESIAN_POINT('Ctrl Pts',(-8.72031100372346,5.04967029942666,
10.2898073359778));
#108769=CARTESIAN_POINT('Ctrl Pts',(-8.66936308286706,5.04406355405327,
10.3834187975242));
#108770=CARTESIAN_POINT('Ctrl Pts',(-8.63232514855251,5.03939311447577,
10.4706275187085));
#108771=CARTESIAN_POINT('Ctrl Pts',(-8.5836573710158,5.0314876418374,10.6253263373739));
#108772=CARTESIAN_POINT('Ctrl Pts',(-8.5678579871171,5.0282259393576,10.6911710418615));
#108773=CARTESIAN_POINT('Ctrl Pts',(-8.549470926683,5.0226690827907,10.8007754380119));
#108774=CARTESIAN_POINT('Ctrl Pts',(-8.54419044154288,5.02044590578664,
10.843977898029));
#108775=CARTESIAN_POINT('Ctrl Pts',(-8.54027073440169,5.01773083054033,
10.8947487349756));
#108776=CARTESIAN_POINT('Ctrl Pts',(-8.53975564997126,5.01733225976145,
10.9021542477164));
#108777=CARTESIAN_POINT('Ctrl Pts',(-8.53904928581138,5.01671387287829,
10.9135631910024));
#108778=CARTESIAN_POINT('Ctrl Pts',(-8.53881806813722,5.01649619147403,
10.9175641312434));
#108779=CARTESIAN_POINT('Ctrl Pts',(-8.5384221115899,5.01609320076966,10.9249416591144));
#108780=CARTESIAN_POINT('Ctrl Pts',(-8.53825263613581,5.01590815301889,
10.928317910064));
#108781=CARTESIAN_POINT('Ctrl Pts',(-8.53789495387849,5.0154871710431,10.9359732125391));
#108782=CARTESIAN_POINT('Ctrl Pts',(-8.53771383417716,5.01525085628491,
10.9402525004867));
#108783=CARTESIAN_POINT('Ctrl Pts',(-8.53729274356122,5.0146352972543,10.9513549110742));
#108784=CARTESIAN_POINT('Ctrl Pts',(-8.53708173196008,5.01425454615045,
10.9581789513449));
#108785=CARTESIAN_POINT('Ctrl Pts',(-8.5359916359523,5.01169682256599,11.0037528201883));
#108786=CARTESIAN_POINT('Ctrl Pts',(-8.53660458914721,5.00944947749499,
11.0425201051546));
#108787=CARTESIAN_POINT('Ctrl Pts',(-8.54099486081677,5.00478280293501,
11.1215122312014));
#108788=CARTESIAN_POINT('Ctrl Pts',(-8.54490058019728,5.00236223813583,
11.1616993806745));
#108789=CARTESIAN_POINT('Ctrl Pts',(-8.56696475193314,4.99273178500378,
11.3202876460314));
#108790=CARTESIAN_POINT('Ctrl Pts',(-8.59796787395804,4.9855527947838,11.4364512222269));
#108791=CARTESIAN_POINT('Ctrl Pts',(-8.64934541078253,4.97786394070211,
11.5638009987782));
#108792=CARTESIAN_POINT('Ctrl Pts',(-8.65619384643042,4.97689220511196,
11.5799348623083));
#108793=CARTESIAN_POINT('Ctrl Pts',(-8.66659808387112,4.97548965641671,
11.6032710555377));
#108794=CARTESIAN_POINT('Ctrl Pts',(-8.66992579261374,4.97505123054245,
11.6105728808316));
#108795=CARTESIAN_POINT('Ctrl Pts',(-8.67588715520685,4.97428329456737,
11.6233735560062));
#108796=CARTESIAN_POINT('Ctrl Pts',(-8.67849541015373,4.97395293199002,
11.6288839611913));
#108797=CARTESIAN_POINT('Ctrl Pts',(-8.68399875609455,4.97326738486312,
11.6403253320366));
#108798=CARTESIAN_POINT('Ctrl Pts',(-8.6868996909777,4.97291240976163,11.6462533444407));
#108799=CARTESIAN_POINT('Ctrl Pts',(-8.69454824430736,4.97199277000197,
11.6616188974231));
#108800=CARTESIAN_POINT('Ctrl Pts',(-8.6993581710419,4.97143026259548,11.6710251056552));
#108801=CARTESIAN_POINT('Ctrl Pts',(-8.71959996188531,4.96912600634019,
11.7095740906443));
#108802=CARTESIAN_POINT('Ctrl Pts',(-8.73591332439671,4.96741500709989,
11.7382443600286));
#108803=CARTESIAN_POINT('Ctrl Pts',(-8.75592542847624,4.96546474548255,
11.7708035772006));
#108804=CARTESIAN_POINT('Ctrl Pts',(-8.75869256791548,4.96519812670549,
11.7752519293319));
#108805=CARTESIAN_POINT('Ctrl Pts',(-8.77605019957874,4.96354421552162,
11.8028242212755));
#108806=CARTESIAN_POINT('Ctrl Pts',(-8.79126281992638,4.96217528399169,
11.8255509437413));
#108807=CARTESIAN_POINT('Ctrl Pts',(-8.86401032068164,4.95594935304557,
11.9279055733614));
#108808=CARTESIAN_POINT('Ctrl Pts',(-8.92883005670084,4.9512839532081,12.0020353917433));
#108809=CARTESIAN_POINT('Ctrl Pts',(-9.02371395851486,4.94481269803343,
12.0907338686076));
#108810=CARTESIAN_POINT('Ctrl Pts',(-9.04753887886299,4.9432114755027,12.1115990312943));
#108811=CARTESIAN_POINT('Ctrl Pts',(-9.08632673136406,4.94060796013744,
12.1434053114422));
#108812=CARTESIAN_POINT('Ctrl Pts',(-9.10085367148046,4.9396335569343,12.1548637865274));
#108813=CARTESIAN_POINT('Ctrl Pts',(-9.12016310113909,4.93833359319286,
12.1695093753298));
#108814=CARTESIAN_POINT('Ctrl Pts',(-9.12475323281289,4.9380242274341,12.1729485248401));
#108815=CARTESIAN_POINT('Ctrl Pts',(-9.13228720623301,4.93751567952162,
12.1785244965391));
#108816=CARTESIAN_POINT('Ctrl Pts',(-9.13521905212088,4.93731758864125,
12.1806775143976));
#108817=CARTESIAN_POINT('Ctrl Pts',(-9.14094660622165,4.93693017280231,
12.1848507982467));
#108818=CARTESIAN_POINT('Ctrl Pts',(-9.14374147298838,4.93674092313489,
12.1868721420564));
#108819=CARTESIAN_POINT('Ctrl Pts',(-9.15061203303867,4.9362752494116,12.1918042690779));
#108820=CARTESIAN_POINT('Ctrl Pts',(-9.15469555582124,4.93599809475877,
12.1947040342125));
#108821=CARTESIAN_POINT('Ctrl Pts',(-9.16863735566406,4.93505078028545,
12.2044970345653));
#108822=CARTESIAN_POINT('Ctrl Pts',(-9.17856544750274,4.93437439213182,
12.2112894822088));
#108823=CARTESIAN_POINT('Ctrl Pts',(-9.25117887590748,4.92942100961916,
12.2596657529805));
#108824=CARTESIAN_POINT('Ctrl Pts',(-9.31689934892642,4.92490967114821,
12.2964808148705));
#108825=CARTESIAN_POINT('Ctrl Pts',(-9.4438347339112,4.91649359397749,12.3552469547261));
#108826=CARTESIAN_POINT('Ctrl Pts',(-9.50425752596735,4.91260104888622,
12.3784971344845));
#108827=CARTESIAN_POINT('Ctrl Pts',(-9.60421650183225,4.90644809066128,
12.4095343557478));
#108828=CARTESIAN_POINT('Ctrl Pts',(-9.64288269011412,4.9041331906841,12.4198236844504));
#108829=CARTESIAN_POINT('Ctrl Pts',(-9.70739660982814,4.90038528060468,
12.4341884506568));
#108830=CARTESIAN_POINT('Ctrl Pts',(-9.73301708663121,4.89892589713732,
12.4391780647415));
#108831=CARTESIAN_POINT('Ctrl Pts',(-9.76800160948269,4.8969714786752,12.445024850324));
#108832=CARTESIAN_POINT('Ctrl Pts',(-9.77725948387391,4.89645789234265,
12.4464808119842));
#108833=CARTESIAN_POINT('Ctrl Pts',(-9.79280679586059,4.89560130172806,
12.4487730911937));
#108834=CARTESIAN_POINT('Ctrl Pts',(-9.79908875064772,4.89525680376032,
12.449657602763));
#108835=CARTESIAN_POINT('Ctrl Pts',(-9.81147995074967,4.89458038906313,
12.4513202148215));
#108836=CARTESIAN_POINT('Ctrl Pts',(-9.81758874477589,4.89424840603649,
12.4521006543883));
#108837=CARTESIAN_POINT('Ctrl Pts',(-9.83103491461209,4.89352086359869,
12.4537323027876));
#108838=CARTESIAN_POINT('Ctrl Pts',(-9.83837420046035,4.89312583683215,
12.4545665718233));
#108839=CARTESIAN_POINT('Ctrl Pts',(-9.86415595162818,4.89174524857921,
12.4572996823306));
#108840=CARTESIAN_POINT('Ctrl Pts',(-9.88262830129421,4.89076879311007,
12.4589036618054));
#108841=CARTESIAN_POINT('Ctrl Pts',(-10.0007090555364,4.88459951236762,
12.4668994038411));
#108842=CARTESIAN_POINT('Ctrl Pts',(-10.1007213423544,4.87972693026157,
12.4634384122665));
#108843=CARTESIAN_POINT('Ctrl Pts',(-10.2678917957476,4.87151565336667,
12.4404224677659));
#108844=CARTESIAN_POINT('Ctrl Pts',(-10.3354189620596,4.8681719934354,12.4262102986747));
#108845=CARTESIAN_POINT('Ctrl Pts',(-10.4210140868126,4.86364294751704,
12.40177861866));
#108846=CARTESIAN_POINT('Ctrl Pts',(-10.4402232318274,4.86260677039464,
12.395865178525));
#108847=CARTESIAN_POINT('Ctrl Pts',(-10.4719723016849,4.86085200656935,
12.3853708618621));
#108848=CARTESIAN_POINT('Ctrl Pts',(-10.4845826095537,4.86014378911869,
12.3810104808462));
#108849=CARTESIAN_POINT('Ctrl Pts',(-10.5018990546098,4.85915344031472,
12.3747564467042));
#108850=CARTESIAN_POINT('Ctrl Pts',(-10.5066579673278,4.85887939794238,
12.373009705496));
#108851=CARTESIAN_POINT('Ctrl Pts',(-10.5146829359345,4.85841395632396,
12.3700167682107));
#108852=CARTESIAN_POINT('Ctrl Pts',(-10.5179538264672,4.85822330989188,
12.3687835121437));
#108853=CARTESIAN_POINT('Ctrl Pts',(-10.5242024590992,4.85785725383048,
12.3664019237951));
#108854=CARTESIAN_POINT('Ctrl Pts',(-10.5271809090208,4.85768196700306,
12.365255552722));
#108855=CARTESIAN_POINT('Ctrl Pts',(-10.5342879153417,4.8572618262478,12.3624934235686));
#108856=CARTESIAN_POINT('Ctrl Pts',(-10.5384129012509,4.85701645025387,
12.3608686389492));
#108857=CARTESIAN_POINT('Ctrl Pts',(-10.5531646978716,4.85613364067106,
12.3549805063869));
#108858=CARTESIAN_POINT('Ctrl Pts',(-10.5637485015492,4.85549038716004,
12.3506113305621));
#108859=CARTESIAN_POINT('Ctrl Pts',(-10.6615021365235,4.84946440876787,
12.3089077829852));
#108860=CARTESIAN_POINT('Ctrl Pts',(-10.7448953321199,4.84370913233129,
12.2633104177998));
#108861=CARTESIAN_POINT('Ctrl Pts',(-10.9090151852976,4.83177891169248,
12.1516404715025));
#108862=CARTESIAN_POINT('Ctrl Pts',(-10.9883152594438,4.82565873900936,
12.0843541723756));
#108863=CARTESIAN_POINT('Ctrl Pts',(-11.0693445868901,4.8191227575577,11.9992618241951));
#108864=CARTESIAN_POINT('Ctrl Pts',(-11.0787037384997,4.81836239790206,
11.9891513036427));
#108865=CARTESIAN_POINT('Ctrl Pts',(-11.0927965728734,4.81720872523634,
11.9734891247832));
#108866=CARTESIAN_POINT('Ctrl Pts',(-11.0976336567299,4.81681112244816,
11.9680319127218));
#108867=CARTESIAN_POINT('Ctrl Pts',(-11.1060064907584,4.81611994398244,
11.9584422081271));
#108868=CARTESIAN_POINT('Ctrl Pts',(-11.1095603410807,4.81582562811086,
11.9543257695994));
#108869=CARTESIAN_POINT('Ctrl Pts',(-11.1175313959552,4.81516330106177,
11.9449881477051));
#108870=CARTESIAN_POINT('Ctrl Pts',(-11.1219351306993,4.81479584016562,
11.9397555985006));
#108871=CARTESIAN_POINT('Ctrl Pts',(-11.1337447976585,4.81380605208387,
11.9255219314478));
#108872=CARTESIAN_POINT('Ctrl Pts',(-11.1410802224491,4.81318654519539,
11.9164627914667));
#108873=CARTESIAN_POINT('Ctrl Pts',(-11.1753981465701,4.81026415733355,
11.8730297758536));
#108874=CARTESIAN_POINT('Ctrl Pts',(-11.2009416210287,4.80801749314418,
11.837544909161));
#108875=CARTESIAN_POINT('Ctrl Pts',(-11.2992659116678,4.79896335548206,
11.6871848714425));
#108876=CARTESIAN_POINT('Ctrl Pts',(-11.3574454588929,4.79264724596364,
11.5636049577396));
#108877=CARTESIAN_POINT('Ctrl Pts',(-11.4037531167807,4.78470173335965,
11.4143931677321));
#108878=CARTESIAN_POINT('Ctrl Pts',(-11.4093668779,4.78365530825791,11.3948790263124));
#108879=CARTESIAN_POINT('Ctrl Pts',(-11.4180199275808,4.7818847734404,11.3622602506343));
#108880=CARTESIAN_POINT('Ctrl Pts',(-11.4212878688681,4.78117127378845,
11.3492188034843));
#108881=CARTESIAN_POINT('Ctrl Pts',(-11.4255433633915,4.78017470792175,
11.3311860824075));
#108882=CARTESIAN_POINT('Ctrl Pts',(-11.4266853493238,4.77989986441022,
11.3262315352193));
#108883=CARTESIAN_POINT('Ctrl Pts',(-11.4285695120784,4.77943345855209,
11.317857892444));
#108884=CARTESIAN_POINT('Ctrl Pts',(-11.4293252997111,4.77924265632408,
11.3144418514934));
#108885=CARTESIAN_POINT('Ctrl Pts',(-11.4307464106937,4.77887662150018,
11.3079076545134));
#108886=CARTESIAN_POINT('Ctrl Pts',(-11.4314138045369,4.77870151384946,
11.3047899854013));
#108887=CARTESIAN_POINT('Ctrl Pts',(-11.4329823902885,4.77828222544987,
11.297343687328));
#108888=CARTESIAN_POINT('Ctrl Pts',(-11.4338741585712,4.7780375272814,11.293013132166));
#108889=CARTESIAN_POINT('Ctrl Pts',(-11.4369896913701,4.77715970790461,
11.2775287902159));
#108890=CARTESIAN_POINT('Ctrl Pts',(-11.4391029861991,4.77652085037875,
11.2663534897693));
#108891=CARTESIAN_POINT('Ctrl Pts',(-11.4560043752805,4.77102517608869,
11.1708964297008));
#108892=CARTESIAN_POINT('Ctrl Pts',(-11.463499998108,4.76586314678454,11.0855178363557));
#108893=CARTESIAN_POINT('Ctrl Pts',(-11.4635,4.76071734372175,11.0000000323785));
#108894=CARTESIAN_POINT('',(-11.4635901039152,4.6891878772753,11.0012825185114));
#108895=CARTESIAN_POINT('Ctrl Pts',(-11.4635,4.68907309470234,10.9999999999272));
#108896=CARTESIAN_POINT('Ctrl Pts',(-11.4635,4.68909395150544,11.0004283215526));
#108897=CARTESIAN_POINT('Ctrl Pts',(-11.4634998119651,4.68911480929044,
11.0008566484887));
#108898=CARTESIAN_POINT('Ctrl Pts',(-11.4634994358813,4.68913566809525,
11.0012849806131));
#108899=CARTESIAN_POINT('Ctrl Pts',(-11.4635901039152,4.6891878772753,11.0012825185114));
#108900=CARTESIAN_POINT('Ctrl Pts',(-11.4636777388583,4.69192656168224,
11.0559186640038));
#108901=CARTESIAN_POINT('Ctrl Pts',(-11.4607004171936,4.69466807467494,
11.1104470385295));
#108902=CARTESIAN_POINT('Ctrl Pts',(-11.4546742551396,4.6974780640643,11.1645633069226));
#108903=CARTESIAN_POINT('Ctrl Pts',(-11.4521770961465,4.69864248516869,
11.1869883471191));
#108904=CARTESIAN_POINT('Ctrl Pts',(-11.4491562647747,4.69981866476636,
11.2093432254121));
#108905=CARTESIAN_POINT('Ctrl Pts',(-11.4456120588868,4.70101127414283,
11.2316087754002));
#108906=CARTESIAN_POINT('Ctrl Pts',(-11.4419641095429,4.70223879272668,
11.2545260666185));
#108907=CARTESIAN_POINT('Ctrl Pts',(-11.4377624835256,4.70348395493515,
11.2773470170919));
#108908=CARTESIAN_POINT('Ctrl Pts',(-11.4330092972674,4.70475224144607,
11.3000478316342));
#108909=CARTESIAN_POINT('Ctrl Pts',(-11.4330055055567,4.7047532531833,11.3000659405228));
#108910=CARTESIAN_POINT('Ctrl Pts',(-11.433001713495,4.70475426493525,11.3000840493352));
#108911=CARTESIAN_POINT('Ctrl Pts',(-11.4329979210824,4.70475527670191,
11.3001021580711));
#108912=CARTESIAN_POINT('Ctrl Pts',(-11.4226630846898,4.70751247744201,
11.3494509081483));
#108913=CARTESIAN_POINT('Ctrl Pts',(-11.4096940881357,4.71038302461506,
11.3983377215902));
#108914=CARTESIAN_POINT('Ctrl Pts',(-11.3941777570286,4.71330675141998,
11.4464751367945));
#108915=CARTESIAN_POINT('Ctrl Pts',(-11.3927529584519,4.71357522479565,
11.4508953905386));
#108916=CARTESIAN_POINT('Ctrl Pts',(-11.3913067089278,4.71384414658019,
11.4553093023841));
#108917=CARTESIAN_POINT('Ctrl Pts',(-11.3898390930296,4.71411347018816,
11.4597166362923));
#108918=CARTESIAN_POINT('Ctrl Pts',(-11.3724198559226,4.71731009117817,
11.5120275947979));
#108919=CARTESIAN_POINT('Ctrl Pts',(-11.3519864902487,4.72056269471266,
11.5634159156947));
#108920=CARTESIAN_POINT('Ctrl Pts',(-11.3286919207662,4.72380664698362,
11.6135342257182));
#108921=CARTESIAN_POINT('Ctrl Pts',(-11.305420384918,4.7270473916396,11.6636029788341));
#108922=CARTESIAN_POINT('Ctrl Pts',(-11.2792935959025,4.73027916828496,
11.7124044339615));
#108923=CARTESIAN_POINT('Ctrl Pts',(-11.2504954040596,4.7334578634879,11.75961562067));
#108924=CARTESIAN_POINT('Ctrl Pts',(-11.2217143150982,4.73663467090403,
11.8067987692526));
#108925=CARTESIAN_POINT('Ctrl Pts',(-11.1902650975266,4.73975832445199,
11.8523936230707));
#108926=CARTESIAN_POINT('Ctrl Pts',(-11.156359763586,4.7428085445757,11.8960989536284));
#108927=CARTESIAN_POINT('Ctrl Pts',(-11.1224611767944,4.74585815770673,
11.9397955868414));
#108928=CARTESIAN_POINT('Ctrl Pts',(-11.0861074410123,4.74883437026357,
11.9816034092265));
#108929=CARTESIAN_POINT('Ctrl Pts',(-11.0475382901878,4.75174162379175,
12.0212422055306));
#108930=CARTESIAN_POINT('Ctrl Pts',(-11.0089336898426,4.75465154942293,
12.0609174344837));
#108931=CARTESIAN_POINT('Ctrl Pts',(-10.9681095032209,4.75749251768213,
12.0984194850311));
#108932=CARTESIAN_POINT('Ctrl Pts',(-10.9253348492182,4.76029276749457,
12.1334897620612));
#108933=CARTESIAN_POINT('Ctrl Pts',(-10.8825407135108,4.76309429268005,
12.1685760118397));
#108934=CARTESIAN_POINT('Ctrl Pts',(-10.8377941693208,4.76585535578055,
12.2012279601467));
#108935=CARTESIAN_POINT('Ctrl Pts',(-10.7913954152356,4.76862491232382,
12.2312125760717));
#108936=CARTESIAN_POINT('Ctrl Pts',(-10.7449091644897,4.77139969157089,
12.2612537356219));
#108937=CARTESIAN_POINT('Ctrl Pts',(-10.6967642821325,4.77418351636668,
12.2886169451701));
#108938=CARTESIAN_POINT('Ctrl Pts',(-10.6472962190233,4.77704033974134,
12.3131002464411));
#108939=CARTESIAN_POINT('Ctrl Pts',(-10.6095693929895,4.77921909653291,
12.3317724399682));
#108940=CARTESIAN_POINT('Ctrl Pts',(-10.5710736568645,4.78144073976509,
12.3487701007965));
#108941=CARTESIAN_POINT('Ctrl Pts',(-10.5319715987086,4.7837358552565,12.3640199685171));
#108942=CARTESIAN_POINT('Ctrl Pts',(-10.5319543624768,4.78373686694603,
12.3640266906761));
#108943=CARTESIAN_POINT('Ctrl Pts',(-10.531937126127,4.78373787864983,12.364033412496));
#108944=CARTESIAN_POINT('Ctrl Pts',(-10.5319198896591,4.78373889036791,
12.3640401339767));
#108945=CARTESIAN_POINT('Ctrl Pts',(-10.4849457905787,4.78649609942676,
12.3823580109954));
#108946=CARTESIAN_POINT('Ctrl Pts',(-10.4369187753071,4.78936665361016,
12.398217521904));
#108947=CARTESIAN_POINT('Ctrl Pts',(-10.3881270251176,4.79229038588681,
12.4115342578971));
#108948=CARTESIAN_POINT('Ctrl Pts',(-10.3836467989776,4.79255885302975,
12.4127570463493));
#108949=CARTESIAN_POINT('Ctrl Pts',(-10.3791601595532,4.79282776854608,
12.4139584062387));
#108950=CARTESIAN_POINT('Ctrl Pts',(-10.3746673507138,4.7930970858537,12.4151382793806));
#108951=CARTESIAN_POINT('Ctrl Pts',(-10.3213406599093,4.79629370545296,
12.4291425988338));
#108952=CARTESIAN_POINT('Ctrl Pts',(-10.2671391755717,4.79954630567773,
12.4401185686787));
#108953=CARTESIAN_POINT('Ctrl Pts',(-10.2124373755102,4.80279025309127,
12.4480043869183));
#108954=CARTESIAN_POINT('Ctrl Pts',(-10.1577896650668,4.80603099286124,
12.4558824075919));
#108955=CARTESIAN_POINT('Ctrl Pts',(-10.1026426195312,4.80926276308256,
12.4606767426257));
#108956=CARTESIAN_POINT('Ctrl Pts',(-10.0473671845871,4.81244145074323,
12.4623648252431));
#108957=CARTESIAN_POINT('Ctrl Pts',(-9.99212457740991,4.81561825059936,
12.4640519053179));
#108958=CARTESIAN_POINT('Ctrl Pts',(-9.93675371764679,4.81874189547464,
12.4626365536171));
#108959=CARTESIAN_POINT('Ctrl Pts',(-9.88162273653403,4.82179210620845,
12.4581316699812));
#108960=CARTESIAN_POINT('Ctrl Pts',(-9.8265027266688,4.82484170994024,12.4536276828321));
#108961=CARTESIAN_POINT('Ctrl Pts',(-9.77162252759448,4.8278179123832,12.4460353632545));
#108962=CARTESIAN_POINT('Ctrl Pts',(-9.71734782564662,4.83072515541604,
12.4354023108552));
#108963=CARTESIAN_POINT('Ctrl Pts',(-9.66302323850774,4.83363507056626,
12.4247594853604));
#108964=CARTESIAN_POINT('Ctrl Pts',(-9.60930534586025,4.83647602796213,
12.4110701644286));
#108965=CARTESIAN_POINT('Ctrl Pts',(-9.55655778992746,4.83927626678178,
12.3944183719835));
#108966=CARTESIAN_POINT('Ctrl Pts',(-9.50378621001815,4.84207778097562,
12.3777589954473));
#108967=CARTESIAN_POINT('Ctrl Pts',(-9.45198602283035,4.84483883295526,
12.3581341401879));
#108968=CARTESIAN_POINT('Ctrl Pts',(-9.40151644989201,4.84760837841011,
12.335667829337));
#108969=CARTESIAN_POINT('Ctrl Pts',(-9.35095170251484,4.8503831466144,12.3131591519986));
#108970=CARTESIAN_POINT('Ctrl Pts',(-9.30172295088496,4.85316696040023,
12.2877978380731));
#108971=CARTESIAN_POINT('Ctrl Pts',(-9.25418266356744,4.85602377286918,
12.2597544147948));
#108972=CARTESIAN_POINT('Ctrl Pts',(-9.21792543860034,4.85820255844705,
12.2383667294437));
#108973=CARTESIAN_POINT('Ctrl Pts',(-9.1826502608637,4.86042423198564,12.2154198526192));
#108974=CARTESIAN_POINT('Ctrl Pts',(-9.14850735228077,4.86271938086069,
12.1910099010785));
#108975=CARTESIAN_POINT('Ctrl Pts',(-9.14849230179559,4.86272039258188,
12.1909991409638));
#108976=CARTESIAN_POINT('Ctrl Pts',(-9.14847725152997,4.86272140431735,
12.1909883805648));
#108977=CARTESIAN_POINT('Ctrl Pts',(-9.14846220148391,4.8627224160671,12.1909776198815));
#108978=CARTESIAN_POINT('Ctrl Pts',(-9.10744809109168,4.86547961798553,
12.1616528025972));
#108979=CARTESIAN_POINT('Ctrl Pts',(-9.06791715830832,4.8683501659533,12.1301026005958));
#108980=CARTESIAN_POINT('Ctrl Pts',(-9.03009759816841,4.87127389294877,
12.0965222052036));
#108981=CARTESIAN_POINT('Ctrl Pts',(-9.02662483274124,4.87154236296774,
12.0934386993216));
#108982=CARTESIAN_POINT('Ctrl Pts',(-9.02316650693239,4.87181128137922,
12.0903381103193));
#108983=CARTESIAN_POINT('Ctrl Pts',(-9.01972280276393,4.87208060159934,
12.0872206106208));
#108984=CARTESIAN_POINT('Ctrl Pts',(-8.97884876513542,4.8752772190418,12.0502183613705));
#108985=CARTESIAN_POINT('Ctrl Pts',(-8.94003257657952,4.87852981825204,
12.010828350913));
#108986=CARTESIAN_POINT('Ctrl Pts',(-8.90353066838096,4.88177376548853,
11.9693303933416));
#108987=CARTESIAN_POINT('Ctrl Pts',(-8.86706485408297,4.88501450503768,
11.9278734698756));
#108988=CARTESIAN_POINT('Ctrl Pts',(-8.83290844136806,4.8882462758721,11.884312954634));
#108989=CARTESIAN_POINT('Ctrl Pts',(-8.80128307475971,4.89142496464193,
11.8389471485505));
#108990=CARTESIAN_POINT('Ctrl Pts',(-8.76967649066713,4.89460176556735,
11.7936082855212));
#108991=CARTESIAN_POINT('Ctrl Pts',(-8.74059782794154,4.89772541200718,
11.7464663345094));
#108992=CARTESIAN_POINT('Ctrl Pts',(-8.71423749251512,4.90077562445434,
11.6978366244731));
#108993=CARTESIAN_POINT('Ctrl Pts',(-8.68788240317584,4.90382522986521,
11.6492165924508));
#108994=CARTESIAN_POINT('Ctrl Pts',(-8.66424459950063,4.9068014341363,11.5991094002226));
#108995=CARTESIAN_POINT('Ctrl Pts',(-8.64348409300462,4.90970867880946,
11.5478472950859));
#108996=CARTESIAN_POINT('Ctrl Pts',(-8.62270450527309,4.91261859556678,
11.4965380743212));
#108997=CARTESIAN_POINT('Ctrl Pts',(-8.60480769478582,4.91545955438148,
11.444071793711));
#108998=CARTESIAN_POINT('Ctrl Pts',(-8.5899220535533,4.91825979412484,11.3907988970815));
#108999=CARTESIAN_POINT('Ctrl Pts',(-8.57502963273937,4.92106130922161,
11.3375017376113));
#109000=CARTESIAN_POINT('Ctrl Pts',(-8.56315147659081,4.92382236160641,
11.2833972028079));
#109001=CARTESIAN_POINT('Ctrl Pts',(-8.55438006501671,4.9265919067251,11.2288538967451));
#109002=CARTESIAN_POINT('Ctrl Pts',(-8.54559211254022,4.92936667458076,
11.1742077343183));
#109003=CARTESIAN_POINT('Ctrl Pts',(-8.53992320908011,4.93215048726976,
11.1191211960121));
#109004=CARTESIAN_POINT('Ctrl Pts',(-8.53742320045547,4.93500729776356,
11.0639826484335));
#109005=CARTESIAN_POINT('Ctrl Pts',(-8.53551652341311,4.93718609624019,
11.0219302323813));
#109006=CARTESIAN_POINT('Ctrl Pts',(-8.53545231415658,4.93940778273591,
10.9798479931522));
#109007=CARTESIAN_POINT('Ctrl Pts',(-8.53723218952537,4.94170294524313,
10.9379142664522));
#109008=CARTESIAN_POINT('Ctrl Pts',(-8.53723297410106,4.94170395695931,
10.9378957819092));
#109009=CARTESIAN_POINT('Ctrl Pts',(-8.53723375903481,4.94170496868977,
10.9378772973948));
#109010=CARTESIAN_POINT('Ctrl Pts',(-8.53723454432658,4.94170598043451,
10.9378588129088));
#109011=CARTESIAN_POINT('Ctrl Pts',(-8.53937461911631,4.94446318416237,
10.8874849473202));
#109012=CARTESIAN_POINT('Ctrl Pts',(-8.54418892528037,4.94733373376795,
10.8371367959789));
#109013=CARTESIAN_POINT('Ctrl Pts',(-8.55163873023419,4.95025746228649,
10.7871121384603));
#109014=CARTESIAN_POINT('Ctrl Pts',(-8.55232280526123,4.95052593235755,
10.7825186465291));
#109015=CARTESIAN_POINT('Ctrl Pts',(-8.5530290781923,4.95079485081986,10.7779279094913));
#109016=CARTESIAN_POINT('Ctrl Pts',(-8.55375750412409,4.95106417108964,
10.7733401740161));
#109017=CARTESIAN_POINT('Ctrl Pts',(-8.56240334503963,4.95426079013659,
10.7188873746995));
#109018=CARTESIAN_POINT('Ctrl Pts',(-8.57417349074655,4.95751339082138,
10.6648527792948));
#109019=CARTESIAN_POINT('Ctrl Pts',(-8.58897377717765,4.96075733947533,
10.6116040649015));
#109020=CARTESIAN_POINT('Ctrl Pts',(-8.60375942891101,4.9639980804746,10.5584080034649));
#109021=CARTESIAN_POINT('Ctrl Pts',(-8.62156890761889,4.96722985270143,
10.5059961179758));
#109022=CARTESIAN_POINT('Ctrl Pts',(-8.64227355478145,4.97040854288448,
10.4547170588198));
#109023=CARTESIAN_POINT('Ctrl Pts',(-8.6629659055008,4.97358534525061,10.4034684541812));
#109024=CARTESIAN_POINT('Ctrl Pts',(-8.686549872134,4.9767089931509,10.3533512631977));
#109025=CARTESIAN_POINT('Ctrl Pts',(-8.71286546266174,4.97975920716823,
10.3046972835109));
#109026=CARTESIAN_POINT('Ctrl Pts',(-8.73917581620004,4.98280881417132,
10.2560529863115));
#109027=CARTESIAN_POINT('Ctrl Pts',(-8.76821672288897,4.98578502014355,
10.2088713554413));
#109028=CARTESIAN_POINT('Ctrl Pts',(-8.79979741045243,4.9886922667281,10.163467982791));
#109029=CARTESIAN_POINT('Ctrl Pts',(-8.83140712435621,4.99160218541182,
10.1180228791383));
#109030=CARTESIAN_POINT('Ctrl Pts',(-8.86556141226627,4.99444314636371,
10.0743594493715));
#109031=CARTESIAN_POINT('Ctrl Pts',(-8.9020369816636,4.99724338856117,10.0327767523536));
#109032=CARTESIAN_POINT('Ctrl Pts',(-8.93852916378889,5.00004490612356,
9.99117511657633));
#109033=CARTESIAN_POINT('Ctrl Pts',(-8.97734495513403,5.00280596129228,
9.95165639069483));
#109034=CARTESIAN_POINT('Ctrl Pts',(-9.01822622710116,5.00557550960801,
9.91449948603069));
#109035=CARTESIAN_POINT('Ctrl Pts',(-9.05918459175291,5.00835028065543,
9.87727251198282));
#109036=CARTESIAN_POINT('Ctrl Pts',(-9.10221650595725,5.01113409695313,
9.84241678604415));
#109037=CARTESIAN_POINT('Ctrl Pts',(-9.14702398921705,5.01399091152725,
9.81018631863586));
#109038=CARTESIAN_POINT('Ctrl Pts',(-9.18119694485144,5.01616969485973,
9.78560537249271));
#109039=CARTESIAN_POINT('Ctrl Pts',(-9.2164018910126,5.01839136576603,9.76255101345989));
#109040=CARTESIAN_POINT('Ctrl Pts',(-9.25249037392882,5.02068651146548,
9.74112206565098));
#109041=CARTESIAN_POINT('Ctrl Pts',(-9.25250628189288,5.02068752317593,
9.74111261967531));
#109042=CARTESIAN_POINT('Ctrl Pts',(-9.25252219002876,5.02068853490066,
9.74110317401505));
#109043=CARTESIAN_POINT('Ctrl Pts',(-9.25253809833646,5.02068954663967,
9.7410937286702));
#109044=CARTESIAN_POINT('Ctrl Pts',(-9.29589163065568,5.02344675127292,
9.71535314888678));
#109045=CARTESIAN_POINT('Ctrl Pts',(-9.34068527737832,5.02631730163087,
9.69186606518692));
#109046=CARTESIAN_POINT('Ctrl Pts',(-9.38664850341049,5.02924103071376,
9.67076279903192));
#109047=CARTESIAN_POINT('Ctrl Pts',(-9.39086904267049,5.02950949997594,
9.66882500721419));
#109048=CARTESIAN_POINT('Ctrl Pts',(-9.39509940753062,5.02977841762489,
9.66690730986158));
#109049=CARTESIAN_POINT('Ctrl Pts',(-9.39933936688573,5.03004773707729,
9.66500980419198));
#109050=CARTESIAN_POINT('Ctrl Pts',(-9.44966448569674,5.03324435579571,
9.64248784342076));
#109051=CARTESIAN_POINT('Ctrl Pts',(-9.50134703697919,5.03649695591628,
9.62281079755896));
#109052=CARTESIAN_POINT('Ctrl Pts',(-9.55402765561808,5.0397409038115,9.60610077255766));
#109053=CARTESIAN_POINT('Ctrl Pts',(-9.60665618291867,5.04298164404532,
9.58940727066462));
#109054=CARTESIAN_POINT('Ctrl Pts',(-9.6602807545277,5.04621341531348,9.57567457046145));
#109055=CARTESIAN_POINT('Ctrl Pts',(-9.7145390850099,5.04939210439157,9.56498549236436));
#109056=CARTESIAN_POINT('Ctrl Pts',(-9.76876519149828,5.05256890564789,
9.55430276250511));
#109057=CARTESIAN_POINT('Ctrl Pts',(-9.82362429815191,5.05569255229287,
9.54665990766906));
#109058=CARTESIAN_POINT('Ctrl Pts',(-9.87875110638128,5.05874276495213,
9.54210429797237));
#109059=CARTESIAN_POINT('Ctrl Pts',(-9.93386694392061,5.06179237059389,
9.53754959487963));
#109060=CARTESIAN_POINT('Ctrl Pts',(-9.98925035416447,5.06476857510239,
9.53608094240158));
#109061=CARTESIAN_POINT('Ctrl Pts',(-10.0445327859616,5.06767582015448,
9.53771107726475));
#109062=CARTESIAN_POINT('Ctrl Pts',(-10.0998660288059,5.07058573730618,
9.5393427104133));
#109063=CARTESIAN_POINT('Ctrl Pts',(-10.1550980526427,5.07342669665712,
9.54407901163698));
#109064=CARTESIAN_POINT('Ctrl Pts',(-10.2098563768151,5.07622693720748,
9.55189644830043));
#109065=CARTESIAN_POINT('Ctrl Pts',(-10.2646396405576,5.07902845312185,
9.55971744539991));
#109066=CARTESIAN_POINT('Ctrl Pts',(-10.3189486537228,5.08178950659631,
9.57062271717316));
#109067=CARTESIAN_POINT('Ctrl Pts',(-10.3724087672457,5.08455905318362,
9.58454854673317));
#109068=CARTESIAN_POINT('Ctrl Pts',(-10.4259696944439,5.08733382250901,
9.59850063725613));
#109069=CARTESIAN_POINT('Ctrl Pts',(-10.478678237989,5.09011763705019,9.61548519505742));
#109070=CARTESIAN_POINT('Ctrl Pts',(-10.5301588194608,5.09297444983745,
9.63539152064834));
#109071=CARTESIAN_POINT('Ctrl Pts',(-10.5694212090269,5.09515323829253,
9.65057335985521));
#109072=CARTESIAN_POINT('Ctrl Pts',(-10.607969260143,5.09737491455902,9.66745379563866));
#109073=CARTESIAN_POINT('Ctrl Pts',(-10.6456390746319,5.09967006612909,
9.68596252398159));
#109074=CARTESIAN_POINT('Ctrl Pts',(-10.6456556796874,5.09967107784415,
9.6859706827279));
#109075=CARTESIAN_POINT('Ctrl Pts',(-10.6456722845726,5.0996720895735,9.6859788417905));
#109076=CARTESIAN_POINT('Ctrl Pts',(-10.6456888892876,5.09967310131713,
9.68598700116936));
#109077=CARTESIAN_POINT('Ctrl Pts',(-10.6909400568651,5.10243030494418,
9.70822293961197));
#109078=CARTESIAN_POINT('Ctrl Pts',(-10.7350912328075,5.10530085442953,
9.73289653818946));
#109079=CARTESIAN_POINT('Ctrl Pts',(-10.7778854184091,5.1082245827779,9.75985247627576));
#109080=CARTESIAN_POINT('Ctrl Pts',(-10.7818149703992,5.10849305248677,
9.76232769010826));
#109081=CARTESIAN_POINT('Ctrl Pts',(-10.7857330652942,5.10876197058531,
9.76482211509285));
#109082=CARTESIAN_POINT('Ctrl Pts',(-10.7896394953668,5.1090312904899,9.76733561083399));
#109083=CARTESIAN_POINT('Ctrl Pts',(-10.83600579177,5.11222790896037,9.79716885663062));
#109084=CARTESIAN_POINT('Ctrl Pts',(-10.8807316418915,5.11548050900234,
9.82969377446877));
#109085=CARTESIAN_POINT('Ctrl Pts',(-10.9235183751133,5.11872445694514,
9.86467616570817));
#109086=CARTESIAN_POINT('Ctrl Pts',(-10.9662628001444,5.12196519722151,
9.89962396581228));
#109087=CARTESIAN_POINT('Ctrl Pts',(-11.0070722105773,5.12519696865785,
9.93702414598331));
#109088=CARTESIAN_POINT('Ctrl Pts',(-11.0456792379536,5.12837565798173,
9.97661858986932));
#109089=CARTESIAN_POINT('Ctrl Pts',(-11.0842633365815,5.13155245947915,
10.0161895185793));
#109090=CARTESIAN_POINT('Ctrl Pts',(-11.1206477753381,5.13467610644268,
10.0579520276114));
#109091=CARTESIAN_POINT('Ctrl Pts',(-11.1545932254964,5.13772631944924,
10.1016261013782));
#109092=CARTESIAN_POINT('Ctrl Pts',(-11.1885319201848,5.14077592543417,
10.1452914835857));
#109093=CARTESIAN_POINT('Ctrl Pts',(-11.2200325561578,5.14375213031462,
10.1908676697158));
#109094=CARTESIAN_POINT('Ctrl Pts',(-11.2488830294713,5.14665937572077,
10.2380529909611));
#109095=CARTESIAN_POINT('Ctrl Pts',(-11.2777600197117,5.1495692932222,10.2852816809822));
#109096=CARTESIAN_POINT('Ctrl Pts',(-11.3039817912036,5.15241025290498,
10.3341225188811));
#109097=CARTESIAN_POINT('Ctrl Pts',(-11.327364464775,5.15521049372753,10.3842507215798));
#109098=CARTESIAN_POINT('Ctrl Pts',(-11.350757787916,5.15801200991149,10.4344017550202));
#109099=CARTESIAN_POINT('Ctrl Pts',(-11.3713090831897,5.16077306359557,
10.4858414077179));
#109100=CARTESIAN_POINT('Ctrl Pts',(-11.3888669371384,5.16354261029997,
10.538221117345));
#109101=CARTESIAN_POINT('Ctrl Pts',(-11.4064579012108,5.16631737974024,
10.5906996032044));
#109102=CARTESIAN_POINT('Ctrl Pts',(-11.4210435465301,5.16910119430287,
10.6441217377681));
#109103=CARTESIAN_POINT('Ctrl Pts',(-11.4325112956144,5.17195800700105,
10.6981125013045));
#109104=CARTESIAN_POINT('Ctrl Pts',(-11.441257340803,5.1741367966458,10.7392893402973));
#109105=CARTESIAN_POINT('Ctrl Pts',(-11.4481905195216,5.17635847408748,
10.7807963793421));
#109106=CARTESIAN_POINT('Ctrl Pts',(-11.4532801239676,5.17865362687244,
10.8224579414613));
#109107=CARTESIAN_POINT('Ctrl Pts',(-11.4532823674888,5.17865463858643,
10.8224763060711));
#109108=CARTESIAN_POINT('Ctrl Pts',(-11.4532846106522,5.1786556503147,10.8224946707113));
#109109=CARTESIAN_POINT('Ctrl Pts',(-11.4532868534577,5.17865666205725,
10.8225130353818));
#109110=CARTESIAN_POINT('Ctrl Pts',(-11.4597488615248,5.1815717113611,10.8754256265488));
#109111=CARTESIAN_POINT('Ctrl Pts',(-11.4632505365527,5.18460896799363,
10.9286963294922));
#109112=CARTESIAN_POINT('Ctrl Pts',(-11.4638019408274,5.18770184618821,
10.9820734860361));
#109113=CARTESIAN_POINT('Ctrl Pts',(-11.4638605279395,5.18803046678456,
10.9877448484085));
#109114=CARTESIAN_POINT('Ctrl Pts',(-11.4638857947485,5.18835971530495,
10.9934173661873));
#109115=CARTESIAN_POINT('Ctrl Pts',(-11.4638777447092,5.18868951188054,
10.999090704177));
#109116=CARTESIAN_POINT('Origin',(-10.,3.5,11.));
#109117=CARTESIAN_POINT('',(-11.4634999578674,5.75937264474327,10.9996488274338));
#109118=CARTESIAN_POINT('',(-11.4634999536212,5.6893446890626,10.9996315564861));
#109119=CARTESIAN_POINT('',(-11.4635,3.5,11.));
#109120=CARTESIAN_POINT('Ctrl Pts',(-11.4634999578674,5.75937264475447,
10.9996488276474));
#109121=CARTESIAN_POINT('Ctrl Pts',(-11.4634751845613,5.75396169207678,
10.8964068375278));
#109122=CARTESIAN_POINT('Ctrl Pts',(-11.4525265696792,5.74891300107215,
10.7934557525576));
#109123=CARTESIAN_POINT('Ctrl Pts',(-11.4259999127222,5.7427693151185,10.6700222404515));
#109124=CARTESIAN_POINT('Ctrl Pts',(-11.4206389907439,5.74165103674276,
10.6476565306573));
#109125=CARTESIAN_POINT('Ctrl Pts',(-11.4091188354672,5.73945225024823,
10.604145228243));
#109126=CARTESIAN_POINT('Ctrl Pts',(-11.403004960128,5.73837244821277,10.5829940732423));
#109127=CARTESIAN_POINT('Ctrl Pts',(-11.3882387752976,5.73592997125282,
10.5359181889912));
#109128=CARTESIAN_POINT('Ctrl Pts',(-11.3793329094427,5.73456239736482,
10.5100822163276));
#109129=CARTESIAN_POINT('Ctrl Pts',(-11.3599257625239,5.73175108511031,
10.4585152748437));
#109130=CARTESIAN_POINT('Ctrl Pts',(-11.3494045105388,5.73030702904237,
10.4328042122368));
#109131=CARTESIAN_POINT('Ctrl Pts',(-11.3354097251332,5.72846081828386,
10.4012018609594));
#109132=CARTESIAN_POINT('Ctrl Pts',(-11.3326175154221,5.72809581569482,
10.3950133064784));
#109133=CARTESIAN_POINT('Ctrl Pts',(-11.3281494377969,5.72751659991553,
10.3852914415388));
#109134=CARTESIAN_POINT('Ctrl Pts',(-11.3265022600051,5.72730407670075,
10.3817449600354));
#109135=CARTESIAN_POINT('Ctrl Pts',(-11.3235442150275,5.72692412715543,
10.3754423361269));
#109136=CARTESIAN_POINT('Ctrl Pts',(-11.3222389178505,5.72675704010261,
10.3726836458046));
#109137=CARTESIAN_POINT('Ctrl Pts',(-11.3191012445146,5.72635676583078,
10.3661056069008));
#109138=CARTESIAN_POINT('Ctrl Pts',(-11.3172609185385,5.72612309845923,
10.3622901392861));
#109139=CARTESIAN_POINT('Ctrl Pts',(-11.3116657873252,5.72541609907429,
10.3508175583392));
#109140=CARTESIAN_POINT('Ctrl Pts',(-11.3078606574134,5.7249398409676,10.3431853579949));
#109141=CARTESIAN_POINT('Ctrl Pts',(-11.2657307358421,5.71971904013604,
10.2605003968687));
#109142=CARTESIAN_POINT('Ctrl Pts',(-11.2210617867717,5.71465341987026,
10.1888653232984));
#109143=CARTESIAN_POINT('Ctrl Pts',(-11.1030396053925,5.7028217672449,10.0316203727491));
#109144=CARTESIAN_POINT('Ctrl Pts',(-11.02546074452,5.69611448254029,9.94981255713691));
#109145=CARTESIAN_POINT('Ctrl Pts',(-10.9256444203635,5.68882098988141,
9.8662758296158));
#109146=CARTESIAN_POINT('Ctrl Pts',(-10.9118086775227,5.68783492589036,
9.85511875640572));
#109147=CARTESIAN_POINT('Ctrl Pts',(-10.8919444391134,5.68645345897277,
9.83968890734707));
#109148=CARTESIAN_POINT('Ctrl Pts',(-10.8860819386882,5.68604985736793,
9.8352058057695));
#109149=CARTESIAN_POINT('Ctrl Pts',(-10.8752669265492,5.68531271865177,
9.82706438268404));
#109150=CARTESIAN_POINT('Ctrl Pts',(-10.8703247838548,5.68497866562314,
9.82339261973629));
#109151=CARTESIAN_POINT('Ctrl Pts',(-10.8602418527226,5.68430272781746,
9.81599979912695));
#109152=CARTESIAN_POINT('Ctrl Pts',(-10.8550997349456,5.68396092499455,
9.81228077144696));
#109153=CARTESIAN_POINT('Ctrl Pts',(-10.8422961207512,5.68311694730654,
9.80314683001247));
#109154=CARTESIAN_POINT('Ctrl Pts',(-10.8346063792301,5.68261628936738,
9.79777187573294));
#109155=CARTESIAN_POINT('Ctrl Pts',(-10.8052700618333,5.68072918415379,
9.77768358987166));
#109156=CARTESIAN_POINT('Ctrl Pts',(-10.7832811845505,5.67936154595055,
9.76347746699176));
#109157=CARTESIAN_POINT('Ctrl Pts',(-10.7266197596804,5.67594343044391,
9.7289891569875));
#109158=CARTESIAN_POINT('Ctrl Pts',(-10.6914711183829,5.67392031772148,
9.70952999718739));
#109159=CARTESIAN_POINT('Ctrl Pts',(-10.5979003951866,5.66872485468788,
9.66264916333116));
#109160=CARTESIAN_POINT('Ctrl Pts',(-10.5383879783768,5.66560704674836,
9.63760110345522));
#109161=CARTESIAN_POINT('Ctrl Pts',(-10.4063970857854,5.65879999027099,
9.59205176891092));
#109162=CARTESIAN_POINT('Ctrl Pts',(-10.3336020572187,5.65511096054384,
9.57305077187021));
#109163=CARTESIAN_POINT('Ctrl Pts',(-10.2478384602662,5.65052616382632,
9.55758774414966));
#109164=CARTESIAN_POINT('Ctrl Pts',(-10.2359719117291,5.64988650988392,
9.55559899725329));
#109165=CARTESIAN_POINT('Ctrl Pts',(-10.2191328204539,5.64896966465492,
9.55298992912052));
#109166=CARTESIAN_POINT('Ctrl Pts',(-10.2141792352614,5.64869883681889,
9.55224843570045));
#109167=CARTESIAN_POINT('Ctrl Pts',(-10.2058081376365,5.64823913171723,
9.55103928341762));
#109168=CARTESIAN_POINT('Ctrl Pts',(-10.2023925485951,5.64805099159888,
9.55055824409221));
#109169=CARTESIAN_POINT('Ctrl Pts',(-10.1953716961818,5.6476630370557,9.54959475288144));
#109170=CARTESIAN_POINT('Ctrl Pts',(-10.191766299478,5.64746315279071,9.54911366181618));
#109171=CARTESIAN_POINT('Ctrl Pts',(-10.1824716902298,5.64694622577664,
9.54790867244031));
#109172=CARTESIAN_POINT('Ctrl Pts',(-10.1767800033127,5.64662810518481,
9.54720477371541));
#109173=CARTESIAN_POINT('Ctrl Pts',(-10.1527148175632,5.6452768330234,9.54437211065711));
#109174=CARTESIAN_POINT('Ctrl Pts',(-10.1343067200596,5.64422792563633,
9.54255840327747));
#109175=CARTESIAN_POINT('Ctrl Pts',(-10.084318370806,5.64134705476572,9.53858819838437));
#109176=CARTESIAN_POINT('Ctrl Pts',(-10.0526952848321,5.6394896638266,9.53710662368729));
#109177=CARTESIAN_POINT('Ctrl Pts',(-9.92296211249676,5.63178824003443,
9.53524035496927));
#109178=CARTESIAN_POINT('Ctrl Pts',(-9.82497810757726,5.62580122030368,
9.54369478198711));
#109179=CARTESIAN_POINT('Ctrl Pts',(-9.70388979024914,5.61854609135911,
9.56654895927752));
#109180=CARTESIAN_POINT('Ctrl Pts',(-9.67933119119105,5.61708083113229,
9.57184218409491));
#109181=CARTESIAN_POINT('Ctrl Pts',(-9.61677945002552,5.61336909554873,
9.5870192468214));
#109182=CARTESIAN_POINT('Ctrl Pts',(-9.57902427984222,5.61114865112057,
9.59780441858418));
#109183=CARTESIAN_POINT('Ctrl Pts',(-9.53106311061488,5.60835377661213,
9.61361730866616));
#109184=CARTESIAN_POINT('Ctrl Pts',(-9.52042126618845,5.60773525419424,
9.61726249019927));
#109185=CARTESIAN_POINT('Ctrl Pts',(-9.50346254046259,5.60675198387285,
9.62329075023911));
#109186=CARTESIAN_POINT('Ctrl Pts',(-9.49711843267061,5.60638469245826,
9.62559542402473));
#109187=CARTESIAN_POINT('Ctrl Pts',(-9.48511146426278,5.60569051149681,
9.63005155629995));
#109188=CARTESIAN_POINT('Ctrl Pts',(-9.47944559020952,5.60536334880239,
9.63219443977061));
#109189=CARTESIAN_POINT('Ctrl Pts',(-9.46658550475148,5.60462163544372,
9.63714971871467));
#109190=CARTESIAN_POINT('Ctrl Pts',(-9.45939989423287,5.60420781903006,
9.63998402888817));
#109191=CARTESIAN_POINT('Ctrl Pts',(-9.43746554908926,5.60294629900765,
9.64883717405807));
#109192=CARTESIAN_POINT('Ctrl Pts',(-9.42279210151057,5.60210471859063,
9.65504012751637));
#109193=CARTESIAN_POINT('Ctrl Pts',(-9.35325211640324,5.59812368510101,
9.68578471831097));
#109194=CARTESIAN_POINT('Ctrl Pts',(-9.29982832664854,5.59509056882238,
9.71345219354998));
#109195=CARTESIAN_POINT('Ctrl Pts',(-9.16108869688416,5.58709484046341,
9.79651303161479));
#109196=CARTESIAN_POINT('Ctrl Pts',(-9.07960050566415,5.58227967614869,
9.8576271266484));
#109197=CARTESIAN_POINT('Ctrl Pts',(-8.97612388070272,5.57519700773471,
9.95354352513776));
#109198=CARTESIAN_POINT('Ctrl Pts',(-8.94824795382478,5.57317087940225,
9.98156463383729));
#109199=CARTESIAN_POINT('Ctrl Pts',(-8.9168971938909,5.57069971731275,10.0157399865872));
#109200=CARTESIAN_POINT('Ctrl Pts',(-8.91228811892609,5.57033123425293,
10.0208359061147));
#109201=CARTESIAN_POINT('Ctrl Pts',(-8.90485573970207,5.56972818882087,
10.0291705825478));
#109202=CARTESIAN_POINT('Ctrl Pts',(-8.90201046193255,5.56949518468129,
10.0323897055122));
#109203=CARTESIAN_POINT('Ctrl Pts',(-8.89695123557325,5.56907692763916,
10.0381647192384));
#109204=CARTESIAN_POINT('Ctrl Pts',(-8.8947319240538,5.56889207194336,10.0407158064448));
#109205=CARTESIAN_POINT('Ctrl Pts',(-8.88990825141467,5.5684872433973,10.0462995550094));
#109206=CARTESIAN_POINT('Ctrl Pts',(-8.88730750298332,5.56826702624702,
10.049335161397));
#109207=CARTESIAN_POINT('Ctrl Pts',(-8.87994370990434,5.56763802831837,
10.058001829791));
#109208=CARTESIAN_POINT('Ctrl Pts',(-8.87521081981659,5.56722717663803,
10.0636582134797));
#109209=CARTESIAN_POINT('Ctrl Pts',(-8.84361926069765,5.56444149849838,
10.1019991614934));
#109210=CARTESIAN_POINT('Ctrl Pts',(-8.81814803464039,5.56198257101558,
10.1357967613737));
#109211=CARTESIAN_POINT('Ctrl Pts',(-8.75528778205999,5.55542204332419,
10.2271911557369));
#109212=CARTESIAN_POINT('Ctrl Pts',(-8.72042312836446,5.55126199252031,
10.2864000872698));
#109213=CARTESIAN_POINT('Ctrl Pts',(-8.64759971134318,5.54146485055223,
10.4326978858288));
#109214=CARTESIAN_POINT('Ctrl Pts',(-8.61369675606955,5.53590411863829,
10.5214744415114));
#109215=CARTESIAN_POINT('Ctrl Pts',(-8.58542759551829,5.52996312122784,
10.6245501201369));
#109216=CARTESIAN_POINT('Ctrl Pts',(-8.58238160814586,5.52929731675091,
10.6362201117934));
#109217=CARTESIAN_POINT('Ctrl Pts',(-8.57764252592889,5.52821730858377,
10.6553410158908));
#109218=CARTESIAN_POINT('Ctrl Pts',(-8.5758629469609,5.52780037672069,10.6627697276098));
#109219=CARTESIAN_POINT('Ctrl Pts',(-8.57277864493263,5.52705662783049,
10.6761048997457));
#109220=CARTESIAN_POINT('Ctrl Pts',(-8.5714522317532,5.5267291302939,10.6820061200553));
#109221=CARTESIAN_POINT('Ctrl Pts',(-8.5687123185696,5.52603588030677,10.6945592275047));
#109222=CARTESIAN_POINT('Ctrl Pts',(-8.56730851784191,5.52567044088332,
10.7012131000287));
#109223=CARTESIAN_POINT('Ctrl Pts',(-8.56365983179548,5.52469201377673,
10.7191246880075));
#109224=CARTESIAN_POINT('Ctrl Pts',(-8.56150091082136,5.52408173412774,
10.7303995547849));
#109225=CARTESIAN_POINT('Ctrl Pts',(-8.55109180550355,5.52096694416077,
10.7884503208215));
#109226=CARTESIAN_POINT('Ctrl Pts',(-8.54498922372527,5.51853011876217,
10.8355845415506));
#109227=CARTESIAN_POINT('Ctrl Pts',(-8.53259470071599,5.51074545742772,
10.9900400917294));
#109228=CARTESIAN_POINT('Ctrl Pts',(-8.53582116955131,5.50565193260519,
11.0977597896024));
#109229=CARTESIAN_POINT('Ctrl Pts',(-8.55462079935962,5.49898023715777,
11.2312092810011));
#109230=CARTESIAN_POINT('Ctrl Pts',(-8.55918896416599,5.49761272712688,
11.258151524485));
#109231=CARTESIAN_POINT('Ctrl Pts',(-8.56991772437733,5.49480118658392,
11.312199953099));
#109232=CARTESIAN_POINT('Ctrl Pts',(-8.57610167191231,5.49335682468041,
11.3392896763584));
#109233=CARTESIAN_POINT('Ctrl Pts',(-8.584751264952,5.49151026392779,11.372759131778));
#109234=CARTESIAN_POINT('Ctrl Pts',(-8.58649586849336,5.49114523381042,
11.3793209973634));
#109235=CARTESIAN_POINT('Ctrl Pts',(-8.58931708511743,5.49056598383598,
11.3896424714518));
#109236=CARTESIAN_POINT('Ctrl Pts',(-8.59036323671866,5.49035345428409,
11.3934103923145));
#109237=CARTESIAN_POINT('Ctrl Pts',(-8.5922527280972,5.48997349937632,11.4001114631985));
#109238=CARTESIAN_POINT('Ctrl Pts',(-8.59309015561774,5.48980641335692,
11.403046217942));
#109239=CARTESIAN_POINT('Ctrl Pts',(-8.59511182572198,5.48940614934375,
11.4100480596921));
#109240=CARTESIAN_POINT('Ctrl Pts',(-8.59630454375795,5.48917249127103,
11.4141126159481));
#109241=CARTESIAN_POINT('Ctrl Pts',(-8.59995143745772,5.48846554736997,
11.4263437447193));
#109242=CARTESIAN_POINT('Ctrl Pts',(-8.60245931730221,5.48798933610691,
11.4344939577332));
#109243=CARTESIAN_POINT('Ctrl Pts',(-8.62994017114206,5.48287744936242,
11.521102342605));
#109244=CARTESIAN_POINT('Ctrl Pts',(-8.6614184597517,5.47793480198223,11.5973345113501));
#109245=CARTESIAN_POINT('Ctrl Pts',(-8.75160458821776,5.46608980884087,
11.7723064487831));
#109246=CARTESIAN_POINT('Ctrl Pts',(-8.81585200155387,5.45924476080286,
11.867611813658));
#109247=CARTESIAN_POINT('Ctrl Pts',(-8.90220574751374,5.45182716053409,
11.9679868464299));
#109248=CARTESIAN_POINT('Ctrl Pts',(-8.91409176617374,5.45083724424171,
11.9813022484115));
#109249=CARTESIAN_POINT('Ctrl Pts',(-8.93165118536552,5.44941837984032,
12.0002634567994));
#109250=CARTESIAN_POINT('Ctrl Pts',(-8.93713167711307,5.44898144814165,
12.0060850383939));
#109251=CARTESIAN_POINT('Ctrl Pts',(-8.94688621259826,5.44821401530213,
12.0162779983136));
#109252=CARTESIAN_POINT('Ctrl Pts',(-8.95114042123761,5.44788268275679,
12.0206680188376));
#109253=CARTESIAN_POINT('Ctrl Pts',(-8.96001183880727,5.44719861235042,
12.029708608236));
#109254=CARTESIAN_POINT('Ctrl Pts',(-8.96463303443362,5.4468460581491,12.0343550849767));
#109255=CARTESIAN_POINT('Ctrl Pts',(-8.97663391877337,5.44594008831225,
12.0462606091984));
#109256=CARTESIAN_POINT('Ctrl Pts',(-8.98405976100066,5.44538870881714,
12.0534727508013));
#109257=CARTESIAN_POINT('Ctrl Pts',(-9.01647678889355,5.44302023808074,
12.0842953054544));
#109258=CARTESIAN_POINT('Ctrl Pts',(-9.04222004650754,5.44123709629285,
12.1071007249004));
#109259=CARTESIAN_POINT('Ctrl Pts',(-9.11485506446146,5.43643698710528,
12.1670148256588));
#109260=CARTESIAN_POINT('Ctrl Pts',(-9.16325495190777,5.43348800578885,
12.2021911517027));
#109261=CARTESIAN_POINT('Ctrl Pts',(-9.29109000396541,5.42608651869492,
12.2836294975852));
#109262=CARTESIAN_POINT('Ctrl Pts',(-9.3729691046201,5.42169686344296,12.3255518478415));
#109263=CARTESIAN_POINT('Ctrl Pts',(-9.4828185889188,5.41565060637893,12.3693269994291));
#109264=CARTESIAN_POINT('Ctrl Pts',(-9.50767029696129,5.41427210959858,
12.3784572311984));
#109265=CARTESIAN_POINT('Ctrl Pts',(-9.53908618184528,5.41250063641447,
12.3890411602327));
#109266=CARTESIAN_POINT('Ctrl Pts',(-9.54543243094899,5.41214132864644,
12.3911309120148));
#109267=CARTESIAN_POINT('Ctrl Pts',(-9.55549153064934,5.41156918822611,
12.3943670852765));
#109268=CARTESIAN_POINT('Ctrl Pts',(-9.55919509641632,5.41135797793863,
12.3955423261554));
#109269=CARTESIAN_POINT('Ctrl Pts',(-9.5658195423956,5.410979123565,12.3976154399182));
#109270=CARTESIAN_POINT('Ctrl Pts',(-9.5687386030014,5.4108118065162,12.3985189289317));
#109271=CARTESIAN_POINT('Ctrl Pts',(-9.57574476515266,5.41040933565046,
12.4006634106976));
#109272=CARTESIAN_POINT('Ctrl Pts',(-9.57983446569008,5.41017368600598,
12.4018956513223));
#109273=CARTESIAN_POINT('Ctrl Pts',(-9.59227516179633,5.40945480484898,
12.4055847472982));
#109274=CARTESIAN_POINT('Ctrl Pts',(-9.60064258559932,5.40896850454128,
12.4079849692451));
#109275=CARTESIAN_POINT('Ctrl Pts',(-9.6201049153665,5.40783173372233,12.4133803584342));
#109276=CARTESIAN_POINT('Ctrl Pts',(-9.63121457885076,5.40717859637654,
12.4163197417373));
#109277=CARTESIAN_POINT('Ctrl Pts',(-9.75031488693492,5.40013989327112,
12.4463348987012));
#109278=CARTESIAN_POINT('Ctrl Pts',(-9.8610203945715,5.39330691625596,12.4611335607252));
#109279=CARTESIAN_POINT('Ctrl Pts',(-10.0530981639029,5.38185587283728,
12.4647657110337));
#109280=CARTESIAN_POINT('Ctrl Pts',(-10.1338624216389,5.37715698106629,
12.4596034144204));
#109281=CARTESIAN_POINT('Ctrl Pts',(-10.225726492517,5.37199539598312,12.4460377567033));
#109282=CARTESIAN_POINT('Ctrl Pts',(-10.2376330578694,5.37132972349012,
12.4441288672457));
#109283=CARTESIAN_POINT('Ctrl Pts',(-10.257041069279,5.37024988534706,12.4407707927581));
#109284=CARTESIAN_POINT('Ctrl Pts',(-10.2645569976898,5.36983299295565,
12.4394096660144));
#109285=CARTESIAN_POINT('Ctrl Pts',(-10.2780048613045,5.36908928759158,
12.4368653828941));
#109286=CARTESIAN_POINT('Ctrl Pts',(-10.283940728777,5.36876179442335,12.4357041810645));
#109287=CARTESIAN_POINT('Ctrl Pts',(-10.2965351810392,5.36806852584463,
12.4331592322019));
#109288=CARTESIAN_POINT('Ctrl Pts',(-10.3031916776256,5.36770306367599,
12.4317658003962));
#109289=CARTESIAN_POINT('Ctrl Pts',(-10.3210591360553,5.36672450877786,
12.4278953380821));
#109290=CARTESIAN_POINT('Ctrl Pts',(-10.3322511861807,5.36611412533469,
12.4253326715511));
#109291=CARTESIAN_POINT('Ctrl Pts',(-10.3896103689285,5.36299776132738,
12.4114866809262));
#109292=CARTESIAN_POINT('Ctrl Pts',(-10.4352403475258,5.3605595508308,12.398090594355));
#109293=CARTESIAN_POINT('Ctrl Pts',(-10.5817832296746,5.35276621454822,
12.3471962836403));
#109294=CARTESIAN_POINT('Ctrl Pts',(-10.6792175310725,5.34766620346676,
12.300796752291));
#109295=CARTESIAN_POINT('Ctrl Pts',(-10.8155966594527,5.33972311825338,
12.2163163638748));
#109296=CARTESIAN_POINT('Ctrl Pts',(-10.8589656600076,5.33705279799055,
12.1860861391736));
#109297=CARTESIAN_POINT('Ctrl Pts',(-10.9063592134991,5.33385381070026,
12.149085979583));
#109298=CARTESIAN_POINT('Ctrl Pts',(-10.912083377669,5.33346251160953,12.144547736108));
#109299=CARTESIAN_POINT('Ctrl Pts',(-10.9211837887232,5.33283206237605,
12.1372211081993));
#109300=CARTESIAN_POINT('Ctrl Pts',(-10.9245819828745,5.3325947579296,12.1344600378519));
#109301=CARTESIAN_POINT('Ctrl Pts',(-10.9305933451481,5.33217150373321,
12.1295307899567));
#109302=CARTESIAN_POINT('Ctrl Pts',(-10.9332114224758,5.33198598579658,
12.127368715312));
#109303=CARTESIAN_POINT('Ctrl Pts',(-10.9358469810233,5.3317980178168,12.1251767324135));
#109304=CARTESIAN_POINT('Ctrl Pts',(-10.935871955471,5.33179623653024,12.1251559598643));
#109305=CARTESIAN_POINT('Ctrl Pts',(-10.9359210161429,5.33179273709403,
12.125115150784));
#109306=CARTESIAN_POINT('Ctrl Pts',(-10.9359451023203,5.33179101895536,
12.12509511439));
#109307=CARTESIAN_POINT('Ctrl Pts',(-10.9359924261973,5.3317876430024,12.1250557448478));
#109308=CARTESIAN_POINT('Ctrl Pts',(-10.9360156639595,5.33178598519068,
12.1250364117379));
#109309=CARTESIAN_POINT('Ctrl Pts',(-10.9360613285538,5.33178272723379,
12.1249984177932));
#109310=CARTESIAN_POINT('Ctrl Pts',(-10.936083755474,5.33178112708882,12.1249797569685));
#109311=CARTESIAN_POINT('Ctrl Pts',(-10.9361278340951,5.33177798193673,
12.124943078127));
#109312=CARTESIAN_POINT('Ctrl Pts',(-10.9361494857658,5.33177643693775,
12.1249250602124));
#109313=CARTESIAN_POINT('Ctrl Pts',(-10.9361920472674,5.33177339971353,
12.1248896396417));
#109314=CARTESIAN_POINT('Ctrl Pts',(-10.9362129571844,5.33177190748768,
12.1248722369852));
#109315=CARTESIAN_POINT('Ctrl Pts',(-10.9362540669237,5.33176897356067,
12.124838020721));
#109316=CARTESIAN_POINT('Ctrl Pts',(-10.936274266782,5.33176753186205,12.1248212071492));
#109317=CARTESIAN_POINT('Ctrl Pts',(-10.9363139866415,5.33176469684657,
12.1247881440808));
#109318=CARTESIAN_POINT('Ctrl Pts',(-10.9363335065546,5.33176330354071,
12.1247718947183));
#109319=CARTESIAN_POINT('Ctrl Pts',(-10.9363718946589,5.33176056331656,
12.1247399368279));
#109320=CARTESIAN_POINT('Ctrl Pts',(-10.9363907629483,5.33175921639562,
12.1247242282746));
#109321=CARTESIAN_POINT('Ctrl Pts',(-10.9364278748516,5.33175656702357,
12.1246933296523));
#109322=CARTESIAN_POINT('Ctrl Pts',(-10.9364461184771,5.33175526457569,
12.124678139626));
#109323=CARTESIAN_POINT('Ctrl Pts',(-10.9364820065062,5.33175270234464,
12.1246482570197));
#109324=CARTESIAN_POINT('Ctrl Pts',(-10.9364996509585,5.33175144256175,
12.1246335644474));
#109325=CARTESIAN_POINT('Ctrl Pts',(-10.9365343649454,5.3317489639366,12.1246046566548));
#109326=CARTESIAN_POINT('Ctrl Pts',(-10.9365514344763,5.33174774509809,
12.1245904414825));
#109327=CARTESIAN_POINT('Ctrl Pts',(-10.9365850215086,5.33174534673773,
12.1245624695622));
#109328=CARTESIAN_POINT('Ctrl Pts',(-10.9366015390759,5.33174416721444,
12.1245487128011));
#109329=CARTESIAN_POINT('Ctrl Pts',(-10.9366340439596,5.33174184593896,
12.124521639689));
#109330=CARTESIAN_POINT('Ctrl Pts',(-10.9366500313338,5.33174070418565,
12.1245083233286));
#109331=CARTESIAN_POINT('Ctrl Pts',(-10.9366814969533,5.33173845695068,
12.1244821135399));
#109332=CARTESIAN_POINT('Ctrl Pts',(-10.936696975063,5.3317373514815,12.1244692202606));
#109333=CARTESIAN_POINT('Ctrl Pts',(-10.9367274412923,5.33173517545619,
12.1244438407989));
#109334=CARTESIAN_POINT('Ctrl Pts',(-10.9367424296135,5.33173410488827,
12.1244313544821));
#109335=CARTESIAN_POINT('Ctrl Pts',(-10.9367719358495,5.33173199727443,
12.1244067727304));
#109336=CARTESIAN_POINT('Ctrl Pts',(-10.9367864535228,5.33173096024819,
12.1243946775279));
#109337=CARTESIAN_POINT('Ctrl Pts',(-10.9368150353102,5.33172891852154,
12.1243708640621));
#109338=CARTESIAN_POINT('Ctrl Pts',(-10.9368290998166,5.33172791379536,
12.1243591455011));
#109339=CARTESIAN_POINT('Ctrl Pts',(-10.9368567931844,5.33172593539581,
12.1243360704784));
#109340=CARTESIAN_POINT('Ctrl Pts',(-10.9368704218646,5.3317249617375,12.1243247141951));
#109341=CARTESIAN_POINT('Ctrl Pts',(-10.9368972593753,5.33172304435154,
12.1243023506472));
#109342=CARTESIAN_POINT('Ctrl Pts',(-10.9369104683585,5.33172210061494,
12.1242913432807));
#109343=CARTESIAN_POINT('Ctrl Pts',(-10.936939951615,5.33171999406892,12.1242667732867));
#109344=CARTESIAN_POINT('Ctrl Pts',(-10.936956225926,5.33171883124094,12.1242532104234));
#109345=CARTESIAN_POINT('Ctrl Pts',(-10.9369886671538,5.33171651316581,
12.1242261730044));
#109346=CARTESIAN_POINT('Ctrl Pts',(-10.9370048339043,5.33171535793116,
12.1242126985953));
#109347=CARTESIAN_POINT('Ctrl Pts',(-10.9370370617322,5.33171305492154,
12.1241858366735));
#109348=CARTESIAN_POINT('Ctrl Pts',(-10.9370531227587,5.3317119071508,12.1241724492111));
#109349=CARTESIAN_POINT('Ctrl Pts',(-10.9401701544016,5.33148914562101,
12.1215741742901));
#109350=CARTESIAN_POINT('Ctrl Pts',(-10.9432603785816,5.33126661211374,
12.1189764988862));
#109351=CARTESIAN_POINT('Ctrl Pts',(-10.9520171785946,5.33063130069911,
12.1115533890752));
#109352=CARTESIAN_POINT('Ctrl Pts',(-10.9576576639757,5.33021642320187,
12.1066975372728));
#109353=CARTESIAN_POINT('Ctrl Pts',(-10.970538068595,5.32925643764137,12.0954366917194));
#109354=CARTESIAN_POINT('Ctrl Pts',(-10.9777520006666,5.32870948082866,
12.0890026188933));
#109355=CARTESIAN_POINT('Ctrl Pts',(-11.0011312587027,5.32690773868589,
12.0677311968709));
#109356=CARTESIAN_POINT('Ctrl Pts',(-11.0170261777752,5.32563647999188,
12.0526021907316));
#109357=CARTESIAN_POINT('Ctrl Pts',(-11.0812036386707,5.3203299720508,11.9887061673248));
#109358=CARTESIAN_POINT('Ctrl Pts',(-11.1263658751875,5.31617932768404,
11.9369314316597));
#109359=CARTESIAN_POINT('Ctrl Pts',(-11.2261998167071,5.30622416108125,
11.8047830664502));
#109360=CARTESIAN_POINT('Ctrl Pts',(-11.2768398944601,5.30048358756676,
11.7217526381657));
#109361=CARTESIAN_POINT('Ctrl Pts',(-11.3269480063776,5.29399935499248,
11.6175649812107));
#109362=CARTESIAN_POINT('Ctrl Pts',(-11.334682150088,5.29296785414346,11.6006672292563));
#109363=CARTESIAN_POINT('Ctrl Pts',(-11.3450408823767,5.29154114339736,
11.5768465399465));
#109364=CARTESIAN_POINT('Ctrl Pts',(-11.3479377299785,5.29113681741341,
11.5700445463398));
#109365=CARTESIAN_POINT('Ctrl Pts',(-11.353153594213,5.29039877158046,11.5575352419882));
#109366=CARTESIAN_POINT('Ctrl Pts',(-11.3554883440904,5.29006453105387,
11.5518347091583));
#109367=CARTESIAN_POINT('Ctrl Pts',(-11.360153480323,5.28938863376775,11.5402360369109));
#109368=CARTESIAN_POINT('Ctrl Pts',(-11.362481661722,5.28904705593197,11.534337149013));
#109369=CARTESIAN_POINT('Ctrl Pts',(-11.3681512763652,5.2882044151365,11.5196940987448));
#109370=CARTESIAN_POINT('Ctrl Pts',(-11.3714473246283,5.28770485840317,
11.5109325909669));
#109371=CARTESIAN_POINT('Ctrl Pts',(-11.383585847489,5.28582704331821,11.4777021494433));
#109372=CARTESIAN_POINT('Ctrl Pts',(-11.3918596346968,5.28446734965808,
11.4530298071265));
#109373=CARTESIAN_POINT('Ctrl Pts',(-11.4111225462403,5.2810736224459,11.3900659779375));
#109374=CARTESIAN_POINT('Ctrl Pts',(-11.4212146428339,5.27906643000164,
11.3515217464882));
#109375=CARTESIAN_POINT('Ctrl Pts',(-11.4522441215614,5.27185225915579,
11.2096092834566));
#109376=CARTESIAN_POINT('Ctrl Pts',(-11.4635668322466,5.26686403610331,
11.1044858904008));
#109377=CARTESIAN_POINT('Ctrl Pts',(-11.4634997032748,5.26158528452068,
10.9990680587078));
#109378=CARTESIAN_POINT('Ctrl Pts',(-11.4634997007504,5.18934561127431,
10.9990641028533));
#109379=CARTESIAN_POINT('Ctrl Pts',(-11.4635344412489,5.1923113975619,11.0533892061211));
#109380=CARTESIAN_POINT('Ctrl Pts',(-11.4605401187862,5.1952771838495,11.107830788412));
#109381=CARTESIAN_POINT('Ctrl Pts',(-11.4545042019612,5.19824297013709,
11.1620178276524));
#109382=CARTESIAN_POINT('Ctrl Pts',(-11.4484754290084,5.20120524623744,
11.2161407332582));
#109383=CARTESIAN_POINT('Ctrl Pts',(-11.4394122436747,5.20416752233779,
11.2700091551932));
#109384=CARTESIAN_POINT('Ctrl Pts',(-11.4273541165932,5.20712979843813,
11.3232529595293));
#109385=CARTESIAN_POINT('Ctrl Pts',(-11.4153051826419,5.21008981609572,
11.3764561707266));
#109386=CARTESIAN_POINT('Ctrl Pts',(-11.4002659467465,5.2130498337533,11.4290351781191));
#109387=CARTESIAN_POINT('Ctrl Pts',(-11.3823272438335,5.21600985141088,
11.4806283813465));
#109388=CARTESIAN_POINT('Ctrl Pts',(-11.3643946646374,5.21896885861022,
11.5322039722542));
#109389=CARTESIAN_POINT('Ctrl Pts',(-11.3435647590433,5.22192786580955,
11.582793912705));
#109390=CARTESIAN_POINT('Ctrl Pts',(-11.319977939129,5.22488687300889,11.6320526008275));
#109391=CARTESIAN_POINT('Ctrl Pts',(-11.2963724811946,5.22784821837996,
11.6813502125701));
#109392=CARTESIAN_POINT('Ctrl Pts',(-11.2700059889758,5.23080956375103,
11.729313977122));
#109393=CARTESIAN_POINT('Ctrl Pts',(-11.2410659713646,5.2337709091221,11.7756207222095));
#109394=CARTESIAN_POINT('Ctrl Pts',(-11.2121150934498,5.23673336579552,
11.8219448448023));
#109395=CARTESIAN_POINT('Ctrl Pts',(-11.1805890795016,5.23969582246895,
11.8666102632355));
#109396=CARTESIAN_POINT('Ctrl Pts',(-11.1467182142998,5.24265827914237,
11.9093236975869));
#109397=CARTESIAN_POINT('Ctrl Pts',(-11.1127842183309,5.2456262574392,11.9521167440727));
#109398=CARTESIAN_POINT('Ctrl Pts',(-11.0764970050056,5.24859423573603,
11.9929501330113));
#109399=CARTESIAN_POINT('Ctrl Pts',(-11.0381255798866,5.25156221403285,
12.0315655725086));
#109400=CARTESIAN_POINT('Ctrl Pts',(-11.0075603484484,5.25392639371253,
12.0623251766064));
#109401=CARTESIAN_POINT('Ctrl Pts',(-10.9756734759043,5.2562905733922,12.0916781261071));
#109402=CARTESIAN_POINT('Ctrl Pts',(-10.9426152373223,5.25865475307187,
12.1195127352415));
#109403=CARTESIAN_POINT('Ctrl Pts',(-10.9005236294952,5.26166495954922,
12.1549533243944));
#109404=CARTESIAN_POINT('Ctrl Pts',(-10.8563421100876,5.26467516602657,
12.1880911796638));
#109405=CARTESIAN_POINT('Ctrl Pts',(-10.8103525819758,5.26768537250392,
12.2186717945719));
#109406=CARTESIAN_POINT('Ctrl Pts',(-10.7644447514548,5.27069023153313,
12.2491980848835));
#109407=CARTESIAN_POINT('Ctrl Pts',(-10.7167357223031,5.27369509056234,
12.2771758599914));
#109408=CARTESIAN_POINT('Ctrl Pts',(-10.667540039108,5.27669994959155,12.3023910880329));
#109409=CARTESIAN_POINT('Ctrl Pts',(-10.6183930013213,5.27970183737237,
12.3275813828896));
#109410=CARTESIAN_POINT('Ctrl Pts',(-10.567762689191,5.28270372515319,12.3500143022685));
#109411=CARTESIAN_POINT('Ctrl Pts',(-10.5159905746625,5.28570561293401,
12.3695203455442));
#109412=CARTESIAN_POINT('Ctrl Pts',(-10.464249207591,5.28870571789379,12.3890148041814));
#109413=CARTESIAN_POINT('Ctrl Pts',(-10.4113678753837,5.29170582285357,
12.40558564628));
#109414=CARTESIAN_POINT('Ctrl Pts',(-10.3577083591411,5.29470592781335,
12.4191113345332));
#109415=CARTESIAN_POINT('Ctrl Pts',(-10.3040595216126,5.29770543572594,
12.4326343310558));
#109416=CARTESIAN_POINT('Ctrl Pts',(-10.2496333193866,5.30070494363854,
12.4431132482567));
#109417=CARTESIAN_POINT('Ctrl Pts',(-10.1948047908919,5.30370445155113,
12.4504769365438));
#109418=CARTESIAN_POINT('Ctrl Pts',(-10.1399258685872,5.30670671636121,
12.457847392919));
#109419=CARTESIAN_POINT('Ctrl Pts',(-10.0846444057419,5.30970898117128,
12.4620968295451));
#109420=CARTESIAN_POINT('Ctrl Pts',(-10.0293421949471,5.31271124598135,
12.4632058247546));
#109421=CARTESIAN_POINT('Ctrl Pts',(-9.97401479689575,5.31571487816558,
12.4643153250532));
#109422=CARTESIAN_POINT('Ctrl Pts',(-9.91866716070167,5.31871851034982,
12.4622815521487));
#109423=CARTESIAN_POINT('Ctrl Pts',(-9.86367939318694,5.32172214253405,
12.4571372420462));
#109424=CARTESIAN_POINT('Ctrl Pts',(-9.80858793123272,5.32473143888633,
12.4519832309434));
#109425=CARTESIAN_POINT('Ctrl Pts',(-9.75385821704293,5.32774073523861,
12.4437070440616));
#109426=CARTESIAN_POINT('Ctrl Pts',(-9.69986239769726,5.33075003159089,
12.4323929871666));
#109427=CARTESIAN_POINT('Ctrl Pts',(-9.65866357676656,5.33304612530791,
12.423760359499));
#109428=CARTESIAN_POINT('Ctrl Pts',(-9.61789185484979,5.33534221902494,
12.4133602535439));
#109429=CARTESIAN_POINT('Ctrl Pts',(-9.57770581235786,5.33763831274196,
12.4012493957478));
#109430=CARTESIAN_POINT('Ctrl Pts',(-9.52502142744368,5.34064851921379,
12.3853719155532));
#109431=CARTESIAN_POINT('Ctrl Pts',(-9.47312310926445,5.34365872568562,
12.3664857125845));
#109432=CARTESIAN_POINT('Ctrl Pts',(-9.42237806430953,5.34666893215746,
12.3446877516395));
#109433=CARTESIAN_POINT('Ctrl Pts',(-9.37172316484394,5.34967379118038,
12.3229285134477));
#109434=CARTESIAN_POINT('Ctrl Pts',(-9.32221795418694,5.3526786502033,12.2982679890259));
#109435=CARTESIAN_POINT('Ctrl Pts',(-9.27421358566678,5.35568350922622,
12.2708525999381));
#109436=CARTESIAN_POINT('Ctrl Pts',(-9.22625668457319,5.35868539700029,
12.2434643195907));
#109437=CARTESIAN_POINT('Ctrl Pts',(-9.17979814208299,5.36168728477436,
12.2133268314117));
#109438=CARTESIAN_POINT('Ctrl Pts',(-9.13516653800798,5.36468917254843,
12.1806334456633));
#109439=CARTESIAN_POINT('Ctrl Pts',(-9.09056144064778,5.367689277501,12.1479594765206));
#109440=CARTESIAN_POINT('Ctrl Pts',(-9.04778155628123,5.37068938245357,
12.1127329299325));
#109441=CARTESIAN_POINT('Ctrl Pts',(-9.0071263998327,5.37368948740614,12.0751903385405));
#109442=CARTESIAN_POINT('Ctrl Pts',(-8.96647933412269,5.37668899531109,
12.0376552184589));
#109443=CARTESIAN_POINT('Ctrl Pts',(-8.92795654433096,5.37968850321604,
11.9978053269995));
#109444=CARTESIAN_POINT('Ctrl Pts',(-8.89182259597033,5.38268801112098,
11.9559158389723));
#109445=CARTESIAN_POINT('Ctrl Pts',(-8.85565543630597,5.38569027592277,
11.9139878496306));
#109446=CARTESIAN_POINT('Ctrl Pts',(-8.82188185029077,5.38869254072455,
11.8700169192059));
#109447=CARTESIAN_POINT('Ctrl Pts',(-8.79072677729523,5.39169480552634,
11.8243121513415));
#109448=CARTESIAN_POINT('Ctrl Pts',(-8.75955751480167,5.39469843770192,
11.7785865673578));
#109449=CARTESIAN_POINT('Ctrl Pts',(-8.73100941535191,5.39770206987751,
11.7311260250927));
#109450=CARTESIAN_POINT('Ctrl Pts',(-8.70526281930563,5.40070570205309,
11.6822667241831));
#109451=CARTESIAN_POINT('Ctrl Pts',(-8.67946767103144,5.40371499839623,
11.6333152857379));
#109452=CARTESIAN_POINT('Ctrl Pts',(-8.65648479953044,5.40672429473936,
11.5829603009542));
#109453=CARTESIAN_POINT('Ctrl Pts',(-8.63644700932875,5.4097335910825,11.5315594902092));
#109454=CARTESIAN_POINT('Ctrl Pts',(-8.62115817096553,5.41202968485902,
11.492340660223));
#109455=CARTESIAN_POINT('Ctrl Pts',(-8.60758288415365,5.41432577863554,
11.4525134434279));
#109456=CARTESIAN_POINT('Ctrl Pts',(-8.59576032018933,5.41662187241205,
11.4122416422988));
#109457=CARTESIAN_POINT('Ctrl Pts',(-8.58026079688599,5.41963207892083,
11.3594448275003));
#109458=CARTESIAN_POINT('Ctrl Pts',(-8.5677104620999,5.4226422854296,11.3056618072144));
#109459=CARTESIAN_POINT('Ctrl Pts',(-8.55822881911808,5.42565249193837,
11.2512530835201));
#109460=CARTESIAN_POINT('Ctrl Pts',(-8.54876401969558,5.42865735099924,
11.1969410135984));
#109461=CARTESIAN_POINT('Ctrl Pts',(-8.54235718375553,5.43166221006011,
11.1420059621385));
#109462=CARTESIAN_POINT('Ctrl Pts',(-8.53907762460567,5.43466706912098,
11.0868220195123));
#109463=CARTESIAN_POINT('Ctrl Pts',(-8.53580130833152,5.43766895693358,
11.0316926435698));
#109464=CARTESIAN_POINT('Ctrl Pts',(-8.53564617431162,5.44067084474618,
10.9763153885533));
#109465=CARTESIAN_POINT('Ctrl Pts',(-8.5386299326001,5.44367273255878,10.921071069261));
#109466=CARTESIAN_POINT('Ctrl Pts',(-8.54161191883472,5.4466728375504,10.8658595595665));
#109467=CARTESIAN_POINT('Ctrl Pts',(-8.5477290739976,5.44967294254202,10.8107813553735));
#109468=CARTESIAN_POINT('Ctrl Pts',(-8.55694702714935,5.45267304753364,
10.7562165560443));
#109469=CARTESIAN_POINT('Ctrl Pts',(-8.56616314584764,5.45567255547808,
10.7016626155883));
#109470=CARTESIAN_POINT('Ctrl Pts',(-8.57847874910111,5.45867206342252,
10.6476223974979));
#109471=CARTESIAN_POINT('Ctrl Pts',(-8.59380800422581,5.46167157136696,
10.5944678545163));
#109472=CARTESIAN_POINT('Ctrl Pts',(-8.60915134872175,5.46467383620863,
10.5412644563175));
#109473=CARTESIAN_POINT('Ctrl Pts',(-8.62751373231333,5.46767610105029,
10.4889488680559));
#109474=CARTESIAN_POINT('Ctrl Pts',(-8.64875925144211,5.47067836589196,
10.4378784033354));
#109475=CARTESIAN_POINT('Ctrl Pts',(-8.67001444678982,5.47368199810769,
10.3867846786986));
#109476=CARTESIAN_POINT('Ctrl Pts',(-8.69415516470174,5.47668563032343,
10.336937684158));
#109477=CARTESIAN_POINT('Ctrl Pts',(-8.72099843466032,5.47968926253916,
10.2886721952161));
#109478=CARTESIAN_POINT('Ctrl Pts',(-8.7478923249234,5.4826985589224,10.2403156885349));
#109479=CARTESIAN_POINT('Ctrl Pts',(-8.77749866489277,5.48570785530564,
10.1935470924382));
#109480=CARTESIAN_POINT('Ctrl Pts',(-8.80959048072246,5.48871715168887,
10.1486731377353));
#109481=CARTESIAN_POINT('Ctrl Pts',(-8.83407653965581,5.49101324515329,
10.1144343054655));
#109482=CARTESIAN_POINT('Ctrl Pts',(-8.86000864186209,5.49330933861771,
10.0812979025415));
#109483=CARTESIAN_POINT('Ctrl Pts',(-8.88727102647093,5.49560543208213,
10.0493862606353));
#109484=CARTESIAN_POINT('Ctrl Pts',(-8.92301234464173,5.49861563857137,
10.007549709538));
#109485=CARTESIAN_POINT('Ctrl Pts',(-8.96119145638884,5.50162584506061,
9.96764382578134));
#109486=CARTESIAN_POINT('Ctrl Pts',(-9.00157178841649,5.50463605154986,
9.92996572189758));
#109487=CARTESIAN_POINT('Ctrl Pts',(-9.04188038724669,5.50764091059083,
9.89235455086778));
#109488=CARTESIAN_POINT('Ctrl Pts',(-9.08438206327088,5.5106457696318,9.85696366333679));
#109489=CARTESIAN_POINT('Ctrl Pts',(-9.12880143194597,5.51365062867278,
9.82405556890616));
#109490=CARTESIAN_POINT('Ctrl Pts',(-9.17317687810099,5.51665251646528,
9.79118001447963));
#109491=CARTESIAN_POINT('Ctrl Pts',(-9.21946583829074,5.51965440425778,
9.76078270267316));
#109492=CARTESIAN_POINT('Ctrl Pts',(-9.26735909218071,5.52265629205027,
9.73308660509499));
#109493=CARTESIAN_POINT('Ctrl Pts',(-9.31522390226739,5.52565639702162,
9.70540695622907));
#109494=CARTESIAN_POINT('Ctrl Pts',(-9.36469066131898,5.52865650199297,
9.68042560568449));
#109495=CARTESIAN_POINT('Ctrl Pts',(-9.41542228234622,5.53165660696432,
9.65832152062325));
#109496=CARTESIAN_POINT('Ctrl Pts',(-9.46614380733411,5.53465611488836,
9.6362218344696));
#109497=CARTESIAN_POINT('Ctrl Pts',(-9.5181292105367,5.5376556228124,9.61699848744594));
#109498=CARTESIAN_POINT('Ctrl Pts',(-9.57102009975651,5.54065513073644,
9.60078289919431));
#109499=CARTESIAN_POINT('Ctrl Pts',(-9.62395960186442,5.54365739555766,
9.58455240692823));
#109500=CARTESIAN_POINT('Ctrl Pts',(-9.6778057467329,5.54665966037887,9.5713353516049));
#109501=CARTESIAN_POINT('Ctrl Pts',(-9.73218503409507,5.54966192520009,
9.5612132214823));
#109502=CARTESIAN_POINT('Ctrl Pts',(-9.78658908836782,5.55266555739531,
9.55108648126082));
#109503=CARTESIAN_POINT('Ctrl Pts',(-9.84152624445177,5.55566918959054,
9.54405754326308));
#109504=CARTESIAN_POINT('Ctrl Pts',(-9.89661615056347,5.55867282178577,
9.54015616257228));
#109505=CARTESIAN_POINT('Ctrl Pts',(-9.95180994371746,5.56168211814866,
9.53624742476419));
#109506=CARTESIAN_POINT('Ctrl Pts',(-10.007156533005,5.56469141451155,9.53547803346949));
#109507=CARTESIAN_POINT('Ctrl Pts',(-10.0622750009097,5.56770071087444,
9.53782556640403));
#109508=CARTESIAN_POINT('Ctrl Pts',(-10.104330401098,5.56999680450037,9.53961673442394));
#109509=CARTESIAN_POINT('Ctrl Pts',(-10.1462529703101,5.5722928981263,9.54322139313254));
#109510=CARTESIAN_POINT('Ctrl Pts',(-10.1878769950017,5.57458899175222,
9.5486094651166));
#109511=CARTESIAN_POINT('Ctrl Pts',(-10.242446594371,5.57759919824257,9.55567329259896));
#109512=CARTESIAN_POINT('Ctrl Pts',(-10.2967318420896,5.58060940473292,
9.5658338050913));
#109513=CARTESIAN_POINT('Ctrl Pts',(-10.3503546283818,5.58361961122327,
9.57905528454784));
#109514=CARTESIAN_POINT('Ctrl Pts',(-10.4038821570629,5.58662447026528,
9.59225327685206));
#109515=CARTESIAN_POINT('Ctrl Pts',(-10.4567490511495,5.58962932930729,
9.60850131970296));
#109516=CARTESIAN_POINT('Ctrl Pts',(-10.5085849649228,5.5926341883493,9.62771228109608));
#109517=CARTESIAN_POINT('Ctrl Pts',(-10.5603696225872,5.59563607614279,
9.64690424640994));
#109518=CARTESIAN_POINT('Ctrl Pts',(-10.6111248266843,5.59863796393629,
9.66905314388547));
#109519=CARTESIAN_POINT('Ctrl Pts',(-10.6604948476701,5.60163985172978,
9.69402189673743));
#109520=CARTESIAN_POINT('Ctrl Pts',(-10.7098355477998,5.60463995670208,
9.7189758206468));
#109521=CARTESIAN_POINT('Ctrl Pts',(-10.757792225087,5.60764006167438,9.74674604267606));
#109522=CARTESIAN_POINT('Ctrl Pts',(-10.8040307689732,5.61064016664668,
9.77714809868718));
#109523=CARTESIAN_POINT('Ctrl Pts',(-10.8502601109811,5.61363967457162,
9.80754410442088));
#109524=CARTESIAN_POINT('Ctrl Pts',(-10.8947715576388,5.61663918249656,
9.84057061400552));
#109525=CARTESIAN_POINT('Ctrl Pts',(-10.9372591706691,5.61963869042149,
9.87599933407643));
#109526=CARTESIAN_POINT('Ctrl Pts',(-10.9797858347639,5.62264095524354,
9.91146061726712));
#109527=CARTESIAN_POINT('Ctrl Pts',(-11.0202845424836,5.62564322006558,
9.94932818312116));
#109528=CARTESIAN_POINT('Ctrl Pts',(-11.0584829112703,5.62864548488763,
9.98933379568286));
#109529=CARTESIAN_POINT('Ctrl Pts',(-11.0966986774081,5.63164911708365,
10.0293576287004));
#109530=CARTESIAN_POINT('Ctrl Pts',(-11.1326116731147,5.63465274927966,
10.0715210468442));
#109531=CARTESIAN_POINT('Ctrl Pts',(-11.1659890931607,5.63765638147568,
10.1155218009299));
#109532=CARTESIAN_POINT('Ctrl Pts',(-11.1994294554341,5.64066567783928,
10.1596055304363));
#109533=CARTESIAN_POINT('Ctrl Pts',(-11.2303243947869,5.64367497420289,
10.2055330780896));
#109534=CARTESIAN_POINT('Ctrl Pts',(-11.258484490896,5.64668427056649,10.2529732025059));
#109535=CARTESIAN_POINT('Ctrl Pts',(-11.2799706488423,5.64898036418509,
10.2891700252103));
#109536=CARTESIAN_POINT('Ctrl Pts',(-11.2998655611633,5.6512764578037,10.3262468080652));
#109537=CARTESIAN_POINT('Ctrl Pts',(-11.3181038415257,5.65357255142231,
10.3640483407089));
#109538=CARTESIAN_POINT('Ctrl Pts',(-11.343785672609,5.6568057448645,10.4172777327763));
#109539=CARTESIAN_POINT('Ctrl Pts',(-11.3662764748868,5.66003893830669,
10.4721417934287));
#109540=CARTESIAN_POINT('Ctrl Pts',(-11.3853830805078,5.66327213174888,
10.5282522175539));
#109541=CARTESIAN_POINT('Ctrl Pts',(-11.4044415639912,5.66649718202937,
10.5842213212585));
#109542=CARTESIAN_POINT('Ctrl Pts',(-11.4201326703982,5.66972223230985,
10.6414301682071));
#109543=CARTESIAN_POINT('Ctrl Pts',(-11.4323106215473,5.67294728259033,
10.6994695799044));
#109544=CARTESIAN_POINT('Ctrl Pts',(-11.4444430750598,5.67616028386819,
10.7572921524944));
#109545=CARTESIAN_POINT('Ctrl Pts',(-11.4530884204079,5.67937328514605,
10.8159387204676));
#109546=CARTESIAN_POINT('Ctrl Pts',(-11.4581508364159,5.68258628642391,
10.8749864476965));
#109547=CARTESIAN_POINT('Ctrl Pts',(-11.4617003573309,5.68483908730347,
10.9163878541492));
#109548=CARTESIAN_POINT('Ctrl Pts',(-11.4634894691637,5.68709188818304,
10.9579860868412));
#109549=CARTESIAN_POINT('Ctrl Pts',(-11.4634999536212,5.6893446890626,10.9996315564861));
#109550=CARTESIAN_POINT('Origin',(-10.,3.5,11.));
#109551=CARTESIAN_POINT('',(-11.4635,6.26064415683876,11.0000000000891));
#109552=CARTESIAN_POINT('',(-11.4635,6.189145110564,10.9999999999277));
#109553=CARTESIAN_POINT('',(-11.4635,3.5,11.));
#109554=CARTESIAN_POINT('Ctrl Pts',(-11.4635,6.26064415683876,11.0000000000891));
#109555=CARTESIAN_POINT('Ctrl Pts',(-11.463500000006,6.25468158645031,10.9008697580982));
#109556=CARTESIAN_POINT('Ctrl Pts',(-11.4534281618735,6.24879590921732,
10.8019773468397));
#109557=CARTESIAN_POINT('Ctrl Pts',(-11.430651981289,6.24244638816578,10.6913631549977));
#109558=CARTESIAN_POINT('Ctrl Pts',(-11.4276852120321,6.24167813351364,
10.6779181051389));
#109559=CARTESIAN_POINT('Ctrl Pts',(-11.4218987475142,6.2402804437222,10.6533476290882));
#109560=CARTESIAN_POINT('Ctrl Pts',(-11.4191370896103,6.23964925057465,
10.6422097740023));
#109561=CARTESIAN_POINT('Ctrl Pts',(-11.4145308461038,6.23865067548806,
10.6245256809034));
#109562=CARTESIAN_POINT('Ctrl Pts',(-11.4127711709199,6.23828060963525,
10.617957987041));
#109563=CARTESIAN_POINT('Ctrl Pts',(-11.4093597359101,6.23758410218281,
10.6055713383786));
#109564=CARTESIAN_POINT('Ctrl Pts',(-11.4077175513289,6.23725736278335,
10.5997499137986));
#109565=CARTESIAN_POINT('Ctrl Pts',(-11.4039194350033,6.23652050575121,
10.5865984466453));
#109566=CARTESIAN_POINT('Ctrl Pts',(-11.4017420881184,6.23611108503517,
10.57927473847));
#109567=CARTESIAN_POINT('Ctrl Pts',(-11.3959785985095,6.2350597932708,10.5604302297379));
#109568=CARTESIAN_POINT('Ctrl Pts',(-11.3923071187277,6.23442067481777,
10.5489360034574));
#109569=CARTESIAN_POINT('Ctrl Pts',(-11.3626723958532,6.22948775571548,
10.4599704120041));
#109570=CARTESIAN_POINT('Ctrl Pts',(-11.3304038902835,6.22541035961006,
10.3847475118716));
#109571=CARTESIAN_POINT('Ctrl Pts',(-11.2877604284509,6.22096502876809,
10.3045953515623));
#109572=CARTESIAN_POINT('Ctrl Pts',(-11.2834251126999,6.22052175378133,
10.2966263243695));
#109573=CARTESIAN_POINT('Ctrl Pts',(-11.2389352487734,6.21605502547736,
10.2166275988383));
#109574=CARTESIAN_POINT('Ctrl Pts',(-11.1928373310914,6.21209729880708,
10.148078462951));
#109575=CARTESIAN_POINT('Ctrl Pts',(-11.1206139507306,6.20625438657933,
10.0581191218579));
#109576=CARTESIAN_POINT('Ctrl Pts',(-11.0991534708841,6.2045534982045,10.0331615667196));
#109577=CARTESIAN_POINT('Ctrl Pts',(-11.072163524223,6.20242633165054,10.0038343672439));
#109578=CARTESIAN_POINT('Ctrl Pts',(-11.06741897992,6.20205282048312,9.99875212456149));
#109579=CARTESIAN_POINT('Ctrl Pts',(-11.0598922158294,6.20146057824844,
9.99080393721421));
#109580=CARTESIAN_POINT('Ctrl Pts',(-11.0571341080158,6.20124361882877,
9.98791518180678));
#109581=CARTESIAN_POINT('Ctrl Pts',(-11.0520189543992,6.20084128168649,
9.9826014518897));
#109582=CARTESIAN_POINT('Ctrl Pts',(-11.0496652999348,6.20065615887383,
9.98017332670547));
#109583=CARTESIAN_POINT('Ctrl Pts',(-11.0442992224879,6.20023412125252,
9.97467571956473));
#109584=CARTESIAN_POINT('Ctrl Pts',(-11.0412816850758,6.19999681772598,
9.97161135872589));
#109585=CARTESIAN_POINT('Ctrl Pts',(-11.0333978981535,6.19937699611587,
9.96367551124866));
#109586=CARTESIAN_POINT('Ctrl Pts',(-11.0285107528044,6.19899293758773,
9.95882504374669));
#109587=CARTESIAN_POINT('Ctrl Pts',(-10.9951073239107,6.19637021401389,
9.92613698475134));
#109588=CARTESIAN_POINT('Ctrl Pts',(-10.9655006423753,6.1940572193856,9.89944180101318));
#109589=CARTESIAN_POINT('Ctrl Pts',(-10.8521258426725,6.18535631354391,
9.8053149155226));
#109590=CARTESIAN_POINT('Ctrl Pts',(-10.762090541751,6.17877269448143,9.74596194987916));
#109591=CARTESIAN_POINT('Ctrl Pts',(-10.6310102219934,6.17012074557002,
9.67892666276233));
#109592=CARTESIAN_POINT('Ctrl Pts',(-10.5949376411045,6.16782328053937,
9.66229366129145));
#109593=CARTESIAN_POINT('Ctrl Pts',(-10.534233528875,6.16410014637168,9.63724517479193));
#109594=CARTESIAN_POINT('Ctrl Pts',(-10.5099759310201,6.16264854528252,
9.62798292757365));
#109595=CARTESIAN_POINT('Ctrl Pts',(-10.4766603218739,6.16070272563627,
9.61626784941353));
#109596=CARTESIAN_POINT('Ctrl Pts',(-10.4678073367868,6.1601901657414,9.61324983204027));
#109597=CARTESIAN_POINT('Ctrl Pts',(-10.4529056764005,6.15933480694297,
9.60832874079627));
#109598=CARTESIAN_POINT('Ctrl Pts',(-10.4468725517433,6.15899052367183,
9.60637976131909));
#109599=CARTESIAN_POINT('Ctrl Pts',(-10.4349518180935,6.15831417285298,
9.60261418122248));
#109600=CARTESIAN_POINT('Ctrl Pts',(-10.4290650293143,6.1579820416617,9.6007954356872));
#109601=CARTESIAN_POINT('Ctrl Pts',(-10.4160851123234,6.1572537500392,9.59687486087051));
#109602=CARTESIAN_POINT('Ctrl Pts',(-10.4089871544659,6.15685812645046,
9.59478952219154));
#109603=CARTESIAN_POINT('Ctrl Pts',(-10.3839773469203,6.15547314938425,
9.58764733777428));
#109604=CARTESIAN_POINT('Ctrl Pts',(-10.3659847389951,6.15449298071503,
9.58287831954562));
#109605=CARTESIAN_POINT('Ctrl Pts',(-10.2558684471843,6.14858425230046,
9.55592874864663));
#109606=CARTESIAN_POINT('Ctrl Pts',(-10.1618595433146,6.14394035810551,
9.54239434931393));
#109607=CARTESIAN_POINT('Ctrl Pts',(-9.97470908243032,6.13482118376619,
9.53379259654499));
#109608=CARTESIAN_POINT('Ctrl Pts',(-9.88203954894,6.13035863826809,9.53832789996629));
#109609=CARTESIAN_POINT('Ctrl Pts',(-9.77616284332801,6.1247583683835,9.55364698991818));
#109610=CARTESIAN_POINT('Ctrl Pts',(-9.76192614438314,6.12399444596427,
9.55592212437193));
#109611=CARTESIAN_POINT('Ctrl Pts',(-9.74257976371953,6.12293870615667,
9.55930767827695));
#109612=CARTESIAN_POINT('Ctrl Pts',(-9.7374385466064,6.12265644299577,9.560235774357));
#109613=CARTESIAN_POINT('Ctrl Pts',(-9.72883492021662,6.122181064772,9.5618365218929));
#109614=CARTESIAN_POINT('Ctrl Pts',(-9.72536972433999,6.12198877831556,
9.56249420816729));
#109615=CARTESIAN_POINT('Ctrl Pts',(-9.71880265285195,6.12162274769433,
9.56376523516815));
#109616=CARTESIAN_POINT('Ctrl Pts',(-9.71570032486233,6.12144914751057,
9.56437611399104));
#109617=CARTESIAN_POINT('Ctrl Pts',(-9.70836612330892,6.12103715891014,
9.5658449954833));
#109618=CARTESIAN_POINT('Ctrl Pts',(-9.70413604307504,6.12079829274913,
9.56671167832684));
#109619=CARTESIAN_POINT('Ctrl Pts',(-9.68937994587993,6.11996082956113,
9.56980309787453));
#109620=CARTESIAN_POINT('Ctrl Pts',(-9.67887493033025,6.11935714154363,
9.57212512005518));
#109621=CARTESIAN_POINT('Ctrl Pts',(-9.566922276486,6.11285036928516,9.59816895866746));
#109622=CARTESIAN_POINT('Ctrl Pts',(-9.46826517280139,6.10649452775306,
9.63254167021684));
#109623=CARTESIAN_POINT('Ctrl Pts',(-9.31539704671918,6.09635222401178,
9.70486739555222));
#109624=CARTESIAN_POINT('Ctrl Pts',(-9.25860345323244,6.09250533866046,
9.73651980365157));
#109625=CARTESIAN_POINT('Ctrl Pts',(-9.17368509345593,6.08669432250208,
9.79155093279611));
#109626=CARTESIAN_POINT('Ctrl Pts',(-9.14401494811772,6.08465063039165,
9.81238247479895));
#109627=CARTESIAN_POINT('Ctrl Pts',(-9.10675271694636,6.08206567258003,
9.84066717386384));
#109628=CARTESIAN_POINT('Ctrl Pts',(-9.09842751197536,6.08148686470424,
9.84712950970302));
#109629=CARTESIAN_POINT('Ctrl Pts',(-9.08500778697391,6.08055160584312,
9.85778067741105));
#109630=CARTESIAN_POINT('Ctrl Pts',(-9.07987060044323,6.08019303202526,
9.86191493251127));
#109631=CARTESIAN_POINT('Ctrl Pts',(-9.07003654436081,6.07950549071964,
9.8699392006974));
#109632=CARTESIAN_POINT('Ctrl Pts',(-9.06533571250799,6.07917633140616,
9.87382412111696));
#109633=CARTESIAN_POINT('Ctrl Pts',(-9.05460067019202,6.0784234117105,9.88280942565999));
#109634=CARTESIAN_POINT('Ctrl Pts',(-9.04858317536251,6.07800045697459,
9.88792954301572));
#109635=CARTESIAN_POINT('Ctrl Pts',(-9.0295064064749,6.07665642146172,9.90442961403695));
#109636=CARTESIAN_POINT('Ctrl Pts',(-9.01660732180629,6.07574283202611,
9.91599300769827));
#109637=CARTESIAN_POINT('Ctrl Pts',(-8.89865904575401,6.06733379481988,
10.0255663205996));
#109638=CARTESIAN_POINT('Ctrl Pts',(-8.80838211625585,6.06058130811177,
10.1383047984967));
#109639=CARTESIAN_POINT('Ctrl Pts',(-8.70810989499425,6.05074622164784,
10.3101386046344));
#109640=CARTESIAN_POINT('Ctrl Pts',(-8.68297629057774,6.04795677449364,
10.3594251658984));
#109641=CARTESIAN_POINT('Ctrl Pts',(-8.65755062505719,6.04459797572021,
10.41714265703));
#109642=CARTESIAN_POINT('Ctrl Pts',(-8.65446542243667,6.04417984271746,
10.4243006845394));
#109643=CARTESIAN_POINT('Ctrl Pts',(-8.64985034858313,6.04353746870808,
10.4352479621997));
#109644=CARTESIAN_POINT('Ctrl Pts',(-8.64827887770282,6.04331563025753,
10.4390196508486));
#109645=CARTESIAN_POINT('Ctrl Pts',(-8.64543769417484,6.04290873903866,
10.4459200324381));
#109646=CARTESIAN_POINT('Ctrl Pts',(-8.64416299569114,6.04272398547366,
10.449046582715));
#109647=CARTESIAN_POINT('Ctrl Pts',(-8.64133047038344,6.04230846503045,
10.4560634957915));
#109648=CARTESIAN_POINT('Ctrl Pts',(-8.63977853956789,6.04207736100753,
10.4599561230735));
#109649=CARTESIAN_POINT('Ctrl Pts',(-8.63529592710011,6.0413997952144,10.4713415333798));
#109650=CARTESIAN_POINT('Ctrl Pts',(-8.63241033577073,6.04095080983986,
10.4788517626643));
#109651=CARTESIAN_POINT('Ctrl Pts',(-8.61000061901428,6.03736224893733,
10.5386447660254));
#109652=CARTESIAN_POINT('Ctrl Pts',(-8.5934214887583,6.03407862599628,10.5919771717417));
#109653=CARTESIAN_POINT('Ctrl Pts',(-8.55994771052658,6.02581151713361,
10.7263027446489));
#109654=CARTESIAN_POINT('Ctrl Pts',(-8.54679227229088,6.02079153274629,
10.8080386513347));
#109655=CARTESIAN_POINT('Ctrl Pts',(-8.53599821490542,6.01226981040269,
10.9518317012995));
#109656=CARTESIAN_POINT('Ctrl Pts',(-8.53526726654161,6.00871318162902,
11.0134498120937));
#109657=CARTESIAN_POINT('Ctrl Pts',(-8.53924543824087,6.00437330895556,
11.0910404204562));
#109658=CARTESIAN_POINT('Ctrl Pts',(-8.54033717277281,6.00348070107881,
11.1071293971752));
#109659=CARTESIAN_POINT('Ctrl Pts',(-8.54234799401081,6.00217056282188,
11.1309317566409));
#109660=CARTESIAN_POINT('Ctrl Pts',(-8.54306290932061,6.00174676488769,
11.1386607821215));
#109661=CARTESIAN_POINT('Ctrl Pts',(-8.54444560600152,6.0009953896149,11.1524152259739));
#109662=CARTESIAN_POINT('Ctrl Pts',(-8.54508939561608,6.0006670770928,11.1584428280959));
#109663=CARTESIAN_POINT('Ctrl Pts',(-8.54652677103316,5.99997678764282,
11.171152260392));
#109664=CARTESIAN_POINT('Ctrl Pts',(-8.54732902675747,5.99961508791348,
11.1778329809677));
#109665=CARTESIAN_POINT('Ctrl Pts',(-8.54958334753883,5.99865765595457,
11.1955713654895));
#109666=CARTESIAN_POINT('Ctrl Pts',(-8.55111579628466,5.99806442932944,
11.2066184843933));
#109667=CARTESIAN_POINT('Ctrl Pts',(-8.55846922427464,5.99545112532016,
11.2555144430481));
#109668=CARTESIAN_POINT('Ctrl Pts',(-8.5656483167018,5.99347343793423,11.2931453164796));
#109669=CARTESIAN_POINT('Ctrl Pts',(-8.60632568254466,5.98433942074173,
11.4686432156434));
#109670=CARTESIAN_POINT('Ctrl Pts',(-8.65827055332199,5.97776955788723,
11.6014231125141));
#109671=CARTESIAN_POINT('Ctrl Pts',(-8.73869416933328,5.9695144334023,11.7425389020239));
#109672=CARTESIAN_POINT('Ctrl Pts',(-8.74926803588948,5.9684535859667,11.7602143792621));
#109673=CARTESIAN_POINT('Ctrl Pts',(-8.76743067278315,5.9666608832001,11.7891702689197));
#109674=CARTESIAN_POINT('Ctrl Pts',(-8.77481014694678,5.96593998170809,
11.8005789515333));
#109675=CARTESIAN_POINT('Ctrl Pts',(-8.78517942399309,5.96493471021708,
11.8161306784213));
#109676=CARTESIAN_POINT('Ctrl Pts',(-8.78803388935176,5.9646587521615,11.8203636152517));
#109677=CARTESIAN_POINT('Ctrl Pts',(-8.79288401360932,5.96419100340557,
11.8274753865341));
#109678=CARTESIAN_POINT('Ctrl Pts',(-8.79486799567978,5.96399998301618,
11.8303621931434));
#109679=CARTESIAN_POINT('Ctrl Pts',(-8.79867515680284,5.96363396998255,
11.8358594435637));
#109680=CARTESIAN_POINT('Ctrl Pts',(-8.800496520631,5.96345910523305,11.8384711031749));
#109681=CARTESIAN_POINT('Ctrl Pts',(-8.80485795815687,5.96304097903037,
11.8446816880644));
#109682=CARTESIAN_POINT('Ctrl Pts',(-8.80740577152801,5.96279720649603,
11.8482751083982));
#109683=CARTESIAN_POINT('Ctrl Pts',(-8.81653132384033,5.96192595345758,
11.861023356524));
#109684=CARTESIAN_POINT('Ctrl Pts',(-8.82319840302699,5.96129284472315,
11.8701133912286));
#109685=CARTESIAN_POINT('Ctrl Pts',(-8.88932645771598,5.95505351759766,
11.9581234177758));
#109686=CARTESIAN_POINT('Ctrl Pts',(-8.95652719445512,5.94904269562805,
12.0309016967563));
#109687=CARTESIAN_POINT('Ctrl Pts',(-9.08164779529878,5.93901307299818,
12.141540878415));
#109688=CARTESIAN_POINT('Ctrl Pts',(-9.13585535488944,5.9349614775753,12.1831068988301));
#109689=CARTESIAN_POINT('Ctrl Pts',(-9.21341639038986,5.92961487194081,
12.2343950599313));
#109690=CARTESIAN_POINT('Ctrl Pts',(-9.23440694465341,5.92820866170775,
12.2475224700076));
#109691=CARTESIAN_POINT('Ctrl Pts',(-9.2714095297554,5.92579973020932,12.2693778632288));
#109692=CARTESIAN_POINT('Ctrl Pts',(-9.28726990844085,5.92478866802482,
12.2783505354414));
#109693=CARTESIAN_POINT('Ctrl Pts',(-9.31046095609257,5.92334051850038,
12.2909045549492));
#109694=CARTESIAN_POINT('Ctrl Pts',(-9.31766006318078,5.92289510484147,
12.2947242476409));
#109695=CARTESIAN_POINT('Ctrl Pts',(-9.33031655222631,5.9221191369893,12.3013046247338));
#109696=CARTESIAN_POINT('Ctrl Pts',(-9.33575998453134,5.92178767369947,
12.3040915803712));
#109697=CARTESIAN_POINT('Ctrl Pts',(-9.34706727987358,5.92110377654723,
12.3097915790624));
#109698=CARTESIAN_POINT('Ctrl Pts',(-9.35293355154243,5.92075152307699,
12.3126995584584));
#109699=CARTESIAN_POINT('Ctrl Pts',(-9.36810030600404,5.91984725550665,
12.3200915221431));
#109700=CARTESIAN_POINT('Ctrl Pts',(-9.37742916571599,5.9192972626419,12.3245166717272));
#109701=CARTESIAN_POINT('Ctrl Pts',(-9.41494620054885,5.9171093455325,12.3418289427692));
#109702=CARTESIAN_POINT('Ctrl Pts',(-9.44349472361689,5.91549831552876,
12.3539183558332));
#109703=CARTESIAN_POINT('Ctrl Pts',(-9.60328906756971,5.90673391503435,
12.4156770729975));
#109704=CARTESIAN_POINT('Ctrl Pts',(-9.7407494839937,5.90020171935599,12.4471716880945));
#109705=CARTESIAN_POINT('Ctrl Pts',(-9.92083274204873,5.89113470822527,
12.4619150778616));
#109706=CARTESIAN_POINT('Ctrl Pts',(-9.96119843300378,5.88906389013771,
12.4635426379631));
#109707=CARTESIAN_POINT('Ctrl Pts',(-10.0088699210632,5.88652104768634,
12.4634912958913));
#109708=CARTESIAN_POINT('Ctrl Pts',(-10.0161633469098,5.88612931754385,
12.4634289154214));
#109709=CARTESIAN_POINT('Ctrl Pts',(-10.0274352523485,5.88551933255902,
12.4632482347966));
#109710=CARTESIAN_POINT('Ctrl Pts',(-10.0314143293995,5.88530312212138,
12.4631682161845));
#109711=CARTESIAN_POINT('Ctrl Pts',(-10.0387750524838,5.88490145469829,
12.4629901538958));
#109712=CARTESIAN_POINT('Ctrl Pts',(-10.0421567257087,5.88471624569875,
12.4628966145593));
#109713=CARTESIAN_POINT('Ctrl Pts',(-10.0498554038322,5.88429307570149,
12.4626569475945));
#109714=CARTESIAN_POINT('Ctrl Pts',(-10.054172088726,5.88405471726738,12.4625034329757));
#109715=CARTESIAN_POINT('Ctrl Pts',(-10.0654304041672,5.88343033789776,
12.4620531408435));
#109716=CARTESIAN_POINT('Ctrl Pts',(-10.0723706325022,5.88304274020497,
12.4617260386823));
#109717=CARTESIAN_POINT('Ctrl Pts',(-10.1205870278084,5.88033243510874,
12.4591093121567));
#109718=CARTESIAN_POINT('Ctrl Pts',(-10.1617491875743,5.87792979837102,
12.4551212468549));
#109719=CARTESIAN_POINT('Ctrl Pts',(-10.2406297538487,5.87322061327362,
12.4440905928907));
#109720=CARTESIAN_POINT('Ctrl Pts',(-10.2783518497674,5.87092160476448,
12.4372962118317));
#109721=CARTESIAN_POINT('Ctrl Pts',(-10.3747225849288,5.86498482981741,
12.416001848089));
#109722=CARTESIAN_POINT('Ctrl Pts',(-10.4328222622625,5.8613463099866,12.3993368872924));
#109723=CARTESIAN_POINT('Ctrl Pts',(-10.5313648372406,5.85517014089614,
12.3643444926323));
#109724=CARTESIAN_POINT('Ctrl Pts',(-10.5723132439562,5.85260135211813,
12.3476804323186));
#109725=CARTESIAN_POINT('Ctrl Pts',(-10.6294833023553,5.84902275284938,
12.321338280286));
#109726=CARTESIAN_POINT('Ctrl Pts',(-10.6463670062081,5.84796675597217,
12.313161763469));
#109727=CARTESIAN_POINT('Ctrl Pts',(-10.6761683010796,5.84610417196677,
12.2980153782613));
#109728=CARTESIAN_POINT('Ctrl Pts',(-10.6891468032443,5.84529347300159,
12.2911716381169));
#109729=CARTESIAN_POINT('Ctrl Pts',(-10.7085798662642,5.8440799448123,12.280547815017));
#109730=CARTESIAN_POINT('Ctrl Pts',(-10.7151117002444,5.84367211290044,
12.2769116619723));
#109731=CARTESIAN_POINT('Ctrl Pts',(-10.7268650342372,5.84293828681873,
12.2702503225802));
#109732=CARTESIAN_POINT('Ctrl Pts',(-10.7320961980485,5.84261168450075,
12.2672426043656));
#109733=CARTESIAN_POINT('Ctrl Pts',(-10.7432766352881,5.8419136009126,12.2607219459371));
#109734=CARTESIAN_POINT('Ctrl Pts',(-10.7492199515903,5.84154248526698,
12.257199048639));
#109735=CARTESIAN_POINT('Ctrl Pts',(-10.7651357047218,5.84054845522319,
12.247612047021));
#109736=CARTESIAN_POINT('Ctrl Pts',(-10.7750610277711,5.83992834111113,
12.2414704507844));
#109737=CARTESIAN_POINT('Ctrl Pts',(-10.8233422285407,5.8369092937055,12.2107902633161));
#109738=CARTESIAN_POINT('Ctrl Pts',(-10.8606137851685,5.83457183224753,
12.1845884995604));
#109739=CARTESIAN_POINT('Ctrl Pts',(-10.9841403881607,5.82671034511541,
12.0888371165977));
#109740=CARTESIAN_POINT('Ctrl Pts',(-11.0636853820692,5.82146967821963,
12.0112718929093));
#109741=CARTESIAN_POINT('Ctrl Pts',(-11.1664350503357,5.81341266616767,
11.8854027033054));
#109742=CARTESIAN_POINT('Ctrl Pts',(-11.1969993297778,5.81079252232597,
11.8436232877529));
#109743=CARTESIAN_POINT('Ctrl Pts',(-11.229495568897,5.80762691933193,11.7938716426076));
#109744=CARTESIAN_POINT('Ctrl Pts',(-11.2336552585333,5.80721377624935,
11.7873920477452));
#109745=CARTESIAN_POINT('Ctrl Pts',(-11.2399331126891,5.80657751500617,
11.7774410972377));
#109746=CARTESIAN_POINT('Ctrl Pts',(-11.2420883239202,5.80635672971682,
11.7739931384626));
#109747=CARTESIAN_POINT('Ctrl Pts',(-11.246007202858,5.80595084731565,11.7676650999878));
#109748=CARTESIAN_POINT('Ctrl Pts',(-11.247775295103,5.80576603995084,11.7647878579543));
#109749=CARTESIAN_POINT('Ctrl Pts',(-11.2517266142452,5.80534922840342,
11.7583076425111));
#109750=CARTESIAN_POINT('Ctrl Pts',(-11.2539042362142,5.80511687664165,
11.7547013733906));
#109751=CARTESIAN_POINT('Ctrl Pts',(-11.2602480636208,5.8044323027948,11.7440923758801));
#109752=CARTESIAN_POINT('Ctrl Pts',(-11.2643713227785,5.80397748014325,
11.7370643104111));
#109753=CARTESIAN_POINT('Ctrl Pts',(-11.3023823204292,5.79969363571814,
11.6710172597385));
#109754=CARTESIAN_POINT('Ctrl Pts',(-11.3321701018699,5.79565151853014,
11.6097416293405));
#109755=CARTESIAN_POINT('Ctrl Pts',(-11.3927064663139,5.78592380186845,
11.4593945914242));
#109756=CARTESIAN_POINT('Ctrl Pts',(-11.4193433606829,5.7802339626094,11.368974493906));
#109757=CARTESIAN_POINT('Ctrl Pts',(-11.4457820611401,5.77211814078187,
11.2316175052003));
#109758=CARTESIAN_POINT('Ctrl Pts',(-11.4523261255213,5.76951522049873,
11.1862307808025));
#109759=CARTESIAN_POINT('Ctrl Pts',(-11.457821008752,5.76634923678101,11.1293025905695));
#109760=CARTESIAN_POINT('Ctrl Pts',(-11.4587806178301,5.7657245705065,11.1179846290805));
#109761=CARTESIAN_POINT('Ctrl Pts',(-11.4601020403181,5.76473387787134,
11.0999007720322));
#109762=CARTESIAN_POINT('Ctrl Pts',(-11.4605487862389,5.76436524029729,
11.093141706839));
#109763=CARTESIAN_POINT('Ctrl Pts',(-11.4613058529663,5.76366994150187,
11.0803373612867));
#109764=CARTESIAN_POINT('Ctrl Pts',(-11.4616256254357,5.76334299511159,
11.07429279989));
#109765=CARTESIAN_POINT('Ctrl Pts',(-11.4622661527338,5.76260369142407,
11.060572041164));
#109766=CARTESIAN_POINT('Ctrl Pts',(-11.4625639829453,5.7621920498984,11.0528949188275));
#109767=CARTESIAN_POINT('Ctrl Pts',(-11.463270694087,5.76097192828551,11.0300316685418));
#109768=CARTESIAN_POINT('Ctrl Pts',(-11.4635036032574,5.76016886599224,
11.0148408779313));
#109769=CARTESIAN_POINT('Ctrl Pts',(-11.4634999578674,5.75937264475447,
10.9996488276474));
#109770=CARTESIAN_POINT('Ctrl Pts',(-11.4634999336402,5.69064613435915,
10.9995592789452));
#109771=CARTESIAN_POINT('Ctrl Pts',(-11.4635018158397,5.69099324829457,
11.0058094882762));
#109772=CARTESIAN_POINT('Ctrl Pts',(-11.4634636586465,5.69133914072625,
11.0120597265349));
#109773=CARTESIAN_POINT('Ctrl Pts',(-11.4633069419806,5.69202989168994,
11.0245852180884));
#109774=CARTESIAN_POINT('Ctrl Pts',(-11.4631880541147,5.69237473197048,
11.0308603209495));
#109775=CARTESIAN_POINT('Ctrl Pts',(-11.4628785535384,5.69304250044161,
11.0430540448561));
#109776=CARTESIAN_POINT('Ctrl Pts',(-11.4626923785698,5.69336555901081,
11.0489726483889));
#109777=CARTESIAN_POINT('Ctrl Pts',(-11.4622520981427,5.69400379743485,
11.060703324342));
#109778=CARTESIAN_POINT('Ctrl Pts',(-11.4619992489765,5.69431901010776,
11.0665153324534));
#109779=CARTESIAN_POINT('Ctrl Pts',(-11.4614260227125,5.69494536437348,
11.078100303415));
#109780=CARTESIAN_POINT('Ctrl Pts',(-11.4611060769315,5.69525651342251,
11.0838731811664));
#109781=CARTESIAN_POINT('Ctrl Pts',(-11.4601549556133,5.69608933733519,
11.099371722434));
#109782=CARTESIAN_POINT('Ctrl Pts',(-11.4594608206098,5.69660906162184,
11.1090933218267));
#109783=CARTESIAN_POINT('Ctrl Pts',(-11.4565053105407,5.69853958675306,
11.1453798823484));
#109784=CARTESIAN_POINT('Ctrl Pts',(-11.453615233189,5.69993101215188,11.1718892054966));
#109785=CARTESIAN_POINT('Ctrl Pts',(-11.4318802298353,5.70818535003896,
11.3308144042948));
#109786=CARTESIAN_POINT('Ctrl Pts',(-11.3956831478777,5.71446881975616,
11.4602022255253));
#109787=CARTESIAN_POINT('Ctrl Pts',(-11.3217986098834,5.72366742386944,
11.6303661184226));
#109788=CARTESIAN_POINT('Ctrl Pts',(-11.2986736785502,5.72628956170694,
11.6767264265003));
#109789=CARTESIAN_POINT('Ctrl Pts',(-11.2693452632507,5.72945751305295,
11.7284601454959));
#109790=CARTESIAN_POINT('Ctrl Pts',(-11.2654937575343,5.72987079994713,
11.7351306859564));
#109791=CARTESIAN_POINT('Ctrl Pts',(-11.2595283040555,5.73050727438153,
11.7452766232226));
#109792=CARTESIAN_POINT('Ctrl Pts',(-11.2574521663534,5.73072812735691,
11.7487742265598));
#109793=CARTESIAN_POINT('Ctrl Pts',(-11.2536250842806,5.73113413010189,
11.7551607841085));
#109794=CARTESIAN_POINT('Ctrl Pts',(-11.2518786940854,5.73131898991543,
11.7580523705641));
#109795=CARTESIAN_POINT('Ctrl Pts',(-11.2479312808657,5.73173591871051,
11.7645374585956));
#109796=CARTESIAN_POINT('Ctrl Pts',(-11.2457247556789,5.73196833545115,
11.7681274891187));
#109797=CARTESIAN_POINT('Ctrl Pts',(-11.2392049449242,5.73265310091989,
11.7786332813967));
#109798=CARTESIAN_POINT('Ctrl Pts',(-11.2348494244724,5.7331080515989,11.7855224854465));
#109799=CARTESIAN_POINT('Ctrl Pts',(-11.1944066929683,5.73730720135154,
11.8483238535662));
#109800=CARTESIAN_POINT('Ctrl Pts',(-11.1546059160706,5.74125525498306,
11.9017450485799));
#109801=CARTESIAN_POINT('Ctrl Pts',(-11.0719281981403,5.74887798584088,
11.9982314972652));
#109802=CARTESIAN_POINT('Ctrl Pts',(-11.029727482961,5.75253796344038,12.0417090925008));
#109803=CARTESIAN_POINT('Ctrl Pts',(-10.929084190016,5.76063360683702,12.1332876912415));
#109804=CARTESIAN_POINT('Ctrl Pts',(-10.8693553018973,5.76502107948247,
12.1797298247095));
#109805=CARTESIAN_POINT('Ctrl Pts',(-10.7978222489062,5.76979424140855,
12.2269535832448));
#109806=CARTESIAN_POINT('Ctrl Pts',(-10.7892867017011,5.77035668701215,
12.2324617422363));
#109807=CARTESIAN_POINT('Ctrl Pts',(-10.7748757565478,5.77129457251933,
12.2415502945528));
#109808=CARTESIAN_POINT('Ctrl Pts',(-10.7690313006929,5.77167175670782,
12.2451788758255));
#109809=CARTESIAN_POINT('Ctrl Pts',(-10.7575594193737,5.77240598825224,
12.2521897137076));
#109810=CARTESIAN_POINT('Ctrl Pts',(-10.7519343963433,5.7727631604787,12.2555755726135));
#109811=CARTESIAN_POINT('Ctrl Pts',(-10.7413107810232,5.77343246209394,
12.2618732252943));
#109812=CARTESIAN_POINT('Ctrl Pts',(-10.7363173543253,5.7737448900131,12.2647934478863));
#109813=CARTESIAN_POINT('Ctrl Pts',(-10.724682700833,5.7744678989753,12.2715052939605));
#109814=CARTESIAN_POINT('Ctrl Pts',(-10.718028774827,5.77487768168256,12.2752746413932));
#109815=CARTESIAN_POINT('Ctrl Pts',(-10.7007842929702,5.77593033981439,
12.2848656222116));
#109816=CARTESIAN_POINT('Ctrl Pts',(-10.6901505147949,5.77657045145195,
12.2906086048096));
#109817=CARTESIAN_POINT('Ctrl Pts',(-10.5968456511078,5.78211203073737,
12.3395167421728));
#109818=CARTESIAN_POINT('Ctrl Pts',(-10.5102926696713,5.78672444256759,
12.3748214091085));
#109819=CARTESIAN_POINT('Ctrl Pts',(-10.3569385672893,5.79453224801308,
12.4208784133698));
#109820=CARTESIAN_POINT('Ctrl Pts',(-10.2916781874053,5.79775525008546,
12.4356962729558));
#109821=CARTESIAN_POINT('Ctrl Pts',(-10.1808056222508,5.8033546033765,12.4529970134473));
#109822=CARTESIAN_POINT('Ctrl Pts',(-10.1356774862987,5.80566845286733,
12.4579032497131));
#109823=CARTESIAN_POINT('Ctrl Pts',(-10.0829175857108,5.80848625382296,
12.4611684044641));
#109824=CARTESIAN_POINT('Ctrl Pts',(-10.0754331290326,5.80888862218868,
12.4615739018387));
#109825=CARTESIAN_POINT('Ctrl Pts',(-10.0639267358958,5.80951170710604,
12.4621086868606));
#109826=CARTESIAN_POINT('Ctrl Pts',(-10.0599067206813,5.80973023837359,
12.4622789144981));
#109827=CARTESIAN_POINT('Ctrl Pts',(-10.0525080964303,5.81013406583393,
12.4625616490958));
#109828=CARTESIAN_POINT('Ctrl Pts',(-10.0491297563374,5.8103190931176,12.4626790297303));
#109829=CARTESIAN_POINT('Ctrl Pts',(-10.0414872913104,5.81073908625171,
12.4629180605544));
#109830=CARTESIAN_POINT('Ctrl Pts',(-10.0372230465051,5.81097442418408,
12.4630327717126));
#109831=CARTESIAN_POINT('Ctrl Pts',(-10.0261921950495,5.81158566939605,
12.4632812524953));
#109832=CARTESIAN_POINT('Ctrl Pts',(-10.0194251275474,5.81196304928457,
12.4633867280592));
#109833=CARTESIAN_POINT('Ctrl Pts',(-9.975121286419,5.81444838972668,12.4637699230797));
#109834=CARTESIAN_POINT('Ctrl Pts',(-9.93758910661046,5.81662239483701,
12.4626502560444));
#109835=CARTESIAN_POINT('Ctrl Pts',(-9.79685753361064,5.824933353312,12.4530256449793));
#109836=CARTESIAN_POINT('Ctrl Pts',(-9.69461059367506,5.83127028825392,
12.4350224212767));
#109837=CARTESIAN_POINT('Ctrl Pts',(-9.55303933856826,5.83996772701815,
12.3942652309968));
#109838=CARTESIAN_POINT('Ctrl Pts',(-9.51152576431471,5.84251227649355,
12.3802690998282));
#109839=CARTESIAN_POINT('Ctrl Pts',(-9.45331720404425,5.84606094950681,
12.3576883967957));
#109840=CARTESIAN_POINT('Ctrl Pts',(-9.43606486065199,5.84711040773884,
12.3506135882876));
#109841=CARTESIAN_POINT('Ctrl Pts',(-9.40554975264926,5.84896264112461,
12.337413317028));
#109842=CARTESIAN_POINT('Ctrl Pts',(-9.39223485454473,5.84976946276726,
12.3314154222908));
#109843=CARTESIAN_POINT('Ctrl Pts',(-9.37225389676864,5.85097846221475,
12.3220524853212));
#109844=CARTESIAN_POINT('Ctrl Pts',(-9.36552042417658,5.85138558545128,
12.318834187759));
#109845=CARTESIAN_POINT('Ctrl Pts',(-9.35343698450079,5.85211571632636,
12.3129448837118));
#109846=CARTESIAN_POINT('Ctrl Pts',(-9.34807824432272,5.85243934712233,
12.3102923439504));
#109847=CARTESIAN_POINT('Ctrl Pts',(-9.33656947070323,5.85313409928735,
12.3045074986618));
#109848=CARTESIAN_POINT('Ctrl Pts',(-9.33042501847381,5.85350483746499,
12.3013643715741));
#109849=CARTESIAN_POINT('Ctrl Pts',(-9.31398288559632,5.85449654487967,
12.2928062988305));
#109850=CARTESIAN_POINT('Ctrl Pts',(-9.30372704551955,5.85511473770878,
12.2873117690531));
#109851=CARTESIAN_POINT('Ctrl Pts',(-9.25396406184489,5.85811382584124,
12.2598827281003));
#109852=CARTESIAN_POINT('Ctrl Pts',(-9.21541998207495,5.86043423088415,
12.2362478748867));
#109853=CARTESIAN_POINT('Ctrl Pts',(-9.08612297010179,5.86829774753281,
12.1484772551841));
#109854=CARTESIAN_POINT('Ctrl Pts',(-9.001623964051,5.87355348532776,12.0758324169943));
#109855=CARTESIAN_POINT('Ctrl Pts',(-8.89095192632912,5.88163018933566,
11.9563103765689));
#109856=CARTESIAN_POINT('Ctrl Pts',(-8.85779427609208,5.88425424699069,
11.9164508822542));
#109857=CARTESIAN_POINT('Ctrl Pts',(-8.82221749491582,5.88742438522831,
11.8687462053216));
#109858=CARTESIAN_POINT('Ctrl Pts',(-8.8176608774552,5.88783773241379,11.8625345168288));
#109859=CARTESIAN_POINT('Ctrl Pts',(-8.81077364781177,5.8884742807303,11.8529885574001));
#109860=CARTESIAN_POINT('Ctrl Pts',(-8.80840747500743,5.88869514645983,
11.8496799687909));
#109861=CARTESIAN_POINT('Ctrl Pts',(-8.80410154027517,5.88910116134296,
11.8436056755123));
#109862=CARTESIAN_POINT('Ctrl Pts',(-8.80215753390207,5.88928602042566,
11.8408430814198));
#109863=CARTESIAN_POINT('Ctrl Pts',(-8.79781013540917,5.88970293323143,
11.8346193950126));
#109864=CARTESIAN_POINT('Ctrl Pts',(-8.79541213362944,5.88993533458507,
11.8311546645128));
#109865=CARTESIAN_POINT('Ctrl Pts',(-8.78842031618624,5.89062001342604,
11.8209587879242));
#109866=CARTESIAN_POINT('Ctrl Pts',(-8.78386779669529,5.89107489190595,
11.814199680439));
#109867=CARTESIAN_POINT('Ctrl Pts',(-8.74136185618165,5.8954061015063,11.7499394113873));
#109868=CARTESIAN_POINT('Ctrl Pts',(-8.70746051135611,5.89950074572649,
11.6898687455693));
#109869=CARTESIAN_POINT('Ctrl Pts',(-8.64271775038151,5.90856366704315,
11.5534927851825));
#109870=CARTESIAN_POINT('Ctrl Pts',(-8.61381439684384,5.91352833716397,
11.4765086927922));
#109871=CARTESIAN_POINT('Ctrl Pts',(-8.57638126639981,5.92159871598075,
11.3438714363327));
#109872=CARTESIAN_POINT('Ctrl Pts',(-8.56431938417028,5.92478572460804,
11.2894134848219));
#109873=CARTESIAN_POINT('Ctrl Pts',(-8.55346989003923,5.92854073272195,
11.2225465528112));
#109874=CARTESIAN_POINT('Ctrl Pts',(-8.55169324807884,5.92920155069513,
11.2106748478936));
#109875=CARTESIAN_POINT('Ctrl Pts',(-8.54912347875291,5.93023592720241,
11.1919307108425));
#109876=CARTESIAN_POINT('Ctrl Pts',(-8.5482327016119,5.930612509227,11.1850723947104));
#109877=CARTESIAN_POINT('Ctrl Pts',(-8.54665565670268,5.93131489230008,
11.1722175784007));
#109878=CARTESIAN_POINT('Ctrl Pts',(-8.5459578065378,5.93164104670507,11.1662226688449));
#109879=CARTESIAN_POINT('Ctrl Pts',(-8.54447915982048,5.93236835797635,
11.1527977277578));
#109880=CARTESIAN_POINT('Ctrl Pts',(-8.5437181283908,5.93276889393007,11.1453656597392));
#109881=CARTESIAN_POINT('Ctrl Pts',(-8.54192986516025,5.93378176512366,
11.126475553821));
#109882=CARTESIAN_POINT('Ctrl Pts',(-8.54098074943659,5.9343916828451,11.1150105222727));
#109883=CARTESIAN_POINT('Ctrl Pts',(-8.53583441652369,5.93822322226448,
11.0424479349112));
#109884=CARTESIAN_POINT('Ctrl Pts',(-8.5353402088393,5.94132829683979,10.9811456480205));
#109885=CARTESIAN_POINT('Ctrl Pts',(-8.54406865517426,5.94924500661307,
10.8217334865408));
#109886=CARTESIAN_POINT('Ctrl Pts',(-8.55934352295727,5.95391822225966,
10.724278014087));
#109887=CARTESIAN_POINT('Ctrl Pts',(-8.59231118522894,5.96039902178524,
10.5984422836911));
#109888=CARTESIAN_POINT('Ctrl Pts',(-8.60133521384235,5.96200145006498,
10.5680590306082));
#109889=CARTESIAN_POINT('Ctrl Pts',(-8.61718181856105,5.96460678829333,
10.5204284825906));
#109890=CARTESIAN_POINT('Ctrl Pts',(-8.62335845861017,5.96558176448198,
10.5029758888031));
#109891=CARTESIAN_POINT('Ctrl Pts',(-8.63188078677515,5.96688244083867,
10.4802741185329));
#109892=CARTESIAN_POINT('Ctrl Pts',(-8.63392893887717,5.96719192650651,
10.4749142667749));
#109893=CARTESIAN_POINT('Ctrl Pts',(-8.63732732554378,5.96770065815684,
10.4661754294132));
#109894=CARTESIAN_POINT('Ctrl Pts',(-8.63865875671988,5.96789881191781,
10.4627891395131));
#109895=CARTESIAN_POINT('Ctrl Pts',(-8.64127722998413,5.96828634130444,
10.4562017027723));
#109896=CARTESIAN_POINT('Ctrl Pts',(-8.64256298332213,5.96847564152219,
10.4530000925222));
#109897=CARTESIAN_POINT('Ctrl Pts',(-8.64574334924329,5.96894142945178,
10.4451610417707));
#109898=CARTESIAN_POINT('Ctrl Pts',(-8.64765046717005,5.96921864803859,
10.4405287449364));
#109899=CARTESIAN_POINT('Ctrl Pts',(-8.654218521303,5.97016612285981,10.4248050722618));
#109900=CARTESIAN_POINT('Ctrl Pts',(-8.65899230585262,5.97084260881341,
10.4137617049339));
#109901=CARTESIAN_POINT('Ctrl Pts',(-8.69459159750092,5.97579512373317,
10.3341192537659));
#109902=CARTESIAN_POINT('Ctrl Pts',(-8.73052596092311,5.98030537611432,
10.2679330302557));
#109903=CARTESIAN_POINT('Ctrl Pts',(-8.80650541858622,5.98871882464578,
10.1505405124206));
#109904=CARTESIAN_POINT('Ctrl Pts',(-8.84518686104693,5.99260982639114,
10.0986575633365));
#109905=CARTESIAN_POINT('Ctrl Pts',(-8.91316235232629,5.99876275002727,
10.019073192881));
#109906=CARTESIAN_POINT('Ctrl Pts',(-8.94038947346599,6.0010790137886,9.98972310901098));
#109907=CARTESIAN_POINT('Ctrl Pts',(-8.98731296814261,6.00482894172307,
9.94312779677988));
#109908=CARTESIAN_POINT('Ctrl Pts',(-9.00632849838731,6.00628901107473,
9.92522981637639));
#109909=CARTESIAN_POINT('Ctrl Pts',(-9.03280939964125,6.00824427520805,
9.90160914350378));
#109910=CARTESIAN_POINT('Ctrl Pts',(-9.03986510669321,6.00875803880145,
9.89543622935417));
#109911=CARTESIAN_POINT('Ctrl Pts',(-9.05179557554975,6.00961490930766,
9.88519917152931));
#109912=CARTESIAN_POINT('Ctrl Pts',(-9.0566382714208,6.00995951102347,9.88109823106945));
#109913=CARTESIAN_POINT('Ctrl Pts',(-9.06623421285141,6.01063611894035,
9.87307868501824));
#109914=CARTESIAN_POINT('Ctrl Pts',(-9.07098582629186,6.0109681915467,9.86915833909039));
#109915=CARTESIAN_POINT('Ctrl Pts',(-9.0814905423681,6.01169591903647,9.86060225949758));
#109916=CARTESIAN_POINT('Ctrl Pts',(-9.08725430213539,6.01209104107755,
9.85597983909939));
#109917=CARTESIAN_POINT('Ctrl Pts',(-9.10760622534809,6.01347191313485,
9.83990972130842));
#109918=CARTESIAN_POINT('Ctrl Pts',(-9.1223770475581,6.01444855376954,9.82869555724841));
#109919=CARTESIAN_POINT('Ctrl Pts',(-9.21790552660439,6.0206128083508,9.75899121276381));
#109920=CARTESIAN_POINT('Ctrl Pts',(-9.30424999006816,6.02548090844909,
9.70860195576097));
#109921=CARTESIAN_POINT('Ctrl Pts',(-9.47528932216425,6.0346211351749,9.63095832930934));
#109922=CARTESIAN_POINT('Ctrl Pts',(-9.5586405582549,6.038886713264,9.60186021444274));
#109923=CARTESIAN_POINT('Ctrl Pts',(-9.65778770622451,6.04424117704663,
9.57700232354516));
#109924=CARTESIAN_POINT('Ctrl Pts',(-9.67153286674872,6.04498973945566,
9.57376686531283));
#109925=CARTESIAN_POINT('Ctrl Pts',(-9.69038436459785,6.04602753189032,
9.56961638844169));
#109926=CARTESIAN_POINT('Ctrl Pts',(-9.69545235965242,6.0463076243835,9.56852878092943));
#109927=CARTESIAN_POINT('Ctrl Pts',(-9.70397079825143,6.04678040793251,
9.56674798192163));
#109928=CARTESIAN_POINT('Ctrl Pts',(-9.70741820900085,6.04697229085019,
9.56604026177898));
#109929=CARTESIAN_POINT('Ctrl Pts',(-9.71397601012079,6.04733839398079,
9.56471864133534));
#109930=CARTESIAN_POINT('Ctrl Pts',(-9.71708590101527,6.04751247577093,
9.56410240145144));
#109931=CARTESIAN_POINT('Ctrl Pts',(-9.72446682569966,6.04792669936896,
9.56266474460264));
#109932=CARTESIAN_POINT('Ctrl Pts',(-9.72873954281502,6.04816733067398,
9.56185225726512));
#109933=CARTESIAN_POINT('Ctrl Pts',(-9.74377070226655,6.04901666308925,
9.5590633436134));
#109934=CARTESIAN_POINT('Ctrl Pts',(-9.75454735747312,6.04963063994186,
9.55718854779365));
#109935=CARTESIAN_POINT('Ctrl Pts',(-9.86708102150152,6.05608732616832,
9.53890849037532));
#109936=CARTESIAN_POINT('Ctrl Pts',(-9.97027283774919,6.06237177883906,
9.53317697744838));
#109937=CARTESIAN_POINT('Ctrl Pts',(-10.1386582383289,6.07248561257343,
9.54161004850172));
#109938=CARTESIAN_POINT('Ctrl Pts',(-10.2038241163778,6.07636962968115,
9.54928138586425));
#109939=CARTESIAN_POINT('Ctrl Pts',(-10.3040906765611,6.08222823466551,
9.56797713593471));
#109940=CARTESIAN_POINT('Ctrl Pts',(-10.3396598823935,6.08428401957572,
9.57599434166768));
#109941=CARTESIAN_POINT('Ctrl Pts',(-10.385103320301,6.08688185296976,9.58803710690994));
#109942=CARTESIAN_POINT('Ctrl Pts',(-10.3952822633051,6.08746190171635,
9.59085283974348));
#109943=CARTESIAN_POINT('Ctrl Pts',(-10.4117717670066,6.08839872628173,
9.59560695580029));
#109944=CARTESIAN_POINT('Ctrl Pts',(-10.4181011360617,6.08875763713726,
9.5974782523236));
#109945=CARTESIAN_POINT('Ctrl Pts',(-10.4302542151432,6.08944553617087,
9.60116092662981));
#109946=CARTESIAN_POINT('Ctrl Pts',(-10.4360796749492,6.08977471857208,
9.6029660127691));
#109947=CARTESIAN_POINT('Ctrl Pts',(-10.4494190677138,6.09052729151737,
9.60719094524674));
#109948=CARTESIAN_POINT('Ctrl Pts',(-10.4569250824447,6.09094988003365,
9.60963528750308));
#109949=CARTESIAN_POINT('Ctrl Pts',(-10.4807938701271,6.09229113394196,
9.61762235466242));
#109950=CARTESIAN_POINT('Ctrl Pts',(-10.4970787556461,6.09320235437092,
9.62339423089913));
#109951=CARTESIAN_POINT('Ctrl Pts',(-10.6474864103047,6.10159206091621,
9.67972061799816));
#109952=CARTESIAN_POINT('Ctrl Pts',(-10.7735907189672,6.10833137986445,
9.74942705050562));
#109953=CARTESIAN_POINT('Ctrl Pts',(-10.9318176043906,6.11816573209087,
9.87011177771781));
#109954=CARTESIAN_POINT('Ctrl Pts',(-10.9741152411387,6.12097342024244,
9.90636857268308));
#109955=CARTESIAN_POINT('Ctrl Pts',(-11.0198680247962,6.12435315626382,
9.95035130128564));
#109956=CARTESIAN_POINT('Ctrl Pts',(-11.0254517645181,6.12477187058527,
9.95580564450794));
#109957=CARTESIAN_POINT('Ctrl Pts',(-11.033893581289,6.12541499353086,9.96418484639018));
#109958=CARTESIAN_POINT('Ctrl Pts',(-11.0367835590472,6.12563699172452,
9.96707753401152));
#109959=CARTESIAN_POINT('Ctrl Pts',(-11.0420383852228,6.12604409212517,
9.97238155879598));
#109960=CARTESIAN_POINT('Ctrl Pts',(-11.044407043167,6.12622889409269,9.97478900482839));
#109961=CARTESIAN_POINT('Ctrl Pts',(-11.0496955546545,6.12664442185702,
9.98020146706591));
#109962=CARTESIAN_POINT('Ctrl Pts',(-11.0526108252374,6.1268754840808,9.98321081096621));
#109963=CARTESIAN_POINT('Ctrl Pts',(-11.0610817406891,6.12755264327352,
9.99203054824887));
#109964=CARTESIAN_POINT('Ctrl Pts',(-11.0666023923804,6.12800125869232,
9.99787415623807));
#109965=CARTESIAN_POINT('Ctrl Pts',(-11.1102798839339,6.13160711449606,
10.0448765420532));
#109966=CARTESIAN_POINT('Ctrl Pts',(-11.1460851233871,6.13491006420475,
10.0881502754917));
#109967=CARTESIAN_POINT('Ctrl Pts',(-11.2180312990137,6.1421668727748,10.1860547029032));
#109968=CARTESIAN_POINT('Ctrl Pts',(-11.2531747000291,6.14612842125434,
10.2412770080597));
#109969=CARTESIAN_POINT('Ctrl Pts',(-11.3113028665365,6.15336603784884,
10.3477398181162));
#109970=CARTESIAN_POINT('Ctrl Pts',(-11.3352649894794,6.15665310519098,
10.3983132786174));
#109971=CARTESIAN_POINT('Ctrl Pts',(-11.3686425860636,6.16173476555258,
10.4806416156491));
#109972=CARTESIAN_POINT('Ctrl Pts',(-11.3799774194024,6.16358618069123,
10.5115553004252));
#109973=CARTESIAN_POINT('Ctrl Pts',(-11.3934463799746,6.16596676404683,
10.5525143211884));
#109974=CARTESIAN_POINT('Ctrl Pts',(-11.3965307380355,6.16652652501124,
10.5622350497297));
#109975=CARTESIAN_POINT('Ctrl Pts',(-11.401420403865,6.16743882689903,10.5782232526967));
#109976=CARTESIAN_POINT('Ctrl Pts',(-11.4032858342451,6.16779329866697,
10.5844718514325));
#109977=CARTESIAN_POINT('Ctrl Pts',(-11.4068233260975,6.16847830398121,
10.5966168829201));
#109978=CARTESIAN_POINT('Ctrl Pts',(-11.4085002324507,6.16880898732581,
10.602511752687));
#109979=CARTESIAN_POINT('Ctrl Pts',(-11.4123025598992,6.16957301203859,
10.6162044179329));
#109980=CARTESIAN_POINT('Ctrl Pts',(-11.4144005256689,6.17000546789695,
10.6240096729527));
#109981=CARTESIAN_POINT('Ctrl Pts',(-11.4210453507104,6.17141217520674,
10.6495739665638));
#109982=CARTESIAN_POINT('Ctrl Pts',(-11.4253233166392,6.17237789432764,
10.6674014793967));
#109983=CARTESIAN_POINT('Ctrl Pts',(-11.4520207565273,6.17885204802569,
10.7886545978085));
#109984=CARTESIAN_POINT('Ctrl Pts',(-11.4634999999948,6.18399426631462,
10.8941661500697));
#109985=CARTESIAN_POINT('Ctrl Pts',(-11.4635,6.189145110564,10.9999999999277));
#109986=CARTESIAN_POINT('Origin',(-10.,3.5,11.));
#109987=CARTESIAN_POINT('',(-11.463499727355,6.76164013593975,10.9991066719022));
#109988=CARTESIAN_POINT('',(-11.4634998124304,6.68841477993962,10.9993388722436));
#109989=CARTESIAN_POINT('',(-11.4635,3.5,11.));
#109990=CARTESIAN_POINT('',(-11.4634994513784,6.26072181654729,11.0012916812098));
#109991=CARTESIAN_POINT('Ctrl Pts',(-11.4634997273561,6.76164013612511,
10.9991066755872));
#109992=CARTESIAN_POINT('Ctrl Pts',(-11.4634766903338,6.75974140573439,
10.9613659897967));
#109993=CARTESIAN_POINT('Ctrl Pts',(-11.4619937755461,6.75780217778772,
10.9236431515581));
#109994=CARTESIAN_POINT('Ctrl Pts',(-11.4585272507504,6.75542963641581,
10.8792671204678));
#109995=CARTESIAN_POINT('Ctrl Pts',(-11.4579526020483,6.75506614139962,
10.8725151927497));
#109996=CARTESIAN_POINT('Ctrl Pts',(-11.4569396555713,6.75446965761194,
10.861517857471));
#109997=CARTESIAN_POINT('Ctrl Pts',(-11.4565296337154,6.75423817156922,
10.8572698737035));
#109998=CARTESIAN_POINT('Ctrl Pts',(-11.4557616291221,6.75382152041032,
10.8496612113574));
#109999=CARTESIAN_POINT('Ctrl Pts',(-11.4554105796174,6.7536367393457,10.8462999134854));
#110000=CARTESIAN_POINT('Ctrl Pts',(-11.4546164770431,6.75323072781694,
10.8389431335412));
#110001=CARTESIAN_POINT('Ctrl Pts',(-11.4541686098306,6.7530092420216,10.8349483023107));
#110002=CARTESIAN_POINT('Ctrl Pts',(-11.4528401893041,6.75237306281412,
10.8235245075761));
#110003=CARTESIAN_POINT('Ctrl Pts',(-11.4519191372956,6.75195622559339,
10.8161004920473));
#110004=CARTESIAN_POINT('Ctrl Pts',(-11.445056196504,6.7490115083928,10.7640519173877));
#110005=CARTESIAN_POINT('Ctrl Pts',(-11.4371154006979,6.74638849443986,
10.7197188648445));
#110006=CARTESIAN_POINT('Ctrl Pts',(-11.412278507717,6.73974205495098,10.6103766182953));
#110007=CARTESIAN_POINT('Ctrl Pts',(-11.3929271760902,6.73567406805343,
10.5460278484075));
#110008=CARTESIAN_POINT('Ctrl Pts',(-11.3362644788532,6.7260581820716,10.3958935241019));
#110009=CARTESIAN_POINT('Ctrl Pts',(-11.2950151259913,6.72058644684051,
10.311895241961));
#110010=CARTESIAN_POINT('Ctrl Pts',(-11.2396961722212,6.71472362894013,
10.2220978425876));
#110011=CARTESIAN_POINT('Ctrl Pts',(-11.2332286693612,6.71405627235717,
10.2118848895927));
#110012=CARTESIAN_POINT('Ctrl Pts',(-11.2224642832084,6.71297426498855,
10.1953436740972));
#110013=CARTESIAN_POINT('Ctrl Pts',(-11.2182431053344,6.71255686917061,
10.1889670377024));
#110014=CARTESIAN_POINT('Ctrl Pts',(-11.2105935739528,6.71181260843058,
10.1776059088211));
#110015=CARTESIAN_POINT('Ctrl Pts',(-11.2071839504809,6.71148505930871,
10.1726090683842));
#110016=CARTESIAN_POINT('Ctrl Pts',(-11.1998786983763,6.71079202658371,
10.162044432933));
#110017=CARTESIAN_POINT('Ctrl Pts',(-11.1959750674047,6.71042685349088,
10.1564823277114));
#110018=CARTESIAN_POINT('Ctrl Pts',(-11.1853866833407,6.70944992244013,
10.1416166960353));
#110019=CARTESIAN_POINT('Ctrl Pts',(-11.178631123743,6.70884085787608,10.1323640339432));
#110020=CARTESIAN_POINT('Ctrl Pts',(-11.1435070314095,6.70574440846674,
10.085424174251));
#110021=CARTESIAN_POINT('Ctrl Pts',(-11.1134357649663,6.70332372090919,
10.04904330392));
#110022=CARTESIAN_POINT('Ctrl Pts',(-11.010429451743,6.69563873161764,9.93602359092591));
#110023=CARTESIAN_POINT('Ctrl Pts',(-10.9309449463051,6.69061964110309,
9.86582439238452));
#110024=CARTESIAN_POINT('Ctrl Pts',(-10.8358594916264,6.6848653261675,9.79863182612754));
#110025=CARTESIAN_POINT('Ctrl Pts',(-10.8270600022895,6.68433468123143,
9.79255711267202));
#110026=CARTESIAN_POINT('Ctrl Pts',(-10.8102001626127,6.68332003863133,
9.78118872614371));
#110027=CARTESIAN_POINT('Ctrl Pts',(-10.8021525054238,6.6828366022932,9.77587722108606));
#110028=CARTESIAN_POINT('Ctrl Pts',(-10.7639092061498,6.68054065376398,
9.75117546598622));
#110029=CARTESIAN_POINT('Ctrl Pts',(-10.7330616269854,6.67869287451012,
9.7328219316908));
#110030=CARTESIAN_POINT('Ctrl Pts',(-10.6957061354172,6.67642332534775,
9.71241702480914));
#110031=CARTESIAN_POINT('Ctrl Pts',(-10.6898171800818,6.67606461998427,
9.70925246481979));
#110032=CARTESIAN_POINT('Ctrl Pts',(-10.6801581267935,6.67547444157025,
9.7041469404916));
#110033=CARTESIAN_POINT('Ctrl Pts',(-10.6764008469551,6.67524441878227,
9.70218178368297));
#110034=CARTESIAN_POINT('Ctrl Pts',(-10.6696348114144,6.67482929967808,
9.69868033056869));
#110035=CARTESIAN_POINT('Ctrl Pts',(-10.6666292206017,6.67464457469725,
9.69713809458523));
#110036=CARTESIAN_POINT('Ctrl Pts',(-10.6600151946942,6.67423735221615,
9.69377316856977));
#110037=CARTESIAN_POINT('Ctrl Pts',(-10.6564045818955,6.67401458833853,
9.69195504036094));
#110038=CARTESIAN_POINT('Ctrl Pts',(-10.6459951871039,6.67337114078406,
9.68676732984023));
#110039=CARTESIAN_POINT('Ctrl Pts',(-10.639177773248,6.67294823832128,9.68343568447771));
#110040=CARTESIAN_POINT('Ctrl Pts',(-10.5889686876092,6.66982443740236,
9.6593805776535));
#110041=CARTESIAN_POINT('Ctrl Pts',(-10.5446085625831,6.66701515702606,
9.64075564474417));
#110042=CARTESIAN_POINT('Ctrl Pts',(-10.4018261915461,6.65799038901365,
9.58891986233803));
#110043=CARTESIAN_POINT('Ctrl Pts',(-10.3007315592184,6.65165006672066,
9.56397256221287));
#110044=CARTESIAN_POINT('Ctrl Pts',(-10.1713997405622,6.64400535460004,
9.54632640320552));
#110045=CARTESIAN_POINT('Ctrl Pts',(-10.1448564578488,6.64245867828334,
9.54344189338611));
#110046=CARTESIAN_POINT('Ctrl Pts',(-10.0862057576738,6.63909347156352,
9.53868748352496));
#110047=CARTESIAN_POINT('Ctrl Pts',(-10.0540850429118,6.63728494193385,
9.53714637172762));
#110048=CARTESIAN_POINT('Ctrl Pts',(-10.011473187987,6.63493050387279,9.53650755110172));
#110049=CARTESIAN_POINT('Ctrl Pts',(-10.0010070445002,6.63435576535727,
9.53646292297054));
#110050=CARTESIAN_POINT('Ctrl Pts',(-9.98396317181616,6.63342542648385,
9.53657308297943));
#110051=CARTESIAN_POINT('Ctrl Pts',(-9.97738550405315,6.63306774475773,
9.53665994797766));
#110052=CARTESIAN_POINT('Ctrl Pts',(-9.96470600657196,6.63238081298814,
9.53691290753786));
#110053=CARTESIAN_POINT('Ctrl Pts',(-9.95860420259536,6.63205137986552,
9.53707283311547));
#110054=CARTESIAN_POINT('Ctrl Pts',(-9.94443361847941,6.63128889570631,
9.53753296819654));
#110055=CARTESIAN_POINT('Ctrl Pts',(-9.93636592447998,6.63085673593114,
9.53786178839829));
#110056=CARTESIAN_POINT('Ctrl Pts',(-9.91052186942392,6.62947830581525,
9.53912944407066));
#110057=CARTESIAN_POINT('Ctrl Pts',(-9.89275940559183,6.62853996961731,
9.5403258555737));
#110058=CARTESIAN_POINT('Ctrl Pts',(-9.80031280902038,6.62369741941265,
9.54824938749413));
#110059=CARTESIAN_POINT('Ctrl Pts',(-9.72620235328725,6.6199632061122,9.56038502841752));
#110060=CARTESIAN_POINT('Ctrl Pts',(-9.57927208519921,6.61255915156996,
9.59620772058036));
#110061=CARTESIAN_POINT('Ctrl Pts',(-9.50672943114754,6.60890157887665,
9.62002605113209));
#110062=CARTESIAN_POINT('Ctrl Pts',(-9.42432347592268,6.60445447073088,
9.65441487566535));
#110063=CARTESIAN_POINT('Ctrl Pts',(-9.41233984663203,6.60380004068105,
9.65960516299982));
#110064=CARTESIAN_POINT('Ctrl Pts',(-9.36893416929882,6.60139610096152,
9.67909877613972));
#110065=CARTESIAN_POINT('Ctrl Pts',(-9.33795340122862,6.59961564764115,
9.69435147188901));
#110066=CARTESIAN_POINT('Ctrl Pts',(-9.30171591329662,6.59742189589772,
9.71381364609854));
#110067=CARTESIAN_POINT('Ctrl Pts',(-9.2959099828604,6.59706692152894,9.7169827564594));
#110068=CARTESIAN_POINT('Ctrl Pts',(-9.28643668965028,6.59648165791445,
9.72223732673075));
#110069=CARTESIAN_POINT('Ctrl Pts',(-9.2827564476262,6.59625277862423,9.72429951291286));
#110070=CARTESIAN_POINT('Ctrl Pts',(-9.27614603032912,6.5958388452928,9.72804123994868));
#110071=CARTESIAN_POINT('Ctrl Pts',(-9.27321269979408,6.59565415262042,
9.72971504120123));
#110072=CARTESIAN_POINT('Ctrl Pts',(-9.26676495754305,6.59524593246318,
9.73342386162479));
#110073=CARTESIAN_POINT('Ctrl Pts',(-9.26325325342763,6.59502212966786,
9.73546333687484));
#110074=CARTESIAN_POINT('Ctrl Pts',(-9.25312893352764,6.59437274808814,
9.7413996772089));
#110075=CARTESIAN_POINT('Ctrl Pts',(-9.24653852850315,6.59394488841513,
9.74533392161576));
#110076=CARTESIAN_POINT('Ctrl Pts',(-9.19648890119403,6.59065796194353,
9.77574836305994));
#110077=CARTESIAN_POINT('Ctrl Pts',(-9.1544102622679,6.58767768782419,9.80442516748937));
#110078=CARTESIAN_POINT('Ctrl Pts',(-9.02723419317661,6.57816578136807,
9.9011730339746));
#110079=CARTESIAN_POINT('Ctrl Pts',(-8.94817448956919,6.57151747219421,
9.97659336176716));
#110080=CARTESIAN_POINT('Ctrl Pts',(-8.84743432461422,6.56239080822099,
10.0968268410983));
#110081=CARTESIAN_POINT('Ctrl Pts',(-8.81847411603009,6.55966201937285,
10.1350568194189));
#110082=CARTESIAN_POINT('Ctrl Pts',(-8.78476405623198,6.556348839506,10.1844180116743));
#110083=CARTESIAN_POINT('Ctrl Pts',(-8.77820682725676,6.55569711042855,
10.1942743436741));
#110084=CARTESIAN_POINT('Ctrl Pts',(-8.76799234867724,6.55466994369967,
10.2100394591696));
#110085=CARTESIAN_POINT('Ctrl Pts',(-8.76425644412322,6.55429162076989,
10.2158964510924));
#110086=CARTESIAN_POINT('Ctrl Pts',(-8.75735557852207,6.55358773206872,
10.2268871626428));
#110087=CARTESIAN_POINT('Ctrl Pts',(-8.75418038399279,6.55326179750983,
10.2320142557398));
#110088=CARTESIAN_POINT('Ctrl Pts',(-8.74716722693097,6.55253717597813,
10.2434965904973));
#110089=CARTESIAN_POINT('Ctrl Pts',(-8.74334573428496,6.55213908969481,
10.2498617293605));
#110090=CARTESIAN_POINT('Ctrl Pts',(-8.73224605268452,6.55097299417077,
10.2686724169392));
#110091=CARTESIAN_POINT('Ctrl Pts',(-8.72510302808039,6.55020980815627,
10.2811969427675));
#110092=CARTESIAN_POINT('Ctrl Pts',(-8.66951087766547,6.54416082360184,
10.3821082529389));
#110093=CARTESIAN_POINT('Ctrl Pts',(-8.63012436627499,6.53921440948321,
10.4751808704421));
#110094=CARTESIAN_POINT('Ctrl Pts',(-8.57227405234132,6.52959503197681,
10.6641389410706));
#110095=CARTESIAN_POINT('Ctrl Pts',(-8.55319228286888,6.52493384855663,
10.7592783469866));
#110096=CARTESIAN_POINT('Ctrl Pts',(-8.54252131499585,6.51923518128711,
10.8668941694635));
#110097=CARTESIAN_POINT('Ctrl Pts',(-8.54153213907268,6.51863061424948,
10.8782101710165));
#110098=CARTESIAN_POINT('Ctrl Pts',(-8.54034125799299,6.51778128682468,
10.8939427699123));
#110099=CARTESIAN_POINT('Ctrl Pts',(-8.54002766683981,6.51754236153391,
10.8983507768655));
#110100=CARTESIAN_POINT('Ctrl Pts',(-8.53952224486626,6.51712921396665,
10.9059407717107));
#110101=CARTESIAN_POINT('Ctrl Pts',(-8.53932083550362,6.51695551426358,
10.9091221166943));
#110102=CARTESIAN_POINT('Ctrl Pts',(-8.53892014000824,6.51658991093408,
10.9157970450796));
#110103=CARTESIAN_POINT('Ctrl Pts',(-8.53872298852783,6.51639788648051,
10.9192907078615));
#110104=CARTESIAN_POINT('Ctrl Pts',(-8.53826995841372,6.51592501326122,
10.9278652859457));
#110105=CARTESIAN_POINT('Ctrl Pts',(-8.53802804143712,6.51564340986202,
10.9329468699114));
#110106=CARTESIAN_POINT('Ctrl Pts',(-8.53724250649838,6.51461157419837,
10.9514814936588));
#110107=CARTESIAN_POINT('Ctrl Pts',(-8.53685806753742,6.51385327151785,
10.9649402015591));
#110108=CARTESIAN_POINT('Ctrl Pts',(-8.53635914556255,6.51192918152371,
10.9987436042074));
#110109=CARTESIAN_POINT('Ctrl Pts',(-8.53648311164518,6.51075342434788,
11.0190886041612));
#110110=CARTESIAN_POINT('Ctrl Pts',(-8.54071338631265,6.50157673869878,
11.1760702021066));
#110111=CARTESIAN_POINT('Ctrl Pts',(-8.56352053996646,6.49312720394605,
11.3115331982211));
#110112=CARTESIAN_POINT('Ctrl Pts',(-8.61777463768181,6.48272372482155,
11.4828366145295));
#110113=CARTESIAN_POINT('Ctrl Pts',(-8.63254496264598,6.48028619518263,
11.5232068418696));
#110114=CARTESIAN_POINT('Ctrl Pts',(-8.65353402259502,6.47726366782131,
11.5735819425154));
#110115=CARTESIAN_POINT('Ctrl Pts',(-8.65812379982414,6.476625293157,11.5842389471223));
#110116=CARTESIAN_POINT('Ctrl Pts',(-8.6656148546357,6.47561804847663,11.6010783184673));
#110117=CARTESIAN_POINT('Ctrl Pts',(-8.66843343461874,6.47524641362629,
11.6072967522178));
#110118=CARTESIAN_POINT('Ctrl Pts',(-8.67357575850673,6.47458132572557,
11.6184339671171));
#110119=CARTESIAN_POINT('Ctrl Pts',(-8.67588359514665,6.47428734034416,
11.6233599181879));
#110120=CARTESIAN_POINT('Ctrl Pts',(-8.68135615977891,6.47360058499883,
11.6348732785525));
#110121=CARTESIAN_POINT('Ctrl Pts',(-8.68454288719673,6.47320857468935,
11.6414501104343));
#110122=CARTESIAN_POINT('Ctrl Pts',(-8.69391246520662,6.47207831580035,
11.6604237283802));
#110123=CARTESIAN_POINT('Ctrl Pts',(-8.7002223221774,6.47134444232889,11.6727571293239));
#110124=CARTESIAN_POINT('Ctrl Pts',(-8.75283245229806,6.46543665597835,
11.7720861843529));
#110125=CARTESIAN_POINT('Ctrl Pts',(-8.80763729227501,6.46058702717733,
11.8542938533409));
#110126=CARTESIAN_POINT('Ctrl Pts',(-8.9340223552646,6.45090540583437,12.00775627458));
#110127=CARTESIAN_POINT('Ctrl Pts',(-9.00552306219934,6.44609346584908,
12.0783745565994));
#110128=CARTESIAN_POINT('Ctrl Pts',(-9.09238560791968,6.44022045134425,
12.1481260493683));
#110129=CARTESIAN_POINT('Ctrl Pts',(-9.1011849735275,6.43962506323052,12.1550276374416));
#110130=CARTESIAN_POINT('Ctrl Pts',(-9.11354717114549,6.43878666981082,
12.1644968449683));
#110131=CARTESIAN_POINT('Ctrl Pts',(-9.11704398933176,6.43854930638491,
12.167150462432));
#110132=CARTESIAN_POINT('Ctrl Pts',(-9.12309454251176,6.43813813124554,
12.1716992710455));
#110133=CARTESIAN_POINT('Ctrl Pts',(-9.12564263440511,6.43796483060316,
12.1736019597695));
#110134=CARTESIAN_POINT('Ctrl Pts',(-9.13101364315418,6.43759919604268,
12.1775853514085));
#110135=CARTESIAN_POINT('Ctrl Pts',(-9.13383785742809,6.43740673566227,
12.179664227753));
#110136=CARTESIAN_POINT('Ctrl Pts',(-9.14080813552137,6.43693129886868,
12.1847564561603));
#110137=CARTESIAN_POINT('Ctrl Pts',(-9.14496258964638,6.43664754967818,
12.1877582016945));
#110138=CARTESIAN_POINT('Ctrl Pts',(-9.16029864175547,6.4355989784113,12.198716906009));
#110139=CARTESIAN_POINT('Ctrl Pts',(-9.17157589690446,6.43482574909199,
12.2065380513964));
#110140=CARTESIAN_POINT('Ctrl Pts',(-9.25141701923626,6.42934578582872,
12.260263428372));
#110141=CARTESIAN_POINT('Ctrl Pts',(-9.32364095183151,6.42436841393295,
12.3004525518307));
#110142=CARTESIAN_POINT('Ctrl Pts',(-9.49556378061459,6.41302193435636,
12.3779064377561));
#110143=CARTESIAN_POINT('Ctrl Pts',(-9.59673243830619,6.40671184978047,
12.410838062045));
#110144=CARTESIAN_POINT('Ctrl Pts',(-9.7167942168775,6.39983462798635,12.4359320842108));
#110145=CARTESIAN_POINT('Ctrl Pts',(-9.73306019329736,6.39891461834012,
12.4390446960002));
#110146=CARTESIAN_POINT('Ctrl Pts',(-9.75815932025603,6.39751257495687,
12.4434073623064));
#110147=CARTESIAN_POINT('Ctrl Pts',(-9.7669565621134,6.39702445482888,12.4448537949936));
#110148=CARTESIAN_POINT('Ctrl Pts',(-9.78132698594896,6.39623235675098,
12.4470818995353));
#110149=CARTESIAN_POINT('Ctrl Pts',(-9.78689234006223,6.39592687492211,
12.4479119577992));
#110150=CARTESIAN_POINT('Ctrl Pts',(-9.79860936751232,6.39528637339991,
12.4495905021196));
#110151=CARTESIAN_POINT('Ctrl Pts',(-9.80476194335179,6.3949515781827,12.4504319748111));
#110152=CARTESIAN_POINT('Ctrl Pts',(-9.81954207845712,6.39415089740001,
12.4523576677396));
#110153=CARTESIAN_POINT('Ctrl Pts',(-9.82817436396092,6.39368619096771,
12.4534042148267));
#110154=CARTESIAN_POINT('Ctrl Pts',(-9.85815242857285,6.39208212867266,
12.4567678293239));
#110155=CARTESIAN_POINT('Ctrl Pts',(-9.87954002367731,6.39095491276024,
12.4586921190527));
#110156=CARTESIAN_POINT('Ctrl Pts',(-9.967364125955,6.38638764105288,12.4646489500817));
#110157=CARTESIAN_POINT('Ctrl Pts',(-10.0339989373755,6.38307052646329,
12.4646183338377));
#110158=CARTESIAN_POINT('Ctrl Pts',(-10.1742840578023,6.37617619102798,
12.4549712470941));
#110159=CARTESIAN_POINT('Ctrl Pts',(-10.2476690867091,6.37262193757632,
12.4442907364485));
#110160=CARTESIAN_POINT('Ctrl Pts',(-10.3703656339709,6.36639019577888,
12.416803842459));
#110161=CARTESIAN_POINT('Ctrl Pts',(-10.4201642585547,6.36377463331692,
12.4028416920848));
#110162=CARTESIAN_POINT('Ctrl Pts',(-10.4760223017506,6.36063704414652,
12.3839393747946));
#110163=CARTESIAN_POINT('Ctrl Pts',(-10.4829119300004,6.36024642016737,
12.3815503930139));
#110164=CARTESIAN_POINT('Ctrl Pts',(-10.4939058042378,6.35961685278395,
12.3776459796838));
#110165=CARTESIAN_POINT('Ctrl Pts',(-10.498021692195,6.35937974692176,12.3761634284863));
#110166=CARTESIAN_POINT('Ctrl Pts',(-10.5053198100759,6.35895671391064,
12.3734976032463));
#110167=CARTESIAN_POINT('Ctrl Pts',(-10.5085046474403,6.35877121690252,
12.3723216823753));
#110168=CARTESIAN_POINT('Ctrl Pts',(-10.5153320479257,6.35837162115853,
12.3697738061966));
#110169=CARTESIAN_POINT('Ctrl Pts',(-10.5189731793357,6.35815733072261,
12.3683984208447));
#110170=CARTESIAN_POINT('Ctrl Pts',(-10.5285795127667,6.35758892916199,
12.3647259099395));
#110171=CARTESIAN_POINT('Ctrl Pts',(-10.5345351592353,6.357233426039,12.3624042245558));
#110172=CARTESIAN_POINT('Ctrl Pts',(-10.5664558270761,6.35531201089413,
12.3497190931489));
#110173=CARTESIAN_POINT('Ctrl Pts',(-10.5921335479654,6.3537093000427,12.3386528643372));
#110174=CARTESIAN_POINT('Ctrl Pts',(-10.6723985087093,6.34855158440738,
12.3013001707151));
#110175=CARTESIAN_POINT('Ctrl Pts',(-10.7256776817075,6.34490808157574,
12.2723572954693));
#110176=CARTESIAN_POINT('Ctrl Pts',(-10.8596083154647,6.33539696344837,
12.1884472580106));
#110177=CARTESIAN_POINT('Ctrl Pts',(-10.93684309052,6.32956591955387,12.1285668055197));
#110178=CARTESIAN_POINT('Ctrl Pts',(-11.0275976349151,6.32245076275521,
12.0424197556812));
#110179=CARTESIAN_POINT('Ctrl Pts',(-11.0470974435837,6.32090215137806,
12.0228308435569));
#110180=CARTESIAN_POINT('Ctrl Pts',(-11.0728068959623,6.31883185757511,
11.9954975630767));
#110181=CARTESIAN_POINT('Ctrl Pts',(-11.07950888307,6.31828938031217,11.9882259924712));
#110182=CARTESIAN_POINT('Ctrl Pts',(-11.0904617852464,6.31739801243513,
11.976097836299));
#110183=CARTESIAN_POINT('Ctrl Pts',(-11.0947551226691,6.31704735862846,
11.9712801420549));
#110184=CARTESIAN_POINT('Ctrl Pts',(-11.1030834874465,6.31636461565882,
11.9618092326366));
#110185=CARTESIAN_POINT('Ctrl Pts',(-11.1071212784697,6.31603241629205,
11.9571586371196));
#110186=CARTESIAN_POINT('Ctrl Pts',(-11.116605011712,6.31524925239579,11.9460952784903));
#110187=CARTESIAN_POINT('Ctrl Pts',(-11.1220252840222,6.31479933437832,
11.9396607335401));
#110188=CARTESIAN_POINT('Ctrl Pts',(-11.139361647786,6.31335242828277,11.9187163857525));
#110189=CARTESIAN_POINT('Ctrl Pts',(-11.1510543444261,6.31236431281994,
11.904023616946));
#110190=CARTESIAN_POINT('Ctrl Pts',(-11.2012248891629,6.30806326651345,
11.8384284049846));
#110191=CARTESIAN_POINT('Ctrl Pts',(-11.2366343255074,6.30486667020402,
11.7852643245582));
#110192=CARTESIAN_POINT('Ctrl Pts',(-11.2960505243368,6.29900710509381,
11.6820150514864));
#110193=CARTESIAN_POINT('Ctrl Pts',(-11.3208982213808,6.29633352547457,
11.6325499390586));
#110194=CARTESIAN_POINT('Ctrl Pts',(-11.3570837304205,6.29188944614951,
11.5490277081228));
#110195=CARTESIAN_POINT('Ctrl Pts',(-11.3700763642429,6.29013560249887,
11.5157501987438));
#110196=CARTESIAN_POINT('Ctrl Pts',(-11.3954917384352,6.28627098578904,
11.4428920920733));
#110197=CARTESIAN_POINT('Ctrl Pts',(-11.4074748804916,6.28414992097693,
11.4031928697614));
#110198=CARTESIAN_POINT('Ctrl Pts',(-11.4194808850742,6.28157176804751,
11.3563068987934));
#110199=CARTESIAN_POINT('Ctrl Pts',(-11.4211575362389,6.2811989962082,11.3495594980313));
#110200=CARTESIAN_POINT('Ctrl Pts',(-11.4237981003146,6.280590313098,11.338599895542));
#110201=CARTESIAN_POINT('Ctrl Pts',(-11.4247915658701,6.28035600849023,
11.3343948453261));
#110202=CARTESIAN_POINT('Ctrl Pts',(-11.4265296658571,6.27993636329822,
11.3268895961812));
#110203=CARTESIAN_POINT('Ctrl Pts',(-11.4272814953309,6.27975143116474,
11.3235911439764));
#110204=CARTESIAN_POINT('Ctrl Pts',(-11.4288926792881,6.27934756017723,
11.3164076366362));
#110205=CARTESIAN_POINT('Ctrl Pts',(-11.4297476173439,6.2791283861473,11.3125217294455));
#110206=CARTESIAN_POINT('Ctrl Pts',(-11.4314814097162,6.27867372956234,
11.3044851784145));
#110207=CARTESIAN_POINT('Ctrl Pts',(-11.4323580818218,6.27843813149116,
11.3003341052601));
#110208=CARTESIAN_POINT('Ctrl Pts',(-11.4345664444169,6.27782977950123,
11.2896478021357));
#110209=CARTESIAN_POINT('Ctrl Pts',(-11.4358715189401,6.27745567019768,
11.2831072421368));
#110210=CARTESIAN_POINT('Ctrl Pts',(-11.4395749326088,6.27635017379599,
11.2638624853237));
#110211=CARTESIAN_POINT('Ctrl Pts',(-11.4418496348152,6.27561304523844,
11.2511354359563));
#110212=CARTESIAN_POINT('Ctrl Pts',(-11.4568941607282,6.27029981905276,
11.1600053367267));
#110213=CARTESIAN_POINT('Ctrl Pts',(-11.4634293422371,6.26549925452231,
11.0807138769344));
#110214=CARTESIAN_POINT('Ctrl Pts',(-11.4634994301469,6.26072184081485,
11.0012914950893));
#110215=CARTESIAN_POINT('Ctrl Pts',(-11.4634994299846,6.26072185188138,
11.0012916790654));
#110216=CARTESIAN_POINT('Ctrl Pts',(-11.4634998099988,6.26069595259754,
11.0008611149732));
#110217=CARTESIAN_POINT('Ctrl Pts',(-11.4635,6.26067005423938,11.000430555273));
#110218=CARTESIAN_POINT('Ctrl Pts',(-11.4635,6.26064415683876,11.0000000000891));
#110219=CARTESIAN_POINT('Ctrl Pts',(-11.4635,6.189145110564,10.9999999999277));
#110220=CARTESIAN_POINT('Ctrl Pts',(-11.4635,6.1891661123127,11.000431520628));
#110221=CARTESIAN_POINT('Ctrl Pts',(-11.463499809146,6.18918711470186,11.0008630466623));
#110222=CARTESIAN_POINT('Ctrl Pts',(-11.4634246718514,6.19332130417299,
11.0858045405408));
#110223=CARTESIAN_POINT('Ctrl Pts',(-11.4560299909816,6.19743501857092,
11.1701401052918));
#110224=CARTESIAN_POINT('Ctrl Pts',(-11.439337749849,6.20250900789312,11.2651064768895));
#110225=CARTESIAN_POINT('Ctrl Pts',(-11.4371287182732,6.20314340504571,
11.2768314133686));
#110226=CARTESIAN_POINT('Ctrl Pts',(-11.4338894976385,6.20402750178027,
11.292939256193));
#110227=CARTESIAN_POINT('Ctrl Pts',(-11.432982012597,6.20427070847752,11.2973466827823));
#110228=CARTESIAN_POINT('Ctrl Pts',(-11.4313924650699,6.20468931615201,
11.304890410363));
#110229=CARTESIAN_POINT('Ctrl Pts',(-11.430720379412,6.20486416293798,11.3080288085857));
#110230=CARTESIAN_POINT('Ctrl Pts',(-11.4292977500027,6.20522990781271,
11.3145668655167));
#110231=CARTESIAN_POINT('Ctrl Pts',(-11.4285453952363,6.20542091206794,
11.3179660735744));
#110232=CARTESIAN_POINT('Ctrl Pts',(-11.4266846000497,6.20588747796026,
11.3262333972047));
#110233=CARTESIAN_POINT('Ctrl Pts',(-11.4255633671261,6.20616374915755,
11.3310985688485));
#110234=CARTESIAN_POINT('Ctrl Pts',(-11.4214720769915,6.20715463933583,
11.3484451039024));
#110235=CARTESIAN_POINT('Ctrl Pts',(-11.4183628973471,6.20787653344378,
11.3608926774896));
#110236=CARTESIAN_POINT('Ctrl Pts',(-11.4102273434133,6.20968941312915,
11.3917328284722));
#110237=CARTESIAN_POINT('Ctrl Pts',(-11.4050045031911,6.21078903755881,
11.4100707918858));
#110238=CARTESIAN_POINT('Ctrl Pts',(-11.381077359834,6.21555559142255,11.4882500874388));
#110239=CARTESIAN_POINT('Ctrl Pts',(-11.3588971493999,6.21933127001888,
11.5469557935838));
#110240=CARTESIAN_POINT('Ctrl Pts',(-11.2883626102926,6.2296151342905,11.702610624167));
#110241=CARTESIAN_POINT('Ctrl Pts',(-11.2329035090032,6.23605972907879,
11.7959245909927));
#110242=CARTESIAN_POINT('Ctrl Pts',(-11.1566563845335,6.24314953014151,
11.896833886094));
#110243=CARTESIAN_POINT('Ctrl Pts',(-11.145387764013,6.24416180167514,11.9111816082512));
#110244=CARTESIAN_POINT('Ctrl Pts',(-11.1287534449904,6.24560657884361,
11.9315647997032));
#110245=CARTESIAN_POINT('Ctrl Pts',(-11.1236017645435,6.24604747802263,
11.937772037316));
#110246=CARTESIAN_POINT('Ctrl Pts',(-11.1144477726761,6.24681959406337,
11.9486179103597));
#110247=CARTESIAN_POINT('Ctrl Pts',(-11.1104671951861,6.24715167334041,
11.9532745605917));
#110248=CARTESIAN_POINT('Ctrl Pts',(-11.1021852624572,6.24783512414195,
11.9628408488933));
#110249=CARTESIAN_POINT('Ctrl Pts',(-11.0978800600493,6.24818632779997,
11.9677469858936));
#110250=CARTESIAN_POINT('Ctrl Pts',(-11.0867459466133,6.24908433764534,
11.9802653069339));
#110251=CARTESIAN_POINT('Ctrl Pts',(-11.0798697503712,6.24962917811855,
11.9878350842966));
#110252=CARTESIAN_POINT('Ctrl Pts',(-11.0503505133671,6.25192805190795,
12.0196552333213));
#110253=CARTESIAN_POINT('Ctrl Pts',(-11.0269648428255,6.25365063691154,
12.0432048805704));
#110254=CARTESIAN_POINT('Ctrl Pts',(-10.9615792014568,6.25823401738371,
12.1047172895536));
#110255=CARTESIAN_POINT('Ctrl Pts',(-10.9181444979434,6.26103473532356,
12.1410723693714));
#110256=CARTESIAN_POINT('Ctrl Pts',(-10.8049950104029,6.26792965623479,
12.2251249544868));
#110257=CARTESIAN_POINT('Ctrl Pts',(-10.7330603779082,6.27196720254323,
12.269475920929));
#110258=CARTESIAN_POINT('Ctrl Pts',(-10.6534326940461,6.27645443154008,
12.309534613145));
#110259=CARTESIAN_POINT('Ctrl Pts',(-10.6491436612378,6.27669620948599,
12.3116659998137));
#110260=CARTESIAN_POINT('Ctrl Pts',(-10.6153194396795,6.27860411246096,
12.3282680316871));
#110261=CARTESIAN_POINT('Ctrl Pts',(-10.5853165066602,6.28030351165344,
12.3417593892835));
#110262=CARTESIAN_POINT('Ctrl Pts',(-10.548265233972,6.28243969939094,12.3569409312405));
#110263=CARTESIAN_POINT('Ctrl Pts',(-10.541623903592,6.28282404815149,12.3596054576904));
#110264=CARTESIAN_POINT('Ctrl Pts',(-10.5312453583326,6.28342731073243,
12.3636812587087));
#110265=CARTESIAN_POINT('Ctrl Pts',(-10.5275213644763,6.28364429634303,
12.3651261536406));
#110266=CARTESIAN_POINT('Ctrl Pts',(-10.520632868438,6.28404671630293,12.3677664674015));
#110267=CARTESIAN_POINT('Ctrl Pts',(-10.5174700982641,6.28423189592542,
12.3689661755446));
#110268=CARTESIAN_POINT('Ctrl Pts',(-10.510274744673,6.28465411166599,12.3716670331593));
#110269=CARTESIAN_POINT('Ctrl Pts',(-10.5062397001636,6.28489153716534,
12.373161363395));
#110270=CARTESIAN_POINT('Ctrl Pts',(-10.49387491415,6.28562095722229,12.3776786062192));
#110271=CARTESIAN_POINT('Ctrl Pts',(-10.4855244116701,6.28611614911237,
12.3806436218913));
#110272=CARTESIAN_POINT('Ctrl Pts',(-10.4080677621062,6.29072979436664,
12.4073565916349));
#110273=CARTESIAN_POINT('Ctrl Pts',(-10.3373068469105,6.29508939958693,
12.425971216637));
#110274=CARTESIAN_POINT('Ctrl Pts',(-10.1426733474741,6.30698568471396,
12.4618707413526));
#110275=CARTESIAN_POINT('Ctrl Pts',(-10.0174679729956,6.31448853329586,
12.4687162676468));
#110276=CARTESIAN_POINT('Ctrl Pts',(-9.87615001354495,6.32241275794081,
12.4583468563332));
#110277=CARTESIAN_POINT('Ctrl Pts',(-9.85942048903276,6.3233433074189,12.4568293676562));
#110278=CARTESIAN_POINT('Ctrl Pts',(-9.8349596064023,6.32469329148715,12.4541852875142));
#110279=CARTESIAN_POINT('Ctrl Pts',(-9.82720565654582,6.3251196651968,12.453284314958));
#110280=CARTESIAN_POINT('Ctrl Pts',(-9.81341995082756,6.32587501861012,
12.4515705877286));
#110281=CARTESIAN_POINT('Ctrl Pts',(-9.80738540188954,6.32620474593271,
12.4507821697445));
#110282=CARTESIAN_POINT('Ctrl Pts',(-9.79477583607914,6.3268918656907,12.4490546581122));
#110283=CARTESIAN_POINT('Ctrl Pts',(-9.7882019301542,6.32724902698332,12.4481084003785));
#110284=CARTESIAN_POINT('Ctrl Pts',(-9.77100491799356,6.32818067126909,
12.4455134263385));
#110285=CARTESIAN_POINT('Ctrl Pts',(-9.76039303226953,6.32875288963202,
12.4437923405117));
#110286=CARTESIAN_POINT('Ctrl Pts',(-9.71191716242938,6.33135557150926,
12.4353811040017));
#110287=CARTESIAN_POINT('Ctrl Pts',(-9.67430544550673,6.33334289558289,
12.4273170697689));
#110288=CARTESIAN_POINT('Ctrl Pts',(-9.52383457807275,6.34122292841183,
12.3887970100353));
#110289=CARTESIAN_POINT('Ctrl Pts',(-9.41450233072162,6.34674913683043,
12.3463588857786));
#110290=CARTESIAN_POINT('Ctrl Pts',(-9.30447220946037,6.35291694712337,
12.2876857789482));
#110291=CARTESIAN_POINT('Ctrl Pts',(-9.2975920995346,6.3533054953928,12.2839457589748));
#110292=CARTESIAN_POINT('Ctrl Pts',(-9.27946745323676,6.35433752114194,
12.2739039390322));
#110293=CARTESIAN_POINT('Ctrl Pts',(-9.26827572561913,6.35498347439784,
12.267508568528));
#110294=CARTESIAN_POINT('Ctrl Pts',(-9.22735266738228,6.35738279077261,
12.2434009701976));
#110295=CARTESIAN_POINT('Ctrl Pts',(-9.19816973426201,6.35916735452538,
12.2247847761987));
#110296=CARTESIAN_POINT('Ctrl Pts',(-9.16422465343283,6.36136579441722,
12.2013973726671));
#110297=CARTESIAN_POINT('Ctrl Pts',(-9.15879874826343,6.36172106447749,
12.1976044955671));
#110298=CARTESIAN_POINT('Ctrl Pts',(-9.14995581642798,6.36230675086501,
12.1913332668282));
#110299=CARTESIAN_POINT('Ctrl Pts',(-9.1465233915624,6.36253575433924,12.1888766734289));
#110300=CARTESIAN_POINT('Ctrl Pts',(-9.14036295824545,6.36294986651786,
12.1844272117324));
#110301=CARTESIAN_POINT('Ctrl Pts',(-9.13763117347545,6.36313461313047,
12.1824397109788));
#110302=CARTESIAN_POINT('Ctrl Pts',(-9.13163048846169,6.36354290077385,
12.1780420770394));
#110303=CARTESIAN_POINT('Ctrl Pts',(-9.12836476777925,6.36376671683052,
12.1756278173726));
#110304=CARTESIAN_POINT('Ctrl Pts',(-9.11895787239892,6.36441599764191,
12.1686128103497));
#110305=CARTESIAN_POINT('Ctrl Pts',(-9.11284287248267,6.36484374152741,
12.163977386823));
#110306=CARTESIAN_POINT('Ctrl Pts',(-9.06654742417541,6.36812376872548,
12.1283067806633));
#110307=CARTESIAN_POINT('Ctrl Pts',(-9.02797339718941,6.3710966889408,12.0952503000835));
#110308=CARTESIAN_POINT('Ctrl Pts',(-8.91232403265526,6.38059833723132,
11.9852138856488));
#110309=CARTESIAN_POINT('Ctrl Pts',(-8.84206017340091,6.38724453507976,
11.9015901411413));
#110310=CARTESIAN_POINT('Ctrl Pts',(-8.75508586776139,6.39637842719503,
11.770929198254));
#110311=CARTESIAN_POINT('Ctrl Pts',(-8.73043522396423,6.39911558255167,
11.729622532684));
#110312=CARTESIAN_POINT('Ctrl Pts',(-8.70229679931413,6.40243736565787,
11.6767119465783));
#110313=CARTESIAN_POINT('Ctrl Pts',(-8.6968602194612,6.40308975022912,11.6661826923902));
#110314=CARTESIAN_POINT('Ctrl Pts',(-8.68843836003114,6.40411777885849,
11.6493740271501));
#110315=CARTESIAN_POINT('Ctrl Pts',(-8.68536899305357,6.4044963152003,11.6431375284242));
#110316=CARTESIAN_POINT('Ctrl Pts',(-8.67971911596831,6.40520050167493,
11.6314483537237));
#110317=CARTESIAN_POINT('Ctrl Pts',(-8.6771276722616,6.40552652169316,11.6260011518868));
#110318=CARTESIAN_POINT('Ctrl Pts',(-8.6714222638398,6.40625120981021,11.6138147597212));
#110319=CARTESIAN_POINT('Ctrl Pts',(-8.66832573701981,6.40664927798001,
11.6070675583003));
#110320=CARTESIAN_POINT('Ctrl Pts',(-8.65937029274392,6.40781493437883,
11.5871557400214));
#110321=CARTESIAN_POINT('Ctrl Pts',(-8.65365421070497,6.40857770642582,
11.5739276174317));
#110322=CARTESIAN_POINT('Ctrl Pts',(-8.60965499604112,6.41460838482074,
11.4678283751579));
#110323=CARTESIAN_POINT('Ctrl Pts',(-8.5808295789151,6.41953944699433,11.3713230142977));
#110324=CARTESIAN_POINT('Ctrl Pts',(-8.54401287212679,6.42916065784511,
11.1771374313188));
#110325=CARTESIAN_POINT('Ctrl Pts',(-8.53546768393207,6.43383817344887,
11.0801042342729));
#110326=CARTESIAN_POINT('Ctrl Pts',(-8.53673142403795,6.43955595299073,
10.971608574267));
#110327=CARTESIAN_POINT('Ctrl Pts',(-8.53699552216339,6.44015987425747,
10.9602648673176));
#110328=CARTESIAN_POINT('Ctrl Pts',(-8.53754566418645,6.44100847472973,
10.9445105094832));
#110329=CARTESIAN_POINT('Ctrl Pts',(-8.53771983316455,6.44124733293883,
10.9400960722164));
#110330=CARTESIAN_POINT('Ctrl Pts',(-8.53805408919055,6.44166042705985,
10.932497651389));
#110331=CARTESIAN_POINT('Ctrl Pts',(-8.53820459831125,6.441834141094,10.9293132515738));
#110332=CARTESIAN_POINT('Ctrl Pts',(-8.53854221978982,6.44219985107157,
10.9226329322084));
#110333=CARTESIAN_POINT('Ctrl Pts',(-8.53873147288181,6.44239196840482,
10.919137169389));
#110334=CARTESIAN_POINT('Ctrl Pts',(-8.53922678545627,6.44286520452323,
10.9105584191917));
#110335=CARTESIAN_POINT('Ctrl Pts',(-8.53954683370768,6.44314707998011,
10.9054763087917));
#110336=CARTESIAN_POINT('Ctrl Pts',(-8.54081157520264,6.44418070538868,
10.8869363069883));
#110337=CARTESIAN_POINT('Ctrl Pts',(-8.54191579521966,6.44494055990392,
10.8734903833549));
#110338=CARTESIAN_POINT('Ctrl Pts',(-8.54515607803518,6.44686934033336,
10.8397580836191));
#110339=CARTESIAN_POINT('Ctrl Pts',(-8.54753064830014,6.44804829259003,
10.8194978700412));
#110340=CARTESIAN_POINT('Ctrl Pts',(-8.56921625361718,6.45728946592261,
10.6628650315527));
#110341=CARTESIAN_POINT('Ctrl Pts',(-8.60726816982389,6.46580451983366,
10.529778137404));
#110342=CARTESIAN_POINT('Ctrl Pts',(-8.68046501034125,6.47619955536067,
10.3656337038305));
#110343=CARTESIAN_POINT('Ctrl Pts',(-8.69919702582557,6.47857868578438,
10.3280585563514));
#110344=CARTESIAN_POINT('Ctrl Pts',(-8.72510674434366,6.48154181482339,
10.2812423438655));
#110345=CARTESIAN_POINT('Ctrl Pts',(-8.73081315283062,6.48217657863567,
10.2712132416078));
#110346=CARTESIAN_POINT('Ctrl Pts',(-8.7400774365639,6.48317953014526,10.2553700118201));
#110347=CARTESIAN_POINT('Ctrl Pts',(-8.74355826775016,6.48355044135184,
10.2495115851688));
#110348=CARTESIAN_POINT('Ctrl Pts',(-8.74989293783888,6.48421498862915,
10.2390176008194));
#110349=CARTESIAN_POINT('Ctrl Pts',(-8.75273194616726,6.48450915024345,
10.2343732752066));
#110350=CARTESIAN_POINT('Ctrl Pts',(-8.75945506014903,6.48519728179882,
10.2235115959183));
#110351=CARTESIAN_POINT('Ctrl Pts',(-8.76336011968737,6.48559048279469,
10.2173073409469));
#110352=CARTESIAN_POINT('Ctrl Pts',(-8.77483460541817,6.48672739955703,
10.1993772493488));
#110353=CARTESIAN_POINT('Ctrl Pts',(-8.78252546186566,6.48746665996089,
10.1877298481481));
#110354=CARTESIAN_POINT('Ctrl Pts',(-8.85104538468401,6.49386328915692,
10.0871200763126));
#110355=CARTESIAN_POINT('Ctrl Pts',(-8.92136186301909,6.49912516150783,
10.0050179513429));
#110356=CARTESIAN_POINT('Ctrl Pts',(-9.0658530029645,6.50875409282547,9.86981435689484));
#110357=CARTESIAN_POINT('Ctrl Pts',(-9.13717931779434,6.51311800831979,
9.81446767233331));
#110358=CARTESIAN_POINT('Ctrl Pts',(-9.22300917556595,6.51847745592388,
9.75973599955377));
#110359=CARTESIAN_POINT('Ctrl Pts',(-9.23296325327591,6.51910067118624,
9.75355539865387));
#110360=CARTESIAN_POINT('Ctrl Pts',(-9.24681765252976,6.51997186850159,
9.74518184476771));
#110361=CARTESIAN_POINT('Ctrl Pts',(-9.25065568571012,6.52021360957955,
9.74288610347632));
#110362=CARTESIAN_POINT('Ctrl Pts',(-9.25725976737182,6.52063035559362,
9.73897682369774));
#110363=CARTESIAN_POINT('Ctrl Pts',(-9.2600207233144,6.52080481728032,9.7373546919234));
#110364=CARTESIAN_POINT('Ctrl Pts',(-9.26579989889062,6.52117053060454,
9.7339847449228));
#110365=CARTESIAN_POINT('Ctrl Pts',(-9.26881905908328,6.52136189346068,
9.73223864810285));
#110366=CARTESIAN_POINT('Ctrl Pts',(-9.27620343452705,6.52183063089651,
9.72800313113295));
#110367=CARTESIAN_POINT('Ctrl Pts',(-9.28057526831405,6.5221087303593,9.72552538019659));
#110368=CARTESIAN_POINT('Ctrl Pts',(-9.29633973795588,6.52311340214833,
9.71669777571772));
#110369=CARTESIAN_POINT('Ctrl Pts',(-9.30780405049165,6.52384751199259,
9.71047795414609));
#110370=CARTESIAN_POINT('Ctrl Pts',(-9.336604391639,6.52569747132265,9.69534739449104));
#110371=CARTESIAN_POINT('Ctrl Pts',(-9.35403790318474,6.52682239192262,
9.68662836203254));
#110372=CARTESIAN_POINT('Ctrl Pts',(-9.43052037306454,6.53176346335816,
9.65026827947765));
#110373=CARTESIAN_POINT('Ctrl Pts',(-9.49120329026381,6.53569551182621,
9.62624312824905));
#110374=CARTESIAN_POINT('Ctrl Pts',(-9.65304267545736,6.54592100760255,
9.57436769384756));
#110375=CARTESIAN_POINT('Ctrl Pts',(-9.75596277995621,6.55214847789187,
9.55319000017357));
#110376=CARTESIAN_POINT('Ctrl Pts',(-9.87676489717327,6.55895291078649,
9.54160369432716));
#110377=CARTESIAN_POINT('Ctrl Pts',(-9.89328111144568,6.55987327941634,
9.54030215960327));
#110378=CARTESIAN_POINT('Ctrl Pts',(-9.9187173547735,6.56127583823559,9.5387317455743));
#110379=CARTESIAN_POINT('Ctrl Pts',(-9.92762332550629,6.56176411968257,
9.53826356626391));
#110380=CARTESIAN_POINT('Ctrl Pts',(-9.94215633180019,6.56255646827424,
9.53763272749554));
#110381=CARTESIAN_POINT('Ctrl Pts',(-9.94778091850796,6.56286204034146,
9.53742107960036));
#110382=CARTESIAN_POINT('Ctrl Pts',(-9.95961490822182,6.56350272319044,
9.53704413052024));
#110383=CARTESIAN_POINT('Ctrl Pts',(-9.96582443519107,6.56383760941523,
9.53688590189154));
#110384=CARTESIAN_POINT('Ctrl Pts',(-9.98073060105931,6.564638494985,9.53660101680788));
#110385=CARTESIAN_POINT('Ctrl Pts',(-9.98942778501862,6.56510331467634,
9.53651234156083));
#110386=CARTESIAN_POINT('Ctrl Pts',(-10.0196004744835,6.56670771840745,
9.53647369268325));
#110387=CARTESIAN_POINT('Ctrl Pts',(-10.0410742440011,6.56783515775781,
9.53691886782261));
#110388=CARTESIAN_POINT('Ctrl Pts',(-10.1291437699085,6.5724088316484,9.54068526796777));
#110389=CARTESIAN_POINT('Ctrl Pts',(-10.1954876020823,6.57573161966994,
9.5480828719828));
#110390=CARTESIAN_POINT('Ctrl Pts',(-10.3174533901714,6.58180865329662,
9.57019731491684));
#110391=CARTESIAN_POINT('Ctrl Pts',(-10.3731579472535,6.58457296050827,
9.58371420542063));
#110392=CARTESIAN_POINT('Ctrl Pts',(-10.4930608471273,6.59071660020756,
9.62037601683172));
#110393=CARTESIAN_POINT('Ctrl Pts',(-10.5567183513361,6.59410600146427,
9.64481220949848));
#110394=CARTESIAN_POINT('Ctrl Pts',(-10.6258040654603,6.59816000944756,
9.67702319678472));
#110395=CARTESIAN_POINT('Ctrl Pts',(-10.6331437805256,6.59859567182318,
9.68052006555455));
#110396=CARTESIAN_POINT('Ctrl Pts',(-10.6442388846093,6.5992623592887,9.68592000625582));
#110397=CARTESIAN_POINT('Ctrl Pts',(-10.6480159439431,6.59949075654161,
9.68777848443906));
#110398=CARTESIAN_POINT('Ctrl Pts',(-10.654809362227,6.59990424409247,9.69115762603904));
#110399=CARTESIAN_POINT('Ctrl Pts',(-10.6578285279339,6.60008897759479,
9.69267246331612));
#110400=CARTESIAN_POINT('Ctrl Pts',(-10.6608562316969,6.60027521475029,
9.6942047284258));
#110401=CARTESIAN_POINT('Ctrl Pts',(-10.6608700002742,6.60027606168986,
9.69421169672277));
#110402=CARTESIAN_POINT('Ctrl Pts',(-10.6608973651576,6.60027774501247,
9.69422554667354));
#110403=CARTESIAN_POINT('Ctrl Pts',(-10.6609109616453,6.60027858140619,
9.69423242841259));
#110404=CARTESIAN_POINT('Ctrl Pts',(-10.6609379853764,6.60028024382181,
9.69424610675938));
#110405=CARTESIAN_POINT('Ctrl Pts',(-10.6609514124614,6.60028106983348,
9.69425290328039));
#110406=CARTESIAN_POINT('Ctrl Pts',(-10.6609780994838,6.60028271161252,
9.69426641223271));
#110407=CARTESIAN_POINT('Ctrl Pts',(-10.6609913595032,6.60028352738446,
9.69427312469913));
#110408=CARTESIAN_POINT('Ctrl Pts',(-10.66101771496,6.60028514884045,9.69428646682185));
#110409=CARTESIAN_POINT('Ctrl Pts',(-10.6610308103756,6.6002859545227,9.69429309646091));
#110410=CARTESIAN_POINT('Ctrl Pts',(-10.6610568389154,6.60028755593885,
9.69430627406986));
#110411=CARTESIAN_POINT('Ctrl Pts',(-10.661069772066,6.60028835167393,9.69431282204704));
#110412=CARTESIAN_POINT('Ctrl Pts',(-10.6610954784154,6.60028993333834,
9.69432583749862));
#110413=CARTESIAN_POINT('Ctrl Pts',(-10.6611082515916,6.60029071926584,
9.69433230495565));
#110414=CARTESIAN_POINT('Ctrl Pts',(-10.6611336406667,6.60029228147833,
9.69434516070334));
#110415=CARTESIAN_POINT('Ctrl Pts',(-10.6611462563701,6.60029305775087,
9.6943515488893));
#110416=CARTESIAN_POINT('Ctrl Pts',(-10.6611713320181,6.6002946007456,9.69436424684657));
#110417=CARTESIAN_POINT('Ctrl Pts',(-10.6611837922187,6.60029536748313,
9.69437055674194));
#110418=CARTESIAN_POINT('Ctrl Pts',(-10.6612085596618,6.60029689157894,
9.6943830995195));
#110419=CARTESIAN_POINT('Ctrl Pts',(-10.6612208667562,6.60029764892769,
9.69438933232128));
#110420=CARTESIAN_POINT('Ctrl Pts',(-10.6612453299952,6.60029915436833,
9.69440172191245));
#110421=CARTESIAN_POINT('Ctrl Pts',(-10.6612574861225,6.60029990245875,
9.69440787868774));
#110422=CARTESIAN_POINT('Ctrl Pts',(-10.6612816496026,6.60030138951539,
9.69442011731182));
#110423=CARTESIAN_POINT('Ctrl Pts',(-10.6612936569411,6.60030212848036,
9.6944261991482));
#110424=CARTESIAN_POINT('Ctrl Pts',(-10.6613175247513,6.60030359740235,
9.69443828884514));
#110425=CARTESIAN_POINT('Ctrl Pts',(-10.66132938531,6.60030432736435,9.69444429674476));
#110426=CARTESIAN_POINT('Ctrl Pts',(-10.6613529619118,6.60030577842402,
9.69445623974416));
#110427=CARTESIAN_POINT('Ctrl Pts',(-10.6613646778394,6.6003064995142,9.6944621747805));
#110428=CARTESIAN_POINT('Ctrl Pts',(-10.6613879672468,6.60030793295638,
9.69447397308615));
#110429=CARTESIAN_POINT('Ctrl Pts',(-10.661399540627,6.6003086453019,9.6944798363002));
#110430=CARTESIAN_POINT('Ctrl Pts',(-10.6614225467408,6.60031006136458,
9.69449149185953));
#110431=CARTESIAN_POINT('Ctrl Pts',(-10.6614339795171,6.60031076508402,
9.69449728422175));
#110432=CARTESIAN_POINT('Ctrl Pts',(-10.6614567065215,6.60031216402264,
9.69450879912654));
#110433=CARTESIAN_POINT('Ctrl Pts',(-10.6614680007405,6.60031285924093,
9.69451452165997));
#110434=CARTESIAN_POINT('Ctrl Pts',(-10.6614904523384,6.60031424128141,
9.69452589775912));
#110435=CARTESIAN_POINT('Ctrl Pts',(-10.6615016098699,6.60031492811267,
9.69453155139775));
#110436=CARTESIAN_POINT('Ctrl Pts',(-10.6615237900186,6.60031629349663,
9.69454279066984));
#110437=CARTESIAN_POINT('Ctrl Pts',(-10.6615348127304,6.60031697205484,
9.69454837634692));
#110438=CARTESIAN_POINT('Ctrl Pts',(-10.6615567254061,6.60031832102514,
9.69455948078091));
#110439=CARTESIAN_POINT('Ctrl Pts',(-10.6615676152757,6.60031899143111,
9.69456499948583));
#110440=CARTESIAN_POINT('Ctrl Pts',(-10.66158926399,6.60032032420204,9.69457597083605));
#110441=CARTESIAN_POINT('Ctrl Pts',(-10.6616000228429,6.60032098656721,
9.69458142348145));
#110442=CARTESIAN_POINT('Ctrl Pts',(-10.661621411343,6.60032230336766,9.69459226362238));
#110443=CARTESIAN_POINT('Ctrl Pts',(-10.6616320410279,6.60032295780496,
9.69459765113308));
#110444=CARTESIAN_POINT('Ctrl Pts',(-10.6616531728078,6.60032425884825,
9.69460836181169));
#110445=CARTESIAN_POINT('Ctrl Pts',(-10.661663675057,6.60032490546345,9.69461368505383));
#110446=CARTESIAN_POINT('Ctrl Pts',(-10.6616845536058,6.60032619096267,
9.6946242680152));
#110447=CARTESIAN_POINT('Ctrl Pts',(-10.6616949300017,6.60032682985235,
9.69462952777942));
#110448=CARTESIAN_POINT('Ctrl Pts',(-10.6617155595835,6.60032810006836,
9.69463998516226));
#110449=CARTESIAN_POINT('Ctrl Pts',(-10.6617258122715,6.60032873136377,
9.69464518252478));
#110450=CARTESIAN_POINT('Ctrl Pts',(-10.6654343566185,6.60055708403641,
9.69652519804279));
#110451=CARTESIAN_POINT('Ctrl Pts',(-10.6691246179307,6.60078577311935,
9.69841570110886));
#110452=CARTESIAN_POINT('Ctrl Pts',(-10.6800603018615,6.60146770675667,
9.70407679641653));
#110453=CARTESIAN_POINT('Ctrl Pts',(-10.6872821259072,6.60192359970746,
9.7078923276443));
#110454=CARTESIAN_POINT('Ctrl Pts',(-10.7039030469933,6.60298505265313,
9.71685248043823));
#110455=CARTESIAN_POINT('Ctrl Pts',(-10.7132782552238,6.60359291536704,
9.72204022965949));
#110456=CARTESIAN_POINT('Ctrl Pts',(-10.7447389593693,6.60566164121148,
9.73990296342047));
#110457=CARTESIAN_POINT('Ctrl Pts',(-10.7665495665393,6.60714440722668,
9.75305080578825));
#110458=CARTESIAN_POINT('Ctrl Pts',(-10.8592216606337,6.61362307637913,
9.81226562251631));
#110459=CARTESIAN_POINT('Ctrl Pts',(-10.9263619093737,6.61876885787463,
9.86385368610624));
#110460=CARTESIAN_POINT('Ctrl Pts',(-11.0502770203702,6.62879998993099,
9.97739008166031));
#110461=CARTESIAN_POINT('Ctrl Pts',(-11.106939806136,6.63366808543925,10.0390105451841));
#110462=CARTESIAN_POINT('Ctrl Pts',(-11.1654265735219,6.63898511210841,
10.1146983048499));
#110463=CARTESIAN_POINT('Ctrl Pts',(-11.1726947627775,6.6396520585584,10.124348702223));
#110464=CARTESIAN_POINT('Ctrl Pts',(-11.1843666526428,6.64073359858019,
10.1402521637163));
#110465=CARTESIAN_POINT('Ctrl Pts',(-11.188842204727,6.64115093218281,10.1464515683117));
#110466=CARTESIAN_POINT('Ctrl Pts',(-11.1967720803589,6.64189520404111,
10.1576191794491));
#110467=CARTESIAN_POINT('Ctrl Pts',(-11.2002445405426,6.64222282544031,
10.1625742399626));
#110468=CARTESIAN_POINT('Ctrl Pts',(-11.2075535311362,6.64291613857872,
10.173142729415));
#110469=CARTESIAN_POINT('Ctrl Pts',(-11.211381882382,6.64328151864185,10.1787616584449));
#110470=CARTESIAN_POINT('Ctrl Pts',(-11.2215621078048,6.64425931265827,
10.1939294154844));
#110471=CARTESIAN_POINT('Ctrl Pts',(-11.2278412002845,6.64486902591594,
10.2035266688422));
#110472=CARTESIAN_POINT('Ctrl Pts',(-11.2594444600442,6.64797371384926,
10.2530926193604));
#110473=CARTESIAN_POINT('Ctrl Pts',(-11.2829335812133,6.65040155593496,
10.2942004656664));
#110474=CARTESIAN_POINT('Ctrl Pts',(-11.3533353981179,6.65820302020536,
10.432579542871));
#110475=CARTESIAN_POINT('Ctrl Pts',(-11.3914843664654,6.66331834433958,
10.5338959229662));
#110476=CARTESIAN_POINT('Ctrl Pts',(-11.4251962124842,6.67007609535568,
10.6661399063797));
#110477=CARTESIAN_POINT('Ctrl Pts',(-11.4314355274829,6.6715056956944,10.6939950921619));
#110478=CARTESIAN_POINT('Ctrl Pts',(-11.4418852528145,6.67431859535422,
10.7480076446833));
#110479=CARTESIAN_POINT('Ctrl Pts',(-11.4462076672111,6.67569726484906,
10.7741317993417));
#110480=CARTESIAN_POINT('Ctrl Pts',(-11.4507306035821,6.67746899546247,
10.8069776493351));
#110481=CARTESIAN_POINT('Ctrl Pts',(-11.4515968819988,6.67782838025732,
10.8136041824377));
#110482=CARTESIAN_POINT('Ctrl Pts',(-11.4528951229609,6.67840065201192,
10.8240934418338));
#110483=CARTESIAN_POINT('Ctrl Pts',(-11.4533571447579,6.67861191597662,
10.827952435071));
#110484=CARTESIAN_POINT('Ctrl Pts',(-11.4541860066022,6.67900557207377,
10.8351171015171));
#110485=CARTESIAN_POINT('Ctrl Pts',(-11.4545569545076,6.67918773591917,
10.8384222250234));
#110486=CARTESIAN_POINT('Ctrl Pts',(-11.4552760619228,6.67955318959257,
10.845032649447));
#110487=CARTESIAN_POINT('Ctrl Pts',(-11.4556242327026,6.67973647327445,
10.8483379122315));
#110488=CARTESIAN_POINT('Ctrl Pts',(-11.456401637062,6.68016077410182,10.8559673496354));
#110489=CARTESIAN_POINT('Ctrl Pts',(-11.4568228741368,6.68040221252141,
10.8602922863916));
#110490=CARTESIAN_POINT('Ctrl Pts',(-11.4578648961559,6.68103060637719,
10.8715084846775));
#110491=CARTESIAN_POINT('Ctrl Pts',(-11.4584560753435,6.68141903918606,
10.878402312484));
#110492=CARTESIAN_POINT('Ctrl Pts',(-11.4619768989559,6.68395562947491,
10.9231876055651));
#110493=CARTESIAN_POINT('Ctrl Pts',(-11.4634782570727,6.68616795268897,
10.9611737192897));
#110494=CARTESIAN_POINT('Ctrl Pts',(-11.4634997655431,6.68841487495421,
10.9991715947004));
#110495=CARTESIAN_POINT('Origin',(-10.,3.5,11.));
#110496=CARTESIAN_POINT('',(-11.46349956662,7.25939591416304,10.9995759468747));
#110497=CARTESIAN_POINT('',(-11.4634999176128,7.19062697240001,10.9995089322141));
#110498=CARTESIAN_POINT('',(-11.4635,3.5,11.));
#110499=CARTESIAN_POINT('Ctrl Pts',(-11.4634999385744,7.25939527076697,
10.9995759803274));
#110500=CARTESIAN_POINT('Ctrl Pts',(-11.4634561086694,7.25150470342572,
10.8482974725707));
#110501=CARTESIAN_POINT('Ctrl Pts',(-11.4399600529956,7.24445648298535,
10.6979562985416));
#110502=CARTESIAN_POINT('Ctrl Pts',(-11.3841873946785,7.23534112134271,
10.5236997451596));
#110503=CARTESIAN_POINT('Ctrl Pts',(-11.3735491355026,7.23373847646734,
10.4938387263501));
#110504=CARTESIAN_POINT('Ctrl Pts',(-11.3551746365144,7.23113287186272,
10.447119638399));
#110505=CARTESIAN_POINT('Ctrl Pts',(-11.3480726623283,7.23015785665119,
10.4300219090754));
#110506=CARTESIAN_POINT('Ctrl Pts',(-11.3383478102608,7.22885718813728,
10.4078088976472));
#110507=CARTESIAN_POINT('Ctrl Pts',(-11.3360161543885,7.22854775148114,
10.4025671619657));
#110508=CARTESIAN_POINT('Ctrl Pts',(-11.3321557556474,7.22803911636505,
10.3940243187581));
#110509=CARTESIAN_POINT('Ctrl Pts',(-11.3306453944295,7.22784100989487,
10.3907149129892));
#110510=CARTESIAN_POINT('Ctrl Pts',(-11.3276790142784,7.22745358865733,
10.3842788120689));
#110511=CARTESIAN_POINT('Ctrl Pts',(-11.3262242586613,7.22726434936961,
10.3811515846654));
#110512=CARTESIAN_POINT('Ctrl Pts',(-11.3226303757709,7.22679873971834,
10.3734968366618));
#110513=CARTESIAN_POINT('Ctrl Pts',(-11.320479048771,7.22652163921353,10.3689751155117));
#110514=CARTESIAN_POINT('Ctrl Pts',(-11.3130836741868,7.22557474941248,
10.3536347329811));
#110515=CARTESIAN_POINT('Ctrl Pts',(-11.3077296724927,7.224898739375,10.3428699682646));
#110516=CARTESIAN_POINT('Ctrl Pts',(-11.2678372935943,7.21993582069678,
10.2650809826297));
#110517=CARTESIAN_POINT('Ctrl Pts',(-11.2283001042013,7.21541344708913,
10.2007538992219));
#110518=CARTESIAN_POINT('Ctrl Pts',(-11.1457918060659,7.20696771984628,
10.0871932804422));
#110519=CARTESIAN_POINT('Ctrl Pts',(-11.1041344827091,7.20305654393707,
10.0372212746924));
#110520=CARTESIAN_POINT('Ctrl Pts',(-11.0319028578451,7.19690479936103,
9.96145083724244));
#110521=CARTESIAN_POINT('Ctrl Pts',(-11.0033548208978,7.19460793576585,
9.93384459040236));
#110522=CARTESIAN_POINT('Ctrl Pts',(-10.9606938758796,7.19136812140267,
9.89582434566826));
#110523=CARTESIAN_POINT('Ctrl Pts',(-10.9474630890683,7.19038810169876,
9.88445066004649));
#110524=CARTESIAN_POINT('Ctrl Pts',(-10.9264594044912,7.18887028638219,
9.86703840822607));
#110525=CARTESIAN_POINT('Ctrl Pts',(-10.9188238958734,7.18832610510823,
9.86083730241024));
#110526=CARTESIAN_POINT('Ctrl Pts',(-10.9045643329139,7.1873236584229,9.8494931858813));
#110527=CARTESIAN_POINT('Ctrl Pts',(-10.8979575111157,7.18686458014011,
9.84432925362347));
#110528=CARTESIAN_POINT('Ctrl Pts',(-10.8864861825065,7.1860766067585,9.83552096007787));
#110529=CARTESIAN_POINT('Ctrl Pts',(-10.8816427316178,7.1857466648648,9.83184963231519));
#110530=CARTESIAN_POINT('Ctrl Pts',(-10.8718309782948,7.18508375479992,
9.82450812569221));
#110531=CARTESIAN_POINT('Ctrl Pts',(-10.8668620287145,7.18475083177108,
9.82083901605691));
#110532=CARTESIAN_POINT('Ctrl Pts',(-10.8558423987814,7.18401857124539,
9.81280934123141));
#110533=CARTESIAN_POINT('Ctrl Pts',(-10.8497812929292,7.18361979284818,
9.80846333301115));
#110534=CARTESIAN_POINT('Ctrl Pts',(-10.8291434521048,7.18227515480108,
9.79390290988805));
#110535=CARTESIAN_POINT('Ctrl Pts',(-10.8144133893468,7.18133751360094,
9.78390793026951));
#110536=CARTESIAN_POINT('Ctrl Pts',(-10.7077425758979,7.17469494872909,
9.71433488179106));
#110537=CARTESIAN_POINT('Ctrl Pts',(-10.6095516740272,7.16938695966699,
9.66497806325042));
#110538=CARTESIAN_POINT('Ctrl Pts',(-10.4488431486929,7.16104624644524,
9.60566000258238));
#110539=CARTESIAN_POINT('Ctrl Pts',(-10.3896304517091,7.15803181718587,
9.58796907139328));
#110540=CARTESIAN_POINT('Ctrl Pts',(-10.3110681493146,7.15391800909917,
9.56981608390005));
#110541=CARTESIAN_POINT('Ctrl Pts',(-10.2925742164616,7.15294134526078,
9.56591851741472));
#110542=CARTESIAN_POINT('Ctrl Pts',(-10.2614910867608,7.15127848920049,
9.55999406322988));
#110543=CARTESIAN_POINT('Ctrl Pts',(-10.2489411941998,7.15060132411581,
9.55777153457303));
#110544=CARTESIAN_POINT('Ctrl Pts',(-10.2314508067843,7.14964759595845,
9.5549091505766));
#110545=CARTESIAN_POINT('Ctrl Pts',(-10.2265333111016,7.14937835771907,
9.55413012461104));
#110546=CARTESIAN_POINT('Ctrl Pts',(-10.2181739900313,7.14891867645609,
9.55284953877119));
#110547=CARTESIAN_POINT('Ctrl Pts',(-10.2147341254406,7.14872894279279,
9.55233512077534));
#110548=CARTESIAN_POINT('Ctrl Pts',(-10.208114586624,7.14836267053087,9.55136930767716));
#110549=CARTESIAN_POINT('Ctrl Pts',(-10.2049352204108,7.14818624150505,
9.55091611045767));
#110550=CARTESIAN_POINT('Ctrl Pts',(-10.1972881264566,7.14776071097816,
9.5498517388271));
#110551=CARTESIAN_POINT('Ctrl Pts',(-10.1928190432518,7.147511057857,9.54925074541061));
#110552=CARTESIAN_POINT('Ctrl Pts',(-10.1764365195446,7.14659253395523,
9.54712469189819));
#110553=CARTESIAN_POINT('Ctrl Pts',(-10.1645075306806,7.14591720873392,
9.5457256930597));
#110554=CARTESIAN_POINT('Ctrl Pts',(-10.0771011463043,7.14092809384779,
9.53656406754474));
#110555=CARTESIAN_POINT('Ctrl Pts',(-10.0011444510717,7.13637582896727,
9.53453553545142));
#110556=CARTESIAN_POINT('Ctrl Pts',(-9.85963515868684,7.12785014603256,
9.54176008105266));
#110557=CARTESIAN_POINT('Ctrl Pts',(-9.79418766767498,7.1238888756256,9.54954898341644));
#110558=CARTESIAN_POINT('Ctrl Pts',(-9.69126761459346,7.1177406879781,9.56890644995313));
#110559=CARTESIAN_POINT('Ctrl Pts',(-9.65335051137601,7.11549252160925,
9.57761505620045));
#110560=CARTESIAN_POINT('Ctrl Pts',(-9.59922353067405,7.11231391154806,
9.59234009616497));
#110561=CARTESIAN_POINT('Ctrl Pts',(-9.58270456515201,7.11134793613943,
9.59714835493381));
#110562=CARTESIAN_POINT('Ctrl Pts',(-9.55318833705484,7.10962911367722,
9.60630731438806));
#110563=CARTESIAN_POINT('Ctrl Pts',(-9.54016033078031,7.10887299860853,
9.61055138254992));
#110564=CARTESIAN_POINT('Ctrl Pts',(-9.52030725867447,7.1077243897284,9.61732864689626));
#110565=CARTESIAN_POINT('Ctrl Pts',(-9.51343853700391,7.1073276639999,9.61973077185539));
#110566=CARTESIAN_POINT('Ctrl Pts',(-9.50097055186475,7.10660867387954,
9.62419570376299));
#110567=CARTESIAN_POINT('Ctrl Pts',(-9.49536547393588,7.10628586832316,
9.62624170677365));
#110568=CARTESIAN_POINT('Ctrl Pts',(-9.48316956817425,7.10558434642002,
9.63077825259796));
#110569=CARTESIAN_POINT('Ctrl Pts',(-9.47658387604776,7.1052060815214,9.63328223382947));
#110570=CARTESIAN_POINT('Ctrl Pts',(-9.45857844210802,7.10417326286533,
9.64027741026515));
#110571=CARTESIAN_POINT('Ctrl Pts',(-9.44719656239041,7.10352190123299,
9.64486487912139));
#110572=CARTESIAN_POINT('Ctrl Pts',(-9.38581513487595,7.10001556471446,
9.67050673599305));
#110573=CARTESIAN_POINT('Ctrl Pts',(-9.33695560333863,7.09724990139249,
9.69418671668403));
#110574=CARTESIAN_POINT('Ctrl Pts',(-9.19811296580911,7.08932858261299,
9.77128480758423));
#110575=CARTESIAN_POINT('Ctrl Pts',(-9.11241339409874,7.08437483904717,
9.83168818786137));
#110576=CARTESIAN_POINT('Ctrl Pts',(-8.99762119814698,7.0767718444092,9.93257339558022));
#110577=CARTESIAN_POINT('Ctrl Pts',(-8.96296141032011,7.07431772668654,
9.96621427529028));
#110578=CARTESIAN_POINT('Ctrl Pts',(-8.92484910683395,7.07134092493417,
10.007054644556));
#110579=CARTESIAN_POINT('Ctrl Pts',(-8.91971123602365,7.07093335276581,
10.0126469205572));
#110580=CARTESIAN_POINT('Ctrl Pts',(-8.91190458021499,7.0703039208405,10.0212778941769));
#110581=CARTESIAN_POINT('Ctrl Pts',(-8.90920440425667,7.07008431725829,
10.0242881724133));
#110582=CARTESIAN_POINT('Ctrl Pts',(-8.90427150190303,7.0696795507079,10.0298336633525));
#110583=CARTESIAN_POINT('Ctrl Pts',(-8.90203504736995,7.06949466681277,
10.0323654488889));
#110584=CARTESIAN_POINT('Ctrl Pts',(-8.89701222562443,7.06907633445715,
10.0380913839395));
#110585=CARTESIAN_POINT('Ctrl Pts',(-8.89423097507864,7.0688425262761,10.041289888092));
#110586=CARTESIAN_POINT('Ctrl Pts',(-8.88710222072903,7.06823773369535,
10.0495604126518));
#110587=CARTESIAN_POINT('Ctrl Pts',(-8.882775526517,7.06786532587704,10.0546501447926));
#110588=CARTESIAN_POINT('Ctrl Pts',(-8.85549418544437,7.06548396301347,
10.0871915841657));
#110589=CARTESIAN_POINT('Ctrl Pts',(-8.8335196466077,7.0634149499355,10.1154459007797));
#110590=CARTESIAN_POINT('Ctrl Pts',(-8.80661239695558,7.06070777093118,
10.1527908515526));
#110591=CARTESIAN_POINT('Ctrl Pts',(-8.80070812818177,7.06010207118817,
10.161169676074));
#110592=CARTESIAN_POINT('Ctrl Pts',(-8.75070097472611,7.05487442462613,
10.2337427761148));
#110593=CARTESIAN_POINT('Ctrl Pts',(-8.71169961706915,7.05014053212184,
10.3013008316306));
#110594=CARTESIAN_POINT('Ctrl Pts',(-8.64614726578373,7.04103579958989,
10.4391891533336));
#110595=CARTESIAN_POINT('Ctrl Pts',(-8.61925720244162,7.03667148529408,
10.5091050196902));
#110596=CARTESIAN_POINT('Ctrl Pts',(-8.59273551887959,7.0314852943699,10.5978122208329));
#110597=CARTESIAN_POINT('Ctrl Pts',(-8.58795347151401,7.03049923058157,
10.6149377065279));
#110598=CARTESIAN_POINT('Ctrl Pts',(-8.58145605961383,7.02908004295298,
10.6399576878742));
#110599=CARTESIAN_POINT('Ctrl Pts',(-8.57949222847651,7.0286390498249,10.6477855028448));
#110600=CARTESIAN_POINT('Ctrl Pts',(-8.57615710186073,7.02786817090244,
10.6615610834613));
#110601=CARTESIAN_POINT('Ctrl Pts',(-8.57475809043128,7.02753741188211,
10.6675018803389));
#110602=CARTESIAN_POINT('Ctrl Pts',(-8.57192813089073,7.02685251183057,
10.6798652156238));
#110603=CARTESIAN_POINT('Ctrl Pts',(-8.57050324911629,7.0264985693548,10.6862890109489));
#110604=CARTESIAN_POINT('Ctrl Pts',(-8.56692270118805,7.02558475392845,
10.702962292976));
#110605=CARTESIAN_POINT('Ctrl Pts',(-8.56483363060761,7.02502698631723,
10.7132257969748));
#110606=CARTESIAN_POINT('Ctrl Pts',(-8.55676932194068,7.02276748046016,
10.755142773298));
#110607=CARTESIAN_POINT('Ctrl Pts',(-8.5517294903422,7.02109497488892,10.786968124971));
#110608=CARTESIAN_POINT('Ctrl Pts',(-8.54446539887284,7.01809587912323,
10.8452309097326));
#110609=CARTESIAN_POINT('Ctrl Pts',(-8.54190162917352,7.01676107180637,
10.8716112413974));
#110610=CARTESIAN_POINT('Ctrl Pts',(-8.53281531177222,7.01025954382913,
11.0017259039225));
#110611=CARTESIAN_POINT('Ctrl Pts',(-8.53663979392552,7.00533426499684,
11.1058745880121));
#110612=CARTESIAN_POINT('Ctrl Pts',(-8.55832350315784,6.99776949338188,
11.2563498356432));
#110613=CARTESIAN_POINT('Ctrl Pts',(-8.56752747361502,6.99532360438646,
11.3035917846686));
#110614=CARTESIAN_POINT('Ctrl Pts',(-8.58085572767398,6.99235614496052,
11.3576581767258));
#110615=CARTESIAN_POINT('Ctrl Pts',(-8.58272931124193,6.99194886756513,
11.3650118175314));
#110616=CARTESIAN_POINT('Ctrl Pts',(-8.58568852138687,6.99131979713757,
11.3762600628425));
#110617=CARTESIAN_POINT('Ctrl Pts',(-8.58673326666128,6.99110025625424,
11.3801654022495));
#110618=CARTESIAN_POINT('Ctrl Pts',(-8.58868072721365,6.99069554841305,
11.3873261842409));
#110619=CARTESIAN_POINT('Ctrl Pts',(-8.5895785447399,6.9905106599599,11.3905828729979));
#110620=CARTESIAN_POINT('Ctrl Pts',(-8.59162865490153,6.99009224469294,
11.397920070209));
#110621=CARTESIAN_POINT('Ctrl Pts',(-8.59278740213968,6.98985835750087,
11.4019986709788));
#110622=CARTESIAN_POINT('Ctrl Pts',(-8.59581868066643,6.98925322639541,
11.4124945581428));
#110623=CARTESIAN_POINT('Ctrl Pts',(-8.59771746681914,6.98888055647306,
11.4189040842209));
#110624=CARTESIAN_POINT('Ctrl Pts',(-8.61008554598533,6.98649380250803,
11.4596271148942));
#110625=CARTESIAN_POINT('Ctrl Pts',(-8.62176893916401,6.98441935680047,
11.493556501585));
#110626=CARTESIAN_POINT('Ctrl Pts',(-8.63825438343233,6.98172661551061,
11.5362642285839));
#110627=CARTESIAN_POINT('Ctrl Pts',(-8.64191661644619,6.98114108217395,
11.5454722402042));
#110628=CARTESIAN_POINT('Ctrl Pts',(-8.64952006408888,6.97995127098647,
11.5640383745218));
#110629=CARTESIAN_POINT('Ctrl Pts',(-8.65346574080428,6.97934691716196,
11.5733941309488));
#110630=CARTESIAN_POINT('Ctrl Pts',(-8.69075804111194,6.97375669615821,
11.6593112677241));
#110631=CARTESIAN_POINT('Ctrl Pts',(-8.73050539330112,6.96868182988944,
11.7329327269284));
#110632=CARTESIAN_POINT('Ctrl Pts',(-8.81017061667026,6.96009761023257,
11.8543698440775));
#110633=CARTESIAN_POINT('Ctrl Pts',(-8.84725980128844,6.95653097920872,
11.9037883067599));
#110634=CARTESIAN_POINT('Ctrl Pts',(-8.89785229536608,6.95218047500992,
11.9629970899625));
#110635=CARTESIAN_POINT('Ctrl Pts',(-8.90854409431341,6.95128662524302,
11.9750984531));
#110636=CARTESIAN_POINT('Ctrl Pts',(-8.92467187259044,6.94997502970096,
11.9927547428533));
#110637=CARTESIAN_POINT('Ctrl Pts',(-8.9299550951268,6.94955099619432,11.9984470270628));
#110638=CARTESIAN_POINT('Ctrl Pts',(-8.93944272463706,6.94879935740589,
12.0085074450352));
#110639=CARTESIAN_POINT('Ctrl Pts',(-8.94362940555503,6.94847101506171,
12.0128919832518));
#110640=CARTESIAN_POINT('Ctrl Pts',(-8.95251853547159,6.94778081797124,
12.0220861381685));
#110641=CARTESIAN_POINT('Ctrl Pts',(-8.95722715115275,6.9474192392453,12.0268896143853));
#110642=CARTESIAN_POINT('Ctrl Pts',(-8.96982290626582,6.94646248640562,
12.0395631508876));
#110643=CARTESIAN_POINT('Ctrl Pts',(-8.9777671699631,6.94586981145631,12.0473759780709));
#110644=CARTESIAN_POINT('Ctrl Pts',(-9.01333924513926,6.94326197701084,
12.0815692148801));
#110645=CARTESIAN_POINT('Ctrl Pts',(-9.04190557041562,6.94128898570957,
12.1069538353413));
#110646=CARTESIAN_POINT('Ctrl Pts',(-9.18116015542493,6.93215331342288,
12.2212641601196));
#110647=CARTESIAN_POINT('Ctrl Pts',(-9.3033910509643,6.92557886826708,12.2948798789891));
#110648=CARTESIAN_POINT('Ctrl Pts',(-9.45329318071163,6.91731816083869,
12.3577069927749));
#110649=CARTESIAN_POINT('Ctrl Pts',(-9.47245752622063,6.91625706703595,
12.3652675531894));
#110650=CARTESIAN_POINT('Ctrl Pts',(-9.5045180395607,6.91446398585834,12.3771399902268));
#110651=CARTESIAN_POINT('Ctrl Pts',(-9.51732652311142,6.91374295824377,
12.3816812998727));
#110652=CARTESIAN_POINT('Ctrl Pts',(-9.53503155485982,6.91273753847133,
12.3876824798256));
#110653=CARTESIAN_POINT('Ctrl Pts',(-9.53987565486393,6.91246156149984,
12.3892961906095));
#110654=CARTESIAN_POINT('Ctrl Pts',(-9.54805713623244,6.91199378993519,
12.3919741981477));
#110655=CARTESIAN_POINT('Ctrl Pts',(-9.55139012510344,6.91180276582628,
12.3930519373962));
#110656=CARTESIAN_POINT('Ctrl Pts',(-9.55775998119547,6.91143675309572,
12.395086432301));
#110657=CARTESIAN_POINT('Ctrl Pts',(-9.56079615112852,6.91126189241858,
12.3960452594954));
#110658=CARTESIAN_POINT('Ctrl Pts',(-9.56803998918668,6.91084378573381,
12.3983069051391));
#110659=CARTESIAN_POINT('Ctrl Pts',(-9.57225043281855,6.91060002875152,
12.3996006425614));
#110660=CARTESIAN_POINT('Ctrl Pts',(-9.58725552499744,6.90972888388539,
12.4041372045183));
#110661=CARTESIAN_POINT('Ctrl Pts',(-9.59808144697446,6.90909586953382,
12.4072742276474));
#110662=CARTESIAN_POINT('Ctrl Pts',(-9.70419116677746,6.90285494222188,
12.4366973671414));
#110663=CARTESIAN_POINT('Ctrl Pts',(-9.80186423727243,6.8968421742921,12.4533898352714));
#110664=CARTESIAN_POINT('Ctrl Pts',(-9.91638197007264,6.88994948645016,
12.4611963458517));
#110665=CARTESIAN_POINT('Ctrl Pts',(-9.93231448413549,6.88899350107593,
12.4620210044104));
#110666=CARTESIAN_POINT('Ctrl Pts',(-10.0052699898543,6.88463431937991,
12.4646019850538));
#110667=CARTESIAN_POINT('Ctrl Pts',(-10.062355610644,6.88127720938945,12.4632838156791));
#110668=CARTESIAN_POINT('Ctrl Pts',(-10.1524638379184,6.87610293892573,
12.4559187366513));
#110669=CARTESIAN_POINT('Ctrl Pts',(-10.1856038309028,6.87422631486022,
12.4520661348605));
#110670=CARTESIAN_POINT('Ctrl Pts',(-10.2287134318626,6.87181886743842,
12.4455543355882));
#110671=CARTESIAN_POINT('Ctrl Pts',(-10.2388254674448,6.87125657780794,
12.4439181329313));
#110672=CARTESIAN_POINT('Ctrl Pts',(-10.2553541109633,6.87034128615449,
12.4410652876855));
#110673=CARTESIAN_POINT('Ctrl Pts',(-10.2617811125795,6.86998632774579,
12.4399116418629));
#110674=CARTESIAN_POINT('Ctrl Pts',(-10.2742190242701,6.86930115751591,
12.4375930095948));
#110675=CARTESIAN_POINT('Ctrl Pts',(-10.2802307584783,6.86897078994783,
12.4364332417742));
#110676=CARTESIAN_POINT('Ctrl Pts',(-10.2941326693982,6.86820861189812,
12.4336607252557));
#110677=CARTESIAN_POINT('Ctrl Pts',(-10.3020172058147,6.86777767454006,
12.4320205002849));
#110678=CARTESIAN_POINT('Ctrl Pts',(-10.3276498940332,6.86638077003142,
12.4264669972027));
#110679=CARTESIAN_POINT('Ctrl Pts',(-10.3453391321258,6.8654231692313,12.4222881104743));
#110680=CARTESIAN_POINT('Ctrl Pts',(-10.469047016273,6.85876269919855,12.3906193616769));
#110681=CARTESIAN_POINT('Ctrl Pts',(-10.5717632578918,6.85345611235032,
12.3516347713466));
#110682=CARTESIAN_POINT('Ctrl Pts',(-10.724107995675,6.84511572138444,12.2733087085237));
#110683=CARTESIAN_POINT('Ctrl Pts',(-10.7771938259892,6.84210007925424,
12.2416183972237));
#110684=CARTESIAN_POINT('Ctrl Pts',(-10.8437015816534,6.83798473529962,
12.1959754356813));
#110685=CARTESIAN_POINT('Ctrl Pts',(-10.8590786120089,6.83700784214176,
12.1849782628524));
#110686=CARTESIAN_POINT('Ctrl Pts',(-10.8844607448046,6.83534463086534,
12.1660720117431));
#110687=CARTESIAN_POINT('Ctrl Pts',(-10.8945835265429,6.83466734487077,
12.1583242369763));
#110688=CARTESIAN_POINT('Ctrl Pts',(-10.9085175908693,6.83371347387333,
12.1473677831018));
#110689=CARTESIAN_POINT('Ctrl Pts',(-10.912415924773,6.83344421660625,12.1442701697531));
#110690=CARTESIAN_POINT('Ctrl Pts',(-10.9190104131131,6.83298451260617,
12.1389750692726));
#110691=CARTESIAN_POINT('Ctrl Pts',(-10.9217147199965,6.83279477540441,
12.1367877209861));
#110692=CARTESIAN_POINT('Ctrl Pts',(-10.9269008966038,6.83242850431745,
12.1325622681523));
#110693=CARTESIAN_POINT('Ctrl Pts',(-10.9293838868846,6.83225208005877,
12.1305256095097));
#110694=CARTESIAN_POINT('Ctrl Pts',(-10.9353369711805,6.83182657188449,
12.1256097599674));
#110695=CARTESIAN_POINT('Ctrl Pts',(-10.9388004799934,6.83157693647195,
12.1227226901884));
#110696=CARTESIAN_POINT('Ctrl Pts',(-10.9514388586231,6.83065856518419,
12.1120883718689));
#110697=CARTESIAN_POINT('Ctrl Pts',(-10.96053137352,6.82998337766097,12.104244497471));
#110698=CARTESIAN_POINT('Ctrl Pts',(-11.0265147817711,6.82498294556569,
12.0458907420029));
#110699=CARTESIAN_POINT('Ctrl Pts',(-11.0794823117569,6.82041795675947,
11.9911286816822));
#110700=CARTESIAN_POINT('Ctrl Pts',(-11.2031723763488,6.80873744319932,
11.841514216691));
#110701=CARTESIAN_POINT('Ctrl Pts',(-11.2671232508944,6.80168190025662,
11.7417398203432));
#110702=CARTESIAN_POINT('Ctrl Pts',(-11.3253539387938,6.79419054166257,
11.6209076177256));
#110703=CARTESIAN_POINT('Ctrl Pts',(-11.3320770638389,6.79330304820856,
11.6063497814011));
#110704=CARTESIAN_POINT('Ctrl Pts',(-11.3416907887255,6.79199891377795,
11.5846007634169));
#110705=CARTESIAN_POINT('Ctrl Pts',(-11.3447655545249,6.79157608802882,
11.5774927113951));
#110706=CARTESIAN_POINT('Ctrl Pts',(-11.3501454195933,6.79082579901812,
11.5647798831403));
#110707=CARTESIAN_POINT('Ctrl Pts',(-11.3524723840587,6.79049760832443,
11.5591846048779));
#110708=CARTESIAN_POINT('Ctrl Pts',(-11.3573133149562,6.78980693153303,
11.5473373901969));
#110709=CARTESIAN_POINT('Ctrl Pts',(-11.3598189957754,6.78944472753037,
11.541082206751));
#110710=CARTESIAN_POINT('Ctrl Pts',(-11.3663729330044,6.78848446538371,
11.5243878497351));
#110711=CARTESIAN_POINT('Ctrl Pts',(-11.3703447892138,6.78788893975489,
11.513919037311));
#110712=CARTESIAN_POINT('Ctrl Pts',(-11.3874997146924,6.78525332632198,
11.4670895245127));
#110713=CARTESIAN_POINT('Ctrl Pts',(-11.399359055975,6.78325653638187,11.430258809936));
#110714=CARTESIAN_POINT('Ctrl Pts',(-11.4139271728694,6.78050716281447,
11.378000840298));
#110715=CARTESIAN_POINT('Ctrl Pts',(-11.4178687848717,6.77972408663825,
11.3629363738974));
#110716=CARTESIAN_POINT('Ctrl Pts',(-11.4494951677349,6.7730742334028,11.233673592005));
#110717=CARTESIAN_POINT('Ctrl Pts',(-11.4635714444221,6.76755111586632,
11.1165980425647));
#110718=CARTESIAN_POINT('Ctrl Pts',(-11.4634997273561,6.7616401361251,10.9991066755872));
#110719=CARTESIAN_POINT('Ctrl Pts',(-11.4634997643993,6.68841475560911,
10.9991695764457));
#110720=CARTESIAN_POINT('Ctrl Pts',(-11.4635596206349,6.69465254772556,
11.1046574160703));
#110721=CARTESIAN_POINT('Ctrl Pts',(-11.4522146970128,6.70110730256879,
11.209849775773));
#110722=CARTESIAN_POINT('Ctrl Pts',(-11.4211342010557,6.70965114077867,
11.351849419943));
#110723=CARTESIAN_POINT('Ctrl Pts',(-11.4110261863502,6.71195754463812,
11.3904176223993));
#110724=CARTESIAN_POINT('Ctrl Pts',(-11.3917335017398,6.71569346635609,
11.4534178352096));
#110725=CARTESIAN_POINT('Ctrl Pts',(-11.3834482721036,6.7171491391733,11.4781013206337));
#110726=CARTESIAN_POINT('Ctrl Pts',(-11.3712930632926,6.71909954638602,
11.5113465275355));
#110727=CARTESIAN_POINT('Ctrl Pts',(-11.3679931312654,6.71961273076903,
11.5201103105693));
#110728=CARTESIAN_POINT('Ctrl Pts',(-11.3623169939192,6.72046890608534,
11.534756859286));
#110729=CARTESIAN_POINT('Ctrl Pts',(-11.3599862720804,6.72081338656028,
11.540656852341));
#110730=CARTESIAN_POINT('Ctrl Pts',(-11.3553161936784,6.72148995799427,
11.5522573952519));
#110731=CARTESIAN_POINT('Ctrl Pts',(-11.3529790527169,6.72182211386263,
11.5579586901893));
#110732=CARTESIAN_POINT('Ctrl Pts',(-11.3477580431241,6.72255026285652,
11.57046926897));
#110733=CARTESIAN_POINT('Ctrl Pts',(-11.3448584222279,6.72294572077665,
11.5772718220309));
#110734=CARTESIAN_POINT('Ctrl Pts',(-11.3344909228821,6.72432906175696,
11.6010919935522));
#110735=CARTESIAN_POINT('Ctrl Pts',(-11.3267504221815,6.72530779114599,
11.6179894545839));
#110736=CARTESIAN_POINT('Ctrl Pts',(-11.2766454447452,6.73132937679715,
11.722084684804));
#110737=CARTESIAN_POINT('Ctrl Pts',(-11.2260258169689,6.73607248076768,
11.8050421951749));
#110738=CARTESIAN_POINT('Ctrl Pts',(-11.1261687554777,6.74413250657181,
11.9371718856615));
#110739=CARTESIAN_POINT('Ctrl Pts',(-11.0809664536226,6.74745833987433,
11.9889679656975));
#110740=CARTESIAN_POINT('Ctrl Pts',(-11.0167360987691,6.75205032575716,
12.0528826982318));
#110741=CARTESIAN_POINT('Ctrl Pts',(-11.0008275543021,6.75317835845129,
12.0680161016339));
#110742=CARTESIAN_POINT('Ctrl Pts',(-10.9774301987005,6.75483448910199,
12.0892915056516));
#110743=CARTESIAN_POINT('Ctrl Pts',(-10.9702108924955,6.75534511029105,
12.0957265136211));
#110744=CARTESIAN_POINT('Ctrl Pts',(-10.9573211899641,6.75625721875792,
12.1069886333773));
#110745=CARTESIAN_POINT('Ctrl Pts',(-10.9516766695869,6.75665677925589,
12.1118449564195));
#110746=CARTESIAN_POINT('Ctrl Pts',(-10.9429141605765,6.75727770326757,
12.1192682628368));
#110747=CARTESIAN_POINT('Ctrl Pts',(-10.9398221121522,6.75749693334687,
12.1218658365089));
#110748=CARTESIAN_POINT('Ctrl Pts',(-10.9367033181617,6.75771822830531,
12.1244639363637));
#110749=CARTESIAN_POINT('Ctrl Pts',(-10.936687245989,6.75771936871561,12.1244773246442));
#110750=CARTESIAN_POINT('Ctrl Pts',(-10.9366549958661,6.75772165705071,
12.124504188148));
#110751=CARTESIAN_POINT('Ctrl Pts',(-10.9366388180197,6.75772280496821,
12.124517663277));
#110752=CARTESIAN_POINT('Ctrl Pts',(-10.936606354723,6.75772510844752,12.1245447019757));
#110753=CARTESIAN_POINT('Ctrl Pts',(-10.9365900693055,6.75772626400706,
12.1245582655103));
#110754=CARTESIAN_POINT('Ctrl Pts',(-10.936560560025,6.75772835789669,12.1245828416359));
#110755=CARTESIAN_POINT('Ctrl Pts',(-10.9365473361729,6.75772929622445,
12.124593854422));
#110756=CARTESIAN_POINT('Ctrl Pts',(-10.9365204687927,6.75773120266519,
12.1246162286965));
#110757=CARTESIAN_POINT('Ctrl Pts',(-10.9365068251932,6.75773217078344,
12.124627590219));
#110758=CARTESIAN_POINT('Ctrl Pts',(-10.9338974646006,6.75791732559571,
12.126800419463));
#110759=CARTESIAN_POINT('Ctrl Pts',(-10.931294353513,6.75810216095389,12.1289528272895));
#110760=CARTESIAN_POINT('Ctrl Pts',(-10.925434312204,6.75851853404814,12.1337641999434));
#110761=CARTESIAN_POINT('Ctrl Pts',(-10.9221733865764,6.75875041506592,
12.1364181323202));
#110762=CARTESIAN_POINT('Ctrl Pts',(-10.9125918148215,6.75943216748588,
12.1441477803177));
#110763=CARTESIAN_POINT('Ctrl Pts',(-10.9062404811443,6.75988460760571,
12.1491849929213));
#110764=CARTESIAN_POINT('Ctrl Pts',(-10.8512860636664,6.76380139628221,
12.1920301981794));
#110765=CARTESIAN_POINT('Ctrl Pts',(-10.800387720404,6.76744073829635,12.2267852145416));
#110766=CARTESIAN_POINT('Ctrl Pts',(-10.6974610577549,6.77460959539087,
12.2879294159088));
#110767=CARTESIAN_POINT('Ctrl Pts',(-10.6457371176473,6.77812759376995,
12.3146246050011));
#110768=CARTESIAN_POINT('Ctrl Pts',(-10.5404023784224,6.78500663497827,
12.361268391505));
#110769=CARTESIAN_POINT('Ctrl Pts',(-10.4869332522373,6.78836355042131,
12.3812977130133));
#110770=CARTESIAN_POINT('Ctrl Pts',(-10.400564024567,6.79353766959075,12.4080103268243));
#110771=CARTESIAN_POINT('Ctrl Pts',(-10.3683718262633,6.79541432398389,
12.4167734710581));
#110772=CARTESIAN_POINT('Ctrl Pts',(-10.325934941767,6.79782190304961,12.426780859836));
#110773=CARTESIAN_POINT('Ctrl Pts',(-10.3159389462908,6.79838429359283,
12.4290275707402));
#110774=CARTESIAN_POINT('Ctrl Pts',(-10.2995331075555,6.79929977277371,
12.4325344057825));
#110775=CARTESIAN_POINT('Ctrl Pts',(-10.2931370762307,6.79965481830326,
12.433856883629));
#110776=CARTESIAN_POINT('Ctrl Pts',(-10.2807267349852,6.8003401739254,12.436336401126));
#110777=CARTESIAN_POINT('Ctrl Pts',(-10.2747136029402,6.80067063971098,
12.4374985895158));
#110778=CARTESIAN_POINT('Ctrl Pts',(-10.2607742176017,6.80143307072447,
12.440102064692));
#110779=CARTESIAN_POINT('Ctrl Pts',(-10.2528429650155,6.80186416204719,
12.441515725838));
#110780=CARTESIAN_POINT('Ctrl Pts',(-10.226973677596,6.80326169070453,12.4459065747587));
#110781=CARTESIAN_POINT('Ctrl Pts',(-10.2089913885507,6.80421975292176,
12.4486150320302));
#110782=CARTESIAN_POINT('Ctrl Pts',(-10.0825181581231,6.81087316484412,
12.465260021753));
#110783=CARTESIAN_POINT('Ctrl Pts',(-9.97281575410425,6.8161734292533,12.4673307946257));
#110784=CARTESIAN_POINT('Ctrl Pts',(-9.80230389895589,6.8245113964672,12.4514046751808));
#110785=CARTESIAN_POINT('Ctrl Pts',(-9.74113952392938,6.82753142975883,
12.4417522538084));
#110786=CARTESIAN_POINT('Ctrl Pts',(-9.66230781691713,6.8316523822422,12.4241328122582));
#110787=CARTESIAN_POINT('Ctrl Pts',(-9.64392431924812,6.83263016155143,
12.4196479599916));
#110788=CARTESIAN_POINT('Ctrl Pts',(-9.61330104291238,6.83429478108754,
12.4115448664109));
#110789=CARTESIAN_POINT('Ctrl Pts',(-9.60101199952237,6.83497257085374,
12.4081205726034));
#110790=CARTESIAN_POINT('Ctrl Pts',(-9.58398886581891,6.8359270814273,12.4031364160519));
#110791=CARTESIAN_POINT('Ctrl Pts',(-9.57921527111767,6.83619646287801,
12.4017122658729));
#110792=CARTESIAN_POINT('Ctrl Pts',(-9.5711201006356,6.83665635430977,12.399252081574));
#110793=CARTESIAN_POINT('Ctrl Pts',(-9.56779472887721,6.83684615392292,
12.398228507537));
#110794=CARTESIAN_POINT('Ctrl Pts',(-9.56140640637077,6.83721252755628,
12.3962371674203));
#110795=CARTESIAN_POINT('Ctrl Pts',(-9.55834295290392,6.83738899176279,
12.3952711637525));
#110796=CARTESIAN_POINT('Ctrl Pts',(-9.55098632490768,6.83781457454818,
12.3929247311359));
#110797=CARTESIAN_POINT('Ctrl Pts',(-9.54669632905109,6.83806424467616,
12.3915345370642));
#110798=CARTESIAN_POINT('Ctrl Pts',(-9.53100804341105,6.83898257141541,
12.3863704261707));
#110799=CARTESIAN_POINT('Ctrl Pts',(-9.51965019969326,6.83965767753596,
12.382476207544));
#110800=CARTESIAN_POINT('Ctrl Pts',(-9.43749790342484,6.84460908323368,
12.3531744196968));
#110801=CARTESIAN_POINT('Ctrl Pts',(-9.36871298539436,6.84911980188319,
12.3224841928642));
#110802=CARTESIAN_POINT('Ctrl Pts',(-9.24580651655688,6.85753112946694,
12.2558651377387));
#110803=CARTESIAN_POINT('Ctrl Pts',(-9.19111270191376,6.86141953108565,
12.221354669168));
#110804=CARTESIAN_POINT('Ctrl Pts',(-9.106487214051,6.86757262508375,12.1597722687065));
#110805=CARTESIAN_POINT('Ctrl Pts',(-9.07507788678621,6.86989140837263,
12.1348816196434));
#110806=CARTESIAN_POINT('Ctrl Pts',(-9.02493341345033,6.87364491368361,
12.0916776329038));
#110807=CARTESIAN_POINT('Ctrl Pts',(-9.00559884993795,6.87510610501388,
12.0740956092025));
#110808=CARTESIAN_POINT('Ctrl Pts',(-8.97997831504608,6.87706260830936,
12.049512240444));
#110809=CARTESIAN_POINT('Ctrl Pts',(-8.97327458908032,6.87757651946804,
12.042954992752));
#110810=CARTESIAN_POINT('Ctrl Pts',(-8.96214034442399,6.87843356710357,
12.0318526348162));
#110811=CARTESIAN_POINT('Ctrl Pts',(-8.95767559755155,6.87877819972474,
12.0273423803525));
#110812=CARTESIAN_POINT('Ctrl Pts',(-8.94893551096392,6.87945481705159,
12.0183975796382));
#110813=CARTESIAN_POINT('Ctrl Pts',(-8.94465855400984,6.87978686854312,
12.0139648042662));
#110814=CARTESIAN_POINT('Ctrl Pts',(-8.93531452630345,6.88051448902606,
12.0041571853324));
#110815=CARTESIAN_POINT('Ctrl Pts',(-8.93025988756787,6.88090952577499,
11.9987706970588));
#110816=CARTESIAN_POINT('Ctrl Pts',(-8.91266695579176,6.88228977137671,
11.9797359713842));
#110817=CARTESIAN_POINT('Ctrl Pts',(-8.90034704673645,6.88326588206761,
11.9658877499353));
#110818=CARTESIAN_POINT('Ctrl Pts',(-8.82312638224702,6.88945519900141,
11.8756944872158));
#110819=CARTESIAN_POINT('Ctrl Pts',(-8.76594740758156,6.89434531659248,
11.7930882446873));
#110820=CARTESIAN_POINT('Ctrl Pts',(-8.6845843936025,6.9025607224419,11.6451533630232));
#110821=CARTESIAN_POINT('Ctrl Pts',(-8.65578693194417,6.90589048998634,
11.5827787862363));
#110822=CARTESIAN_POINT('Ctrl Pts',(-8.62436771221342,6.91040212822098,
11.499870052806));
#110823=CARTESIAN_POINT('Ctrl Pts',(-8.61764887438325,6.91143596060002,
11.4809777128369));
#110824=CARTESIAN_POINT('Ctrl Pts',(-8.60711602913687,6.91318715110918,
11.4493149457309));
#110825=CARTESIAN_POINT('Ctrl Pts',(-8.60308441241113,6.91389419573213,
11.4366193917475));
#110826=CARTESIAN_POINT('Ctrl Pts',(-8.59775927101976,6.91488320898456,
11.4190213136626));
#110827=CARTESIAN_POINT('Ctrl Pts',(-8.59631697546259,6.91515711867852,
11.4141640839236));
#110828=CARTESIAN_POINT('Ctrl Pts',(-8.59392225571318,6.91562243909074,
11.4059431587993));
#110829=CARTESIAN_POINT('Ctrl Pts',(-8.59295659325351,6.91581309847896,
11.4025833111748));
#110830=CARTESIAN_POINT('Ctrl Pts',(-8.59113191896735,6.91617926557934,
11.396147923076));
#110831=CARTESIAN_POINT('Ctrl Pts',(-8.59027092137268,6.91635465099388,
11.3930729845457));
#110832=CARTESIAN_POINT('Ctrl Pts',(-8.58823734789646,6.91677514533323,
11.3857177210569));
#110833=CARTESIAN_POINT('Ctrl Pts',(-8.58707417229547,6.91702077789832,
11.3814348575776));
#110834=CARTESIAN_POINT('Ctrl Pts',(-8.5829733289263,6.91790525209883,11.3660592078926));
#110835=CARTESIAN_POINT('Ctrl Pts',(-8.58014674692846,6.91854994073291,
11.3549375345572));
#110836=CARTESIAN_POINT('Ctrl Pts',(-8.55525738325087,6.92455795344609,
11.2519475240842));
#110837=CARTESIAN_POINT('Ctrl Pts',(-8.54201023192169,6.93029099700035,
11.1581841658445));
#110838=CARTESIAN_POINT('Ctrl Pts',(-8.53479068798238,6.94024356716922,
10.9927497908704));
#110839=CARTESIAN_POINT('Ctrl Pts',(-8.53687350116914,6.94447698571966,
10.9215560388103));
#110840=CARTESIAN_POINT('Ctrl Pts',(-8.54671279346841,6.95003209912957,
10.8255516136567));
#110841=CARTESIAN_POINT('Ctrl Pts',(-8.54995544707844,6.95147470153436,
10.8003832501425));
#110842=CARTESIAN_POINT('Ctrl Pts',(-8.55670221171229,6.95393937509521,
10.7569595892465));
#110843=CARTESIAN_POINT('Ctrl Pts',(-8.55990258801024,6.95497031224033,
10.738663750576));
#110844=CARTESIAN_POINT('Ctrl Pts',(-8.56501931171436,6.95644150215379,
10.7123715498377));
#110845=CARTESIAN_POINT('Ctrl Pts',(-8.56665603741354,6.95689045244903,
10.7043231665356));
#110846=CARTESIAN_POINT('Ctrl Pts',(-8.56963187842073,6.95767058285896,
10.6902955881215));
#110847=CARTESIAN_POINT('Ctrl Pts',(-8.57094094156094,6.95800270038842,
10.6843102867705));
#110848=CARTESIAN_POINT('Ctrl Pts',(-8.57372183266004,6.95868610746447,
10.6719673459886));
#110849=CARTESIAN_POINT('Ctrl Pts',(-8.5751986768565,6.95903723004494,10.6656109688098));
#110850=CARTESIAN_POINT('Ctrl Pts',(-8.57909721034724,6.95993477954982,
10.6493264480112));
#110851=CARTESIAN_POINT('Ctrl Pts',(-8.5815804823815,6.96047924474578,10.639413315821));
#110852=CARTESIAN_POINT('Ctrl Pts',(-8.59179660425233,6.96261678767688,
10.6003704929802));
#110853=CARTESIAN_POINT('Ctrl Pts',(-8.60032488815041,6.96418455636908,
10.5714556132168));
#110854=CARTESIAN_POINT('Ctrl Pts',(-8.64931794281183,6.97221718918085,
10.4224693081286));
#110855=CARTESIAN_POINT('Ctrl Pts',(-8.70435208244871,6.97819022558426,
10.30777233117));
#110856=CARTESIAN_POINT('Ctrl Pts',(-8.80304301882541,6.98714115844825,
10.1561603744093));
#110857=CARTESIAN_POINT('Ctrl Pts',(-8.83511778071097,6.98987959308141,
10.112407985125));
#110858=CARTESIAN_POINT('Ctrl Pts',(-8.87447554567043,6.99318018156136,
10.0645389854067));
#110859=CARTESIAN_POINT('Ctrl Pts',(-8.8794571799808,6.99359696272611,10.0585774644861));
#110860=CARTESIAN_POINT('Ctrl Pts',(-8.88712782911316,6.99423771814737,
10.0495451412914));
#110861=CARTESIAN_POINT('Ctrl Pts',(-8.88978269394219,6.9944593091221,10.046445366176));
#110862=CARTESIAN_POINT('Ctrl Pts',(-8.89465831517188,6.99486601744895,
10.0408006368541));
#110863=CARTESIAN_POINT('Ctrl Pts',(-8.89687494649953,6.99505083821138,
10.0382522293942));
#110864=CARTESIAN_POINT('Ctrl Pts',(-8.90186664747618,6.99546685624546,
10.0325533523104));
#110865=CARTESIAN_POINT('Ctrl Pts',(-8.90464644145621,6.99569839392618,
10.0294071621228));
#110866=CARTESIAN_POINT('Ctrl Pts',(-8.91281440591627,6.9963782185712,10.0202423819891));
#110867=CARTESIAN_POINT('Ctrl Pts',(-8.91823882983352,6.99682905309783,
10.0142564883552));
#110868=CARTESIAN_POINT('Ctrl Pts',(-8.96348025735389,7.00058158956052,
9.96515537879881));
#110869=CARTESIAN_POINT('Ctrl Pts',(-9.00580467843273,7.0040424364072,9.92442996982021));
#110870=CARTESIAN_POINT('Ctrl Pts',(-9.1114479478125,7.01234521357501,9.83435325367631));
#110871=CARTESIAN_POINT('Ctrl Pts',(-9.17661448509601,7.0172096414026,9.78744302364161));
#110872=CARTESIAN_POINT('Ctrl Pts',(-9.28339623073772,7.02457285237012,
9.72317233696785));
#110873=CARTESIAN_POINT('Ctrl Pts',(-9.32252494562857,7.02715903392574,
9.70198693577445));
#110874=CARTESIAN_POINT('Ctrl Pts',(-9.37951920580308,7.03075920786257,
9.67440927619339));
#110875=CARTESIAN_POINT('Ctrl Pts',(-9.39663530535511,7.03181999763212,
9.66653148754627));
#110876=CARTESIAN_POINT('Ctrl Pts',(-9.42738996569851,7.033690238135,9.65308992076048));
#110877=CARTESIAN_POINT('Ctrl Pts',(-9.44096915358737,7.03450384766016,
9.6473974908191));
#110878=CARTESIAN_POINT('Ctrl Pts',(-9.46158021269106,7.03572089436225,
9.63912071040134));
#110879=CARTESIAN_POINT('Ctrl Pts',(-9.46854953560157,7.03612937634007,
9.63638395616053));
#110880=CARTESIAN_POINT('Ctrl Pts',(-9.48117520591405,7.03686398601031,
9.6315375335166));
#110881=CARTESIAN_POINT('Ctrl Pts',(-9.48682415334722,7.03719072644186,
9.62940916351712));
#110882=CARTESIAN_POINT('Ctrl Pts',(-9.49896166157556,7.03788869140184,
9.62492163954777));
#110883=CARTESIAN_POINT('Ctrl Pts',(-9.50545408993207,7.03825955336081,
9.62257331991396));
#110884=CARTESIAN_POINT('Ctrl Pts',(-9.52294108723694,7.03925192986872,
9.61638782823135));
#110885=CARTESIAN_POINT('Ctrl Pts',(-9.53396536051974,7.03987066146595,
9.61263574599982));
#110886=CARTESIAN_POINT('Ctrl Pts',(-9.58811423622361,7.04287760391771,
9.59492460117495));
#110887=CARTESIAN_POINT('Ctrl Pts',(-9.63182852509501,7.04520492408939,
9.58284191736915));
#110888=CARTESIAN_POINT('Ctrl Pts',(-9.78423708315833,7.05306792450703,
9.54824613456444));
#110889=CARTESIAN_POINT('Ctrl Pts',(-9.89487357590158,7.05831780018609,
9.53607028072708));
#110890=CARTESIAN_POINT('Ctrl Pts',(-10.0576063249621,7.06638689262537,
9.53671755362674));
#110891=CARTESIAN_POINT('Ctrl Pts',(-10.1093394153086,7.06900949152846,
9.53967199929593));
#110892=CARTESIAN_POINT('Ctrl Pts',(-10.1684579706689,7.07217796807265,
9.54620720277377));
#110893=CARTESIAN_POINT('Ctrl Pts',(-10.1761072977786,7.07259126945369,
9.54711397566859));
#110894=CARTESIAN_POINT('Ctrl Pts',(-10.1877842264288,7.0732277616402,9.54859176018141));
#110895=CARTESIAN_POINT('Ctrl Pts',(-10.1918173129703,7.07344861767979,
9.54911926336385));
#110896=CARTESIAN_POINT('Ctrl Pts',(-10.1991958458437,7.07385462334052,
9.55011563330863));
#110897=CARTESIAN_POINT('Ctrl Pts',(-10.20254191379,7.074039482978,9.55057927627422));
#110898=CARTESIAN_POINT('Ctrl Pts',(-10.2100583424044,7.07445640792961,
9.55164731519162));
#110899=CARTESIAN_POINT('Ctrl Pts',(-10.2142276849319,7.07468882097198,
9.55225813595572));
#110900=CARTESIAN_POINT('Ctrl Pts',(-10.2264533211291,7.075373565619,9.5541031949715));
#110901=CARTESIAN_POINT('Ctrl Pts',(-10.2345018789549,7.0758284989442,9.55538671609043));
#110902=CARTESIAN_POINT('Ctrl Pts',(-10.3078234901115,7.08000812844363,
9.56770835294022));
#110903=CARTESIAN_POINT('Ctrl Pts',(-10.372282147508,7.08393458619773,9.58309529959434));
#110904=CARTESIAN_POINT('Ctrl Pts',(-10.4875332723914,7.09117586774178,
9.61901580600354));
#110905=CARTESIAN_POINT('Ctrl Pts',(-10.5386490922233,7.09447156149936,
9.63813973876635));
#110906=CARTESIAN_POINT('Ctrl Pts',(-10.6401391103683,7.10108758056456,
9.68272037176556));
#110907=CARTESIAN_POINT('Ctrl Pts',(-10.6903529533229,7.10439947000089,
9.70832764716165));
#110908=CARTESIAN_POINT('Ctrl Pts',(-10.7675153925176,7.10951403615734,
9.753466374741));
#110909=CARTESIAN_POINT('Ctrl Pts',(-10.7954883212648,7.11137446234339,
9.77112875628979));
#110910=CARTESIAN_POINT('Ctrl Pts',(-10.8312877400935,7.11376468940601,
9.79546802277862));
#110911=CARTESIAN_POINT('Ctrl Pts',(-10.8396748426178,7.11432539340569,
9.80129955491489));
#110912=CARTESIAN_POINT('Ctrl Pts',(-10.8533180527149,7.11523883469738,
9.81099910781346));
#110913=CARTESIAN_POINT('Ctrl Pts',(-10.8586104666825,7.11559351216091,
9.81481525105749));
#110914=CARTESIAN_POINT('Ctrl Pts',(-10.8688229835966,7.11627864218418,
9.82228338980021));
#110915=CARTESIAN_POINT('Ctrl Pts',(-10.8737460130215,7.1166092466612,9.82593113614986));
#110916=CARTESIAN_POINT('Ctrl Pts',(-10.8851019019041,7.11737269581499,
9.83445633246428));
#110917=CARTESIAN_POINT('Ctrl Pts',(-10.8915176356738,7.1178046591728,9.83935633095636));
#110918=CARTESIAN_POINT('Ctrl Pts',(-10.9123261435831,7.11920804880857,
9.85552311663579));
#110919=CARTESIAN_POINT('Ctrl Pts',(-10.9265487481129,7.12017099976067,
9.86700671447932));
#110920=CARTESIAN_POINT('Ctrl Pts',(-11.0228812499225,7.12672812389165,
9.94781487178806));
#110921=CARTESIAN_POINT('Ctrl Pts',(-11.0973535634865,7.13194305879504,
10.0257324668975));
#110922=CARTESIAN_POINT('Ctrl Pts',(-11.2010379905446,7.14025260861692,
10.1613467890855));
#110923=CARTESIAN_POINT('Ctrl Pts',(-11.2361488756505,7.14333590560624,
10.2140188271637));
#110924=CARTESIAN_POINT('Ctrl Pts',(-11.2773138678577,7.14753689633787,
10.2853891767278));
#110925=CARTESIAN_POINT('Ctrl Pts',(-11.2865594175158,7.1485265178306,10.3021718318176));
#110926=CARTESIAN_POINT('Ctrl Pts',(-11.3014632376028,7.15020946816211,
10.3305289356323));
#110927=CARTESIAN_POINT('Ctrl Pts',(-11.3073031112047,7.15089348681348,
10.3420056095124));
#110928=CARTESIAN_POINT('Ctrl Pts',(-11.3151991144883,7.15185535313083,
10.358043195592));
#110929=CARTESIAN_POINT('Ctrl Pts',(-11.3173846064278,7.15212571102489,
10.3625401606742));
#110930=CARTESIAN_POINT('Ctrl Pts',(-11.3210532888134,7.15258677019925,
10.3701884500572));
#110931=CARTESIAN_POINT('Ctrl Pts',(-11.3225483744618,7.15277675232312,
10.3733340783712));
#110932=CARTESIAN_POINT('Ctrl Pts',(-11.3253989295665,7.15314306939153,
10.379387223557));
#110933=CARTESIAN_POINT('Ctrl Pts',(-11.3267560862256,7.15331929178104,
10.3822938983339));
#110934=CARTESIAN_POINT('Ctrl Pts',(-11.3299914011575,7.15374373939651,
10.3892829491349));
#110935=CARTESIAN_POINT('Ctrl Pts',(-11.3318603231066,7.15399250992289,
10.3933695342104));
#110936=CARTESIAN_POINT('Ctrl Pts',(-11.3386024419502,7.1549029586282,10.4082931949829));
#110937=CARTESIAN_POINT('Ctrl Pts',(-11.3433622987065,7.15557094237555,
10.4191806159882));
#110938=CARTESIAN_POINT('Ctrl Pts',(-11.3813285017043,7.16110445648099,
10.5089862202344));
#110939=CARTESIAN_POINT('Ctrl Pts',(-11.4076807520629,7.1662729506619,10.5906155383671));
#110940=CARTESIAN_POINT('Ctrl Pts',(-11.4511307273162,7.17801205783973,
10.7808173744109));
#110941=CARTESIAN_POINT('Ctrl Pts',(-11.4634631656624,7.18451521436854,
10.8899792019832));
#110942=CARTESIAN_POINT('Ctrl Pts',(-11.4634999176129,7.19062697242339,
10.9995089326331));
#110943=CARTESIAN_POINT('Origin',(-10.,3.5,11.));
#110944=CARTESIAN_POINT('',(-11.4635,7.76057136598891,11.0000000000874));
#110945=CARTESIAN_POINT('',(-11.4635,7.68921734064608,10.9999999999359));
#110946=CARTESIAN_POINT('',(-11.4635,3.5,11.));
#110947=CARTESIAN_POINT('Ctrl Pts',(-11.4635,7.76057136598891,11.0000000000874));
#110948=CARTESIAN_POINT('Ctrl Pts',(-11.4635000000058,7.75473127865624,
10.9028434297529));
#110949=CARTESIAN_POINT('Ctrl Pts',(-11.4538253005981,7.7489810398877,10.8059141974648));
#110950=CARTESIAN_POINT('Ctrl Pts',(-11.4309379328563,7.74248848403828,
10.6924387728171));
#110951=CARTESIAN_POINT('Ctrl Pts',(-11.4269190101869,7.74145735128413,
10.6743015829138));
#110952=CARTESIAN_POINT('Ctrl Pts',(-11.4208195038144,7.74003105896416,
10.6490600788052));
#110953=CARTESIAN_POINT('Ctrl Pts',(-11.4190288127671,7.73962679038549,
10.6418881151906));
#110954=CARTESIAN_POINT('Ctrl Pts',(-11.4156464487612,7.73888881646997,
10.6287651356866));
#110955=CARTESIAN_POINT('Ctrl Pts',(-11.4140714018754,7.73855459083289,
10.6228100420527));
#110956=CARTESIAN_POINT('Ctrl Pts',(-11.4107985129743,7.73787869048468,
10.6107442669031));
#110957=CARTESIAN_POINT('Ctrl Pts',(-11.4090984531808,7.73753709493676,
10.6046343199833));
#110958=CARTESIAN_POINT('Ctrl Pts',(-11.4047904693904,7.73669434877157,
10.5895324136441));
#110959=CARTESIAN_POINT('Ctrl Pts',(-11.4021358548523,7.73619470522345,
10.5805539935445));
#110960=CARTESIAN_POINT('Ctrl Pts',(-11.3917758517176,7.73431615923099,
10.5467122791798));
#110961=CARTESIAN_POINT('Ctrl Pts',(-11.3834935563223,7.73295584064186,
10.5220298472499));
#110962=CARTESIAN_POINT('Ctrl Pts',(-11.3608759729155,7.72956019734486,
10.4601509757774));
#110963=CARTESIAN_POINT('Ctrl Pts',(-11.3456713366948,7.72755175465078,
10.4232944180265));
#110964=CARTESIAN_POINT('Ctrl Pts',(-11.3018348496926,7.72235356665669,
10.3282412400242));
#110965=CARTESIAN_POINT('Ctrl Pts',(-11.2708081298361,7.71922009721283,
10.2712471344847));
#110966=CARTESIAN_POINT('Ctrl Pts',(-11.1957868279558,7.71238884414837,
10.1528885494575));
#110967=CARTESIAN_POINT('Ctrl Pts',(-11.1506226096604,7.70869154924494,
10.0924928857486));
#110968=CARTESIAN_POINT('Ctrl Pts',(-11.093096540647,7.70409756612352,10.0268007405701));
#110969=CARTESIAN_POINT('Ctrl Pts',(-11.0850636686296,7.70345828583212,
10.0178525251129));
#110970=CARTESIAN_POINT('Ctrl Pts',(-11.0735307420375,7.70254187826395,
10.0053196123172));
#110971=CARTESIAN_POINT('Ctrl Pts',(-11.0701209369918,7.70227110598106,
10.0016521114985));
#110972=CARTESIAN_POINT('Ctrl Pts',(-11.0643309655621,7.7018114672553,9.99548830664228));
#110973=CARTESIAN_POINT('Ctrl Pts',(-11.0619606388141,7.70162333745661,
9.99298274705127));
#110974=CARTESIAN_POINT('Ctrl Pts',(-11.0570722188718,7.70123537533106,
9.98785188487548));
#110975=CARTESIAN_POINT('Ctrl Pts',(-11.0545531702894,7.7010354729684,9.9852275657572));
#110976=CARTESIAN_POINT('Ctrl Pts',(-11.0480364958302,7.70051844687545,
9.97848903024078));
#110977=CARTESIAN_POINT('Ctrl Pts',(-11.0440244552388,7.70020024453759,
9.97438891748906));
#110978=CARTESIAN_POINT('Ctrl Pts',(-11.0269656966991,7.69884816338197,
9.95715950218753));
#110979=CARTESIAN_POINT('Ctrl Pts',(-11.0136951587265,7.69779850588063,
9.94425528355815));
#110980=CARTESIAN_POINT('Ctrl Pts',(-10.9770546748602,7.69491499295608,
9.90995402469883));
#110981=CARTESIAN_POINT('Ctrl Pts',(-10.9532293802638,7.69305565762345,
9.88905913930285));
#110982=CARTESIAN_POINT('Ctrl Pts',(-10.8527542836138,7.68533843619732,
9.8065550171705));
#110983=CARTESIAN_POINT('Ctrl Pts',(-10.7706658411821,7.67933721882721,
9.75197079903355));
#110984=CARTESIAN_POINT('Ctrl Pts',(-10.6295088858711,7.66993941409464,
9.67738517620508));
#110985=CARTESIAN_POINT('Ctrl Pts',(-10.5735482208729,7.66641687429221,
9.65217384858416));
#110986=CARTESIAN_POINT('Ctrl Pts',(-10.5053994519177,7.66237355454415,
9.62648771331742));
#110987=CARTESIAN_POINT('Ctrl Pts',(-10.4945863913979,7.66173899348304,
9.62255710837732));
#110988=CARTESIAN_POINT('Ctrl Pts',(-10.4766777750269,7.6606993095538,9.61628530796765));
#110989=CARTESIAN_POINT('Ctrl Pts',(-10.4696087764442,7.6602917884261,9.61387026216208));
#110990=CARTESIAN_POINT('Ctrl Pts',(-10.4567970850015,7.65955829696784,
9.60960254666077));
#110991=CARTESIAN_POINT('Ctrl Pts',(-10.4510608703118,7.65923172096216,
9.60773107917474));
#110992=CARTESIAN_POINT('Ctrl Pts',(-10.4387281489814,7.65853345144564,
9.60379168874217));
#110993=CARTESIAN_POINT('Ctrl Pts',(-10.4321282165507,7.65816212547454,
9.6017349164676));
#110994=CARTESIAN_POINT('Ctrl Pts',(-10.4140368234832,7.65715055988169,
9.59623732588747));
#110995=CARTESIAN_POINT('Ctrl Pts',(-10.4025171062465,7.65651336123415,
9.59289086175695));
#110996=CARTESIAN_POINT('Ctrl Pts',(-10.3373516056281,7.6529458560142,9.57482613627531));
#110997=CARTESIAN_POINT('Ctrl Pts',(-10.2829394008663,7.65011029165728,
9.56303346596823));
#110998=CARTESIAN_POINT('Ctrl Pts',(-10.1472269861223,7.64326089530265,
9.54163095801759));
#110999=CARTESIAN_POINT('Ctrl Pts',(-10.0655465404924,7.63933599194206,
9.53568451716217));
#111000=CARTESIAN_POINT('Ctrl Pts',(-9.91445236077482,7.63193678802747,
9.53735752369492));
#111001=CARTESIAN_POINT('Ctrl Pts',(-9.84525812767399,7.62849022084844,
9.5430531218684));
#111002=CARTESIAN_POINT('Ctrl Pts',(-9.76868470762343,7.62436971753075,
9.55487306038602));
#111003=CARTESIAN_POINT('Ctrl Pts',(-9.7606430127828,7.62393313132441,9.55618323089514));
#111004=CARTESIAN_POINT('Ctrl Pts',(-9.74846083086693,7.62326534303885,
9.55827254904853));
#111005=CARTESIAN_POINT('Ctrl Pts',(-9.74431194759029,7.62303678260618,
9.55900256232272));
#111006=CARTESIAN_POINT('Ctrl Pts',(-9.73684281684787,7.62262317804185,
9.5603500591529));
#111007=CARTESIAN_POINT('Ctrl Pts',(-9.73352149582339,7.62243849249484,
9.56096113268532));
#111008=CARTESIAN_POINT('Ctrl Pts',(-9.72620570157026,7.62202998574904,
9.56233332560405));
#111009=CARTESIAN_POINT('Ctrl Pts',(-9.72221231999821,7.62180588669955,
9.56309958990127));
#111010=CARTESIAN_POINT('Ctrl Pts',(-9.71066585334278,7.62115480865239,
9.56536509918817));
#111011=CARTESIAN_POINT('Ctrl Pts',(-9.70312145776466,7.62072553086426,
9.56690730482109));
#111012=CARTESIAN_POINT('Ctrl Pts',(-9.64496912776847,7.61738861048399,
9.57927354701719));
#111013=CARTESIAN_POINT('Ctrl Pts',(-9.59495963048441,7.61435568560235,
9.59271471907147));
#111014=CARTESIAN_POINT('Ctrl Pts',(-9.44043382571202,7.60467412627618,
9.64316657271366));
#111015=CARTESIAN_POINT('Ctrl Pts',(-9.33932796696818,7.59791123469256,
9.68941683375412));
#111016=CARTESIAN_POINT('Ctrl Pts',(-9.20548571697756,7.58884003872102,
9.77010362005083));
#111017=CARTESIAN_POINT('Ctrl Pts',(-9.16767248073269,7.58625677601352,
9.79537160226357));
#111018=CARTESIAN_POINT('Ctrl Pts',(-9.12170697210895,7.58309165832408,
9.82928667681572));
#111019=CARTESIAN_POINT('Ctrl Pts',(-9.11240322321058,7.58244959126441,
9.83632465834419));
#111020=CARTESIAN_POINT('Ctrl Pts',(-9.09772583706522,7.58143417998846,
9.84770607149992));
#111021=CARTESIAN_POINT('Ctrl Pts',(-9.09229722245432,7.58105806050645,
9.85197751212453));
#111022=CARTESIAN_POINT('Ctrl Pts',(-9.0821833036215,7.58035620096151,9.86005211806163));
#111023=CARTESIAN_POINT('Ctrl Pts',(-9.0774909023831,7.58003011076133,9.86384612485723));
#111024=CARTESIAN_POINT('Ctrl Pts',(-9.0670366719485,7.57930251167623,9.87240628319394));
#111025=CARTESIAN_POINT('Ctrl Pts',(-9.06128761189233,7.57890162726258,
9.87718780871681));
#111026=CARTESIAN_POINT('Ctrl Pts',(-9.04436071196861,7.57771884778395,
9.89148688787355));
#111027=CARTESIAN_POINT('Ctrl Pts',(-9.03328897720108,7.57694199195277,
9.90112894866623));
#111028=CARTESIAN_POINT('Ctrl Pts',(-9.00839449840216,7.57518642349276,
9.92347634527813));
#111029=CARTESIAN_POINT('Ctrl Pts',(-8.99466728370875,7.57421196672982,
9.93628442767607));
#111030=CARTESIAN_POINT('Ctrl Pts',(-8.94943140007354,7.57097331148404,
9.98014958402837));
#111031=CARTESIAN_POINT('Ctrl Pts',(-8.91908423043094,7.56875510172294,
10.01237115943));
#111032=CARTESIAN_POINT('Ctrl Pts',(-8.85091453899071,7.56358775581954,
10.0916641277628));
#111033=CARTESIAN_POINT('Ctrl Pts',(-8.81445262760388,7.56067227973134,
10.1397971127062));
#111034=CARTESIAN_POINT('Ctrl Pts',(-8.75988673015752,7.55586252034449,
10.2219153468808));
#111035=CARTESIAN_POINT('Ctrl Pts',(-8.7399669734504,7.55398577678086,10.254605322844));
#111036=CARTESIAN_POINT('Ctrl Pts',(-8.70123071358002,7.54999743373747,
10.3241736150263));
#111037=CARTESIAN_POINT('Ctrl Pts',(-8.68265211281551,7.54788087011945,
10.3611440368657));
#111038=CARTESIAN_POINT('Ctrl Pts',(-8.66281111212311,7.5453077950752,10.4051837135376));
#111039=CARTESIAN_POINT('Ctrl Pts',(-8.66000199535045,7.54493522276934,
10.4115393978377));
#111040=CARTESIAN_POINT('Ctrl Pts',(-8.65552020144677,7.5443268018641,10.4218780568315));
#111041=CARTESIAN_POINT('Ctrl Pts',(-8.65381967951906,7.54409255766012,
10.4258489278284));
#111042=CARTESIAN_POINT('Ctrl Pts',(-8.65081876007786,7.54367297718955,
10.4329429685351));
#111043=CARTESIAN_POINT('Ctrl Pts',(-8.64951158323239,7.54348804885193,
10.4360631852956));
#111044=CARTESIAN_POINT('Ctrl Pts',(-8.64669018868265,7.54308413448502,
10.4428638920726));
#111045=CARTESIAN_POINT('Ctrl Pts',(-8.64518018228551,7.54286491286244,
10.4465459830094));
#111046=CARTESIAN_POINT('Ctrl Pts',(-8.64094566635844,7.54224152777444,
10.4569928603596));
#111047=CARTESIAN_POINT('Ctrl Pts',(-8.63825671616897,7.54183534958293,
10.4637718209926));
#111048=CARTESIAN_POINT('Ctrl Pts',(-8.62101672226235,7.53916378229126,
10.5082006350737));
#111049=CARTESIAN_POINT('Ctrl Pts',(-8.60797904506213,7.53682178312963,
10.5464158161719));
#111050=CARTESIAN_POINT('Ctrl Pts',(-8.55685110415499,7.52617313485845,
10.7193710122347));
#111051=CARTESIAN_POINT('Ctrl Pts',(-8.53662520365909,7.51755628813411,
10.8586592934391));
#111052=CARTESIAN_POINT('Ctrl Pts',(-8.53647278092057,7.50777217626109,
11.0299344718732));
#111053=CARTESIAN_POINT('Ctrl Pts',(-8.53744505908784,7.50601619663285,
11.0611657270828));
#111054=CARTESIAN_POINT('Ctrl Pts',(-8.54006961833363,7.50371878521601,
11.1026779118903));
#111055=CARTESIAN_POINT('Ctrl Pts',(-8.54083265787684,7.5031502480287,11.1130050808016));
#111056=CARTESIAN_POINT('Ctrl Pts',(-8.54225752367472,7.50222740574017,
11.1298540576063));
#111057=CARTESIAN_POINT('Ctrl Pts',(-8.54285366321132,7.5018710818799,11.1363809322538));
#111058=CARTESIAN_POINT('Ctrl Pts',(-8.54409051147143,7.5011850479082,11.1489871692392));
#111059=CARTESIAN_POINT('Ctrl Pts',(-8.54472550364562,7.5008551682207,11.1550669442614));
#111060=CARTESIAN_POINT('Ctrl Pts',(-8.54629407886147,7.50008912742966,
11.1692261508662));
#111061=CARTESIAN_POINT('Ctrl Pts',(-8.54725696110659,7.49965388427216,
11.1773021766336));
#111062=CARTESIAN_POINT('Ctrl Pts',(-8.55058328137308,7.49825513371005,
11.2033520519027));
#111063=CARTESIAN_POINT('Ctrl Pts',(-8.55321341158184,7.49729990037004,
11.221290503065));
#111064=CARTESIAN_POINT('Ctrl Pts',(-8.56019498917973,7.49507153921929,
11.2634359015561));
#111065=CARTESIAN_POINT('Ctrl Pts',(-8.56482467844388,7.49380686043093,
11.2875914166956));
#111066=CARTESIAN_POINT('Ctrl Pts',(-8.58442877192753,7.48912855681503,
11.3775493350142));
#111067=CARTESIAN_POINT('Ctrl Pts',(-8.60333958615982,7.48582353326137,
11.4424091854995));
#111068=CARTESIAN_POINT('Ctrl Pts',(-8.66120469948342,7.47766922229001,
11.5995439272189));
#111069=CARTESIAN_POINT('Ctrl Pts',(-8.70526659266771,7.47286938536262,
11.6895550986922));
#111070=CARTESIAN_POINT('Ctrl Pts',(-8.76407532679442,7.46701019427945,
11.7838673002117));
#111071=CARTESIAN_POINT('Ctrl Pts',(-8.77011143161543,7.46641379973005,
11.7933043782688));
#111072=CARTESIAN_POINT('Ctrl Pts',(-8.77866451149831,7.46557420211996,
11.806344326903));
#111073=CARTESIAN_POINT('Ctrl Pts',(-8.78109042656616,7.46533666191741,
11.8100067899694));
#111074=CARTESIAN_POINT('Ctrl Pts',(-8.78530128125618,7.46492526377293,
11.8163022671063));
#111075=CARTESIAN_POINT('Ctrl Pts',(-8.78707839777739,7.46475191820136,
11.8189405076475));
#111076=CARTESIAN_POINT('Ctrl Pts',(-8.79083226780889,7.46438628847645,
11.8244743401019));
#111077=CARTESIAN_POINT('Ctrl Pts',(-8.79281083918449,7.46419387850358,
11.8273686429241));
#111078=CARTESIAN_POINT('Ctrl Pts',(-8.7977049959379,7.46371873683989,11.8344730065873));
#111079=CARTESIAN_POINT('Ctrl Pts',(-8.80063230186567,7.46343523446217,
11.8386749063782));
#111080=CARTESIAN_POINT('Ctrl Pts',(-8.81146804889436,7.46238859951005,
11.8540559515601));
#111081=CARTESIAN_POINT('Ctrl Pts',(-8.81951098854474,7.46161709903128,
11.8651389677207));
#111082=CARTESIAN_POINT('Ctrl Pts',(-8.84016800491446,7.45965226992434,
11.892779488675));
#111083=CARTESIAN_POINT('Ctrl Pts',(-8.85298178075879,7.45844845978603,
11.9091834801123));
#111084=CARTESIAN_POINT('Ctrl Pts',(-8.9126567131123,7.45292851133689,11.9823083240997));
#111085=CARTESIAN_POINT('Ctrl Pts',(-8.96340331046673,7.44847186652789,
12.0357179623672));
#111086=CARTESIAN_POINT('Ctrl Pts',(-9.08749807401176,7.43841781648588,
12.1480295374196));
#111087=CARTESIAN_POINT('Ctrl Pts',(-9.16294733183338,7.43287664782252,
12.2041508024154));
#111088=CARTESIAN_POINT('Ctrl Pts',(-9.25763547307535,7.42667143557581,
12.2613521404095));
#111089=CARTESIAN_POINT('Ctrl Pts',(-9.27215956465722,7.42573807731485,
12.2697884258457));
#111090=CARTESIAN_POINT('Ctrl Pts',(-9.29466538041419,7.42431941830449,
12.2823478143939));
#111091=CARTESIAN_POINT('Ctrl Pts',(-9.30254487553938,7.42382782161387,
12.286650378714));
#111092=CARTESIAN_POINT('Ctrl Pts',(-9.31543643063254,7.42303165242581,
12.2935365300479));
#111093=CARTESIAN_POINT('Ctrl Pts',(-9.32042462953291,7.42272554484162,
12.2961640915257));
#111094=CARTESIAN_POINT('Ctrl Pts',(-9.33092906311407,7.42208497884518,
12.3016200512283));
#111095=CARTESIAN_POINT('Ctrl Pts',(-9.33644834459411,7.42175073673674,
12.3044423630709));
#111096=CARTESIAN_POINT('Ctrl Pts',(-9.3497001709032,7.42095368795321,12.3111128782097));
#111097=CARTESIAN_POINT('Ctrl Pts',(-9.35744922440065,7.42049203277166,
12.3149278885963));
#111098=CARTESIAN_POINT('Ctrl Pts',(-9.38424839036251,7.41891024115927,
12.3278281649582));
#111099=CARTESIAN_POINT('Ctrl Pts',(-9.40346143954344,7.41780178672107,
12.3365700450466));
#111100=CARTESIAN_POINT('Ctrl Pts',(-9.48582338549034,7.41314890729399,
12.3719145346809));
#111101=CARTESIAN_POINT('Ctrl Pts',(-9.55061275836494,7.4097367782104,12.394481774003));
#111102=CARTESIAN_POINT('Ctrl Pts',(-9.69808838671182,7.4022498603411,12.4344981086635));
#111103=CARTESIAN_POINT('Ctrl Pts',(-9.78117776245955,7.39821891189439,
12.4495002537813));
#111104=CARTESIAN_POINT('Ctrl Pts',(-9.90561494572057,7.39195450593427,
12.4610201619974));
#111105=CARTESIAN_POINT('Ctrl Pts',(-9.94627378363094,7.38987039942979,
12.4630794254649));
#111106=CARTESIAN_POINT('Ctrl Pts',(-9.99388300968915,7.38733392454411,
12.4635035827577));
#111107=CARTESIAN_POINT('Ctrl Pts',(-10.0008042463413,7.38696280217191,
12.4635161440193));
#111108=CARTESIAN_POINT('Ctrl Pts',(-10.0120365540918,7.38635628686158,
12.463456852748));
#111109=CARTESIAN_POINT('Ctrl Pts',(-10.016347753843,7.38612248188271,12.4634150431352));
#111110=CARTESIAN_POINT('Ctrl Pts',(-10.0240407722511,7.38570337132344,
12.4633064382759));
#111111=CARTESIAN_POINT('Ctrl Pts',(-10.0274226155955,7.38551846987643,
12.4632469685215));
#111112=CARTESIAN_POINT('Ctrl Pts',(-10.0347893011276,7.38511423689949,
12.4630918774794));
#111113=CARTESIAN_POINT('Ctrl Pts',(-10.0387739130224,7.38489466672256,
12.4629917020665));
#111114=CARTESIAN_POINT('Ctrl Pts',(-10.0500765773374,7.38426931865933,
12.4626613393003));
#111115=CARTESIAN_POINT('Ctrl Pts',(-10.057393276224,7.38386150648101,12.4623925137953));
#111116=CARTESIAN_POINT('Ctrl Pts',(-10.1056936333741,7.38115095313022,
12.4602548612918));
#111117=CARTESIAN_POINT('Ctrl Pts',(-10.1465820904955,7.37876908258855,
12.4567184102257));
#111118=CARTESIAN_POINT('Ctrl Pts',(-10.3362939836918,7.36746837657589,
12.4322423548232));
#111119=CARTESIAN_POINT('Ctrl Pts',(-10.4815189825224,7.35821742802636,
12.3901683126946));
#111120=CARTESIAN_POINT('Ctrl Pts',(-10.6384924191183,7.34843648984094,
12.3170729757888));
#111121=CARTESIAN_POINT('Ctrl Pts',(-10.6589674959353,7.34716232867441,
12.3069490098001));
#111122=CARTESIAN_POINT('Ctrl Pts',(-10.6873235485571,7.34539932304703,
12.2920923869217));
#111123=CARTESIAN_POINT('Ctrl Pts',(-10.6954089299132,7.34489679804423,
12.287758837007));
#111124=CARTESIAN_POINT('Ctrl Pts',(-10.7084279238612,7.34408779933793,
12.2806226261803));
#111125=CARTESIAN_POINT('Ctrl Pts',(-10.7133868341596,7.34377969117181,
12.2778668397354));
#111126=CARTESIAN_POINT('Ctrl Pts',(-10.7235965515742,7.34314537086463,
12.2721150989263));
#111127=CARTESIAN_POINT('Ctrl Pts',(-10.728845077147,7.34281930263742,12.2691153018498));
#111128=CARTESIAN_POINT('Ctrl Pts',(-10.7411776436207,7.34205310138474,
12.261964880065));
#111129=CARTESIAN_POINT('Ctrl Pts',(-10.7482456819274,7.34161395159393,
12.2577869696807));
#111130=CARTESIAN_POINT('Ctrl Pts',(-10.76314667304,7.34068787864448,12.2488089493809));
#111131=CARTESIAN_POINT('Ctrl Pts',(-10.770970361782,7.34020150201364,12.2439941088732));
#111132=CARTESIAN_POINT('Ctrl Pts',(-10.7921259669915,7.33888550379048,
12.2306983182467));
#111133=CARTESIAN_POINT('Ctrl Pts',(-10.8053668889463,7.33806096431955,
12.2220745052581));
#111134=CARTESIAN_POINT('Ctrl Pts',(-10.9155886779984,7.33118189032094,
12.1477174591916));
#111135=CARTESIAN_POINT('Ctrl Pts',(-11.0044901853269,7.32557656359651,
12.0707748816618));
#111136=CARTESIAN_POINT('Ctrl Pts',(-11.1319517305178,7.31630721827846,
11.930461892167));
#111137=CARTESIAN_POINT('Ctrl Pts',(-11.1765842887161,7.31272003209837,
11.8733390272966));
#111138=CARTESIAN_POINT('Ctrl Pts',(-11.2213335166274,7.30843698041421,
11.8063765830779));
#111139=CARTESIAN_POINT('Ctrl Pts',(-11.2258077342041,7.30800001840562,
11.7995587191176));
#111140=CARTESIAN_POINT('Ctrl Pts',(-11.2325072494409,7.30733176731578,
11.7891615103695));
#111141=CARTESIAN_POINT('Ctrl Pts',(-11.2347745211362,7.30710312538032,
11.7856092479263));
#111142=CARTESIAN_POINT('Ctrl Pts',(-11.2388310655877,7.30668943685984,
11.779192688956));
#111143=CARTESIAN_POINT('Ctrl Pts',(-11.2406257987953,7.30650474957136,
11.776331940962));
#111144=CARTESIAN_POINT('Ctrl Pts',(-11.24455896199,7.30609631643565,11.7700141321322));
#111145=CARTESIAN_POINT('Ctrl Pts',(-11.2466928722943,7.30587229338915,
11.7665544044003));
#111146=CARTESIAN_POINT('Ctrl Pts',(-11.2528240753573,7.30522165075082,
11.7565205115662));
#111147=CARTESIAN_POINT('Ctrl Pts',(-11.2567839117989,7.30479273696936,
11.7499237574829));
#111148=CARTESIAN_POINT('Ctrl Pts',(-11.286862325093,7.30146880469705,11.698908298222));
#111149=CARTESIAN_POINT('Ctrl Pts',(-11.3106682918532,7.29844956906858,
11.6531730862665));
#111150=CARTESIAN_POINT('Ctrl Pts',(-11.3858148088539,7.28764733148999,
11.4880752594081));
#111151=CARTESIAN_POINT('Ctrl Pts',(-11.4236543118523,7.27971207713107,
11.3632056139713));
#111152=CARTESIAN_POINT('Ctrl Pts',(-11.4493042064121,7.27060221910975,
11.2055237581379));
#111153=CARTESIAN_POINT('Ctrl Pts',(-11.4531936142035,7.26892673681237,
11.1759295285654));
#111154=CARTESIAN_POINT('Ctrl Pts',(-11.45719232336,7.26671733720045,11.1361114001376));
#111155=CARTESIAN_POINT('Ctrl Pts',(-11.4581034347236,7.26615885443728,
11.1259768290674));
#111156=CARTESIAN_POINT('Ctrl Pts',(-11.4594244295834,7.26524816245517,
11.1093390452742));
#111157=CARTESIAN_POINT('Ctrl Pts',(-11.4598966988704,7.26489403451313,
11.102841251538));
#111158=CARTESIAN_POINT('Ctrl Pts',(-11.4607061936426,7.26422814505174,
11.0905709543574));
#111159=CARTESIAN_POINT('Ctrl Pts',(-11.4610526269498,7.26391610501315,
11.0847992011743));
#111160=CARTESIAN_POINT('Ctrl Pts',(-11.4616865632727,7.2632846707454,11.0730762460578));
#111161=CARTESIAN_POINT('Ctrl Pts',(-11.4619719484179,7.26296534743556,
11.0671250359433));
#111162=CARTESIAN_POINT('Ctrl Pts',(-11.4626126326677,7.26214668737144,
11.0518105282083));
#111163=CARTESIAN_POINT('Ctrl Pts',(-11.4629143706465,7.26164899911573,
11.0424451837417));
#111164=CARTESIAN_POINT('Ctrl Pts',(-11.4633785691653,7.26056397069535,
11.0219121260251));
#111165=CARTESIAN_POINT('Ctrl Pts',(-11.463503176572,7.25997779352992,11.0107441486259));
#111166=CARTESIAN_POINT('Ctrl Pts',(-11.4634999384891,7.25939525541925,
10.9995756860797));
#111167=CARTESIAN_POINT('Ctrl Pts',(-11.4634999176129,7.19062697242339,
10.9995089326331));
#111168=CARTESIAN_POINT('Ctrl Pts',(-11.4635051213571,7.1914923421607,11.0150173531874));
#111169=CARTESIAN_POINT('Ctrl Pts',(-11.4632638158498,7.19235020755999,
11.0305252719007));
#111170=CARTESIAN_POINT('Ctrl Pts',(-11.4625356658954,7.19361955643145,
11.0536665512648));
#111171=CARTESIAN_POINT('Ctrl Pts',(-11.4622354301267,7.19403675453786,
11.0613043449609));
#111172=CARTESIAN_POINT('Ctrl Pts',(-11.461590362189,7.19478087691799,11.0749831270642));
#111173=CARTESIAN_POINT('Ctrl Pts',(-11.4612678792724,7.1951084832571,11.0810249511718));
#111174=CARTESIAN_POINT('Ctrl Pts',(-11.4605033684944,7.19580185987213,
11.0938531158355));
#111175=CARTESIAN_POINT('Ctrl Pts',(-11.4600514863654,7.19616731773661,
11.100638740175));
#111176=CARTESIAN_POINT('Ctrl Pts',(-11.4587100487841,7.19714554879489,
11.1188651341328));
#111177=CARTESIAN_POINT('Ctrl Pts',(-11.4577331972617,7.19775561701456,
11.1302991253625));
#111178=CARTESIAN_POINT('Ctrl Pts',(-11.4520308368187,7.20086566565634,
11.188908667653));
#111179=CARTESIAN_POINT('Ctrl Pts',(-11.4451492228012,7.20329822460771,
11.2358481206412));
#111180=CARTESIAN_POINT('Ctrl Pts',(-11.415358651437,7.21105579417276,11.3873467227317));
#111181=CARTESIAN_POINT('Ctrl Pts',(-11.3832704409702,7.21612901499671,
11.4897342692634));
#111182=CARTESIAN_POINT('Ctrl Pts',(-11.3293779365529,7.22276968588414,
11.6126398979588));
#111183=CARTESIAN_POINT('Ctrl Pts',(-11.3177526773158,7.22413133361263,
11.6372606312539));
#111184=CARTESIAN_POINT('Ctrl Pts',(-11.2926351018324,7.22696396042054,
11.686826188853));
#111185=CARTESIAN_POINT('Ctrl Pts',(-11.2790910658817,7.228436530401,11.7117313832945));
#111186=CARTESIAN_POINT('Ctrl Pts',(-11.2613911837764,7.23031562663727,
11.7421397122222));
#111187=CARTESIAN_POINT('Ctrl Pts',(-11.2579075986177,7.23068343984053,
11.7480291041618));
#111188=CARTESIAN_POINT('Ctrl Pts',(-11.2523619390566,7.2312661822005,11.7572563735347));
#111189=CARTESIAN_POINT('Ctrl Pts',(-11.2503274788332,7.23147938785848,
11.7606108312396));
#111190=CARTESIAN_POINT('Ctrl Pts',(-11.2465261983596,7.23187676404217,
11.766821993147));
#111191=CARTESIAN_POINT('Ctrl Pts',(-11.2447630107207,7.23206070270992,
11.7696808291665));
#111192=CARTESIAN_POINT('Ctrl Pts',(-11.2406751400041,7.23248626784267,
11.7762581258429));
#111193=CARTESIAN_POINT('Ctrl Pts',(-11.2383435793675,7.23272833385409,
11.7799722170576));
#111194=CARTESIAN_POINT('Ctrl Pts',(-11.2310224920121,7.23348623791284,
11.7915188682637));
#111195=CARTESIAN_POINT('Ctrl Pts',(-11.2259751782284,7.23400563614262,
11.7993142986445));
#111196=CARTESIAN_POINT('Ctrl Pts',(-11.2139687620387,7.23523298025802,
11.8174765984065));
#111197=CARTESIAN_POINT('Ctrl Pts',(-11.2069505719273,7.23594418474576,
11.827803383582));
#111198=CARTESIAN_POINT('Ctrl Pts',(-11.1815364561673,7.2384943466751,11.8641882033712));
#111199=CARTESIAN_POINT('Ctrl Pts',(-11.1624225225761,7.24036668439603,
11.8897321535548));
#111200=CARTESIAN_POINT('Ctrl Pts',(-11.0830318516041,7.24790899459085,
11.9889013385968));
#111201=CARTESIAN_POINT('Ctrl Pts',(-11.0164717811869,7.25371189825479,
12.0571993897305));
#111202=CARTESIAN_POINT('Ctrl Pts',(-10.8948564543984,7.26309728359235,
12.1598088156079));
#111203=CARTESIAN_POINT('Ctrl Pts',(-10.8433067629296,7.26677895392274,
12.1978146542371));
#111204=CARTESIAN_POINT('Ctrl Pts',(-10.7796537744778,7.27097672956484,
12.2385907384724));
#111205=CARTESIAN_POINT('Ctrl Pts',(-10.7698039134366,7.27161717065676,
12.2447365067382));
#111206=CARTESIAN_POINT('Ctrl Pts',(-10.7534694187952,7.27266451547499,
12.2546602646565));
#111207=CARTESIAN_POINT('Ctrl Pts',(-10.7470271297079,7.27307387764979,
12.2585066607562));
#111208=CARTESIAN_POINT('Ctrl Pts',(-10.7353478093011,7.2738094381201,12.265358566995));
#111209=CARTESIAN_POINT('Ctrl Pts',(-10.7301212489474,7.27413625615823,
12.2683815147875));
#111210=CARTESIAN_POINT('Ctrl Pts',(-10.7188882121682,7.2748337095986,12.2747860598122));
#111211=CARTESIAN_POINT('Ctrl Pts',(-10.712876236246,7.27520398777064,12.2781577500034));
#111212=CARTESIAN_POINT('Ctrl Pts',(-10.6964228215469,7.27620934072081,
12.2872330995691));
#111213=CARTESIAN_POINT('Ctrl Pts',(-10.6859351727526,7.27684143938897,
12.2928521759372));
#111214=CARTESIAN_POINT('Ctrl Pts',(-10.6275600038426,7.28031353069479,
12.3232181298679));
#111215=CARTESIAN_POINT('Ctrl Pts',(-10.5783997625433,7.28306492826677,
12.3454338708195));
#111216=CARTESIAN_POINT('Ctrl Pts',(-10.4021100008816,7.29250318902173,
12.4136464034992));
#111217=CARTESIAN_POINT('Ctrl Pts',(-10.2699717475884,7.29877546861338,
12.4447130467065));
#111218=CARTESIAN_POINT('Ctrl Pts',(-10.1141191493033,7.30684838720288,
12.4592013822133));
#111219=CARTESIAN_POINT('Ctrl Pts',(-10.0927328581139,7.30797200025533,
12.4607163917823));
#111220=CARTESIAN_POINT('Ctrl Pts',(-10.0650355306731,7.30945627656537,
12.4620677977752));
#111221=CARTESIAN_POINT('Ctrl Pts',(-10.0587471214867,7.30979520417874,
12.4623339695157));
#111222=CARTESIAN_POINT('Ctrl Pts',(-10.0486978123123,7.31034019996122,
12.4626944058978));
#111223=CARTESIAN_POINT('Ctrl Pts',(-10.044937856662,7.31054486303623,12.4628147491592));
#111224=CARTESIAN_POINT('Ctrl Pts',(-10.0377484816496,7.31093770551627,
12.4630171119189));
#111225=CARTESIAN_POINT('Ctrl Pts',(-10.0343191984752,7.31112575117329,
12.4631015717843));
#111226=CARTESIAN_POINT('Ctrl Pts',(-10.0261884361782,7.31157313678651,
12.4632732237992));
#111227=CARTESIAN_POINT('Ctrl Pts',(-10.0214867931346,7.31183305079773,
12.4633498140056));
#111228=CARTESIAN_POINT('Ctrl Pts',(-10.0057474125166,7.31270701761987,
12.4635303413523));
#111229=CARTESIAN_POINT('Ctrl Pts',(-9.99470914775795,7.31332631265321,
12.4635320580216));
#111230=CARTESIAN_POINT('Ctrl Pts',(-9.93184857472069,7.3168853192916,12.4628307018585));
#111231=CARTESIAN_POINT('Ctrl Pts',(-9.88009636637776,7.31993914587323,
12.4595000780852));
#111232=CARTESIAN_POINT('Ctrl Pts',(-9.68767499445089,7.33151238412982,
12.4368128678463));
#111233=CARTESIAN_POINT('Ctrl Pts',(-9.54984485172418,7.34014800453584,
12.3997692678828));
#111234=CARTESIAN_POINT('Ctrl Pts',(-9.40349365373665,7.34907334235398,
12.3365315280307));
#111235=CARTESIAN_POINT('Ctrl Pts',(-9.38761021903613,7.35004016439006,
12.3293288304509));
#111236=CARTESIAN_POINT('Ctrl Pts',(-9.36470247907094,7.35143233656326,
12.3184430544066));
#111237=CARTESIAN_POINT('Ctrl Pts',(-9.35757378633333,7.35186525546715,
12.3149842551331));
#111238=CARTESIAN_POINT('Ctrl Pts',(-9.34500435241188,7.35262812178203,
12.308759030271));
#111239=CARTESIAN_POINT('Ctrl Pts',(-9.33955221116796,7.3529588683287,12.3060161627873));
#111240=CARTESIAN_POINT('Ctrl Pts',(-9.32825179329688,7.3536441285302,12.3002422786112));
#111241=CARTESIAN_POINT('Ctrl Pts',(-9.32240649299769,7.3539984406497,12.2972057190365));
#111242=CARTESIAN_POINT('Ctrl Pts',(-9.30729678370843,7.35491403903563,
12.2892264188123));
#111243=CARTESIAN_POINT('Ctrl Pts',(-9.29806462561568,7.35547320519396,
12.2842232059346));
#111244=CARTESIAN_POINT('Ctrl Pts',(-9.25756965285052,7.35792558053323,
12.2617104771799));
#111245=CARTESIAN_POINT('Ctrl Pts',(-9.22690092271885,7.35978169260165,
12.2431549512157));
#111246=CARTESIAN_POINT('Ctrl Pts',(-9.14362403862164,7.36485099246882,
12.188494876388));
#111247=CARTESIAN_POINT('Ctrl Pts',(-9.09264793688092,7.36798551343019,
12.1500490595042));
#111248=CARTESIAN_POINT('Ctrl Pts',(-8.96402725450231,7.37626442578684,
12.0391525291314));
#111249=CARTESIAN_POINT('Ctrl Pts',(-8.89148842474422,7.38132987985839,
11.9613915807975));
#111250=CARTESIAN_POINT('Ctrl Pts',(-8.82163247437605,7.38748801189372,
11.8679833497076));
#111251=CARTESIAN_POINT('Ctrl Pts',(-8.81536272450085,7.3880542329676,11.8594065588891));
#111252=CARTESIAN_POINT('Ctrl Pts',(-8.8066900144571,7.38885787013781,11.8472673603374));
#111253=CARTESIAN_POINT('Ctrl Pts',(-8.80420837257014,7.38909023766389,
11.8437612721164));
#111254=CARTESIAN_POINT('Ctrl Pts',(-8.79992973353963,7.3894951703912,11.8376595798839));
#111255=CARTESIAN_POINT('Ctrl Pts',(-8.79812561960328,7.38966726117493,
11.8350689729424));
#111256=CARTESIAN_POINT('Ctrl Pts',(-8.79431892367519,7.39003329157356,
11.8295648805122));
#111257=CARTESIAN_POINT('Ctrl Pts',(-8.79231849751489,7.39022737673062,
11.826649948092));
#111258=CARTESIAN_POINT('Ctrl Pts',(-8.78736767205361,7.39071199706625,
11.8193794986493));
#111259=CARTESIAN_POINT('Ctrl Pts',(-8.78443017859925,7.39100336980907,
11.8150152962724));
#111260=CARTESIAN_POINT('Ctrl Pts',(-8.77338894351127,7.39211289821478,
11.798418976431));
#111261=CARTESIAN_POINT('Ctrl Pts',(-8.76544605449303,7.39294074715676,
11.7860814638972));
#111262=CARTESIAN_POINT('Ctrl Pts',(-8.74560453847067,7.39508218757218,
11.7542194634899));
#111263=CARTESIAN_POINT('Ctrl Pts',(-8.73397574702145,7.39640862886415,
11.7345321411261));
#111264=CARTESIAN_POINT('Ctrl Pts',(-8.68191726887963,7.40266527378569,
11.641486926114));
#111265=CARTESIAN_POINT('Ctrl Pts',(-8.64737227816325,7.40776202133643,
11.5650181597829));
#111266=CARTESIAN_POINT('Ctrl Pts',(-8.59022573212598,7.41805473202854,
11.4027034559474));
#111267=CARTESIAN_POINT('Ctrl Pts',(-8.5684923515426,7.42321642601655,11.3168968767975));
#111268=CARTESIAN_POINT('Ctrl Pts',(-8.5527231635129,7.42880351265699,11.2176455083532));
#111269=CARTESIAN_POINT('Ctrl Pts',(-8.55096648108172,7.42947421945445,
11.2056251011709));
#111270=CARTESIAN_POINT('Ctrl Pts',(-8.54834560045252,7.43056060174405,
11.18598527486));
#111271=CARTESIAN_POINT('Ctrl Pts',(-8.54739128465897,7.43097905826682,
11.178378646203));
#111272=CARTESIAN_POINT('Ctrl Pts',(-8.54579053416922,7.43172457065082,
11.1647534936506));
#111273=CARTESIAN_POINT('Ctrl Pts',(-8.54512159088135,7.43205231859116,
11.1587378353822));
#111274=CARTESIAN_POINT('Ctrl Pts',(-8.54378176882612,7.43274511420222,
11.1459683997064));
#111275=CARTESIAN_POINT('Ctrl Pts',(-8.54312051060801,7.43310985624366,
11.1392137422044));
#111276=CARTESIAN_POINT('Ctrl Pts',(-8.54147336645238,7.43408406681422,
11.1210890308898));
#111277=CARTESIAN_POINT('Ctrl Pts',(-8.54057343877856,7.43469086962136,
11.109711514188));
#111278=CARTESIAN_POINT('Ctrl Pts',(-8.53667982779111,7.43775210031699,
11.0518883911406));
#111279=CARTESIAN_POINT('Ctrl Pts',(-8.53576965607636,7.44014171143158,
11.0053272813691));
#111280=CARTESIAN_POINT('Ctrl Pts',(-8.53861279749361,7.44522030222767,
10.9043769718993));
#111281=CARTESIAN_POINT('Ctrl Pts',(-8.54318115389029,7.44788677725391,
10.8500814446646));
#111282=CARTESIAN_POINT('Ctrl Pts',(-8.56501475568105,7.45552339342862,
10.6948477772222));
#111283=CARTESIAN_POINT('Ctrl Pts',(-8.58984866165421,7.46042604266599,
10.5953168345938));
#111284=CARTESIAN_POINT('Ctrl Pts',(-8.6286190311255,7.46640178005219,10.4888564390466));
#111285=CARTESIAN_POINT('Ctrl Pts',(-8.63250359075304,7.46698821861286,
10.4785529191246));
#111286=CARTESIAN_POINT('Ctrl Pts',(-8.6380885556368,7.46781598684039,10.4642309345609));
#111287=CARTESIAN_POINT('Ctrl Pts',(-8.63969131894239,7.46805186037048,
10.4601745050189));
#111288=CARTESIAN_POINT('Ctrl Pts',(-8.6424915269101,7.46846119030437,10.4531791274877));
#111289=CARTESIAN_POINT('Ctrl Pts',(-8.64368045179287,7.46863414676286,
10.4502367747082));
#111290=CARTESIAN_POINT('Ctrl Pts',(-8.6462067249973,7.46899994385732,10.4440428253987));
#111291=CARTESIAN_POINT('Ctrl Pts',(-8.6475462309671,7.46919291675959,10.4407921555278));
#111292=CARTESIAN_POINT('Ctrl Pts',(-8.65088300145523,7.46967115685227,
10.4327767047353));
#111293=CARTESIAN_POINT('Ctrl Pts',(-8.65289379808268,7.46995721617623,
10.4280176387609));
#111294=CARTESIAN_POINT('Ctrl Pts',(-8.66044751025447,7.47102372081813,
10.4104006202979));
#111295=CARTESIAN_POINT('Ctrl Pts',(-8.66614949364902,7.47181294067455,
10.3976121692255));
#111296=CARTESIAN_POINT('Ctrl Pts',(-8.708343072968,7.47753288539119,10.3065174327056));
#111297=CARTESIAN_POINT('Ctrl Pts',(-8.75151952465032,7.48275757688047,
10.2315013602793));
#111298=CARTESIAN_POINT('Ctrl Pts',(-8.85934602088311,7.49406738642449,
10.0774638468247));
#111299=CARTESIAN_POINT('Ctrl Pts',(-8.92616227905056,7.50009912903132,
10.0004786383826));
#111300=CARTESIAN_POINT('Ctrl Pts',(-9.01393904228906,7.50683834941605,
9.91840018342532));
#111301=CARTESIAN_POINT('Ctrl Pts',(-9.02768800544782,7.50786505249159,
9.90602385556067));
#111302=CARTESIAN_POINT('Ctrl Pts',(-9.04724660510811,7.50928637575882,
9.88907799817574));
#111303=CARTESIAN_POINT('Ctrl Pts',(-9.05286141141777,7.5096900194238,9.88428712366565));
#111304=CARTESIAN_POINT('Ctrl Pts',(-9.06322696806261,7.51042727588632,
9.87557727744809));
#111305=CARTESIAN_POINT('Ctrl Pts',(-9.06796664882473,7.51076140441124,
9.87164544301977));
#111306=CARTESIAN_POINT('Ctrl Pts',(-9.07764240649234,7.51143753751119,
9.8637214166346));
#111307=CARTESIAN_POINT('Ctrl Pts',(-9.08257992664108,7.51177945977164,
9.85973118956467));
#111308=CARTESIAN_POINT('Ctrl Pts',(-9.0948820874528,7.51262381397045,9.84992090659537));
#111309=CARTESIAN_POINT('Ctrl Pts',(-9.10227711041635,7.51312472699741,
9.84413929225245));
#111310=CARTESIAN_POINT('Ctrl Pts',(-9.13052008034112,7.51501336155408,
9.82249279267344));
#111311=CARTESIAN_POINT('Ctrl Pts',(-9.15173769788368,7.51638223672181,
9.80711705064996));
#111312=CARTESIAN_POINT('Ctrl Pts',(-9.20653558845931,7.51980400613857,
9.7696085984048));
#111313=CARTESIAN_POINT('Ctrl Pts',(-9.24063673589528,7.52182946067538,
9.74827458882002));
#111314=CARTESIAN_POINT('Ctrl Pts',(-9.3315693783157,7.52702436290864,9.69647182498859));
#111315=CARTESIAN_POINT('Ctrl Pts',(-9.3896108368714,7.53013955325226,9.66830540558073));
#111316=CARTESIAN_POINT('Ctrl Pts',(-9.51889778889712,7.53694241915899,
9.61579896948401));
#111317=CARTESIAN_POINT('Ctrl Pts',(-9.59054064020714,7.54062991985508,
9.59294190404915));
#111318=CARTESIAN_POINT('Ctrl Pts',(-9.6753238596864,7.54521306543516,9.57291819426744));
#111319=CARTESIAN_POINT('Ctrl Pts',(-9.68706933190899,7.5458528440698,9.57029672486));
#111320=CARTESIAN_POINT('Ctrl Pts',(-9.70374826159777,7.54676988319813,
9.56678952758576));
#111321=CARTESIAN_POINT('Ctrl Pts',(-9.70865629456193,7.54704077793354,
9.5657837699402));
#111322=CARTESIAN_POINT('Ctrl Pts',(-9.71695284291605,7.54750060148584,
9.56412797886911));
#111323=CARTESIAN_POINT('Ctrl Pts',(-9.72033872045786,7.54768879282279,
9.56346468101053));
#111324=CARTESIAN_POINT('Ctrl Pts',(-9.72729999083386,7.54807686091922,
9.56212650286891));
#111325=CARTESIAN_POINT('Ctrl Pts',(-9.7308755899008,7.54827680760877,9.56145297607435));
#111326=CARTESIAN_POINT('Ctrl Pts',(-9.74009558932662,7.54879391449836,
9.55975180515244));
#111327=CARTESIAN_POINT('Ctrl Pts',(-9.74574353347414,7.54911215339402,
9.55874401563994));
#111328=CARTESIAN_POINT('Ctrl Pts',(-9.76963450282196,7.55046410257725,
9.55462583707972));
#111329=CARTESIAN_POINT('Ctrl Pts',(-9.78792898935511,7.55151358528922,
9.55182854790981));
#111330=CARTESIAN_POINT('Ctrl Pts',(-9.83766486347408,7.55439632991313,
9.54518636041899));
#111331=CARTESIAN_POINT('Ctrl Pts',(-9.86918523766847,7.55625505240864,
9.54201416261269));
#111332=CARTESIAN_POINT('Ctrl Pts',(-10.0194478175969,7.56519504215065,
9.53180359938533));
#111333=CARTESIAN_POINT('Ctrl Pts',(-10.1386737666099,7.57247589593899,
9.53823591789497));
#111334=CARTESIAN_POINT('Ctrl Pts',(-10.2980315212906,7.58184573626662,
9.56652567958855));
#111335=CARTESIAN_POINT('Ctrl Pts',(-10.3399095523836,7.5842786842282,9.57587450049699));
#111336=CARTESIAN_POINT('Ctrl Pts',(-10.3925169060043,7.58729656209602,
9.59007190331725));
#111337=CARTESIAN_POINT('Ctrl Pts',(-10.4036780259856,7.58793466176356,
9.59322680524494));
#111338=CARTESIAN_POINT('Ctrl Pts',(-10.4213480823094,7.58894163996855,
9.59844919593738));
#111339=CARTESIAN_POINT('Ctrl Pts',(-10.4278819243169,7.58931327970552,
9.60043009325276));
#111340=CARTESIAN_POINT('Ctrl Pts',(-10.4395979623734,7.58997846700903,
9.6040718174313));
#111341=CARTESIAN_POINT('Ctrl Pts',(-10.444785180374,7.59027254634624,9.60571595295905));
#111342=CARTESIAN_POINT('Ctrl Pts',(-10.456921533673,7.59095963784012,9.60963730057673));
#111343=CARTESIAN_POINT('Ctrl Pts',(-10.463863045253,7.59135188883806,9.61193775292204));
#111344=CARTESIAN_POINT('Ctrl Pts',(-10.4839187732104,7.59248323454975,
9.61875157351024));
#111345=CARTESIAN_POINT('Ctrl Pts',(-10.4969866356625,7.59321794224486,
9.62339951472864));
#111346=CARTESIAN_POINT('Ctrl Pts',(-10.526359988934,7.59486498593115,9.63431974902827));
#111347=CARTESIAN_POINT('Ctrl Pts',(-10.5426233248556,7.59577380163185,
9.64069968542083));
#111348=CARTESIAN_POINT('Ctrl Pts',(-10.5955223506516,7.5987238803772,9.66255216731971));
#111349=CARTESIAN_POINT('Ctrl Pts',(-10.6316431353479,7.60072821052824,
9.67922719009759));
#111350=CARTESIAN_POINT('Ctrl Pts',(-10.7625919203625,7.60803493000037,
9.74628167468931));
#111351=CARTESIAN_POINT('Ctrl Pts',(-10.8524619946855,7.61310817153911,
9.8055702820034));
#111352=CARTESIAN_POINT('Ctrl Pts',(-10.9355639916736,7.61852821411153,
9.87458774733009));
#111353=CARTESIAN_POINT('Ctrl Pts',(-10.9360916260817,7.61856266048545,
9.87502658317914));
#111354=CARTESIAN_POINT('Ctrl Pts',(-10.9564345214131,7.61989202797838,
9.89197007952741));
#111355=CARTESIAN_POINT('Ctrl Pts',(-10.9758094935386,7.6212053769002,9.90899449742122));
#111356=CARTESIAN_POINT('Ctrl Pts',(-11.0071288509552,7.62342718757964,
9.93801612348884));
#111357=CARTESIAN_POINT('Ctrl Pts',(-11.0193333456882,7.62431928497335,
9.94972491294196));
#111358=CARTESIAN_POINT('Ctrl Pts',(-11.0354094034414,7.62553460150051,
9.96569218859426));
#111359=CARTESIAN_POINT('Ctrl Pts',(-11.0394631709508,7.62584458533969,
9.96976624229819));
#111360=CARTESIAN_POINT('Ctrl Pts',(-11.0457917121337,7.62633429285329,
9.97620182876728));
#111361=CARTESIAN_POINT('Ctrl Pts',(-11.0480827695288,7.62651278095177,
9.97854735382787));
#111362=CARTESIAN_POINT('Ctrl Pts',(-11.0527583674781,7.62687956404507,
9.9833664012573));
#111363=CARTESIAN_POINT('Ctrl Pts',(-11.0551420830886,7.62706792199881,
9.98584062495737));
#111364=CARTESIAN_POINT('Ctrl Pts',(-11.0607906533447,7.62751748194107,
9.99174513830514));
#111365=CARTESIAN_POINT('Ctrl Pts',(-11.0640475996165,7.62777927342392,
9.99518291175387));
#111366=CARTESIAN_POINT('Ctrl Pts',(-11.0746968835869,7.62864358238071,
10.0065332845908));
#111367=CARTESIAN_POINT('Ctrl Pts',(-11.0820179195412,7.62925107941532,
10.0145119412173));
#111368=CARTESIAN_POINT('Ctrl Pts',(-11.1290963231606,7.63324099374901,
10.0669762339439));
#111369=CARTESIAN_POINT('Ctrl Pts',(-11.1661870582671,7.63677599153351,
10.113772980933));
#111370=CARTESIAN_POINT('Ctrl Pts',(-11.23313686152,7.6437894073516,10.2097488822825));
#111371=CARTESIAN_POINT('Ctrl Pts',(-11.2631642178905,7.64725864854721,
10.2586905477699));
#111372=CARTESIAN_POINT('Ctrl Pts',(-11.3294588923257,7.65564058228828,
10.3825246629181));
#111373=CARTESIAN_POINT('Ctrl Pts',(-11.3623710085283,7.66048071770189,
10.4589958229372));
#111374=CARTESIAN_POINT('Ctrl Pts',(-11.3924306932414,7.66577214313523,
10.5493173140078));
#111375=CARTESIAN_POINT('Ctrl Pts',(-11.3961026238444,7.66643892474545,
10.5608239591491));
#111376=CARTESIAN_POINT('Ctrl Pts',(-11.4018655978654,7.66752025244773,
10.5796863767382));
#111377=CARTESIAN_POINT('Ctrl Pts',(-11.4040421276465,7.66793753677938,
10.58701525057));
#111378=CARTESIAN_POINT('Ctrl Pts',(-11.4078381680992,7.66868175427716,
10.6001743498469));
#111379=CARTESIAN_POINT('Ctrl Pts',(-11.4094791273435,7.66900937019473,
10.605998160946));
#111380=CARTESIAN_POINT('Ctrl Pts',(-11.4128874020312,7.66970270638948,
10.6183880596459));
#111381=CARTESIAN_POINT('Ctrl Pts',(-11.4146451723637,7.67006811472332,
10.6249566394771));
#111382=CARTESIAN_POINT('Ctrl Pts',(-11.4192450801828,7.67104606754592,
10.642638517003));
#111383=CARTESIAN_POINT('Ctrl Pts',(-11.4220024771116,7.67165590978472,
10.6537734958682));
#111384=CARTESIAN_POINT('Ctrl Pts',(-11.4277792051918,7.67298853821813,
10.6783353407623));
#111385=CARTESIAN_POINT('Ctrl Pts',(-11.4307406584607,7.67370949908612,
10.6917747638016));
#111386=CARTESIAN_POINT('Ctrl Pts',(-11.4534527804026,7.67957299637897,
10.8022364208009));
#111387=CARTESIAN_POINT('Ctrl Pts',(-11.4634999999957,7.68439943215103,
10.9009878497116));
#111388=CARTESIAN_POINT('Ctrl Pts',(-11.4635,7.68921734064608,10.9999999999359));
#111389=CARTESIAN_POINT('Origin',(-10.,3.5,11.));
#111390=CARTESIAN_POINT('',(-11.4634998107004,8.26169270208058,10.9993373195887));
#111391=CARTESIAN_POINT('',(-11.4634997901989,8.18835865039335,10.9992163610944));
#111392=CARTESIAN_POINT('',(-11.4635,3.5,11.));
#111393=CARTESIAN_POINT('Ctrl Pts',(-11.4634997595702,8.26169269924574,
10.9991611090195));
#111394=CARTESIAN_POINT('Ctrl Pts',(-11.4634864167997,8.26051570058515,
10.9758837799716));
#111395=CARTESIAN_POINT('Ctrl Pts',(-11.4629177280139,8.25932189804874,
10.9526108535919));
#111396=CARTESIAN_POINT('Ctrl Pts',(-11.4611828866091,8.25744101470029,
10.9167096405711));
#111397=CARTESIAN_POINT('Ctrl Pts',(-11.4604072524839,8.25677105162849,
10.9040659166203));
#111398=CARTESIAN_POINT('Ctrl Pts',(-11.4591292642527,8.25584855081238,
10.8868857032675));
#111399=CARTESIAN_POINT('Ctrl Pts',(-11.4587696514038,8.25560324219304,
10.8823388042376));
#111400=CARTESIAN_POINT('Ctrl Pts',(-11.4581050060773,8.25517317865635,
10.8744070408744));
#111401=CARTESIAN_POINT('Ctrl Pts',(-11.4578094248404,8.25498892673962,
10.8710213951573));
#111402=CARTESIAN_POINT('Ctrl Pts',(-11.4572093906022,8.25462797069292,
10.8644141853886));
#111403=CARTESIAN_POINT('Ctrl Pts',(-11.4569060391381,8.25445132641096,
10.8611925282721));
#111404=CARTESIAN_POINT('Ctrl Pts',(-11.456231264577,8.25407046296591,10.8542722694741));
#111405=CARTESIAN_POINT('Ctrl Pts',(-11.4558564348213,8.25386606099449,
10.8505740720858));
#111406=CARTESIAN_POINT('Ctrl Pts',(-11.4548297689747,8.253324471006,10.840815364646));
#111407=CARTESIAN_POINT('Ctrl Pts',(-11.4541541585032,8.25298600896113,
10.8347574949308));
#111408=CARTESIAN_POINT('Ctrl Pts',(-11.4511332817111,8.25154483503597,
10.8091254382974));
#111409=CARTESIAN_POINT('Ctrl Pts',(-11.4484305683217,8.25042438498102,
10.789596313735));
#111410=CARTESIAN_POINT('Ctrl Pts',(-11.4410627984828,8.24772244227829,
10.7432708553536));
#111411=CARTESIAN_POINT('Ctrl Pts',(-11.4360436130229,8.24612793856456,
10.7165384601872));
#111412=CARTESIAN_POINT('Ctrl Pts',(-11.4082962911959,8.23836764545882,
10.588532800705));
#111413=CARTESIAN_POINT('Ctrl Pts',(-11.3755826569016,8.23202328267557,
10.489727053627));
#111414=CARTESIAN_POINT('Ctrl Pts',(-11.3164263539626,8.22361455592296,
10.3593734032248));
#111415=CARTESIAN_POINT('Ctrl Pts',(-11.2987248283428,8.22133837283691,
10.3242078901882));
#111416=CARTESIAN_POINT('Ctrl Pts',(-11.26710923146,8.21764552567718,10.2672437345054));
#111417=CARTESIAN_POINT('Ctrl Pts',(-11.2539977458552,8.216203463413,10.2450249537688));
#111418=CARTESIAN_POINT('Ctrl Pts',(-11.2353526367903,8.2142681916172,10.2152559866384));
#111419=CARTESIAN_POINT('Ctrl Pts',(-11.2303244844658,8.21375689657923,
10.2073960810805));
#111420=CARTESIAN_POINT('Ctrl Pts',(-11.2217565290376,8.21290305537858,
10.1942808368283));
#111421=CARTESIAN_POINT('Ctrl Pts',(-11.2182571907706,8.21255903630575,
10.1889995036791));
#111422=CARTESIAN_POINT('Ctrl Pts',(-11.2112852296377,8.21188276131197,
10.178624113085));
#111423=CARTESIAN_POINT('Ctrl Pts',(-11.2078144968864,8.2115504450325,10.173528949177));
#111424=CARTESIAN_POINT('Ctrl Pts',(-11.200100255582,8.21082122027339,10.1623565416016));
#111425=CARTESIAN_POINT('Ctrl Pts',(-11.1958425503987,8.21042485386706,
10.1562892769299));
#111426=CARTESIAN_POINT('Ctrl Pts',(-11.1806802429581,8.20903439996681,
10.1350282290229));
#111427=CARTESIAN_POINT('Ctrl Pts',(-11.169530443889,8.20804959612698,10.1200110324375));
#111428=CARTESIAN_POINT('Ctrl Pts',(-11.101400889668,8.20224255907475,10.0318332049646));
#111429=CARTESIAN_POINT('Ctrl Pts',(-11.0378596797326,8.19769125038252,
9.96400753382538));
#111430=CARTESIAN_POINT('Ctrl Pts',(-10.8975922000422,8.18858355248319,
9.84023347611682));
#111431=CARTESIAN_POINT('Ctrl Pts',(-10.8210025518596,8.18404442896131,
9.78481235785662));
#111432=CARTESIAN_POINT('Ctrl Pts',(-10.7311214273068,8.17859299652699,
9.73217082468049));
#111433=CARTESIAN_POINT('Ctrl Pts',(-10.7225682213949,8.17807295909361,
9.72727673269008));
#111434=CARTESIAN_POINT('Ctrl Pts',(-10.7091501056261,8.17725414549164,
9.71977782392446));
#111435=CARTESIAN_POINT('Ctrl Pts',(-10.7043186442631,8.17695871797525,
9.71711343528997));
#111436=CARTESIAN_POINT('Ctrl Pts',(-10.6952567086822,8.17640328338292,
9.71218270252671));
#111437=CARTESIAN_POINT('Ctrl Pts',(-10.6910299132703,8.17614367407504,
9.7099097162209));
#111438=CARTESIAN_POINT('Ctrl Pts',(-10.6837822932254,8.17569748302378,
9.70605809920393));
#111439=CARTESIAN_POINT('Ctrl Pts',(-10.68076695099,8.17551153967774,9.70446913374219));
#111440=CARTESIAN_POINT('Ctrl Pts',(-10.6748998471318,8.17514909528203,
9.7014035426121));
#111441=CARTESIAN_POINT('Ctrl Pts',(-10.6720487441228,8.17497267605955,
9.69992575292316));
#111442=CARTESIAN_POINT('Ctrl Pts',(-10.6651830792277,8.17454719150037,
9.69639574659041));
#111443=CARTESIAN_POINT('Ctrl Pts',(-10.6611638774789,8.17429757479693,
9.69435268758186));
#111444=CARTESIAN_POINT('Ctrl Pts',(-10.6464079546149,8.17337936488766,
9.68693749438024));
#111445=CARTESIAN_POINT('Ctrl Pts',(-10.6356149723367,8.17270432298697,
9.68167910751061));
#111446=CARTESIAN_POINT('Ctrl Pts',(-10.5566507580465,8.1677473100583,9.64440247938146));
#111447=CARTESIAN_POINT('Ctrl Pts',(-10.4861678174006,8.16323029296284,
9.61755880049686));
#111448=CARTESIAN_POINT('Ctrl Pts',(-10.3518027950886,8.1548017513757,9.5779367964271));
#111449=CARTESIAN_POINT('Ctrl Pts',(-10.2885146819234,8.15090242298709,
9.5637586949654));
#111450=CARTESIAN_POINT('Ctrl Pts',(-10.1850806543593,8.14474989359811,
9.5477024561384));
#111451=CARTESIAN_POINT('Ctrl Pts',(-10.1454326595844,8.14244154995233,
9.54319777126721));
#111452=CARTESIAN_POINT('Ctrl Pts',(-10.0796705421542,8.1387029529165,9.53843809657381));
#111453=CARTESIAN_POINT('Ctrl Pts',(-10.0536468584662,8.13724649259769,
9.53725165225554));
#111454=CARTESIAN_POINT('Ctrl Pts',(-10.0182414063516,8.13529530317956,
9.53658372525667));
#111455=CARTESIAN_POINT('Ctrl Pts',(-10.0088770404208,8.13478210175981,
9.53649696073565));
#111456=CARTESIAN_POINT('Ctrl Pts',(-9.99316997170365,8.13392597306222,
9.53650219465627));
#111457=CARTESIAN_POINT('Ctrl Pts',(-9.98682762507647,8.13358155559569,
9.53654553681148));
#111458=CARTESIAN_POINT('Ctrl Pts',(-9.97432683399538,8.13290516498559,
9.53671223718473));
#111459=CARTESIAN_POINT('Ctrl Pts',(-9.96816849439757,8.13257312653889,
9.53683324767879));
#111460=CARTESIAN_POINT('Ctrl Pts',(-9.95462290706325,8.13184530380463,
9.53718497727766));
#111461=CARTESIAN_POINT('Ctrl Pts',(-9.94723624771688,8.13145005373148,
9.53743278431064));
#111462=CARTESIAN_POINT('Ctrl Pts',(-9.92130077953414,8.13006782482262,
9.53849960614553));
#111463=CARTESIAN_POINT('Ctrl Pts',(-9.90276556184566,8.12908998141345,
9.53961564195093));
#111464=CARTESIAN_POINT('Ctrl Pts',(-9.78631631240663,8.12300103694166,
9.54885421329039));
#111465=CARTESIAN_POINT('Ctrl Pts',(-9.68940628282846,8.11819891164212,
9.56646634538527));
#111466=CARTESIAN_POINT('Ctrl Pts',(-9.52759275726565,8.11000461678469,
9.61306742850065));
#111467=CARTESIAN_POINT('Ctrl Pts',(-9.46168759014302,8.10660593824554,
9.63729347777784));
#111468=CARTESIAN_POINT('Ctrl Pts',(-9.37928739195133,8.10200781914097,
9.67449643773879));
#111469=CARTESIAN_POINT('Ctrl Pts',(-9.36097339661832,8.10096221804414,
9.68322789850165));
#111470=CARTESIAN_POINT('Ctrl Pts',(-9.33084201434401,8.09919295082646,
9.69837010837092));
#111471=CARTESIAN_POINT('Ctrl Pts',(-9.31892050305939,8.09847987531609,
9.70456822714081));
#111472=CARTESIAN_POINT('Ctrl Pts',(-9.30260901874348,8.09748380865861,
9.7133361320728));
#111473=CARTESIAN_POINT('Ctrl Pts',(-9.29814423059944,8.09720902944721,
9.71576615556808));
#111474=CARTESIAN_POINT('Ctrl Pts',(-9.2906282312651,8.09674270110176,9.71990774447461));
#111475=CARTESIAN_POINT('Ctrl Pts',(-9.28757028633244,8.09655191150049,
9.7216071058729));
#111476=CARTESIAN_POINT('Ctrl Pts',(-9.28173692445216,8.09618587506674,
9.72487625253952));
#111477=CARTESIAN_POINT('Ctrl Pts',(-9.27896050076673,8.09601075300766,
9.72644416801724));
#111478=CARTESIAN_POINT('Ctrl Pts',(-9.27234557479452,8.09559139644156,
9.73020834573471));
#111479=CARTESIAN_POINT('Ctrl Pts',(-9.26851188310388,8.09534664414556,
9.73241294517049));
#111480=CARTESIAN_POINT('Ctrl Pts',(-9.25484954374753,8.09446843329774,
9.74035221718689));
#111481=CARTESIAN_POINT('Ctrl Pts',(-9.24507811298438,8.09382923192695,
9.74618395784058));
#111482=CARTESIAN_POINT('Ctrl Pts',(-9.15333031157141,8.08772916501643,
9.80240175923716));
#111483=CARTESIAN_POINT('Ctrl Pts',(-9.07644841715503,8.08188458272259,
9.86064001305839));
#111484=CARTESIAN_POINT('Ctrl Pts',(-8.95449610729651,8.071899949597,9.97352569938206));
#111485=CARTESIAN_POINT('Ctrl Pts',(-8.90661936226839,8.06773896364083,
10.024680406677));
#111486=CARTESIAN_POINT('Ctrl Pts',(-8.83871158169893,8.06152979611651,
10.1085514366615));
#111487=CARTESIAN_POINT('Ctrl Pts',(-8.81599421848539,8.05938762165198,
10.1389529572969));
#111488=CARTESIAN_POINT('Ctrl Pts',(-8.78841526071043,8.05669893754897,
10.1790193835894));
#111489=CARTESIAN_POINT('Ctrl Pts',(-8.7824448312407,8.056111063646,10.1879001462068));
#111490=CARTESIAN_POINT('Ctrl Pts',(-8.7729340345619,8.05516484271529,10.2023877405371));
#111491=CARTESIAN_POINT('Ctrl Pts',(-8.7693335010373,8.0548042793897,10.2079544392391));
#111492=CARTESIAN_POINT('Ctrl Pts',(-8.76249985477756,8.05411532660058,
10.2186788803611));
#111493=CARTESIAN_POINT('Ctrl Pts',(-8.75926085884316,8.0537867261296,10.223832694222));
#111494=CARTESIAN_POINT('Ctrl Pts',(-8.7519319743256,8.05303839184356,10.2356573560826));
#111495=CARTESIAN_POINT('Ctrl Pts',(-8.74786322208443,8.05261943014049,
10.2423411277992));
#111496=CARTESIAN_POINT('Ctrl Pts',(-8.73517412397909,8.05130133479323,
10.2635670258701));
#111497=CARTESIAN_POINT('Ctrl Pts',(-8.72675186593977,8.05040928173178,
10.2782263221184));
#111498=CARTESIAN_POINT('Ctrl Pts',(-8.65869889191197,8.04304565585298,
10.4015751488433));
#111499=CARTESIAN_POINT('Ctrl Pts',(-8.61284792867623,8.03710476693989,
10.5172866849481));
#111500=CARTESIAN_POINT('Ctrl Pts',(-8.56384858926869,8.02744365456947,
10.7088880765153));
#111501=CARTESIAN_POINT('Ctrl Pts',(-8.55100129267519,8.02379684512443,
10.7816487034097));
#111502=CARTESIAN_POINT('Ctrl Pts',(-8.54281568212808,8.01940953676066,
10.8638935849525));
#111503=CARTESIAN_POINT('Ctrl Pts',(-8.54201674256544,8.01893435591819,
10.8727368639456));
#111504=CARTESIAN_POINT('Ctrl Pts',(-8.54094996169062,8.01822240791579,
10.8858782453035));
#111505=CARTESIAN_POINT('Ctrl Pts',(-8.54062052708183,8.01798890672005,
10.8901713049565));
#111506=CARTESIAN_POINT('Ctrl Pts',(-8.54006616289705,8.0175701204292,10.8978389526661));
#111507=CARTESIAN_POINT('Ctrl Pts',(-8.53983398059039,8.01738523684094,
10.9012129372323));
#111508=CARTESIAN_POINT('Ctrl Pts',(-8.53935335075794,8.01698078019691,
10.9085694911119));
#111509=CARTESIAN_POINT('Ctrl Pts',(-8.5391094982778,8.01676096636294,10.912552226442));
#111510=CARTESIAN_POINT('Ctrl Pts',(-8.53847474490722,8.0161454128513,10.9236641796471));
#111511=CARTESIAN_POINT('Ctrl Pts',(-8.5381197294417,8.01574778286453,10.9307952378733));
#111512=CARTESIAN_POINT('Ctrl Pts',(-8.53643209474614,8.01351763880237,
10.970549864329));
#111513=CARTESIAN_POINT('Ctrl Pts',(-8.536139441446,8.01163551675328,11.003206213463));
#111514=CARTESIAN_POINT('Ctrl Pts',(-8.53734383931992,8.00875279562614,
11.0523687694782));
#111515=CARTESIAN_POINT('Ctrl Pts',(-8.53802868107255,8.00777582323257,
11.068886639336));
#111516=CARTESIAN_POINT('Ctrl Pts',(-8.54391603292052,8.00177889571196,
11.1696193619885));
#111517=CARTESIAN_POINT('Ctrl Pts',(-8.55611362085474,7.99664436250698,
11.2532668649875));
#111518=CARTESIAN_POINT('Ctrl Pts',(-8.59078684908308,7.9876672006377,11.4005350885795));
#111519=CARTESIAN_POINT('Ctrl Pts',(-8.61057307455072,7.98378514914999,
11.4645478807354));
#111520=CARTESIAN_POINT('Ctrl Pts',(-8.64073056356577,7.97910136331877,
11.5426801680854));
#111521=CARTESIAN_POINT('Ctrl Pts',(-8.6470575091315,7.97816948212285,11.5582667955786));
#111522=CARTESIAN_POINT('Ctrl Pts',(-8.6567465424071,7.97681336645421,11.5810031922856));
#111523=CARTESIAN_POINT('Ctrl Pts',(-8.65989988888751,7.97638221188876,
11.588239964964));
#111524=CARTESIAN_POINT('Ctrl Pts',(-8.66558472747087,7.97562255543015,
11.6010033908312));
#111525=CARTESIAN_POINT('Ctrl Pts',(-8.66809237102331,7.97529325954224,
11.606540406538));
#111526=CARTESIAN_POINT('Ctrl Pts',(-8.67341982918387,7.97460559466635,
11.6181113630333));
#111527=CARTESIAN_POINT('Ctrl Pts',(-8.67624648875098,7.97424746750451,
11.6241420112194));
#111528=CARTESIAN_POINT('Ctrl Pts',(-8.68378182625239,7.97331009368449,
11.6399370902177));
#111529=CARTESIAN_POINT('Ctrl Pts',(-8.6885580433488,7.97273316522437,11.6496689642238));
#111530=CARTESIAN_POINT('Ctrl Pts',(-8.7093997210082,7.97028649146057,11.6909687014452));
#111531=CARTESIAN_POINT('Ctrl Pts',(-8.72650081102523,7.96845261375559,
11.7220020081914));
#111532=CARTESIAN_POINT('Ctrl Pts',(-8.81931062604574,7.95926794952584,
11.8768467921363));
#111533=CARTESIAN_POINT('Ctrl Pts',(-8.91199182485794,7.9525584411088,11.9895042253733));
#111534=CARTESIAN_POINT('Ctrl Pts',(-9.03511869094809,7.94413331061099,
12.1005755604578));
#111535=CARTESIAN_POINT('Ctrl Pts',(-9.05081353369598,7.94306517624342,
12.1141397958369));
#111536=CARTESIAN_POINT('Ctrl Pts',(-9.07731241337673,7.94126128483738,
12.1360750124462));
#111537=CARTESIAN_POINT('Ctrl Pts',(-9.08795522573274,7.9405366574741,12.1446366758369));
#111538=CARTESIAN_POINT('Ctrl Pts',(-9.10274667960778,7.93952700633262,
12.1561984702662));
#111539=CARTESIAN_POINT('Ctrl Pts',(-9.10679386655468,7.93925049056074,
12.1593279196178));
#111540=CARTESIAN_POINT('Ctrl Pts',(-9.11364124719736,7.93878206909761,
12.1645654537245));
#111541=CARTESIAN_POINT('Ctrl Pts',(-9.11643279874338,7.93859093882967,
12.1666848482997));
#111542=CARTESIAN_POINT('Ctrl Pts',(-9.12177314070547,7.93822493378267,
12.1707091690824));
#111543=CARTESIAN_POINT('Ctrl Pts',(-9.12432057269585,7.93805018836196,
12.1726158429585));
#111544=CARTESIAN_POINT('Ctrl Pts',(-9.1304028876468,7.93763263469327,12.1771373943867));
#111545=CARTESIAN_POINT('Ctrl Pts',(-9.13394335590712,7.93738931848249,
12.1797446635967));
#111546=CARTESIAN_POINT('Ctrl Pts',(-9.14656392341383,7.93652121371726,
12.188951266028));
#111547=CARTESIAN_POINT('Ctrl Pts',(-9.15570790812537,7.93589084800901,
12.1954618763893));
#111548=CARTESIAN_POINT('Ctrl Pts',(-9.24673678398372,7.9296091451164,12.2587100720652));
#111549=CARTESIAN_POINT('Ctrl Pts',(-9.33413253089751,7.92354643585885,
12.3070480626427));
#111550=CARTESIAN_POINT('Ctrl Pts',(-9.5168796120167,7.91161790513388,12.385006207289));
#111551=CARTESIAN_POINT('Ctrl Pts',(-9.61173077356932,7.90578647236496,
12.4145318443178));
#111552=CARTESIAN_POINT('Ctrl Pts',(-9.72244061947996,7.89950157636633,
12.4370056787119));
#111553=CARTESIAN_POINT('Ctrl Pts',(-9.7360688009411,7.89873614922377,12.4395710718936));
#111554=CARTESIAN_POINT('Ctrl Pts',(-9.75693490329717,7.89757643514967,
12.4431926612901));
#111555=CARTESIAN_POINT('Ctrl Pts',(-9.76414743979807,7.89717778888479,
12.4443888920172));
#111556=CARTESIAN_POINT('Ctrl Pts',(-9.7767418903623,7.89648546542641,12.4463808832964));
#111557=CARTESIAN_POINT('Ctrl Pts',(-9.78211979648902,7.89619104002323,
12.4472007673798));
#111558=CARTESIAN_POINT('Ctrl Pts',(-9.79425503338721,7.89552932660027,
12.4489816567372));
#111559=CARTESIAN_POINT('Ctrl Pts',(-9.80101479270884,7.89516258232947,
12.4499254195564));
#111560=CARTESIAN_POINT('Ctrl Pts',(-9.81927381426264,7.89417682239226,
12.4523445525943));
#111561=CARTESIAN_POINT('Ctrl Pts',(-9.83078453914054,7.89356058700529,
12.4537306462004));
#111562=CARTESIAN_POINT('Ctrl Pts',(-9.88491769985231,7.89068556752297,
12.4595975438514));
#111563=CARTESIAN_POINT('Ctrl Pts',(-9.92770900113951,7.8884807025409,12.4623417429202));
#111564=CARTESIAN_POINT('Ctrl Pts',(-9.99149861199725,7.88526236244208,
12.4636251231227));
#111565=CARTESIAN_POINT('Ctrl Pts',(-10.01244240482,7.88421649677356,12.4635969386559));
#111566=CARTESIAN_POINT('Ctrl Pts',(-10.1313992827198,7.87831801824072,
12.4608831188763));
#111567=CARTESIAN_POINT('Ctrl Pts',(-10.2289415353001,7.8736609838397,12.4488028516785));
#111568=CARTESIAN_POINT('Ctrl Pts',(-10.3553897213718,7.86719990921243,
12.4200462452602));
#111569=CARTESIAN_POINT('Ctrl Pts',(-10.3860024950595,7.86559991591479,
12.4120322424405));
#111570=CARTESIAN_POINT('Ctrl Pts',(-10.4340567846516,7.86299820623345,
12.3977728264003));
#111571=CARTESIAN_POINT('Ctrl Pts',(-10.4516816977724,7.86202433206106,
12.392177340711));
#111572=CARTESIAN_POINT('Ctrl Pts',(-10.4746268374049,7.86072497745424,
12.3844112465397));
#111573=CARTESIAN_POINT('Ctrl Pts',(-10.4800476882087,7.86041567289538,
12.3825409032618));
#111574=CARTESIAN_POINT('Ctrl Pts',(-10.4888886276334,7.8599072001777,12.3794322706587));
#111575=CARTESIAN_POINT('Ctrl Pts',(-10.4923153907611,7.8597091226726,12.3782129860776));
#111576=CARTESIAN_POINT('Ctrl Pts',(-10.4989830432694,7.85932171112839,
12.3758125130659));
#111577=CARTESIAN_POINT('Ctrl Pts',(-10.5022243519322,7.85913245221642,
12.3746326229606));
#111578=CARTESIAN_POINT('Ctrl Pts',(-10.5101624117455,7.85866672228905,
12.3717112146059));
#111579=CARTESIAN_POINT('Ctrl Pts',(-10.5148544309898,7.85838952028002,
12.369957027072));
#111580=CARTESIAN_POINT('Ctrl Pts',(-10.5307883911688,7.85744183679314,
12.363906439038));
#111581=CARTESIAN_POINT('Ctrl Pts',(-10.5419860102289,7.85676512040187,
12.3594955816079));
#111582=CARTESIAN_POINT('Ctrl Pts',(-10.6226478189352,7.85181895954054,
12.3265671629433));
#111583=CARTESIAN_POINT('Ctrl Pts',(-10.6898751322926,7.84731602813228,
12.2928809571515));
#111584=CARTESIAN_POINT('Ctrl Pts',(-10.8094296251383,7.83892241618557,
12.2209861087014));
#111585=CARTESIAN_POINT('Ctrl Pts',(-10.8623942811609,7.83504394343544,
12.1841707321315));
#111586=CARTESIAN_POINT('Ctrl Pts',(-10.9442002393989,7.82889005692504,
12.1188993280703));
#111587=CARTESIAN_POINT('Ctrl Pts',(-10.9745926470737,7.82656151224971,
12.092528886242));
#111588=CARTESIAN_POINT('Ctrl Pts',(-11.0229284200694,7.82279423510194,
12.0469652572292));
#111589=CARTESIAN_POINT('Ctrl Pts',(-11.0415094834993,7.82132878125215,
12.0284828252419));
#111590=CARTESIAN_POINT('Ctrl Pts',(-11.0660592401253,7.81936765953194,
12.0027153313425));
#111591=CARTESIAN_POINT('Ctrl Pts',(-11.0724679240559,7.81885327574522,
11.9958578697631));
#111592=CARTESIAN_POINT('Ctrl Pts',(-11.0830990247742,7.81799572775894,
11.9842606533324));
#111593=CARTESIAN_POINT('Ctrl Pts',(-11.0873573130261,7.81765106262433,
11.9795542898343));
#111594=CARTESIAN_POINT('Ctrl Pts',(-11.0956854056592,7.81697459635997,
11.9702286531604));
#111595=CARTESIAN_POINT('Ctrl Pts',(-11.0997569427431,7.81664272688003,
11.9656111101594));
#111596=CARTESIAN_POINT('Ctrl Pts',(-11.1086435564058,7.81591576069624,
11.9554036547644));
#111597=CARTESIAN_POINT('Ctrl Pts',(-11.1134457605037,7.81552119340651,
11.9498027267798));
#111598=CARTESIAN_POINT('Ctrl Pts',(-11.1301304938975,7.81414397814236,
11.9300424654383));
#111599=CARTESIAN_POINT('Ctrl Pts',(-11.1417872083514,7.81317037587054,
11.9156942348498));
#111600=CARTESIAN_POINT('Ctrl Pts',(-11.2159952712165,7.80688749904757,
11.8207305818259));
#111601=CARTESIAN_POINT('Ctrl Pts',(-11.2702422955657,7.80191495581177,
11.7339823850138));
#111602=CARTESIAN_POINT('Ctrl Pts',(-11.3445360818144,7.79367758349093,
11.5818727220127));
#111603=CARTESIAN_POINT('Ctrl Pts',(-11.3698442877853,7.79041103265121,
11.5194984311657));
#111604=CARTESIAN_POINT('Ctrl Pts',(-11.3969459205945,7.78597894418571,
11.4367693004369));
#111605=CARTESIAN_POINT('Ctrl Pts',(-11.4027343684134,7.78495622183093,
11.4178056418038));
#111606=CARTESIAN_POINT('Ctrl Pts',(-11.411734266184,7.78322218827329,11.3860221229114));
#111607=CARTESIAN_POINT('Ctrl Pts',(-11.4151606170667,7.78252093447687,
11.3732654839871));
#111608=CARTESIAN_POINT('Ctrl Pts',(-11.419657391117,7.78153878708231,11.355570861964));
#111609=CARTESIAN_POINT('Ctrl Pts',(-11.4208757106502,7.78126580783051,
11.3506707278953));
#111610=CARTESIAN_POINT('Ctrl Pts',(-11.4228935814655,7.78080164423534,
11.3423715788638));
#111611=CARTESIAN_POINT('Ctrl Pts',(-11.423706382874,7.78061120303904,11.3389757768865));
#111612=CARTESIAN_POINT('Ctrl Pts',(-11.4252397904852,7.780245113233,11.3324665429807));
#111613=CARTESIAN_POINT('Ctrl Pts',(-11.4259623624624,7.780069584556,11.3293536139484));
#111614=CARTESIAN_POINT('Ctrl Pts',(-11.4276666341271,7.77964829475175,
11.3219006546947));
#111615=CARTESIAN_POINT('Ctrl Pts',(-11.4286387413593,7.77940200527548,
11.3175584911955));
#111616=CARTESIAN_POINT('Ctrl Pts',(-11.43206486752,7.77851216221731,11.3019206520528));
#111617=CARTESIAN_POINT('Ctrl Pts',(-11.4344047783189,7.77786266848706,
11.2906007226145));
#111618=CARTESIAN_POINT('Ctrl Pts',(-11.4544136213632,7.77191557802975,
11.1876663162052));
#111619=CARTESIAN_POINT('Ctrl Pts',(-11.4634164151182,7.76625774086926,
11.0945920198759));
#111620=CARTESIAN_POINT('Ctrl Pts',(-11.463499806902,7.76062354882082,11.000868104301));
#111621=CARTESIAN_POINT('Ctrl Pts',(-11.4635,7.76059745675011,11.0004340499109));
#111622=CARTESIAN_POINT('Ctrl Pts',(-11.4635,7.76057136598891,11.0000000000874));
#111623=CARTESIAN_POINT('',(-11.4634994441716,7.68928058350007,11.0012989883455));
#111624=CARTESIAN_POINT('Ctrl Pts',(-11.4635,7.68921734064608,10.9999999999359));
#111625=CARTESIAN_POINT('Ctrl Pts',(-11.4635,7.68923840923771,11.0004329775571));
#111626=CARTESIAN_POINT('Ctrl Pts',(-11.4634998078549,7.68925947810631,
11.0008659601426));
#111627=CARTESIAN_POINT('Ctrl Pts',(-11.4634994235514,7.68928054728939,
11.0012989475658));
#111628=CARTESIAN_POINT('Ctrl Pts',(-11.4634994235137,7.68928054935369,
11.0012989899887));
#111629=CARTESIAN_POINT('Ctrl Pts',(-11.4634190836016,7.69368498754126,
11.0918134790247));
#111630=CARTESIAN_POINT('Ctrl Pts',(-11.4549417134562,7.69807278572729,
11.1821153036776));
#111631=CARTESIAN_POINT('Ctrl Pts',(-11.4367852399318,7.70324800997049,
11.2784552169745));
#111632=CARTESIAN_POINT('Ctrl Pts',(-11.4353311770417,7.70364882957371,
11.2858558050101));
#111633=CARTESIAN_POINT('Ctrl Pts',(-11.4328983795781,7.7042988236619,11.297750969576));
#111634=CARTESIAN_POINT('Ctrl Pts',(-11.4319555261105,7.70454615127574,
11.3022528349211));
#111635=CARTESIAN_POINT('Ctrl Pts',(-11.4301047594257,7.70502316788668,
11.3108866745424));
#111636=CARTESIAN_POINT('Ctrl Pts',(-11.4292001191023,7.70525267803507,
11.3150193105026));
#111637=CARTESIAN_POINT('Ctrl Pts',(-11.4276119976659,7.70564951717479,
11.3221266051275));
#111638=CARTESIAN_POINT('Ctrl Pts',(-11.4269371124375,7.70581635994053,
11.3251031260352));
#111639=CARTESIAN_POINT('Ctrl Pts',(-11.4253749339021,7.70619852752224,
11.3318943910655));
#111640=CARTESIAN_POINT('Ctrl Pts',(-11.4244816506068,7.70641418384707,
11.3357076337634));
#111641=CARTESIAN_POINT('Ctrl Pts',(-11.421992473739,7.70700729330801,11.3461445871728));
#111642=CARTESIAN_POINT('Ctrl Pts',(-11.4203656347107,7.70738642764274,
11.3527607272227));
#111643=CARTESIAN_POINT('Ctrl Pts',(-11.4118258237233,7.70933361574373,
11.3864739794682));
#111644=CARTESIAN_POINT('Ctrl Pts',(-11.4041837878065,7.71093797190499,
11.4133787368306));
#111645=CARTESIAN_POINT('Ctrl Pts',(-11.3875659331127,7.71415965687219,
11.4660886731694));
#111646=CARTESIAN_POINT('Ctrl Pts',(-11.3786285912183,7.71577519582412,
11.4918952756727));
#111647=CARTESIAN_POINT('Ctrl Pts',(-11.3595435726369,7.71899418465574,
11.5423883391644));
#111648=CARTESIAN_POINT('Ctrl Pts',(-11.3494318170698,7.72059648400974,
11.5670780942936));
#111649=CARTESIAN_POINT('Ctrl Pts',(-11.3056900203881,7.72710749897456,
11.6660759875016));
#111650=CARTESIAN_POINT('Ctrl Pts',(-11.2665480177364,7.73201515679448,
11.7377952809545));
#111651=CARTESIAN_POINT('Ctrl Pts',(-11.196322377239,7.73941999909446,11.8442496850267));
#111652=CARTESIAN_POINT('Ctrl Pts',(-11.1692181827876,7.74203269372293,
11.8814047014345));
#111653=CARTESIAN_POINT('Ctrl Pts',(-11.1330538131279,7.74522946179679,
11.9263687110538));
#111654=CARTESIAN_POINT('Ctrl Pts',(-11.125589995688,7.74587518075914,11.9354234897006));
#111655=CARTESIAN_POINT('Ctrl Pts',(-11.1135931060359,7.74689135287718,
11.9496260651385));
#111656=CARTESIAN_POINT('Ctrl Pts',(-11.1091314686049,7.74726465410854,
11.9548333137128));
#111657=CARTESIAN_POINT('Ctrl Pts',(-11.1006699922172,7.7479640826584,11.9645695018436));
#111658=CARTESIAN_POINT('Ctrl Pts',(-11.0966783966775,7.74829053523432,
11.9691053871595));
#111659=CARTESIAN_POINT('Ctrl Pts',(-11.0876326404212,7.74902260269109,
11.9792571515646));
#111660=CARTESIAN_POINT('Ctrl Pts',(-11.0825628315591,7.74942755912315,
11.9848588975205));
#111661=CARTESIAN_POINT('Ctrl Pts',(-11.0694773730217,7.7504594016223,11.9990941791225));
#111662=CARTESIAN_POINT('Ctrl Pts',(-11.0614003642233,7.75108370772191,
12.0076707337359));
#111663=CARTESIAN_POINT('Ctrl Pts',(-11.0053360651424,7.75533406773171,
12.0657803912766));
#111664=CARTESIAN_POINT('Ctrl Pts',(-10.9540009474293,7.75880992968169,
12.1119676750545));
#111665=CARTESIAN_POINT('Ctrl Pts',(-10.8194809492821,7.7672197772654,12.2167987811237));
#111666=CARTESIAN_POINT('Ctrl Pts',(-10.7330916586681,7.77203449804421,
12.2707173193917));
#111667=CARTESIAN_POINT('Ctrl Pts',(-10.6093024626622,7.77898255081495,
12.3311243967917));
#111668=CARTESIAN_POINT('Ctrl Pts',(-10.5762072605312,7.78084671267582,
12.3457809797531));
#111669=CARTESIAN_POINT('Ctrl Pts',(-10.5361943283622,7.78314609879579,
12.3617545847397));
#111670=CARTESIAN_POINT('Ctrl Pts',(-10.5297650417542,7.78351694054014,
12.3642686332424));
#111671=CARTESIAN_POINT('Ctrl Pts',(-10.5195734326441,7.78410731782829,
12.3681709609848));
#111672=CARTESIAN_POINT('Ctrl Pts',(-10.5158226975673,7.7843251269959,12.3695894546494));
#111673=CARTESIAN_POINT('Ctrl Pts',(-10.5088985037763,7.78472829262217,
12.3721756436949));
#111674=CARTESIAN_POINT('Ctrl Pts',(-10.5057267882593,7.78491338677897,
12.3733477707008));
#111675=CARTESIAN_POINT('Ctrl Pts',(-10.4985285853816,7.78533439904986,
12.3759795938061));
#111676=CARTESIAN_POINT('Ctrl Pts',(-10.4944997552563,7.78557069721068,
12.3774326060151));
#111677=CARTESIAN_POINT('Ctrl Pts',(-10.4840349262179,7.78618607278444,
12.3811549559348));
#111678=CARTESIAN_POINT('Ctrl Pts',(-10.4775894005346,7.78656665503836,
12.3833969722983));
#111679=CARTESIAN_POINT('Ctrl Pts',(-10.4344952930847,7.78912043756124,
12.3980497983563));
#111680=CARTESIAN_POINT('Ctrl Pts',(-10.3973852673983,7.79136376991451,
12.4090471475469));
#111681=CARTESIAN_POINT('Ctrl Pts',(-10.2607681729708,7.79967713226848,
12.4437066787406));
#111682=CARTESIAN_POINT('Ctrl Pts',(-10.1592865351854,7.80593319436265,
12.4583958448996));
#111683=CARTESIAN_POINT('Ctrl Pts',(-10.0133428077127,7.81455590384069,
12.4640941451296));
#111684=CARTESIAN_POINT('Ctrl Pts',(-9.96953033525498,7.81710068151394,
12.4638380359867));
#111685=CARTESIAN_POINT('Ctrl Pts',(-9.90717085812578,7.82064963712858,
12.460671986689));
#111686=CARTESIAN_POINT('Ctrl Pts',(-9.88856862256505,7.82169915772471,
12.4593707529206));
#111687=CARTESIAN_POINT('Ctrl Pts',(-9.85545048632595,7.82355149027602,
12.456417156809));
#111688=CARTESIAN_POINT('Ctrl Pts',(-9.84092513326514,7.82435834933385,
12.4549023008203));
#111689=CARTESIAN_POINT('Ctrl Pts',(-9.81901420147948,7.82556739315652,
12.4522851258648));
#111690=CARTESIAN_POINT('Ctrl Pts',(-9.81161068268768,7.82597452389837,
12.4513433136478));
#111691=CARTESIAN_POINT('Ctrl Pts',(-9.79828914330987,7.82670466288694,
12.4495450083023));
#111692=CARTESIAN_POINT('Ctrl Pts',(-9.79236859005619,7.82702829435056,
12.4487088043736));
#111693=CARTESIAN_POINT('Ctrl Pts',(-9.779625687343,7.82772304208109,12.4468293065368));
#111694=CARTESIAN_POINT('Ctrl Pts',(-9.77280523956981,7.82809377520274,
12.4457739875189));
#111695=CARTESIAN_POINT('Ctrl Pts',(-9.75450821001206,7.82908545528883,
12.4428102365794));
#111696=CARTESIAN_POINT('Ctrl Pts',(-9.74304636873106,7.82970362611249,
12.4408131174581));
#111697=CARTESIAN_POINT('Ctrl Pts',(-9.68719435328049,7.83270239391885,
12.430393729704));
#111698=CARTESIAN_POINT('Ctrl Pts',(-9.64318467142702,7.83502251694066,
12.4200552520324));
#111699=CARTESIAN_POINT('Ctrl Pts',(-9.49287043064012,7.84288605485962,
12.3773133220856));
#111700=CARTESIAN_POINT('Ctrl Pts',(-9.38983281309044,7.84814203186436,
12.3348660077122));
#111701=CARTESIAN_POINT('Ctrl Pts',(-9.24722868801146,7.85621904635855,
12.2561260472624));
#111702=CARTESIAN_POINT('Ctrl Pts',(-9.20323324608593,7.85884316342265,
12.2286899543104));
#111703=CARTESIAN_POINT('Ctrl Pts',(-9.15447821090923,7.86201336933541,
12.1945645663843));
#111704=CARTESIAN_POINT('Ctrl Pts',(-9.14820190729647,7.86242671838513,
12.1900973083041));
#111705=CARTESIAN_POINT('Ctrl Pts',(-9.13866609243517,7.86306326898607,
12.1831959666657));
#111706=CARTESIAN_POINT('Ctrl Pts',(-9.13538088026638,7.86328413510992,
12.1807974309059));
#111707=CARTESIAN_POINT('Ctrl Pts',(-9.1293857419162,7.8636901503683,12.1763819428009));
#111708=CARTESIAN_POINT('Ctrl Pts',(-9.12667276230554,7.86387500942836,
12.1743692762748));
#111709=CARTESIAN_POINT('Ctrl Pts',(-9.12059137079255,7.86429192173959,
12.1698249731735));
#111710=CARTESIAN_POINT('Ctrl Pts',(-9.11722693457747,7.8645243226174,12.1672881902264));
#111711=CARTESIAN_POINT('Ctrl Pts',(-9.10738786649167,7.86520899877992,
12.1598026729463));
#111712=CARTESIAN_POINT('Ctrl Pts',(-9.10094366504352,7.86566387502757,
12.1548144272894));
#111713=CARTESIAN_POINT('Ctrl Pts',(-9.04034924594162,7.86999968793884,
12.1070956710803));
#111714=CARTESIAN_POINT('Ctrl Pts',(-8.98924704304983,7.87409944965126,
12.0606446003566));
#111715=CARTESIAN_POINT('Ctrl Pts',(-8.88496051018156,7.88316459084927,
11.9514454053834));
#111716=CARTESIAN_POINT('Ctrl Pts',(-8.83338916047024,7.88812616249957,
11.8874583167264));
#111717=CARTESIAN_POINT('Ctrl Pts',(-8.75626213008583,7.89619171918246,
11.7733373097826));
#111718=CARTESIAN_POINT('Ctrl Pts',(-8.72773165158282,7.89937692802259,
11.7254439082916));
#111719=CARTESIAN_POINT('Ctrl Pts',(-8.69645461676477,7.90313014601722,
11.6653914035331));
#111720=CARTESIAN_POINT('Ctrl Pts',(-8.69104178641452,7.90379086791373,
11.6546790764457));
#111721=CARTESIAN_POINT('Ctrl Pts',(-8.68271863939418,7.90482512865225,
11.6376910611875));
#111722=CARTESIAN_POINT('Ctrl Pts',(-8.67972007360504,7.90520168985487,
11.6314594133897));
#111723=CARTESIAN_POINT('Ctrl Pts',(-8.67418747242458,7.90590405388116,
11.6197498016745));
#111724=CARTESIAN_POINT('Ctrl Pts',(-8.671642944657,7.90623020988444,11.6142769814781));
#111725=CARTESIAN_POINT('Ctrl Pts',(-8.66602442064201,7.90695754991232,
11.6019943713698));
#111726=CARTESIAN_POINT('Ctrl Pts',(-8.662968557807,7.90735811279552,11.5951764401221));
#111727=CARTESIAN_POINT('Ctrl Pts',(-8.6553397935828,7.90837109930553,11.5778006159515));
#111728=CARTESIAN_POINT('Ctrl Pts',(-8.65083889311554,7.908981104441,11.5672115479366));
#111729=CARTESIAN_POINT('Ctrl Pts',(-8.62315800396993,7.91281483970639,
11.4998937251341));
#111730=CARTESIAN_POINT('Ctrl Pts',(-8.60343425463699,7.91592185945244,
11.4418063450803));
#111731=CARTESIAN_POINT('Ctrl Pts',(-8.56169064154546,7.92383852963405,
11.2877049284104));
#111732=CARTESIAN_POINT('Ctrl Pts',(-8.5456106443231,7.92851010290634,11.1904158780445));
#111733=CARTESIAN_POINT('Ctrl Pts',(-8.53741334429938,7.93498890228566,
11.0606329410233));
#111734=CARTESIAN_POINT('Ctrl Pts',(-8.53644360842882,7.93659108732605,
11.0289577979744));
#111735=CARTESIAN_POINT('Ctrl Pts',(-8.5365369599794,7.93919606827804,10.978767520455));
#111736=CARTESIAN_POINT('Ctrl Pts',(-8.53692256662853,7.94017093982024,
10.9602602335768));
#111737=CARTESIAN_POINT('Ctrl Pts',(-8.53788735328215,7.94147149567726,
10.9360329839244));
#111738=CARTESIAN_POINT('Ctrl Pts',(-8.53814936931937,7.94178096923293,
10.9303013470084));
#111739=CARTESIAN_POINT('Ctrl Pts',(-8.53863261121367,7.94228968599261,
10.9209377176078));
#111740=CARTESIAN_POINT('Ctrl Pts',(-8.53883369354465,7.94248783709761,
10.9173046930377));
#111741=CARTESIAN_POINT('Ctrl Pts',(-8.53925183810509,7.94287536559478,
10.9102282808228));
#111742=CARTESIAN_POINT('Ctrl Pts',(-8.53946753185463,7.94306466761138,
10.9067848577892));
#111743=CARTESIAN_POINT('Ctrl Pts',(-8.5400262664723,7.94353046656658,10.8983434962636));
#111744=CARTESIAN_POINT('Ctrl Pts',(-8.5403827967072,7.94380769445833,10.8933465157887));
#111745=CARTESIAN_POINT('Ctrl Pts',(-8.54168288047267,7.94475524206195,
10.876354541451));
#111746=CARTESIAN_POINT('Ctrl Pts',(-8.5427486747948,7.94543179279293,10.8643697055457));
#111747=CARTESIAN_POINT('Ctrl Pts',(-8.55154424014717,7.95038284399966,
10.7776037355537));
#111748=CARTESIAN_POINT('Ctrl Pts',(-8.56487788396161,7.95489139453252,
10.7035091596081));
#111749=CARTESIAN_POINT('Ctrl Pts',(-8.60013784970108,7.96330028644251,
10.5682703942036));
#111750=CARTESIAN_POINT('Ctrl Pts',(-8.62055494429744,7.96718843065789,
10.5069110986626));
#111751=CARTESIAN_POINT('Ctrl Pts',(-8.66009499784457,7.97334154157597,
10.4100070084404));
#111752=CARTESIAN_POINT('Ctrl Pts',(-8.67674727870176,7.97566057435793,
10.3735498640916));
#111753=CARTESIAN_POINT('Ctrl Pts',(-8.70669836901665,7.97941443387721,
10.3145177645699));
#111754=CARTESIAN_POINT('Ctrl Pts',(-8.71914345323122,7.98087573627726,
10.2915357221526));
#111755=CARTESIAN_POINT('Ctrl Pts',(-8.73688237588209,7.98283236223632,
10.2607746939086));
#111756=CARTESIAN_POINT('Ctrl Pts',(-8.74164496198704,7.98334628799769,
10.2526963203974));
#111757=CARTESIAN_POINT('Ctrl Pts',(-8.74976036284207,7.98420335316183,
10.2392284344063));
#111758=CARTESIAN_POINT('Ctrl Pts',(-8.75307113977296,7.98454798884169,
10.2338140273876));
#111759=CARTESIAN_POINT('Ctrl Pts',(-8.75966446318483,7.98522460710227,
10.2231873160559));
#111760=CARTESIAN_POINT('Ctrl Pts',(-8.76294490218532,7.98555665650646,
10.2179738646417));
#111761=CARTESIAN_POINT('Ctrl Pts',(-8.77023132832811,7.98628426640856,
10.2065544615098));
#111762=CARTESIAN_POINT('Ctrl Pts',(-8.77425159530096,7.98667929472334,
10.200357792855));
#111763=CARTESIAN_POINT('Ctrl Pts',(-8.78852243768954,7.98805947838855,
10.1787218491865));
#111764=CARTESIAN_POINT('Ctrl Pts',(-8.79901941753807,7.98903553668597,
10.1634467345273));
#111765=CARTESIAN_POINT('Ctrl Pts',(-8.86813830794615,7.99522720688767,
10.0668490635292));
#111766=CARTESIAN_POINT('Ctrl Pts',(-8.93469488988701,8.00011939284524,
9.99153135850552));
#111767=CARTESIAN_POINT('Ctrl Pts',(-9.07289254244124,8.00926245854925,
9.8642250914525));
#111768=CARTESIAN_POINT('Ctrl Pts',(-9.14254727114707,8.0135070055928,9.81076311619941));
#111769=CARTESIAN_POINT('Ctrl Pts',(-9.22845487459194,8.01883527102883,
9.7563164222544));
#111770=CARTESIAN_POINT('Ctrl Pts',(-9.24046212772905,8.01958214496893,
9.74894727778133));
#111771=CARTESIAN_POINT('Ctrl Pts',(-9.25702591541726,8.02061795768229,
9.7391080222834));
#111772=CARTESIAN_POINT('Ctrl Pts',(-9.2614923277946,8.02089780410412,9.73648684759589));
#111773=CARTESIAN_POINT('Ctrl Pts',(-9.26901631995889,8.02137028963123,
9.73212481354041));
#111774=CARTESIAN_POINT('Ctrl Pts',(-9.27206648096569,8.02156212287942,
9.73037114854506));
#111775=CARTESIAN_POINT('Ctrl Pts',(-9.27787782567664,8.0219282241634,9.7270577891966));
#111776=CARTESIAN_POINT('Ctrl Pts',(-9.28063780649281,8.02210235439946,
9.72549604125686));
#111777=CARTESIAN_POINT('Ctrl Pts',(-9.28719799516707,8.02251681393218,
9.72181202571822));
#111778=CARTESIAN_POINT('Ctrl Pts',(-9.2910026162161,8.02275763400676,9.71969772924704));
#111779=CARTESIAN_POINT('Ctrl Pts',(-9.30441883644531,8.02360826755845,
9.71232023414181));
#111780=CARTESIAN_POINT('Ctrl Pts',(-9.31407982772074,8.02422337735138,
9.70714817659425));
#111781=CARTESIAN_POINT('Ctrl Pts',(-9.41502789336033,8.0306700618053,9.65455511111434));
#111782=CARTESIAN_POINT('Ctrl Pts',(-9.51100905065088,8.03694154165222,
9.61677919567156));
#111783=CARTESIAN_POINT('Ctrl Pts',(-9.67343693028765,8.04705111357372,
9.57188938175917));
#111784=CARTESIAN_POINT('Ctrl Pts',(-9.73783377116377,8.05094274476676,
9.55867642030742));
#111785=CARTESIAN_POINT('Ctrl Pts',(-9.83906208740181,8.05681107099318,
9.54491832280981));
#111786=CARTESIAN_POINT('Ctrl Pts',(-9.8753918033547,8.05886930200793,9.54135788304825));
#111787=CARTESIAN_POINT('Ctrl Pts',(-9.92236465972513,8.06146971772881,
9.53852245333272));
#111788=CARTESIAN_POINT('Ctrl Pts',(-9.93291705660242,8.06204999601479,
9.53800008469242));
#111789=CARTESIAN_POINT('Ctrl Pts',(-9.95007040814681,8.06298709811532,
9.53733706603037));
#111790=CARTESIAN_POINT('Ctrl Pts',(-9.95666815610083,8.06334605931964,
9.53712673965328));
#111791=CARTESIAN_POINT('Ctrl Pts',(-9.96936355111284,8.06403399341913,
9.53680799373421));
#111792=CARTESIAN_POINT('Ctrl Pts',(-9.97546088390145,8.06436316102707,
9.53669303544067));
#111793=CARTESIAN_POINT('Ctrl Pts',(-9.98944997867812,8.06511561481059,
9.5365167485406));
#111794=CARTESIAN_POINT('Ctrl Pts',(-9.99734191249357,8.06553809982905,
9.53648113503215));
#111795=CARTESIAN_POINT('Ctrl Pts',(-10.0224985841497,8.06687867824873,
9.53657110237233));
#111796=CARTESIAN_POINT('Ctrl Pts',(-10.0397613144205,8.0677893375019,9.53693834871143));
#111797=CARTESIAN_POINT('Ctrl Pts',(-10.2003233164913,8.07618313636488,
9.54319816184964));
#111798=CARTESIAN_POINT('Ctrl Pts',(-10.3420199857138,8.08292601769029,
9.56981737403164));
#111799=CARTESIAN_POINT('Ctrl Pts',(-10.5301432290091,8.09276186524038,
9.63476296132847));
#111800=CARTESIAN_POINT('Ctrl Pts',(-10.5816210811619,8.09556638536978,
9.65588702263113));
#111801=CARTESIAN_POINT('Ctrl Pts',(-10.6388064169065,8.0989424979864,9.68325419502645));
#111802=CARTESIAN_POINT('Ctrl Pts',(-10.6458186584237,8.0993611262029,9.68667924393484));
#111803=CARTESIAN_POINT('Ctrl Pts',(-10.6564623828216,8.10000414370963,
9.69198390414119));
#111804=CARTESIAN_POINT('Ctrl Pts',(-10.6601140441921,8.10022612378162,
9.69382297718801));
#111805=CARTESIAN_POINT('Ctrl Pts',(-10.6667679916628,8.10063320669391,
9.69720911028051));
#111806=CARTESIAN_POINT('Ctrl Pts',(-10.6697726718672,8.10081800945702,
9.69875128260628));
#111807=CARTESIAN_POINT('Ctrl Pts',(-10.6764932784537,8.10123355885683,
9.70223012341559));
#111808=CARTESIAN_POINT('Ctrl Pts',(-10.68020621072,8.10146464209668,9.70417234233565));
#111809=CARTESIAN_POINT('Ctrl Pts',(-10.691019480823,8.1021419190061,9.7098879967375));
#111810=CARTESIAN_POINT('Ctrl Pts',(-10.6980970093249,8.10259063240782,
9.71370397517261));
#111811=CARTESIAN_POINT('Ctrl Pts',(-10.7544491594172,8.10620469018094,
9.74468932915694));
#111812=CARTESIAN_POINT('Ctrl Pts',(-10.8021466777634,8.10951648582705,
9.77461928193378));
#111813=CARTESIAN_POINT('Ctrl Pts',(-10.9333366754699,8.11913137585377,
9.86788758309227));
#111814=CARTESIAN_POINT('Ctrl Pts',(-11.011928120378,8.12550442276371,9.93754942836499));
#111815=CARTESIAN_POINT('Ctrl Pts',(-11.1140263900329,8.13431599740379,
10.0497454266749));
#111816=CARTESIAN_POINT('Ctrl Pts',(-11.1439513003832,8.13698604171703,
10.0859897902492));
#111817=CARTESIAN_POINT('Ctrl Pts',(-11.1789362401041,8.1402206774688,10.1327788352374));
#111818=CARTESIAN_POINT('Ctrl Pts',(-11.185681419954,8.14085014105599,10.1420240168744));
#111819=CARTESIAN_POINT('Ctrl Pts',(-11.196257080581,8.14184669301241,10.1568823329826));
#111820=CARTESIAN_POINT('Ctrl Pts',(-11.2001580144326,8.14221644543743,
10.1624445416375));
#111821=CARTESIAN_POINT('Ctrl Pts',(-11.2074602329449,8.1429127934953,10.1730123000309));
#111822=CARTESIAN_POINT('Ctrl Pts',(-11.2108694664639,8.14323968340398,
10.1780121614392));
#111823=CARTESIAN_POINT('Ctrl Pts',(-11.2185207157239,8.14397745451822,
10.1893841166433));
#111824=CARTESIAN_POINT('Ctrl Pts',(-11.2227439651303,8.1443876329496,10.1957686627912));
#111825=CARTESIAN_POINT('Ctrl Pts',(-11.2335185598191,8.14544200285631,
10.2123383587657));
#111826=CARTESIAN_POINT('Ctrl Pts',(-11.2399939978019,8.14608341516626,
10.2225723214083));
#111827=CARTESIAN_POINT('Ctrl Pts',(-11.2952233288456,8.15162576423719,
10.3123042197221));
#111828=CARTESIAN_POINT('Ctrl Pts',(-11.3364040862813,8.1562377396036,10.3962154728327));
#111829=CARTESIAN_POINT('Ctrl Pts',(-11.3929522896933,8.16405048275322,
10.5461289331736));
#111830=CARTESIAN_POINT('Ctrl Pts',(-11.4122546636138,8.16727864449445,
10.6103191919022));
#111831=CARTESIAN_POINT('Ctrl Pts',(-11.4371204585222,8.17287715935779,
10.7197091454464));
#111832=CARTESIAN_POINT('Ctrl Pts',(-11.445095468781,8.17518415094482,10.7642532307434));
#111833=CARTESIAN_POINT('Ctrl Pts',(-11.4519718849272,8.17799418340302,
10.816517030565));
#111834=CARTESIAN_POINT('Ctrl Pts',(-11.4528919258658,8.17839627902209,
10.8239505702295));
#111835=CARTESIAN_POINT('Ctrl Pts',(-11.4542182817031,8.17901902922728,
10.8353864523375));
#111836=CARTESIAN_POINT('Ctrl Pts',(-11.4546652366885,8.17923750220132,
10.8393840627548));
#111837=CARTESIAN_POINT('Ctrl Pts',(-11.4554574694855,8.17964127596287,
10.8467445510814));
#111838=CARTESIAN_POINT('Ctrl Pts',(-11.4558075812906,8.17982630837351,
10.8501068255927));
#111839=CARTESIAN_POINT('Ctrl Pts',(-11.4565732840387,8.18024638256619,
10.8577160337075));
#111840=CARTESIAN_POINT('Ctrl Pts',(-11.456981949444,8.18048179706565,10.8619635667941));
#111841=CARTESIAN_POINT('Ctrl Pts',(-11.457991136118,8.18109337132133,10.8729568465031));
#111842=CARTESIAN_POINT('Ctrl Pts',(-11.4585634121716,8.18147100624279,
10.8797050085364));
#111843=CARTESIAN_POINT('Ctrl Pts',(-11.4620084523365,8.18396193030654,
10.9239755428028));
#111844=CARTESIAN_POINT('Ctrl Pts',(-11.4634796431031,8.18614159399153,
10.9615901349345));
#111845=CARTESIAN_POINT('Ctrl Pts',(-11.4634997901997,8.18835865055823,
10.9992163638923));
#111846=CARTESIAN_POINT('Origin',(-10.,3.5,11.));
#111847=CARTESIAN_POINT('',(-11.463499918694,8.75942153140066,10.9995121649462));
#111848=CARTESIAN_POINT('',(-11.4634998917645,8.69060327775791,10.999437145398));
#111849=CARTESIAN_POINT('',(-11.4635,3.5,11.));
#111850=CARTESIAN_POINT('Ctrl Pts',(-11.463499918694,8.75942153142852,10.9995121654828));
#111851=CARTESIAN_POINT('Ctrl Pts',(-11.4634645275482,8.7539097792227,10.8933389916415));
#111852=CARTESIAN_POINT('Ctrl Pts',(-11.4518762295386,8.7487701525544,10.7874851722145));
#111853=CARTESIAN_POINT('Ctrl Pts',(-11.424673565895,8.74263898727559,10.66455019465));
#111854=CARTESIAN_POINT('Ctrl Pts',(-11.420022973337,8.74167703019694,10.6453789583251));
#111855=CARTESIAN_POINT('Ctrl Pts',(-11.397962437214,8.73744051653036,10.5618466969237));
#111856=CARTESIAN_POINT('Ctrl Pts',(-11.376555287381,8.73411808063943,10.4986309937983));
#111857=CARTESIAN_POINT('Ctrl Pts',(-11.3477832177277,8.7301398374855,10.4295799300859));
#111858=CARTESIAN_POINT('Ctrl Pts',(-11.3445861643966,8.72970318007339,
10.4220841768454));
#111859=CARTESIAN_POINT('Ctrl Pts',(-11.339641619479,8.72903530409525,10.4107544397738));
#111860=CARTESIAN_POINT('Ctrl Pts',(-11.3379398437821,8.7288067282174,10.4069005375074));
#111861=CARTESIAN_POINT('Ctrl Pts',(-11.3348439608678,8.72839310774722,
10.3999706211955));
#111862=CARTESIAN_POINT('Ctrl Pts',(-11.3334558227411,8.72820842187445,
10.3968920298181));
#111863=CARTESIAN_POINT('Ctrl Pts',(-11.3303728802607,8.7277999290969,10.3901174031773));
#111864=CARTESIAN_POINT('Ctrl Pts',(-11.3286733437485,8.72757584446508,
10.3864236581859));
#111865=CARTESIAN_POINT('Ctrl Pts',(-11.3237111364668,8.7269248490244,10.3757561730498));
#111866=CARTESIAN_POINT('Ctrl Pts',(-11.3204088482265,8.72649564029826,
10.3688011433907));
#111867=CARTESIAN_POINT('Ctrl Pts',(-11.2945049298553,8.72316119256339,
10.3153371990089));
#111868=CARTESIAN_POINT('Ctrl Pts',(-11.2695094234793,8.7201308743978,10.2700335770897));
#111869=CARTESIAN_POINT('Ctrl Pts',(-11.1836728604298,8.71046264502916,
10.132249657305));
#111870=CARTESIAN_POINT('Ctrl Pts',(-11.1147056682926,8.70371051829409,
10.0452707990669));
#111871=CARTESIAN_POINT('Ctrl Pts',(-11.0043714788515,8.69463654862207,
9.93456407498749));
#111872=CARTESIAN_POINT('Ctrl Pts',(-10.9706525422068,8.69204186986117,
9.90375638993865));
#111873=CARTESIAN_POINT('Ctrl Pts',(-10.92656438772,8.68886508652711,9.86710675957227));
#111874=CARTESIAN_POINT('Ctrl Pts',(-10.9174937233117,8.68822222501483,
9.85974830079362));
#111875=CARTESIAN_POINT('Ctrl Pts',(-10.9029172236286,8.6872058468382,9.84820987376814));
#111876=CARTESIAN_POINT('Ctrl Pts',(-10.8974683164818,8.68682954592883,
9.84395907044817));
#111877=CARTESIAN_POINT('Ctrl Pts',(-10.8872058189293,8.68612752081308,
9.83606937811493));
#111878=CARTESIAN_POINT('Ctrl Pts',(-10.882399453389,8.68580144492677,9.83242136716051));
#111879=CARTESIAN_POINT('Ctrl Pts',(-10.8715902641912,8.68507409828454,
9.82432210803123));
#111880=CARTESIAN_POINT('Ctrl Pts',(-10.8655756075879,8.6846734499943,9.81988688480623));
#111881=CARTESIAN_POINT('Ctrl Pts',(-10.8476633381812,8.68349208299602,
9.80688894942092));
#111882=CARTESIAN_POINT('Ctrl Pts',(-10.8356705749638,8.6827163850512,9.79845856316399));
#111883=CARTESIAN_POINT('Ctrl Pts',(-10.8080647874357,8.68096381244739,
9.7796661959884));
#111884=CARTESIAN_POINT('Ctrl Pts',(-10.792375247735,8.67999117228726,9.76942094941195));
#111885=CARTESIAN_POINT('Ctrl Pts',(-10.7391025221437,8.67676065057149,
9.73607535735618));
#111886=CARTESIAN_POINT('Ctrl Pts',(-10.7006716093015,8.67454848749691,
9.71437264049394));
#111887=CARTESIAN_POINT('Ctrl Pts',(-10.6073761881982,8.66937978291858,
9.66711493531825));
#111888=CARTESIAN_POINT('Ctrl Pts',(-10.5517930079899,8.66645752213874,
9.64316064526222));
#111889=CARTESIAN_POINT('Ctrl Pts',(-10.459204682147,8.66165810865766,9.60989173804095));
#111890=CARTESIAN_POINT('Ctrl Pts',(-10.4230380243323,8.65979872327951,
9.5984620732433));
#111891=CARTESIAN_POINT('Ctrl Pts',(-10.346209889185,8.65581063076442,9.57742721771588));
#111892=CARTESIAN_POINT('Ctrl Pts',(-10.3055000978816,8.65367548108785,
9.56813278545701));
#111893=CARTESIAN_POINT('Ctrl Pts',(-10.2576027004825,8.65108143748451,
9.55933293164266));
#111894=CARTESIAN_POINT('Ctrl Pts',(-10.2507441621798,8.6507080458886,9.55812340524114));
#111895=CARTESIAN_POINT('Ctrl Pts',(-10.2396134709692,8.65009854841575,
9.55624228667367));
#111896=CARTESIAN_POINT('Ctrl Pts',(-10.2353464377018,8.64986405625463,
9.55554058431793));
#111897=CARTESIAN_POINT('Ctrl Pts',(-10.2277354451056,8.64944420995398,
9.55432359620364));
#111898=CARTESIAN_POINT('Ctrl Pts',(-10.2243927366879,8.64925926588518,
9.55380098295991));
#111899=CARTESIAN_POINT('Ctrl Pts',(-10.217117541099,8.6488555289235,9.55268937887835));
#111900=CARTESIAN_POINT('Ctrl Pts',(-10.213184512234,8.64863650214689,9.55210482988563));
#111901=CARTESIAN_POINT('Ctrl Pts',(-10.202047230758,8.64801421336923,9.55049590640659));
#111902=CARTESIAN_POINT('Ctrl Pts',(-10.194837753614,8.64760894753207,9.54950923955838));
#111903=CARTESIAN_POINT('Ctrl Pts',(-10.147950227359,8.64495874586977,9.54344822333674));
#111904=CARTESIAN_POINT('Ctrl Pts',(-10.1080886437577,8.64263856303524,
9.5399490896912));
#111905=CARTESIAN_POINT('Ctrl Pts',(-9.9330302877212,8.63229477533152,9.53178989743308));
#111906=CARTESIAN_POINT('Ctrl Pts',(-9.7976714362682,8.6239721873824,9.54425322988476));
#111907=CARTESIAN_POINT('Ctrl Pts',(-9.63149742474595,8.61417310132988,
9.58321118057635));
#111908=CARTESIAN_POINT('Ctrl Pts',(-9.59734409446262,8.61217691934041,
9.59253659773072));
#111909=CARTESIAN_POINT('Ctrl Pts',(-9.55321637073037,8.6096206352293,9.60632353839052));
#111910=CARTESIAN_POINT('Ctrl Pts',(-9.54290848116356,8.60902512945052,
9.60967016745398));
#111911=CARTESIAN_POINT('Ctrl Pts',(-9.52632782856627,8.60806968051656,
9.61525768772911));
#111912=CARTESIAN_POINT('Ctrl Pts',(-9.52003165884168,8.6077074412124,9.61742740121706));
#111913=CARTESIAN_POINT('Ctrl Pts',(-9.50801729788666,8.60701724778018,
9.62165961443619));
#111914=CARTESIAN_POINT('Ctrl Pts',(-9.50229673064675,8.60668906680138,
9.62371490785453));
#111915=CARTESIAN_POINT('Ctrl Pts',(-9.48917570351211,8.60593729763585,
9.62852155631383));
#111916=CARTESIAN_POINT('Ctrl Pts',(-9.4817843349884,8.60551452008616,9.63129728895752));
#111917=CARTESIAN_POINT('Ctrl Pts',(-9.45871054150167,8.60419670738976,
9.64017606080606));
#111918=CARTESIAN_POINT('Ctrl Pts',(-9.44311039616428,8.60330863688758,
9.64648996193267));
#111919=CARTESIAN_POINT('Ctrl Pts',(-9.36597807694944,8.59892740871482,
9.67926737737361));
#111920=CARTESIAN_POINT('Ctrl Pts',(-9.30620202708779,8.59556799140007,
9.70966511812181));
#111921=CARTESIAN_POINT('Ctrl Pts',(-9.17590928168139,8.58809934648975,
9.78760408510831));
#111922=CARTESIAN_POINT('Ctrl Pts',(-9.10703267099872,8.58404576976513,
9.83740041902271));
#111923=CARTESIAN_POINT('Ctrl Pts',(-9.03133410730086,8.57906632795377,
9.90284424171761));
#111924=CARTESIAN_POINT('Ctrl Pts',(-9.01996519388132,8.57830278931688,
9.91298752133127));
#111925=CARTESIAN_POINT('Ctrl Pts',(-8.98422373513097,8.57584437164307,
9.94589239436067));
#111926=CARTESIAN_POINT('Ctrl Pts',(-8.96047134018448,8.57412224806746,
9.96930891478624));
#111927=CARTESIAN_POINT('Ctrl Pts',(-8.9326027672369,8.57196052948403,9.99872732981579));
#111928=CARTESIAN_POINT('Ctrl Pts',(-8.92770294745746,8.57157487518657,
10.0039764864715));
#111929=CARTESIAN_POINT('Ctrl Pts',(-8.92013457465902,8.57097002987649,
10.0122050270169));
#111930=CARTESIAN_POINT('Ctrl Pts',(-8.91743920539937,8.57075278395131,
10.0151597232456));
#111931=CARTESIAN_POINT('Ctrl Pts',(-8.91248749465034,8.57035018837538,
10.0206327381118));
#111932=CARTESIAN_POINT('Ctrl Pts',(-8.91022774100975,8.57016509627331,
10.0231478587674));
#111933=CARTESIAN_POINT('Ctrl Pts',(-8.90511818447828,8.56974348170336,
10.0288746240597));
#111934=CARTESIAN_POINT('Ctrl Pts',(-8.90227379997858,8.56950657379071,
10.0320909781475));
#111935=CARTESIAN_POINT('Ctrl Pts',(-8.89363111960035,8.56878009373786,
10.041950988129));
#111936=CARTESIAN_POINT('Ctrl Pts',(-8.88787878689673,8.56828735978756,
10.0486344507625));
#111937=CARTESIAN_POINT('Ctrl Pts',(-8.8359803371556,8.56376029228534,10.1100475986001));
#111938=CARTESIAN_POINT('Ctrl Pts',(-8.793851786785,8.5594940833683,10.1680375262622));
#111939=CARTESIAN_POINT('Ctrl Pts',(-8.68933273635898,8.54757483415237,
10.3366305482554));
#111940=CARTESIAN_POINT('Ctrl Pts',(-8.63679972996406,8.53994854839546,
10.4526389604042));
#111941=CARTESIAN_POINT('Ctrl Pts',(-8.59553948283946,8.53202519140167,
10.5882414297746));
#111942=CARTESIAN_POINT('Ctrl Pts',(-8.59141818716706,8.53119879538267,
10.6025685418436));
#111943=CARTESIAN_POINT('Ctrl Pts',(-8.58552204214379,8.52996054929503,
10.6243107414081));
#111944=CARTESIAN_POINT('Ctrl Pts',(-8.58358512804274,8.52954355706952,
10.6316805383285));
#111945=CARTESIAN_POINT('Ctrl Pts',(-8.58031135743822,8.52882034294646,
10.6445448287062));
#111946=CARTESIAN_POINT('Ctrl Pts',(-8.57894863414682,8.52851330264368,
10.6500325194125));
#111947=CARTESIAN_POINT('Ctrl Pts',(-8.57616220270509,8.52787258180239,
10.6615381597554));
#111948=CARTESIAN_POINT('Ctrl Pts',(-8.57474476286851,8.52753910581542,
10.6675575223498));
#111949=CARTESIAN_POINT('Ctrl Pts',(-8.57145747762567,8.52674716933416,
10.6819250156971));
#111950=CARTESIAN_POINT('Ctrl Pts',(-8.5696225824573,8.52628982156482,10.6902809637171));
#111951=CARTESIAN_POINT('Ctrl Pts',(-8.56361987565763,8.52473905068696,
10.7188085418899));
#111952=CARTESIAN_POINT('Ctrl Pts',(-8.55980457331678,8.5236566875341,10.7390523315748));
#111953=CARTESIAN_POINT('Ctrl Pts',(-8.5516406190662,8.52107693928109,10.7880294705139));
#111954=CARTESIAN_POINT('Ctrl Pts',(-8.54771781973208,8.51959226277391,
10.8168252173628));
#111955=CARTESIAN_POINT('Ctrl Pts',(-8.53550746959374,8.51375183287342,
10.9320070792431));
#111956=CARTESIAN_POINT('Ctrl Pts',(-8.5340520787472,8.50957427623218,11.0189397496178));
#111957=CARTESIAN_POINT('Ctrl Pts',(-8.54318437368548,8.50339092607835,
11.1453077892593));
#111958=CARTESIAN_POINT('Ctrl Pts',(-8.5476900963463,8.50143076917602,11.184991427442));
#111959=CARTESIAN_POINT('Ctrl Pts',(-8.55973626669931,8.49748335768654,
11.2626115467538));
#111960=CARTESIAN_POINT('Ctrl Pts',(-8.5671688783992,8.49550048777836,11.3005311169988));
#111961=CARTESIAN_POINT('Ctrl Pts',(-8.57766734553885,8.49307868112752,
11.3447442194711));
#111962=CARTESIAN_POINT('Ctrl Pts',(-8.57928918803116,8.4927129115927,11.3513681004539));
#111963=CARTESIAN_POINT('Ctrl Pts',(-8.58200434492857,8.49211343510491,
11.3621310502496));
#111964=CARTESIAN_POINT('Ctrl Pts',(-8.58306964897397,8.49188125608041,
11.3662771556589));
#111965=CARTESIAN_POINT('Ctrl Pts',(-8.58500871798621,8.49146387387452,
11.3736888400467));
#111966=CARTESIAN_POINT('Ctrl Pts',(-8.5858756235123,8.49127906075411,11.3769561311992));
#111967=CARTESIAN_POINT('Ctrl Pts',(-8.58779552984267,8.49087359821258,
11.3840922551675));
#111968=CARTESIAN_POINT('Ctrl Pts',(-8.58885309810562,8.49065269854811,
11.3879597227804));
#111969=CARTESIAN_POINT('Ctrl Pts',(-8.59191632878156,8.49001984124107,
11.3989835347516));
#111970=CARTESIAN_POINT('Ctrl Pts',(-8.59396060117968,8.48960577365943,
11.4061289085963));
#111971=CARTESIAN_POINT('Ctrl Pts',(-8.60840690439978,8.48673660581106,
11.4552065862102));
#111972=CARTESIAN_POINT('Ctrl Pts',(-8.62262749217222,8.48419169860697,
11.4965769690411));
#111973=CARTESIAN_POINT('Ctrl Pts',(-8.66343975569986,8.47760848871175,
11.5999910366419));
#111974=CARTESIAN_POINT('Ctrl Pts',(-8.69251057751328,8.47352015796154,
11.660949141893));
#111975=CARTESIAN_POINT('Ctrl Pts',(-8.77214635913729,8.46381277417161,
11.8019573239089));
#111976=CARTESIAN_POINT('Ctrl Pts',(-8.82647537672002,8.45827132665699,
11.8795482874018));
#111977=CARTESIAN_POINT('Ctrl Pts',(-8.89574091556883,8.45234895522086,
11.9605149796252));
#111978=CARTESIAN_POINT('Ctrl Pts',(-8.90367877331684,8.451684430649,11.969565331303));
#111979=CARTESIAN_POINT('Ctrl Pts',(-8.91683029716929,8.45060607136661,
11.9841919982478));
#111980=CARTESIAN_POINT('Ctrl Pts',(-8.92197741353878,8.4501895223523,11.9898271569818));
#111981=CARTESIAN_POINT('Ctrl Pts',(-8.93128184269887,8.44944619543235,
11.9998551516512));
#111982=CARTESIAN_POINT('Ctrl Pts',(-8.93542272355338,8.44911874006213,
12.00426293769));
#111983=CARTESIAN_POINT('Ctrl Pts',(-8.94428046264766,8.44842530881467,
12.0135752604602));
#111984=CARTESIAN_POINT('Ctrl Pts',(-8.94900445413408,8.44805964805249,
12.0184728346226));
#111985=CARTESIAN_POINT('Ctrl Pts',(-8.96180266271756,8.44707997746438,
12.031557440636));
#111986=CARTESIAN_POINT('Ctrl Pts',(-8.96993958117814,8.44646868786663,
12.0396826477542));
#111987=CARTESIAN_POINT('Ctrl Pts',(-9.01237064662943,8.4433385336215,12.0810654887214));
#111988=CARTESIAN_POINT('Ctrl Pts',(-9.04818404919093,8.44088818762806,
12.1127269721376));
#111989=CARTESIAN_POINT('Ctrl Pts',(-9.17052104284699,8.43301799221599,
12.2106447059713));
#111990=CARTESIAN_POINT('Ctrl Pts',(-9.26288470198069,8.42786045935254,
12.2689979882786));
#111991=CARTESIAN_POINT('Ctrl Pts',(-9.37312311800238,8.4217848698338,12.3225140059866));
#111992=CARTESIAN_POINT('Ctrl Pts',(-9.38546347127225,8.42110536400519,
12.3282931767602));
#111993=CARTESIAN_POINT('Ctrl Pts',(-9.43297757838394,8.41848519175475,
12.3497408826223));
#111994=CARTESIAN_POINT('Ctrl Pts',(-9.46868151078588,8.4165084090986,12.3641902628457));
#111995=CARTESIAN_POINT('Ctrl Pts',(-9.51132188528475,8.41409350415803,
12.3795188900771));
#111996=CARTESIAN_POINT('Ctrl Pts',(-9.51774915736539,8.41372807801219,
12.3817788495704));
#111997=CARTESIAN_POINT('Ctrl Pts',(-9.52823824234789,8.41312905327127,
12.3853849293675));
#111998=CARTESIAN_POINT('Ctrl Pts',(-9.53229066266431,8.41289697878885,
12.3867582822295));
#111999=CARTESIAN_POINT('Ctrl Pts',(-9.53955518947212,8.41247970708643,
12.3891847440151));
#112000=CARTESIAN_POINT('Ctrl Pts',(-9.54276498582242,8.4122948990213,12.3902445173527));
#112001=CARTESIAN_POINT('Ctrl Pts',(-9.5497916244935,8.41188935463937,12.3925375244892));
#112002=CARTESIAN_POINT('Ctrl Pts',(-9.55360982436096,8.41166836731739,
12.3937661743609));
#112003=CARTESIAN_POINT('Ctrl Pts',(-9.5645240726853,8.41103501365744,12.3972287971112));
#112004=CARTESIAN_POINT('Ctrl Pts',(-9.57163206604343,8.41062053233552,
12.399424347069));
#112005=CARTESIAN_POINT('Ctrl Pts',(-9.62081453727068,8.40774030186502,
12.4142062488135));
#112006=CARTESIAN_POINT('Ctrl Pts',(-9.66341692522347,8.40518397546698,
12.4249463454607));
#112007=CARTESIAN_POINT('Ctrl Pts',(-9.77236999823677,8.39859753151287,
12.4472548923081));
#112008=CARTESIAN_POINT('Ctrl Pts',(-9.83915822434291,8.39451845795667,
12.4561908859409));
#112009=CARTESIAN_POINT('Ctrl Pts',(-10.000582601754,8.38482236978086,12.4665446649694));
#112010=CARTESIAN_POINT('Ctrl Pts',(-10.0952179730144,8.37928314627308,
12.463452167005));
#112011=CARTESIAN_POINT('Ctrl Pts',(-10.2008361147505,8.37336325744281,
12.4497040413589));
#112012=CARTESIAN_POINT('Ctrl Pts',(-10.2127453585057,8.37269919835224,
12.4480042738326));
#112013=CARTESIAN_POINT('Ctrl Pts',(-10.2321714549076,8.3716214388082,12.4449868068446));
#112014=CARTESIAN_POINT('Ctrl Pts',(-10.2397011873949,8.37120502908746,
12.4437568355721));
#112015=CARTESIAN_POINT('Ctrl Pts',(-10.2531815499531,8.3704618556033,12.4414464692778));
#112016=CARTESIAN_POINT('Ctrl Pts',(-10.2591357126286,8.37013441548307,
12.4403879703003));
#112017=CARTESIAN_POINT('Ctrl Pts',(-10.2717766007379,8.36944091783668,
12.4380598216107));
#112018=CARTESIAN_POINT('Ctrl Pts',(-10.2784613898385,8.36907517618777,
12.4367803686507));
#112019=CARTESIAN_POINT('Ctrl Pts',(-10.2964221329984,8.36809505114387,
12.4332126661064));
#112020=CARTESIAN_POINT('Ctrl Pts',(-10.3076805546494,8.36748339243936,
12.4308379759849));
#112021=CARTESIAN_POINT('Ctrl Pts',(-10.3656314240511,8.3643475954843,12.4178990167684));
#112022=CARTESIAN_POINT('Ctrl Pts',(-10.4118152629097,8.36189228354789,
12.405180679042));
#112023=CARTESIAN_POINT('Ctrl Pts',(-10.5612856545771,8.35399017970294,
12.3560142284773));
#112024=CARTESIAN_POINT('Ctrl Pts',(-10.6611032508813,8.34880873799466,
12.3102509300205));
#112025=CARTESIAN_POINT('Ctrl Pts',(-10.7982722729033,8.34086582861755,
12.2276639197434));
#112026=CARTESIAN_POINT('Ctrl Pts',(-10.8402721890174,8.3383000840131,12.199307720493));
#112027=CARTESIAN_POINT('Ctrl Pts',(-10.8865144077847,8.33521910481808,
12.1644643423327));
#112028=CARTESIAN_POINT('Ctrl Pts',(-10.8922822468455,8.3348300159793,12.1600505969529));
#112029=CARTESIAN_POINT('Ctrl Pts',(-10.9014645336381,8.33420245421187,
12.1529150050947));
#112030=CARTESIAN_POINT('Ctrl Pts',(-10.9049001379506,8.33396580034421,
12.1502204370135));
#112031=CARTESIAN_POINT('Ctrl Pts',(-10.9109848700419,8.33354326999398,
12.1454040058389));
#112032=CARTESIAN_POINT('Ctrl Pts',(-10.9136387384782,8.33335781984476,
12.1432882512257));
#112033=CARTESIAN_POINT('Ctrl Pts',(-10.9192634509966,8.33296226109526,
12.1387719462071));
#112034=CARTESIAN_POINT('Ctrl Pts',(-10.9222322176447,8.33275199231582,
12.1363690306685));
#112035=CARTESIAN_POINT('Ctrl Pts',(-10.9301909097327,8.33218436319737,
12.129875547887));
#112036=CARTESIAN_POINT('Ctrl Pts',(-10.9351631871454,8.33182553746506,
12.1257636042037));
#112037=CARTESIAN_POINT('Ctrl Pts',(-10.9463256713037,8.33101079807887,
12.1164075386335));
#112038=CARTESIAN_POINT('Ctrl Pts',(-10.9524997501412,8.33055368163332,
12.1111445849858));
#112039=CARTESIAN_POINT('Ctrl Pts',(-10.9715355772675,8.32912491986422,
12.0946426847807));
#112040=CARTESIAN_POINT('Ctrl Pts',(-10.9842442021166,8.32814319113209,
12.0832300266417));
#112041=CARTESIAN_POINT('Ctrl Pts',(-11.034821319519,8.32413184947629,12.0361855906138));
#112042=CARTESIAN_POINT('Ctrl Pts',(-11.0709767243198,8.32102267512462,
11.9987712485533));
#112043=CARTESIAN_POINT('Ctrl Pts',(-11.1866316464764,8.31041879568386,
11.8655727777863));
#112044=CARTESIAN_POINT('Ctrl Pts',(-11.255904920208,8.30294436957543,11.761593375002));
#112045=CARTESIAN_POINT('Ctrl Pts',(-11.3185780423716,8.29505336459114,
11.6351857395331));
#112046=CARTESIAN_POINT('Ctrl Pts',(-11.3257129526795,8.29413158759976,
11.6201565742105));
#112047=CARTESIAN_POINT('Ctrl Pts',(-11.3358524524978,8.29278540924576,
11.597823338936));
#112048=CARTESIAN_POINT('Ctrl Pts',(-11.3390564961231,8.29235428198561,
11.5906117362635));
#112049=CARTESIAN_POINT('Ctrl Pts',(-11.3446323849648,8.29159355364524,
11.577782978621));
#112050=CARTESIAN_POINT('Ctrl Pts',(-11.3470277310445,8.29126316703562,
11.5721762966359));
#112051=CARTESIAN_POINT('Ctrl Pts',(-11.3519423797732,8.29057766076519,
11.5604708648192));
#112052=CARTESIAN_POINT('Ctrl Pts',(-11.3544556168449,8.29022274987878,
11.5543697073983));
#112053=CARTESIAN_POINT('Ctrl Pts',(-11.360882939792,8.28930347228406,11.5384620292281));
#112054=CARTESIAN_POINT('Ctrl Pts',(-11.3647323538104,8.28874125958458,
11.5286296841599));
#112055=CARTESIAN_POINT('Ctrl Pts',(-11.3813930067757,8.28625373868709,
11.4846790165273));
#112056=CARTESIAN_POINT('Ctrl Pts',(-11.3930341311937,8.28436689972388,
11.4501295124212));
#112057=CARTESIAN_POINT('Ctrl Pts',(-11.4219653224671,8.27918083089114,
11.3523373889305));
#112058=CARTESIAN_POINT('Ctrl Pts',(-11.4363155392342,8.2759652270832,11.2883148596826));
#112059=CARTESIAN_POINT('Ctrl Pts',(-11.457802347785,8.26911157271654,11.1492952597736));
#112060=CARTESIAN_POINT('Ctrl Pts',(-11.4635427146042,8.26549102312458,
11.0742800636214));
#112061=CARTESIAN_POINT('Ctrl Pts',(-11.4634997607281,8.26169280151533,
10.999163131591));
#112062=CARTESIAN_POINT('Ctrl Pts',(-11.4634997901997,8.18835865055823,
10.9992163638923));
#112063=CARTESIAN_POINT('Ctrl Pts',(-11.463562176983,8.19522390914069,11.1157284074538));
#112064=CARTESIAN_POINT('Ctrl Pts',(-11.4497117361902,8.20237636626697,
11.2318341407186));
#112065=CARTESIAN_POINT('Ctrl Pts',(-11.4096862102963,8.21230185552391,
11.39679931889));
#112066=CARTESIAN_POINT('Ctrl Pts',(-11.3943238830279,8.21534323336146,
11.4478021977668));
#112067=CARTESIAN_POINT('Ctrl Pts',(-11.3720654063134,8.21897268514177,
11.5093305192923));
#112068=CARTESIAN_POINT('Ctrl Pts',(-11.3677722757196,8.21964466356928,
11.5207495285298));
#112069=CARTESIAN_POINT('Ctrl Pts',(-11.360780640102,8.22069650232875,11.538662904316));
#112070=CARTESIAN_POINT('Ctrl Pts',(-11.3581773106712,8.22107948369976,
11.5451936079406));
#112071=CARTESIAN_POINT('Ctrl Pts',(-11.3532767418419,8.22178474860526,
11.5572341889608));
#112072=CARTESIAN_POINT('Ctrl Pts',(-11.3509926653047,8.2221074611636,11.562749234654));
#112073=CARTESIAN_POINT('Ctrl Pts',(-11.3458410310021,8.22282224999222,
11.5749760314164));
#112074=CARTESIAN_POINT('Ctrl Pts',(-11.3429568685593,8.22321376091015,
11.5816806419672));
#112075=CARTESIAN_POINT('Ctrl Pts',(-11.3344743946778,8.22434077497162,
11.6009998339117));
#112076=CARTESIAN_POINT('Ctrl Pts',(-11.3287475729203,8.22507194387926,
11.6135573444699));
#112077=CARTESIAN_POINT('Ctrl Pts',(-11.2800791318426,8.23105247205133,
11.7163966898957));
#112078=CARTESIAN_POINT('Ctrl Pts',(-11.228167345611,8.2359669039415,11.8021437964628));
#112079=CARTESIAN_POINT('Ctrl Pts',(-11.1083926811965,8.24564408637833,
11.9607565766766));
#112080=CARTESIAN_POINT('Ctrl Pts',(-11.0410534883211,8.25039133919379,
12.0333394305755));
#112081=CARTESIAN_POINT('Ctrl Pts',(-10.9584658386875,8.25619015764342,
12.1060301294569));
#112082=CARTESIAN_POINT('Ctrl Pts',(-10.9499154741651,8.25679042162266,
12.1133822290202));
#112083=CARTESIAN_POINT('Ctrl Pts',(-10.9379072203726,8.25763467491169,
12.1234686074574));
#112084=CARTESIAN_POINT('Ctrl Pts',(-10.9345204373518,8.25787292059347,
12.1262873599288));
#112085=CARTESIAN_POINT('Ctrl Pts',(-10.9286638060807,8.25828524076763,
12.1311171156803));
#112086=CARTESIAN_POINT('Ctrl Pts',(-10.9262000072615,8.25845879789903,
12.133135446564));
#112087=CARTESIAN_POINT('Ctrl Pts',(-10.9210119189915,8.25882451794363,
12.1373572755665));
#112088=CARTESIAN_POINT('Ctrl Pts',(-10.9182862861381,8.25901680444896,
12.1395590476643));
#112089=CARTESIAN_POINT('Ctrl Pts',(-10.9115685529625,8.25949103760501,
12.1449458961435));
#112090=CARTESIAN_POINT('Ctrl Pts',(-10.9075676555381,8.25977374798341,
12.1481198895938));
#112091=CARTESIAN_POINT('Ctrl Pts',(-10.8928582358072,8.2608138665798,12.1596642430399));
#112092=CARTESIAN_POINT('Ctrl Pts',(-10.8820501864745,8.26157950947296,
12.1679060010974));
#112093=CARTESIAN_POINT('Ctrl Pts',(-10.8545735010986,8.26352613895776,
12.1882596009126));
#112094=CARTESIAN_POINT('Ctrl Pts',(-10.8377612465624,8.26471737506758,
12.2001719740388));
#112095=CARTESIAN_POINT('Ctrl Pts',(-10.7031531968749,8.27422206780122,
12.2913422966162));
#112096=CARTESIAN_POINT('Ctrl Pts',(-10.5746373240541,8.28300562613413,
12.3534369125592));
#112097=CARTESIAN_POINT('Ctrl Pts',(-10.4027751988324,8.29338230351841,
12.4075013684091));
#112098=CARTESIAN_POINT('Ctrl Pts',(-10.3659439172829,8.29553907304429,
12.4175236811612));
#112099=CARTESIAN_POINT('Ctrl Pts',(-10.3179065967355,8.29826669381606,
12.4285978136565));
#112100=CARTESIAN_POINT('Ctrl Pts',(-10.3070243083436,8.29887907489796,
12.4309760309346));
#112101=CARTESIAN_POINT('Ctrl Pts',(-10.2895281082568,8.299854989207,12.4345908732206));
#112102=CARTESIAN_POINT('Ctrl Pts',(-10.2829311226114,8.30022099846868,
12.435906501467));
#112103=CARTESIAN_POINT('Ctrl Pts',(-10.270370021301,8.30091424755945,12.4383216180819));
#112104=CARTESIAN_POINT('Ctrl Pts',(-10.2644077001493,8.30124174817484,
12.4394296075473));
#112105=CARTESIAN_POINT('Ctrl Pts',(-10.2507899146828,8.30198626506028,
12.4418727593506));
#112106=CARTESIAN_POINT('Ctrl Pts',(-10.2431303226611,8.30240252684143,
12.4431840786317));
#112107=CARTESIAN_POINT('Ctrl Pts',(-10.2195064211466,8.30367889658653,
12.4470350648738));
#112108=CARTESIAN_POINT('Ctrl Pts',(-10.2035099122834,8.30453266646097,
12.4493713432527));
#112109=CARTESIAN_POINT('Ctrl Pts',(-10.1261403632141,8.30861562517538,
12.4593648887214));
#112110=CARTESIAN_POINT('Ctrl Pts',(-10.0643596302101,8.31173185163661,
12.4633920100475));
#112111=CARTESIAN_POINT('Ctrl Pts',(-9.918477662454,8.31893520389298,12.4636416443699));
#112112=CARTESIAN_POINT('Ctrl Pts',(-9.83459757347256,8.32295253376796,
12.4565487374624));
#112113=CARTESIAN_POINT('Ctrl Pts',(-9.74122250894853,8.32763874461858,
12.4404795969636));
#112114=CARTESIAN_POINT('Ctrl Pts',(-9.73067407503415,8.32817142762926,
12.4385446811681));
#112115=CARTESIAN_POINT('Ctrl Pts',(-9.71157210276106,8.32914344959219,
12.4348233115218));
#112116=CARTESIAN_POINT('Ctrl Pts',(-9.70301144970894,8.32958177792835,
12.4330758474191));
#112117=CARTESIAN_POINT('Ctrl Pts',(-9.65944023974028,8.33182879178962,
12.4237745915845));
#112118=CARTESIAN_POINT('Ctrl Pts',(-9.62470225268755,8.33367315287845,
12.4150145775189));
#112119=CARTESIAN_POINT('Ctrl Pts',(-9.58390735404576,8.33593891492404,
12.4031193192117));
#112120=CARTESIAN_POINT('Ctrl Pts',(-9.57750444057204,8.33629749863851,
12.4012046291961));
#112121=CARTESIAN_POINT('Ctrl Pts',(-9.56706103386334,8.33688755007849,
12.3980036051969));
#112122=CARTESIAN_POINT('Ctrl Pts',(-9.56301255218311,8.33711756914424,
12.3967434260017));
#112123=CARTESIAN_POINT('Ctrl Pts',(-9.55574757338747,8.33753273440914,
12.3944473637416));
#112124=CARTESIAN_POINT('Ctrl Pts',(-9.55252912755954,8.33771750966202,
12.3934179153244));
#112125=CARTESIAN_POINT('Ctrl Pts',(-9.54546591729748,8.33812491098005,
12.3911316899335));
#112126=CARTESIAN_POINT('Ctrl Pts',(-9.54162283435333,8.33834780413354,
12.3898701321644));
#112127=CARTESIAN_POINT('Ctrl Pts',(-9.53057813562716,8.33899181337655,
12.3861937304018));
#112128=CARTESIAN_POINT('Ctrl Pts',(-9.52339013399067,8.33941515340762,
12.3837387670904));
#112129=CARTESIAN_POINT('Ctrl Pts',(-9.47065945070101,8.34255010725833,
12.3652697246244));
#112130=CARTESIAN_POINT('Ctrl Pts',(-9.42591864636378,8.34537094457319,
12.3470681432332));
#112131=CARTESIAN_POINT('Ctrl Pts',(-9.28743164844201,8.35444848510096,
12.2825751226901));
#112132=CARTESIAN_POINT('Ctrl Pts',(-9.19768719878795,8.36083040119204,
12.2284338519659));
#112133=CARTESIAN_POINT('Ctrl Pts',(-9.07125969917215,8.37012405691028,
12.1323515430637));
#112134=CARTESIAN_POINT('Ctrl Pts',(-9.02990098642693,8.37322814999408,
12.0971269358041));
#112135=CARTESIAN_POINT('Ctrl Pts',(-8.98170315222449,8.37692108965572,
12.0512157060119));
#112136=CARTESIAN_POINT('Ctrl Pts',(-8.97292168402498,8.37759736335255,
12.0426375575669));
#112137=CARTESIAN_POINT('Ctrl Pts',(-8.95926988267405,8.37865441621118,
12.0289619732202));
#112138=CARTESIAN_POINT('Ctrl Pts',(-8.95432681173402,8.37903836753157,
12.0239382330984));
#112139=CARTESIAN_POINT('Ctrl Pts',(-8.94526500986915,8.37974456752219,
12.0145944866072));
#112140=CARTESIAN_POINT('Ctrl Pts',(-8.94113606408313,8.38006725324379,
12.010284632333));
#112141=CARTESIAN_POINT('Ctrl Pts',(-8.93203074039279,8.38078095161214,
12.00066322229));
#112142=CARTESIAN_POINT('Ctrl Pts',(-8.92706737009981,8.38117140788808,
11.9953395391533));
#112143=CARTESIAN_POINT('Ctrl Pts',(-8.91287388596501,8.38229226165493,
11.9798861464303));
#112144=CARTESIAN_POINT('Ctrl Pts',(-8.90374593510384,8.38301839943941,
11.9696633899011));
#112145=CARTESIAN_POINT('Ctrl Pts',(-8.88348400140476,8.38464353665294,
11.9463193630138));
#112146=CARTESIAN_POINT('Ctrl Pts',(-8.87243506350122,8.38553915442498,
11.9331268170073));
#112147=CARTESIAN_POINT('Ctrl Pts',(-8.83717687216577,8.38843257250811,
11.8894872126356));
#112148=CARTESIAN_POINT('Ctrl Pts',(-8.81394755580074,8.39039508931698,
11.8582686077251));
#112149=CARTESIAN_POINT('Ctrl Pts',(-8.75483124242427,8.39560168227607,
11.7718287247594));
#112150=CARTESIAN_POINT('Ctrl Pts',(-8.72138094557179,8.39878394954023,
11.7150513210164));
#112151=CARTESIAN_POINT('Ctrl Pts',(-8.6578475993725,8.40569034572719,11.5884005855447));
#112152=CARTESIAN_POINT('Ctrl Pts',(-8.62915728630368,8.4094131487917,11.5180503153088));
#112153=CARTESIAN_POINT('Ctrl Pts',(-8.60239269459035,8.41403591243409,
11.434361993951));
#112154=CARTESIAN_POINT('Ctrl Pts',(-8.59887497432264,8.41467448943625,
11.4228772470598));
#112155=CARTESIAN_POINT('Ctrl Pts',(-8.59423141433422,8.41556340900609,
11.4070224513203));
#112156=CARTESIAN_POINT('Ctrl Pts',(-8.59298373682327,8.41580716332854,
11.4026882496474));
#112157=CARTESIAN_POINT('Ctrl Pts',(-8.59088176990448,8.41622646720787,
11.3952573625843));
#112158=CARTESIAN_POINT('Ctrl Pts',(-8.59001759751947,8.41640145847003,
11.3921634778409));
#112159=CARTESIAN_POINT('Ctrl Pts',(-8.58823867421885,8.41676721976179,
11.3857127355157));
#112160=CARTESIAN_POINT('Ctrl Pts',(-8.58732570349959,8.41695809409093,
11.3823554451862));
#112161=CARTESIAN_POINT('Ctrl Pts',(-8.58513485538112,8.41742386728659,
11.374184021141));
#112162=CARTESIAN_POINT('Ctrl Pts',(-8.58386957152157,8.4176994701222,11.369366575636));
#112163=CARTESIAN_POINT('Ctrl Pts',(-8.57945234513414,8.41868535991822,
11.352192053796));
#112164=CARTESIAN_POINT('Ctrl Pts',(-8.57643744559754,8.41940282799774,
11.3398006970764));
#112165=CARTESIAN_POINT('Ctrl Pts',(-8.5693542941181,8.42120232351498,11.3089382077662));
#112166=CARTESIAN_POINT('Ctrl Pts',(-8.56548152298121,8.42229283646565,
11.2904249157429));
#112167=CARTESIAN_POINT('Ctrl Pts',(-8.55048718137838,8.42699770160501,
11.2111057325332));
#112168=CARTESIAN_POINT('Ctrl Pts',(-8.5428656041567,8.43071830912486,11.1497053130997));
#112169=CARTESIAN_POINT('Ctrl Pts',(-8.53256757248105,8.44102364854368,
10.9787721750978));
#112170=CARTESIAN_POINT('Ctrl Pts',(-8.53825888193278,8.44754627336864,
10.8691229507904));
#112171=CARTESIAN_POINT('Ctrl Pts',(-8.55909429964202,8.45470107695163,
10.7431858780285));
#112172=CARTESIAN_POINT('Ctrl Pts',(-8.56239558403761,8.4557098040965,10.7253068705239));
#112173=CARTESIAN_POINT('Ctrl Pts',(-8.56763923514614,8.45715048896585,
10.6996006365608));
#112174=CARTESIAN_POINT('Ctrl Pts',(-8.5693143942948,8.45759077448299,10.6917211659979));
#112175=CARTESIAN_POINT('Ctrl Pts',(-8.57237748821839,8.4583621761024,10.6778762358917));
#112176=CARTESIAN_POINT('Ctrl Pts',(-8.57373796234022,8.4586941497333,10.6719049572823));
#112177=CARTESIAN_POINT('Ctrl Pts',(-8.57662675765324,8.45937772342641,
10.6595833100554));
#112178=CARTESIAN_POINT('Ctrl Pts',(-8.57816019122485,8.45972915311864,
10.6532342723218));
#112179=CARTESIAN_POINT('Ctrl Pts',(-8.58220822696148,8.46062844584909,
10.6369521763666));
#112180=CARTESIAN_POINT('Ctrl Pts',(-8.58478475510275,8.461174332051,10.6270347849095));
#112181=CARTESIAN_POINT('Ctrl Pts',(-8.59619338664465,8.46348403823252,
10.5849428900107));
#112182=CARTESIAN_POINT('Ctrl Pts',(-8.60602050944094,8.4652160283151,10.5530471936992));
#112183=CARTESIAN_POINT('Ctrl Pts',(-8.63559091441868,8.46983263671981,
10.4675736158474));
#112184=CARTESIAN_POINT('Ctrl Pts',(-8.65739228966893,8.47265600593214,
10.4147691279232));
#112185=CARTESIAN_POINT('Ctrl Pts',(-8.68810554025373,8.47610873656122,
10.3511949257709));
#112186=CARTESIAN_POINT('Ctrl Pts',(-8.6941562196692,8.47676817976188,10.3391012765721));
#112187=CARTESIAN_POINT('Ctrl Pts',(-8.74704930390492,8.48237143623563,
10.2369456108601));
#112188=CARTESIAN_POINT('Ctrl Pts',(-8.80297191492606,8.48723905629371,
10.1519103500392));
#112189=CARTESIAN_POINT('Ctrl Pts',(-8.87424920774173,8.49317529330558,
10.0647779735337));
#112190=CARTESIAN_POINT('Ctrl Pts',(-8.8813637016999,8.49376546994874,10.0562797540171));
#112191=CARTESIAN_POINT('Ctrl Pts',(-8.89141926482071,8.49459769134213,
10.0445419253335));
#112192=CARTESIAN_POINT('Ctrl Pts',(-8.89427955371946,8.49483420287198,
10.0412332543581));
#112193=CARTESIAN_POINT('Ctrl Pts',(-8.89924277938828,8.49524433590839,
10.0355437377081));
#112194=CARTESIAN_POINT('Ctrl Pts',(-8.90133873271033,8.49541745279741,
10.0331568069406));
#112195=CARTESIAN_POINT('Ctrl Pts',(-8.90576866600101,8.49578322306104,
10.0281448792033));
#112196=CARTESIAN_POINT('Ctrl Pts',(-8.90810434288859,8.49597600634569,
10.0255214413081));
#112197=CARTESIAN_POINT('Ctrl Pts',(-8.91388786799984,8.49645314536408,
10.0190722703125));
#112198=CARTESIAN_POINT('Ctrl Pts',(-8.91734649212379,8.49673828541715,
10.0152563001443));
#112199=CARTESIAN_POINT('Ctrl Pts',(-8.93020617326974,8.49779749216929,
10.0012175897373));
#112200=CARTESIAN_POINT('Ctrl Pts',(-8.93973217576496,8.49858018230051,
9.9911108847064));
#112201=CARTESIAN_POINT('Ctrl Pts',(-9.00842112069237,8.50420047997656,
9.92028200770669));
#112202=CARTESIAN_POINT('Ctrl Pts',(-9.07261441785144,8.50932226641417,
9.86467027633959));
#112203=CARTESIAN_POINT('Ctrl Pts',(-9.22506057525428,8.52064845337834,
9.75420196556883));
#112204=CARTESIAN_POINT('Ctrl Pts',(-9.31508499756035,8.5267964393579,9.70252493029985));
#112205=CARTESIAN_POINT('Ctrl Pts',(-9.42669382011882,8.53363554491536,
9.65334033319139));
#112206=CARTESIAN_POINT('Ctrl Pts',(-9.4437062420526,8.53465896492501,9.64622397259552));
#112207=CARTESIAN_POINT('Ctrl Pts',(-9.46770226104454,8.5360765536621,9.63671510430525));
#112208=CARTESIAN_POINT('Ctrl Pts',(-9.47457585952681,8.53647968316121,
9.63405122163799));
#112209=CARTESIAN_POINT('Ctrl Pts',(-9.48722583358488,8.53721629621282,
9.62925830369983));
#112210=CARTESIAN_POINT('Ctrl Pts',(-9.49299604931491,8.53755029211606,
9.62711357377558));
#112211=CARTESIAN_POINT('Ctrl Pts',(-9.50474689335524,8.538226456425,9.62283009421822));
#112212=CARTESIAN_POINT('Ctrl Pts',(-9.51072825894231,8.53856854035256,
9.62069374170399));
#112213=CARTESIAN_POINT('Ctrl Pts',(-9.52559761667235,8.53941385349291,
9.61549177727954));
#112214=CARTESIAN_POINT('Ctrl Pts',(-9.53450166937893,8.53991555610423,
9.61247272106114));
#112215=CARTESIAN_POINT('Ctrl Pts',(-9.56843106685285,8.54181088182088,
9.6013318082255));
#112216=CARTESIAN_POINT('Ctrl Pts',(-9.59364548291463,8.54318548127028,
9.59379924171949));
#112217=CARTESIAN_POINT('Ctrl Pts',(-9.65810210584721,8.54662486983234,
9.57642212692828));
#112218=CARTESIAN_POINT('Ctrl Pts',(-9.69757511699048,8.54866183660209,
9.56751697269165));
#112219=CARTESIAN_POINT('Ctrl Pts',(-9.80051791310509,8.55385468287236,
9.54873857335101));
#112220=CARTESIAN_POINT('Ctrl Pts',(-9.86435824548773,8.55695764561674,
9.5413861499925));
#112221=CARTESIAN_POINT('Ctrl Pts',(-10.0033391102513,8.56374149225771,
9.53458567073997));
#112222=CARTESIAN_POINT('Ctrl Pts',(-10.0783665272326,8.56742241296831,
9.53667958823188));
#112223=CARTESIAN_POINT('Ctrl Pts',(-10.1648694171721,8.57199828878615,
9.54576641849568));
#112224=CARTESIAN_POINT('Ctrl Pts',(-10.1768281112655,8.57263840930715,
9.5471720559656));
#112225=CARTESIAN_POINT('Ctrl Pts',(-10.1937368810588,8.57355584903683,
9.54937138409314));
#112226=CARTESIAN_POINT('Ctrl Pts',(-10.1987026218256,8.57382679474518,
9.55004323272374));
#112227=CARTESIAN_POINT('Ctrl Pts',(-10.2070815950578,8.57428667920463,
9.55122073163447));
#112228=CARTESIAN_POINT('Ctrl Pts',(-10.2104967199093,8.57447488001396,
9.55171298212554));
#112229=CARTESIAN_POINT('Ctrl Pts',(-10.2175092048529,8.57486294117044,
9.55274907758688));
#112230=CARTESIAN_POINT('Ctrl Pts',(-10.2211063131601,8.57506287126819,
9.55329426478373));
#112231=CARTESIAN_POINT('Ctrl Pts',(-10.2303691701346,8.57557988731915,
9.55473352088277));
#112232=CARTESIAN_POINT('Ctrl Pts',(-10.2360317082139,8.57589805126673,
9.55564748738326));
#112233=CARTESIAN_POINT('Ctrl Pts',(-10.25992914387,8.57724925897089,9.5596489542636));
#112234=CARTESIAN_POINT('Ctrl Pts',(-10.2781092798684,8.5782980541986,9.56304855390563));
#112235=CARTESIAN_POINT('Ctrl Pts',(-10.32720786699,8.58117837771229,9.57319637659068));
#112236=CARTESIAN_POINT('Ctrl Pts',(-10.3579790289336,8.58303531853346,
9.58060422541263));
#112237=CARTESIAN_POINT('Ctrl Pts',(-10.4830038075964,8.59073256139294,
9.61502679418599));
#112238=CARTESIAN_POINT('Ctrl Pts',(-10.5746713296241,8.59671573349496,
9.65048223041181));
#112239=CARTESIAN_POINT('Ctrl Pts',(-10.7170762997039,8.60611768683711,
9.72272450416851));
#112240=CARTESIAN_POINT('Ctrl Pts',(-10.7702310074735,8.60965952272931,
9.7540558534945));
#112241=CARTESIAN_POINT('Ctrl Pts',(-10.8307900159537,8.61372160780584,
9.79511292897453));
#112242=CARTESIAN_POINT('Ctrl Pts',(-10.8402467554536,8.61435689364736,
9.80168856089531));
#112243=CARTESIAN_POINT('Ctrl Pts',(-10.855711434248,8.61539757491591,9.81271483342963));
#112244=CARTESIAN_POINT('Ctrl Pts',(-10.8617645300593,8.61580537552884,
9.81710100892787));
#112245=CARTESIAN_POINT('Ctrl Pts',(-10.8725253356821,8.6165312519021,9.8250249105237));
#112246=CARTESIAN_POINT('Ctrl Pts',(-10.8772457685836,8.61684999087118,
9.82854501358458));
#112247=CARTESIAN_POINT('Ctrl Pts',(-10.8821298712992,8.61718014297625,
9.83223324507816));
#112248=CARTESIAN_POINT('Ctrl Pts',(-10.8823148332192,8.61719264644289,
9.83237298814202));
#112249=CARTESIAN_POINT('Ctrl Pts',(-10.8826547494333,8.61721562585409,
9.83262992969273));
#112250=CARTESIAN_POINT('Ctrl Pts',(-10.8828097136029,8.61722610230432,
9.83274711509683));
#112251=CARTESIAN_POINT('Ctrl Pts',(-10.8830957338018,8.61724543958754,
9.83296349587668));
#112252=CARTESIAN_POINT('Ctrl Pts',(-10.8832267964294,8.61725430075764,
9.83306268245273));
#112253=CARTESIAN_POINT('Ctrl Pts',(-10.8834695682923,8.61727071512074,
9.83324647352652));
#112254=CARTESIAN_POINT('Ctrl Pts',(-10.8835812820982,8.61727826854765,
9.8333310719992));
#112255=CARTESIAN_POINT('Ctrl Pts',(-10.8837888346769,8.61729230239795,
9.83348829403231));
#112256=CARTESIAN_POINT('Ctrl Pts',(-10.8838846766435,8.61729878298445,
9.8335609133546));
#112257=CARTESIAN_POINT('Ctrl Pts',(-10.8840631927785,8.6173108540603,9.83369620941298));
#112258=CARTESIAN_POINT('Ctrl Pts',(-10.8841458691954,8.61731644466389,
9.83375888310001));
#112259=CARTESIAN_POINT('Ctrl Pts',(-10.8843001957146,8.61732688047422,
9.83387589770824));
#112260=CARTESIAN_POINT('Ctrl Pts',(-10.8843718475026,8.61733172576754,
9.83393023646456));
#112261=CARTESIAN_POINT('Ctrl Pts',(-10.8845058427424,8.61734078705367,
9.8340318742442));
#112262=CARTESIAN_POINT('Ctrl Pts',(-10.88456818739,8.61734500310722,9.8340791716495));
#112263=CARTESIAN_POINT('Ctrl Pts',(-10.8846849634896,8.61735290020268,
9.83416777791806));
#112264=CARTESIAN_POINT('Ctrl Pts',(-10.8847393958202,8.61735658128906,
9.83420908557627));
#112265=CARTESIAN_POINT('Ctrl Pts',(-10.8849033399816,8.61736766845881,
9.83433351777107));
#112266=CARTESIAN_POINT('Ctrl Pts',(-10.8850128430213,8.61737507409398,
9.83441665394966));
#112267=CARTESIAN_POINT('Ctrl Pts',(-10.8852290082587,8.61738969362405,
9.83458081752551));
#112268=CARTESIAN_POINT('Ctrl Pts',(-10.8853356710549,8.61739690754953,
9.83466184414135));
#112269=CARTESIAN_POINT('Ctrl Pts',(-10.8855463767032,8.61741115857174,
9.83482195275282));
#112270=CARTESIAN_POINT('Ctrl Pts',(-10.8856504200868,8.61741819569551,
9.83490103404092));
#112271=CARTESIAN_POINT('Ctrl Pts',(-10.8858560900248,8.6174321068266,9.83505740310208));
#112272=CARTESIAN_POINT('Ctrl Pts',(-10.8859577170739,8.61743898085934,
9.83513469025015));
#112273=CARTESIAN_POINT('Ctrl Pts',(-10.8861587416625,8.61745257845554,
9.83528761053412));
#112274=CARTESIAN_POINT('Ctrl Pts',(-10.8862581396372,8.61745930204116,
9.83536324309806));
#112275=CARTESIAN_POINT('Ctrl Pts',(-10.8864548793219,8.61747261044106,
9.83551298337262));
#112276=CARTESIAN_POINT('Ctrl Pts',(-10.8865522214054,8.61747919527402,
9.8355870905523));
#112277=CARTESIAN_POINT('Ctrl Pts',(-10.892319829634,8.61786936193009,9.83997915178782));
#112278=CARTESIAN_POINT('Ctrl Pts',(-10.8979585532419,8.618251337755,9.84433850728786));
#112279=CARTESIAN_POINT('Ctrl Pts',(-10.9099101288337,8.61906221188221,
9.85371868090665));
#112280=CARTESIAN_POINT('Ctrl Pts',(-10.9162137889156,8.61949065258742,
9.85875085914617));
#112281=CARTESIAN_POINT('Ctrl Pts',(-10.9325932443076,8.62060616784555,
9.8720496736586));
#112282=CARTESIAN_POINT('Ctrl Pts',(-10.9426008939329,8.62128999322471,
9.88039932714788));
#112283=CARTESIAN_POINT('Ctrl Pts',(-10.9722931166602,8.62332719461908,
9.90585271096796));
#112284=CARTESIAN_POINT('Ctrl Pts',(-10.9916338788096,8.62466531384855,
9.92335031568456));
#112285=CARTESIAN_POINT('Ctrl Pts',(-11.0996178315456,8.63223052707207,
10.0264232263889));
#112286=CARTESIAN_POINT('Ctrl Pts',(-11.1776333241315,8.63802441659883,
10.1223959681063));
#112287=CARTESIAN_POINT('Ctrl Pts',(-11.2500157820225,8.64484730417465,
10.2387611996853));
#112288=CARTESIAN_POINT('Ctrl Pts',(-11.2571617373649,8.64554118544223,
10.250621378847));
#112289=CARTESIAN_POINT('Ctrl Pts',(-11.281324433762,8.64796527235781,10.2920428561266));
#112290=CARTESIAN_POINT('Ctrl Pts',(-11.2974742549373,8.64972514532873,
10.322094517553));
#112291=CARTESIAN_POINT('Ctrl Pts',(-11.3154748215364,8.651895793797,10.3585939522987));
#112292=CARTESIAN_POINT('Ctrl Pts',(-11.3183511332756,8.65224965719763,
10.3645269397548));
#112293=CARTESIAN_POINT('Ctrl Pts',(-11.322999347385,8.65283348996994,10.3742822322466));
#112294=CARTESIAN_POINT('Ctrl Pts',(-11.3247950392138,8.65306206157142,
10.3780931731842));
#112295=CARTESIAN_POINT('Ctrl Pts',(-11.3280009159035,8.65347572845334,
10.3849737982508));
#112296=CARTESIAN_POINT('Ctrl Pts',(-11.3294169527542,8.65366046541412,
10.3880406657207));
#112297=CARTESIAN_POINT('Ctrl Pts',(-11.3325150243086,8.65406914122047,
10.3948120029844));
#112298=CARTESIAN_POINT('Ctrl Pts',(-11.3341922157194,8.65429335853351,
10.3985185518789));
#112299=CARTESIAN_POINT('Ctrl Pts',(-11.3390019561159,8.65494493713151,
10.4092670538193));
#112300=CARTESIAN_POINT('Ctrl Pts',(-11.3420943112329,8.65537460180141,
10.4163267123689));
#112301=CARTESIAN_POINT('Ctrl Pts',(-11.3655933878837,8.65872240542073,
10.4711478957596));
#112302=CARTESIAN_POINT('Ctrl Pts',(-11.38349848506,8.66176670882384,10.5199367012462));
#112303=CARTESIAN_POINT('Ctrl Pts',(-11.4416195631694,8.67353797512733,
10.7088125266264));
#112304=CARTESIAN_POINT('Ctrl Pts',(-11.4634438448967,8.68243347362415,
10.8537075295653));
#112305=CARTESIAN_POINT('Ctrl Pts',(-11.4634998917645,8.69060327775791,
10.999437145398));
#112306=CARTESIAN_POINT('Origin',(-10.,3.5,11.));
#112307=CARTESIAN_POINT('',(-11.4634994186103,9.26065510840341,11.0013045026646));
#112308=CARTESIAN_POINT('',(-11.4635,9.18928959125266,10.9999999999375));
#112309=CARTESIAN_POINT('',(-11.4635,3.5,11.));
#112310=CARTESIAN_POINT('Ctrl Pts',(-11.4634994144634,9.26057778709026,
11.0013091467826));
#112311=CARTESIAN_POINT('Ctrl Pts',(-11.4635877435601,9.25464699952005,
10.9025657644569));
#112312=CARTESIAN_POINT('Ctrl Pts',(-11.453682574716,9.24882527675797,10.8040494680401));
#112313=CARTESIAN_POINT('Ctrl Pts',(-11.4318075510817,9.24272775562083,
10.6968970697916));
#112314=CARTESIAN_POINT('Ctrl Pts',(-11.4295782608926,9.24214118776937,
10.6865510347163));
#112315=CARTESIAN_POINT('Ctrl Pts',(-11.4256765068438,9.24116956294663,
10.6693514004638));
#112316=CARTESIAN_POINT('Ctrl Pts',(-11.4240663890846,9.24078256357533,
10.6624841922878));
#112317=CARTESIAN_POINT('Ctrl Pts',(-11.4208068992745,9.24002562963409,
10.6490210451381));
#112318=CARTESIAN_POINT('Ctrl Pts',(-11.4191610865205,9.23965559298378,
10.6424244353211));
#112319=CARTESIAN_POINT('Ctrl Pts',(-11.4159642864132,9.23895911046782,
10.6299811154125));
#112320=CARTESIAN_POINT('Ctrl Pts',(-11.4144229074653,9.2386323670594,10.6241321033962));
#112321=CARTESIAN_POINT('Ctrl Pts',(-11.4108523433904,9.2378954610927,10.6109160727615));
#112322=CARTESIAN_POINT('Ctrl Pts',(-11.4088016250538,9.23748599582921,
10.6035550208059));
#112323=CARTESIAN_POINT('Ctrl Pts',(-11.4033635436957,9.23643451146293,
10.5846102280256));
#112324=CARTESIAN_POINT('Ctrl Pts',(-11.3998903431274,9.23579524668041,
10.5730515990501));
#112325=CARTESIAN_POINT('Ctrl Pts',(-11.3716840569564,9.23084261305947,
10.4832293793748));
#112326=CARTESIAN_POINT('Ctrl Pts',(-11.3405488222683,9.226747800436,10.4071256272865));
#112327=CARTESIAN_POINT('Ctrl Pts',(-11.2710077081991,9.21926660010698,
10.2710458664142));
#112328=CARTESIAN_POINT('Ctrl Pts',(-11.234300280176,9.21586728097053,10.2104830391603));
#112329=CARTESIAN_POINT('Ctrl Pts',(-11.1631402345574,9.20977487976479,
10.1102459817806));
#112330=CARTESIAN_POINT('Ctrl Pts',(-11.1306678701584,9.20713275364292,
10.0693300602632));
#112331=CARTESIAN_POINT('Ctrl Pts',(-11.091376028343,9.20397479104373,10.0249199639207));
#112332=CARTESIAN_POINT('Ctrl Pts',(-11.0866303450342,9.20359395804841,
10.0196341492791));
#112333=CARTESIAN_POINT('Ctrl Pts',(-11.0789436800968,9.20297765779986,
10.0111970048797));
#112334=CARTESIAN_POINT('Ctrl Pts',(-11.0760268727035,9.20274391754153,
10.0080236916936));
#112335=CARTESIAN_POINT('Ctrl Pts',(-11.0707962145072,9.20232487611817,
10.0023832612462));
#112336=CARTESIAN_POINT('Ctrl Pts',(-11.0684877808645,9.20213997852701,
9.99991122779515));
#112337=CARTESIAN_POINT('Ctrl Pts',(-11.0634396352549,9.20173569812629,
9.99454274735059));
#112338=CARTESIAN_POINT('Ctrl Pts',(-11.0606966888662,9.20151607621701,
9.99164952611135));
#112339=CARTESIAN_POINT('Ctrl Pts',(-11.0530189145132,9.20090155726755,
9.98361710968607));
#112340=CARTESIAN_POINT('Ctrl Pts',(-11.0480583945807,9.20050477976735,
9.97850275995187));
#112341=CARTESIAN_POINT('Ctrl Pts',(-11.0203384405045,9.19829001114033,
9.95033765101867));
#112342=CARTESIAN_POINT('Ctrl Pts',(-10.9968573509582,9.19642319689324,
9.92801273362056));
#112343=CARTESIAN_POINT('Ctrl Pts',(-10.9049584905991,9.18921556284882,
9.84627063757526));
#112344=CARTESIAN_POINT('Ctrl Pts',(-10.8318159064224,9.18368979199902,
9.79247214079188));
#112345=CARTESIAN_POINT('Ctrl Pts',(-10.7061921957233,9.17494291371066,
9.71693381234001));
#112346=CARTESIAN_POINT('Ctrl Pts',(-10.6565964945217,9.17165161009305,
9.69085972646669));
#112347=CARTESIAN_POINT('Ctrl Pts',(-10.5757232706713,9.16656983228758,
9.65409739632357));
#112348=CARTESIAN_POINT('Ctrl Pts',(-10.5453711172691,9.16472218955835,
9.64151492879573));
#112349=CARTESIAN_POINT('Ctrl Pts',(-10.5050288979023,9.16234257785429,
9.6263613946514));
#112350=CARTESIAN_POINT('Ctrl Pts',(-10.4954006424304,9.16178019335898,
9.62285969605142));
#112351=CARTESIAN_POINT('Ctrl Pts',(-10.4795764453286,9.16086478707162,
9.61729203254613));
#112352=CARTESIAN_POINT('Ctrl Pts',(-10.4734021506136,9.16050980795201,
9.61516596810784));
#112353=CARTESIAN_POINT('Ctrl Pts',(-10.4614118216881,9.15982462492923,
9.61112676480747));
#112354=CARTESIAN_POINT('Ctrl Pts',(-10.4555976142401,9.15949426506742,
9.60920866119674));
#112355=CARTESIAN_POINT('Ctrl Pts',(-10.4421090038998,9.15873214383523,
9.60485243932671));
#112356=CARTESIAN_POINT('Ctrl Pts',(-10.4344261348479,9.15830125517478,
9.60244104802759));
#112357=CARTESIAN_POINT('Ctrl Pts',(-10.4093443373654,9.15690467741667,
9.59479554203964));
#112358=CARTESIAN_POINT('Ctrl Pts',(-10.3918674125743,9.15594734910451,
9.58982188205164));
#112359=CARTESIAN_POINT('Ctrl Pts',(-10.268342237738,9.14928276504524,9.55714243520837));
#112360=CARTESIAN_POINT('Ctrl Pts',(-10.1595694189549,9.1439724906509,9.54110124596277));
#112361=CARTESIAN_POINT('Ctrl Pts',(-9.98834385028947,9.13563078633208,
9.535245947676));
#112362=CARTESIAN_POINT('Ctrl Pts',(-9.92660263098679,9.13261781086763,
9.53703993268307));
#112363=CARTESIAN_POINT('Ctrl Pts',(-9.84635025586176,9.12850584379428,
9.54446539902446));
#112364=CARTESIAN_POINT('Ctrl Pts',(-9.82757321065347,9.12752945492775,
9.54657020661006));
#112365=CARTESIAN_POINT('Ctrl Pts',(-9.79620984333528,9.12586702481034,
9.55070217437578));
#112366=CARTESIAN_POINT('Ctrl Pts',(-9.78359943722578,9.125190004719,9.55253138547809));
#112367=CARTESIAN_POINT('Ctrl Pts',(-9.76609783805104,9.12423644785596,
9.55530390275256));
#112368=CARTESIAN_POINT('Ctrl Pts',(-9.76118480259052,9.1239672324377,9.55610792134571));
#112369=CARTESIAN_POINT('Ctrl Pts',(-9.75284656196811,9.12350757844391,
9.55751619597944));
#112370=CARTESIAN_POINT('Ctrl Pts',(-9.7494191826153,9.12331784902367,9.55810763211673));
#112371=CARTESIAN_POINT('Ctrl Pts',(-9.74283106582253,9.12295157534914,
9.55926869130808));
#112372=CARTESIAN_POINT('Ctrl Pts',(-9.73967005534391,9.12277514060324,
9.55983650787247));
#112373=CARTESIAN_POINT('Ctrl Pts',(-9.73207493810905,9.12234958325666,
9.56122665133343));
#112374=CARTESIAN_POINT('Ctrl Pts',(-9.72764274101372,9.12209990888812,
9.56205907283771));
#112375=CARTESIAN_POINT('Ctrl Pts',(-9.71141777387722,9.12118120205092,
9.56518402770646));
#112376=CARTESIAN_POINT('Ctrl Pts',(-9.69964982875581,9.12050571179411,
9.56760119681718));
#112377=CARTESIAN_POINT('Ctrl Pts',(-9.61393397834814,9.11552515825988,
9.58631016070359));
#112378=CARTESIAN_POINT('Ctrl Pts',(-9.54132530411738,9.11098259187146,
9.60817330256716));
#112379=CARTESIAN_POINT('Ctrl Pts',(-9.40962004770212,9.10248270405019,
9.65926080061698));
#112380=CARTESIAN_POINT('Ctrl Pts',(-9.35015796570116,9.09853753828418,
9.68705052723216));
#112381=CARTESIAN_POINT('Ctrl Pts',(-9.25848438319621,9.09238812134568,
9.7376532271364));
#112382=CARTESIAN_POINT('Ctrl Pts',(-9.22498247231869,9.09012423039904,
9.75794002361032));
#112383=CARTESIAN_POINT('Ctrl Pts',(-9.17090307224934,9.08644889887496,
9.79372853105894));
#112384=CARTESIAN_POINT('Ctrl Pts',(-9.14985021177433,9.08501236587994,
9.80847239787423));
#112385=CARTESIAN_POINT('Ctrl Pts',(-9.12170728193134,9.08308321239783,
9.82930748738281));
#112386=CARTESIAN_POINT('Ctrl Pts',(-9.11427201437805,9.08257265391562,
9.83492274985579));
#112387=CARTESIAN_POINT('Ctrl Pts',(-9.10187404714724,9.08171969621857,
9.84447322638921));
#112388=CARTESIAN_POINT('Ctrl Pts',(-9.09688242159149,9.08137583075347,
9.84837028822827));
#112389=CARTESIAN_POINT('Ctrl Pts',(-9.08707996100995,9.08069959828645,
9.85612619409373));
#112390=CARTESIAN_POINT('Ctrl Pts',(-9.0822679146617,9.08036717284713,9.85998328847165));
#112391=CARTESIAN_POINT('Ctrl Pts',(-9.07171990907488,9.07963739934561,
9.86854810827699));
#112392=CARTESIAN_POINT('Ctrl Pts',(-9.06599506384981,9.07924059643331,
9.87326929017204));
#112393=CARTESIAN_POINT('Ctrl Pts',(-9.04592842082742,9.07784691697698,
9.89007594544118));
#112394=CARTESIAN_POINT('Ctrl Pts',(-9.03178294821479,9.07685938255403,
9.90239361901702));
#112395=CARTESIAN_POINT('Ctrl Pts',(-8.92583626714218,9.06941289107479,
9.99829287749866));
#112396=CARTESIAN_POINT('Ctrl Pts',(-8.84477233680633,9.06347863700027,
10.0929743220037));
#112397=CARTESIAN_POINT('Ctrl Pts',(-8.73766935095357,9.05393429458585,
10.2560963517692));
#112398=CARTESIAN_POINT('Ctrl Pts',(-8.70308158209386,9.05041570019676,
10.3181850210981));
#112399=CARTESIAN_POINT('Ctrl Pts',(-8.6694249938068,9.04618030387344,10.3905085249929));
#112400=CARTESIAN_POINT('Ctrl Pts',(-8.66578392934718,9.04570924407623,
10.3985208444945));
#112401=CARTESIAN_POINT('Ctrl Pts',(-8.66047576666075,9.0450023022064,10.4104870782155));
#112402=CARTESIAN_POINT('Ctrl Pts',(-8.65875336957229,9.04476961959455,
10.4144164175164));
#112403=CARTESIAN_POINT('Ctrl Pts',(-8.6557045564204,9.04435170401406,10.4214557564669));
#112404=CARTESIAN_POINT('Ctrl Pts',(-8.65437161209333,9.0441668654688,10.424562842095));
#112405=CARTESIAN_POINT('Ctrl Pts',(-8.65148435190901,9.04376179236916,
10.4313579215572));
#112406=CARTESIAN_POINT('Ctrl Pts',(-8.64993441379782,9.0435413112134,10.4350476314832));
#112407=CARTESIAN_POINT('Ctrl Pts',(-8.64564136093768,9.04292215597171,
10.4453860290998));
#112408=CARTESIAN_POINT('Ctrl Pts',(-8.64293213405256,9.04252155710716,
10.4520485579467));
#112409=CARTESIAN_POINT('Ctrl Pts',(-8.62786863555786,9.0402384289018,10.489889713662));
#112410=CARTESIAN_POINT('Ctrl Pts',(-8.61654067885616,9.03830354709428,
10.5214637315354));
#112411=CARTESIAN_POINT('Ctrl Pts',(-8.60173242489681,9.03545624272042,
10.56767505946));
#112412=CARTESIAN_POINT('Ctrl Pts',(-8.59737667660224,9.0345700661961,10.5820228963596));
#112413=CARTESIAN_POINT('Ctrl Pts',(-8.58539915775161,9.03198958910947,
10.6237744337858));
#112414=CARTESIAN_POINT('Ctrl Pts',(-8.5783548896762,9.03028405638726,10.6513363596057));
#112415=CARTESIAN_POINT('Ctrl Pts',(-8.567182480993,9.0272207759877,10.7010470224951));
#112416=CARTESIAN_POINT('Ctrl Pts',(-8.56275396330219,9.02586503872493,
10.7231195989814));
#112417=CARTESIAN_POINT('Ctrl Pts',(-8.54039646531599,9.01814187689005,
10.8496173758894));
#112418=CARTESIAN_POINT('Ctrl Pts',(-8.53333767806876,9.01188069924047,
10.9556591124973));
#112419=CARTESIAN_POINT('Ctrl Pts',(-8.53836947750706,9.00522667768161,
11.0752011769721));
#112420=CARTESIAN_POINT('Ctrl Pts',(-8.53913541319428,9.00447254008878,
11.0888463732003));
#112421=CARTESIAN_POINT('Ctrl Pts',(-8.54060138473717,9.00332629101779,
11.1097304510574));
#112422=CARTESIAN_POINT('Ctrl Pts',(-8.54116441710109,9.00292997446441,
11.1169779245923));
#112423=CARTESIAN_POINT('Ctrl Pts',(-8.54224284347945,9.00224020355104,
11.1296374703578));
#112424=CARTESIAN_POINT('Ctrl Pts',(-8.54273443520403,9.00194601887018,
11.1350513823233));
#112425=CARTESIAN_POINT('Ctrl Pts',(-8.54391421717564,9.00128291307834,
11.1472869635453));
#112426=CARTESIAN_POINT('Ctrl Pts',(-8.54462020480608,9.00091455044507,
11.1541068152049));
#112427=CARTESIAN_POINT('Ctrl Pts',(-8.54666444367924,8.99991968705152,
11.1725854037152));
#112428=CARTESIAN_POINT('Ctrl Pts',(-8.54809505411668,8.99929605738093,
11.1842335462639));
#112429=CARTESIAN_POINT('Ctrl Pts',(-8.5556503577789,8.99631616382051,11.2401792389532));
#112430=CARTESIAN_POINT('Ctrl Pts',(-8.56366333813169,8.99401896161288,
11.284199645879));
#112431=CARTESIAN_POINT('Ctrl Pts',(-8.59865740476869,8.98615322456675,
11.4364714875169));
#112432=CARTESIAN_POINT('Ctrl Pts',(-8.6359729848927,8.98087742108433,11.5419387432681));
#112433=CARTESIAN_POINT('Ctrl Pts',(-8.70768111128317,8.97277481424319,
11.6887956499032));
#112434=CARTESIAN_POINT('Ctrl Pts',(-8.73292477266111,8.97014595620894,
11.7341981270518));
#112435=CARTESIAN_POINT('Ctrl Pts',(-8.76462085291051,8.96697042651294,
11.7846846383864));
#112436=CARTESIAN_POINT('Ctrl Pts',(-8.76876912930578,8.96655701013309,
11.7911777023579));
#112437=CARTESIAN_POINT('Ctrl Pts',(-8.77518512542734,8.96592041398787,
11.8010476362268));
#112438=CARTESIAN_POINT('Ctrl Pts',(-8.77741603600157,8.96569957088621,
11.804448408937));
#112439=CARTESIAN_POINT('Ctrl Pts',(-8.781525215121,8.9652936334501,11.8106558170019));
#112440=CARTESIAN_POINT('Ctrl Pts',(-8.78339904760653,8.96510882938309,
11.8134652894205));
#112441=CARTESIAN_POINT('Ctrl Pts',(-8.78763158915703,8.96469209024615,
11.8197638827522));
#112442=CARTESIAN_POINT('Ctrl Pts',(-8.78999562753456,8.96445980817906,
11.8232492968616));
#112443=CARTESIAN_POINT('Ctrl Pts',(-8.79697436286067,8.96377562666277,
11.8334433803736));
#112444=CARTESIAN_POINT('Ctrl Pts',(-8.80162996774863,8.96332113098491,
11.8401236882514));
#112445=CARTESIAN_POINT('Ctrl Pts',(-8.84366256117029,8.95923732544452,
11.8993757902225));
#112446=CARTESIAN_POINT('Ctrl Pts',(-8.88441816822874,8.95541631039829,
11.9494570112974));
#112447=CARTESIAN_POINT('Ctrl Pts',(-8.97528266815056,8.94741767148317,
12.0471571723222));
#112448=CARTESIAN_POINT('Ctrl Pts',(-9.02573605850253,8.94324496191199,
12.0942550594568));
#112449=CARTESIAN_POINT('Ctrl Pts',(-9.13030537370636,8.93527050962021,
12.1788830809087));
#112450=CARTESIAN_POINT('Ctrl Pts',(-9.18400949515908,8.931469310283,12.2166738713741));
#112451=CARTESIAN_POINT('Ctrl Pts',(-9.25430433536874,8.92687059295574,
12.2593837720315));
#112452=CARTESIAN_POINT('Ctrl Pts',(-9.26868163038639,8.92594825581372,
12.2677866475777));
#112453=CARTESIAN_POINT('Ctrl Pts',(-9.2900540357876,8.92460329304843,12.2797932600741));
#112454=CARTESIAN_POINT('Ctrl Pts',(-9.29693945272598,8.92417390865393,
12.2835886922459));
#112455=CARTESIAN_POINT('Ctrl Pts',(-9.30919814896698,8.92341625423245,
12.2902177907251));
#112456=CARTESIAN_POINT('Ctrl Pts',(-9.3145590729222,8.92308720439056,12.2930738114731));
#112457=CARTESIAN_POINT('Ctrl Pts',(-9.32584899316792,8.92239895513897,
12.2989985515554));
#112458=CARTESIAN_POINT('Ctrl Pts',(-9.33178152923678,8.92204000580957,
12.3020602498734));
#112459=CARTESIAN_POINT('Ctrl Pts',(-9.34746576839214,8.92109801361449,
12.3100192365946));
#112460=CARTESIAN_POINT('Ctrl Pts',(-9.35725175215145,8.92051733158653,
12.3148482886332));
#112461=CARTESIAN_POINT('Ctrl Pts',(-9.39963142815733,8.91803183709967,
12.3351750072951));
#112462=CARTESIAN_POINT('Ctrl Pts',(-9.43273947097119,8.9161643654257,12.349574186859));
#112463=CARTESIAN_POINT('Ctrl Pts',(-9.60075544036781,8.90699164084084,
12.4153698474907));
#112464=CARTESIAN_POINT('Ctrl Pts',(-9.74219040319263,8.90031471510722,
12.4478242421376));
#112465=CARTESIAN_POINT('Ctrl Pts',(-9.90671974814241,8.89192922602425,
12.4606710476978));
#112466=CARTESIAN_POINT('Ctrl Pts',(-9.92739700208817,8.89086275113372,
12.4618446728769));
#112467=CARTESIAN_POINT('Ctrl Pts',(-9.96172529594793,8.88906140705812,
12.4630630257577));
#112468=CARTESIAN_POINT('Ctrl Pts',(-9.97536492275711,8.88833762737753,
12.4633562303468));
#112469=CARTESIAN_POINT('Ctrl Pts',(-9.99411964451016,8.88732897251104,
12.4634971201175));
#112470=CARTESIAN_POINT('Ctrl Pts',(-9.99923321598756,8.88705258342828,
12.4635087323438));
#112471=CARTESIAN_POINT('Ctrl Pts',(-10.0078511222671,8.88658431481434,
12.4634831366297));
#112472=CARTESIAN_POINT('Ctrl Pts',(-10.0113555062541,8.88639320954437,
12.4634601407316));
#112473=CARTESIAN_POINT('Ctrl Pts',(-10.0180420390046,8.88602720285449,
12.4633922450245));
#112474=CARTESIAN_POINT('Ctrl Pts',(-10.0212241768802,8.88585243046118,
12.463349552187));
#112475=CARTESIAN_POINT('Ctrl Pts',(-10.0288042782522,8.88543474726858,
12.4632231247295));
#112476=CARTESIAN_POINT('Ctrl Pts',(-10.0332020273367,8.88519132780118,
12.463129940762));
#112477=CARTESIAN_POINT('Ctrl Pts',(-10.0488312490244,8.88432251515276,
12.4627282730109));
#112478=CARTESIAN_POINT('Ctrl Pts',(-10.0600592291526,8.88369153337334,
12.4623102834184));
#112479=CARTESIAN_POINT('Ctrl Pts',(-10.1706133605633,8.87741870649571,
12.4569192584354));
#112480=CARTESIAN_POINT('Ctrl Pts',(-10.2691865864193,8.87136692621747,
12.4419635334144));
#112481=CARTESIAN_POINT('Ctrl Pts',(-10.3803752379357,8.8644726000103,12.4132882683923));
#112482=CARTESIAN_POINT('Ctrl Pts',(-10.3952146324694,8.86355054100444,
12.4092105786047));
#112483=CARTESIAN_POINT('Ctrl Pts',(-10.4647573789175,8.85922464094281,
12.3889161536527));
#112484=CARTESIAN_POINT('Ctrl Pts',(-10.5185498969593,8.85586712182788,
12.3697424968891));
#112485=CARTESIAN_POINT('Ctrl Pts',(-10.6017995354547,8.85069231105968,
12.3344594704143));
#112486=CARTESIAN_POINT('Ctrl Pts',(-10.6320571595934,8.84881554024162,
12.3203971972723));
#112487=CARTESIAN_POINT('Ctrl Pts',(-10.6709457900428,8.84640793599899,
12.30068017723));
#112488=CARTESIAN_POINT('Ctrl Pts',(-10.6800332401621,8.84584563118905,
12.2959521504849));
#112489=CARTESIAN_POINT('Ctrl Pts',(-10.6948310413796,8.84493032119288,
12.2880546223138));
#112490=CARTESIAN_POINT('Ctrl Pts',(-10.700571039241,8.84457535947025,12.2849416745608));
#112491=CARTESIAN_POINT('Ctrl Pts',(-10.7116523436366,8.84389018719403,
12.2788356720092));
#112492=CARTESIAN_POINT('Ctrl Pts',(-10.7169960714237,8.84355982085968,
12.2758473142713));
#112493=CARTESIAN_POINT('Ctrl Pts',(-10.7293247009485,8.84279765190446,
12.268850889797));
#112494=CARTESIAN_POINT('Ctrl Pts',(-10.7362956231097,8.84236672234093,
12.2648185082604));
#112495=CARTESIAN_POINT('Ctrl Pts',(-10.7588882938449,8.84096987013546,
12.2514995301244));
#112496=CARTESIAN_POINT('Ctrl Pts',(-10.7743707408605,8.84001231295309,
12.2419792712989));
#112497=CARTESIAN_POINT('Ctrl Pts',(-10.8818961487801,8.83335104906587,
12.1730686149851));
#112498=CARTESIAN_POINT('Ctrl Pts',(-10.9671931213109,8.8280437578453,12.1037983168661));
#112499=CARTESIAN_POINT('Ctrl Pts',(-11.0872475666993,8.81970312457884,
11.9816001182988));
#112500=CARTESIAN_POINT('Ctrl Pts',(-11.1276931531803,8.81668800129018,
11.934854666268));
#112501=CARTESIAN_POINT('Ctrl Pts',(-11.1765018762316,8.812573314343,11.870650826866));
#112502=CARTESIAN_POINT('Ctrl Pts',(-11.187648040981,8.81159651927403,11.8553838911712));
#112503=CARTESIAN_POINT('Ctrl Pts',(-11.2058101331925,8.80993345993638,
11.8294676865334));
#112504=CARTESIAN_POINT('Ctrl Pts',(-11.2129883876083,8.80925622565848,
11.8189345945206));
#112505=CARTESIAN_POINT('Ctrl Pts',(-11.2227779052904,8.80830241575764,
11.8041587128331));
#112506=CARTESIAN_POINT('Ctrl Pts',(-11.2255066652886,8.80803316662895,
11.7999940330855));
#112507=CARTESIAN_POINT('Ctrl Pts',(-11.230105421393,8.8075734723539,11.792896588397));
#112508=CARTESIAN_POINT('Ctrl Pts',(-11.2319863395222,8.80738373666567,
11.7899708897618));
#112509=CARTESIAN_POINT('Ctrl Pts',(-11.235583870014,8.80701746507647,11.7843309657018));
#112510=CARTESIAN_POINT('Ctrl Pts',(-11.2373019998119,8.80684103877907,
11.7816177610889));
#112511=CARTESIAN_POINT('Ctrl Pts',(-11.2414110225274,8.80641552104535,
11.7750814510423));
#112512=CARTESIAN_POINT('Ctrl Pts',(-11.2437931889061,8.8061658780594,11.7712529317559));
#112513=CARTESIAN_POINT('Ctrl Pts',(-11.2524548919556,8.80524744148726,
11.7571877025385));
#112514=CARTESIAN_POINT('Ctrl Pts',(-11.2586258830092,8.80457219505848,
11.7468850922605));
#112515=CARTESIAN_POINT('Ctrl Pts',(-11.3029040076387,8.79957747836617,
11.6708544507994));
#112516=CARTESIAN_POINT('Ctrl Pts',(-11.3359652213428,8.79501890264714,
11.6023284504375));
#112517=CARTESIAN_POINT('Ctrl Pts',(-11.3875295987129,8.78647654159967,
11.4700539875952));
#112518=CARTESIAN_POINT('Ctrl Pts',(-11.4073169669729,8.78250489947593,
11.4070000285174));
#112519=CARTESIAN_POINT('Ctrl Pts',(-11.431850260053,8.77635755887737,11.3051821911238));
#112520=CARTESIAN_POINT('Ctrl Pts',(-11.4394231093976,8.77411956582275,
11.2671943231907));
#112521=CARTESIAN_POINT('Ctrl Pts',(-11.4494688200691,8.77048119113625,
11.20377007474));
#112522=CARTESIAN_POINT('Ctrl Pts',(-11.4527984197197,8.76905635526781,
11.1784908101196));
#112523=CARTESIAN_POINT('Ctrl Pts',(-11.4564380588712,8.76714015514075,
11.1438982846547));
#112524=CARTESIAN_POINT('Ctrl Pts',(-11.4573220740337,8.7666311630491,11.1346510814868));
#112525=CARTESIAN_POINT('Ctrl Pts',(-11.4586600988221,8.76578008367204,
11.1190923792931));
#112526=CARTESIAN_POINT('Ctrl Pts',(-11.4591613191023,8.76543654427015,
11.1127853061312));
#112527=CARTESIAN_POINT('Ctrl Pts',(-11.4600706334484,8.76476039818953,
11.1003199058104));
#112528=CARTESIAN_POINT('Ctrl Pts',(-11.4604807031084,8.76442773717901,
11.0941618585566));
#112529=CARTESIAN_POINT('Ctrl Pts',(-11.461382260589,8.76362248398171,11.0791957007959));
#112530=CARTESIAN_POINT('Ctrl Pts',(-11.461833089414,8.76315115558401,11.0703853241859));
#112531=CARTESIAN_POINT('Ctrl Pts',(-11.4630747972514,8.76158230661794,
11.0408970541776));
#112532=CARTESIAN_POINT('Ctrl Pts',(-11.4635068166774,8.76049581071048,
11.0202060640286));
#112533=CARTESIAN_POINT('Ctrl Pts',(-11.463499918694,8.75942153142852,10.9995121654828));
#112534=CARTESIAN_POINT('Ctrl Pts',(-11.4634998922174,8.69060334384545,
10.9994383242407));
#112535=CARTESIAN_POINT('Ctrl Pts',(-11.4635041761544,8.69122911239194,
11.010600531755));
#112536=CARTESIAN_POINT('Ctrl Pts',(-11.4633807578742,8.69185105214708,
11.0217626903887));
#112537=CARTESIAN_POINT('Ctrl Pts',(-11.4629135671457,8.69300092039859,
11.0425253298918));
#112538=CARTESIAN_POINT('Ctrl Pts',(-11.4626029579925,8.69352982726182,
11.0521258289666));
#112539=CARTESIAN_POINT('Ctrl Pts',(-11.4619467181113,8.69438189805341,
11.0676720049115));
#112540=CARTESIAN_POINT('Ctrl Pts',(-11.4616592768631,8.6947068458762,11.0736197437169));
#112541=CARTESIAN_POINT('Ctrl Pts',(-11.4610208788094,8.69534542238823,
11.0853448293847));
#112542=CARTESIAN_POINT('Ctrl Pts',(-11.4606719341333,8.6956591072733,11.0911221728518));
#112543=CARTESIAN_POINT('Ctrl Pts',(-11.4598566930235,8.69632419110991,
11.103408240213));
#112544=CARTESIAN_POINT('Ctrl Pts',(-11.4593811192562,8.69667529608018,
11.1099162360673));
#112545=CARTESIAN_POINT('Ctrl Pts',(-11.4580492371702,8.69757274558584,
11.1266059549511));
#112546=CARTESIAN_POINT('Ctrl Pts',(-11.4571297931297,8.69811712925825,
11.1367823777872));
#112547=CARTESIAN_POINT('Ctrl Pts',(-11.4530757017606,8.70025565995408,
11.1769541213546));
#112548=CARTESIAN_POINT('Ctrl Pts',(-11.4491206982659,8.70182445823039,
11.2068601503051));
#112549=CARTESIAN_POINT('Ctrl Pts',(-11.4221473957723,8.71036873031556,
11.3714927638279));
#112550=CARTESIAN_POINT('Ctrl Pts',(-11.3812720274938,8.71675561709629,
11.5025878047017));
#112551=CARTESIAN_POINT('Ctrl Pts',(-11.3098873644176,8.725087116408,11.6534061608572));
#112552=CARTESIAN_POINT('Ctrl Pts',(-11.2961243703384,8.72661787500154,
11.6802984237786));
#112553=CARTESIAN_POINT('Ctrl Pts',(-11.2757276207569,8.72881269286219,
11.7172838753264));
#112554=CARTESIAN_POINT('Ctrl Pts',(-11.2697855386576,8.72944420292249,
11.7277511864386));
#112555=CARTESIAN_POINT('Ctrl Pts',(-11.2591630097293,8.73056169863935,
11.7459371454822));
#112556=CARTESIAN_POINT('Ctrl Pts',(-11.2545389331615,8.73104455530924,
11.7536881100169));
#112557=CARTESIAN_POINT('Ctrl Pts',(-11.2475882844969,8.7317658580685,11.7650977155111));
#112558=CARTESIAN_POINT('Ctrl Pts',(-11.2453165833911,8.7320009129424,11.7687897294129));
#112559=CARTESIAN_POINT('Ctrl Pts',(-11.2412418095311,8.73242141161767,
11.7753466831609));
#112560=CARTESIAN_POINT('Ctrl Pts',(-11.2394451611175,8.73260644082897,
11.7782155235676));
#112561=CARTESIAN_POINT('Ctrl Pts',(-11.2355194045234,8.73300994659747,
11.7844359864338));
#112562=CARTESIAN_POINT('Ctrl Pts',(-11.2333866353785,8.73322865380585,
11.7877851373768));
#112563=CARTESIAN_POINT('Ctrl Pts',(-11.2274290134348,8.73383809164023,
11.7970570720046));
#112564=CARTESIAN_POINT('Ctrl Pts',(-11.2235750007559,8.73423065406589,
11.8029608785832));
#112565=CARTESIAN_POINT('Ctrl Pts',(-11.2023888347466,8.73637856635628,
11.834908389493));
#112566=CARTESIAN_POINT('Ctrl Pts',(-11.1842687470721,8.73817943874383,
11.8604174497835));
#112567=CARTESIAN_POINT('Ctrl Pts',(-11.0883129876362,8.74746320560208,
11.9867233774404));
#112568=CARTESIAN_POINT('Ctrl Pts',(-10.9983733011471,8.75531439409573,
12.0776382947922));
#112569=CARTESIAN_POINT('Ctrl Pts',(-10.8713828452819,8.76468758076267,
12.1762832954717));
#112570=CARTESIAN_POINT('Ctrl Pts',(-10.8442780517665,8.76660879379222,
12.1958868103142));
#112571=CARTESIAN_POINT('Ctrl Pts',(-10.8036559928054,8.76937210551735,
12.2231965162453));
#112572=CARTESIAN_POINT('Ctrl Pts',(-10.790651080159,8.77024018236295,12.2316426296469));
#112573=CARTESIAN_POINT('Ctrl Pts',(-10.7698305707955,8.77160413693417,
12.2446989166562));
#112574=CARTESIAN_POINT('Ctrl Pts',(-10.7621023627579,8.77210490134224,
12.2494456749752));
#112575=CARTESIAN_POINT('Ctrl Pts',(-10.7473660157143,8.77304948632569,
12.2583093175423));
#112576=CARTESIAN_POINT('Ctrl Pts',(-10.7403667581082,8.77349380065015,
12.2624402430465));
#112577=CARTESIAN_POINT('Ctrl Pts',(-10.7281134394506,8.77426423248375,
12.2695351321741));
#112578=CARTESIAN_POINT('Ctrl Pts',(-10.7228748378746,8.77459127994824,
12.2725252857242));
#112579=CARTESIAN_POINT('Ctrl Pts',(-10.711982338249,8.77526654607694,12.2786536716897));
#112580=CARTESIAN_POINT('Ctrl Pts',(-10.7063258196691,8.77561458590073,
12.2817869949436));
#112581=CARTESIAN_POINT('Ctrl Pts',(-10.6919178059187,8.77649455166173,
12.2896437082547));
#112582=CARTESIAN_POINT('Ctrl Pts',(-10.6831385164502,8.77702466606678,
12.2943156177097));
#112583=CARTESIAN_POINT('Ctrl Pts',(-10.649440554567,8.77903700988905,12.3118096388524));
#112584=CARTESIAN_POINT('Ctrl Pts',(-10.6242023050027,8.78049763845742,
12.3240049765261));
#112585=CARTESIAN_POINT('Ctrl Pts',(-10.4673832087891,8.78932434278479,
12.3942996624366));
#112586=CARTESIAN_POINT('Ctrl Pts',(-10.3281996667631,8.7960116787744,12.4334569852349));
#112587=CARTESIAN_POINT('Ctrl Pts',(-10.1452473095871,8.80526438873417,
12.4568411778385));
#112588=CARTESIAN_POINT('Ctrl Pts',(-10.1047519500462,8.807347193197,12.4603114338398));
#112589=CARTESIAN_POINT('Ctrl Pts',(-10.0568694251549,8.80990364845809,
12.4624129015824));
#112590=CARTESIAN_POINT('Ctrl Pts',(-10.0495684008938,8.81029602026976,
12.4626785687462));
#112591=CARTESIAN_POINT('Ctrl Pts',(-10.0382843104793,8.81090683021201,
12.4630045889954));
#112592=CARTESIAN_POINT('Ctrl Pts',(-10.0343023708242,8.81112321583334,
12.463103366971));
#112593=CARTESIAN_POINT('Ctrl Pts',(-10.0269370377758,8.81152509895022,
12.4632559913406));
#112594=CARTESIAN_POINT('Ctrl Pts',(-10.0235538199722,8.81171034726568,
12.4633143603086));
#112595=CARTESIAN_POINT('Ctrl Pts',(-10.0158529560286,8.81213346855527,
12.4634205061721));
#112596=CARTESIAN_POINT('Ctrl Pts',(-10.0115352986583,8.81237173788718,
12.4634609082618));
#112597=CARTESIAN_POINT('Ctrl Pts',(-10.0002769775564,8.81299561878296,
12.463516431904));
#112598=CARTESIAN_POINT('Ctrl Pts',(-9.99333635320748,8.81338280255223,
12.4635012863553));
#112599=CARTESIAN_POINT('Ctrl Pts',(-9.9452654451271,8.81608101168285,12.4630544305883));
#112600=CARTESIAN_POINT('Ctrl Pts',(-9.90417231774244,8.8184711726772,12.4609382696216));
#112601=CARTESIAN_POINT('Ctrl Pts',(-9.78011980128589,8.82583669264184,
12.4492938098128));
#112602=CARTESIAN_POINT('Ctrl Pts',(-9.69783329735729,8.83091788028911,
12.4343972127257));
#112603=CARTESIAN_POINT('Ctrl Pts',(-9.54603557561309,8.84029120069118,
12.3932676088698));
#112604=CARTESIAN_POINT('Ctrl Pts',(-9.47636117999831,8.84459438315749,
12.3686062787301));
#112605=CARTESIAN_POINT('Ctrl Pts',(-9.39267877979302,8.84971746654369,
12.3316550546928));
#112606=CARTESIAN_POINT('Ctrl Pts',(-9.37665048162581,8.85069701962615,
12.3242279506662));
#112607=CARTESIAN_POINT('Ctrl Pts',(-9.35351801073911,8.85210872370557,
12.3129958491874));
#112608=CARTESIAN_POINT('Ctrl Pts',(-9.34630500497379,8.85254862622572,
12.3094196880721));
#112609=CARTESIAN_POINT('Ctrl Pts',(-9.33367766170435,8.8533183282836,12.3030287877865));
#112610=CARTESIAN_POINT('Ctrl Pts',(-9.32825077939944,8.85364899169769,
12.3002393881487));
#112611=CARTESIAN_POINT('Ctrl Pts',(-9.31699845898757,8.85433438584008,
12.2943664804152));
#112612=CARTESIAN_POINT('Ctrl Pts',(-9.31117607915413,8.85468891276253,
12.2912773902836));
#112613=CARTESIAN_POINT('Ctrl Pts',(-9.29611595811837,8.85560572290779,
12.2831563260414));
#112614=CARTESIAN_POINT('Ctrl Pts',(-9.2869111591315,8.85616587523206,12.2780638537231));
#112615=CARTESIAN_POINT('Ctrl Pts',(-9.24942614195055,8.85844701120498,
12.2567945532017));
#112616=CARTESIAN_POINT('Ctrl Pts',(-9.2216339693851,8.86013803850938,12.2397742502176));
#112617=CARTESIAN_POINT('Ctrl Pts',(-9.17288197040072,8.86311941267036,
12.2076316772401));
#112618=CARTESIAN_POINT('Ctrl Pts',(-9.15171134095858,8.86441953494931,
12.1928557889026));
#112619=CARTESIAN_POINT('Ctrl Pts',(-9.04718037307769,8.87089661411987,
12.115708121791));
#112620=CARTESIAN_POINT('Ctrl Pts',(-8.97025856051638,8.87582979390374,
12.0451320758737));
#112621=CARTESIAN_POINT('Ctrl Pts',(-8.86965832404969,8.88340530742882,
11.9308485229977));
#112622=CARTESIAN_POINT('Ctrl Pts',(-8.83964577580599,8.8858536496044,11.8931564812548));
#112623=CARTESIAN_POINT('Ctrl Pts',(-8.80711791617393,8.88882396997827,
11.8478928112567));
#112624=CARTESIAN_POINT('Ctrl Pts',(-8.80273569034753,8.88923141488444,
11.841693562537));
#112625=CARTESIAN_POINT('Ctrl Pts',(-8.79609338116264,8.8898607275815,11.8321402871411));
#112626=CARTESIAN_POINT('Ctrl Pts',(-8.79379857436683,8.89008034123494,
11.8288104272786));
#112627=CARTESIAN_POINT('Ctrl Pts',(-8.78961161023833,8.89048517412593,
11.8226807492016));
#112628=CARTESIAN_POINT('Ctrl Pts',(-8.78771532323919,8.89067011460675,
11.8198838521814));
#112629=CARTESIAN_POINT('Ctrl Pts',(-8.78346090266613,8.89108864016574,
11.8135618363444));
#112630=CARTESIAN_POINT('Ctrl Pts',(-8.78110841061585,8.89132258575099,
11.8100330421049));
#112631=CARTESIAN_POINT('Ctrl Pts',(-8.77508665612442,8.8919278564787,11.8009146379893));
#112632=CARTESIAN_POINT('Ctrl Pts',(-8.77144034181243,8.89230060816078,
11.79531007802));
#112633=CARTESIAN_POINT('Ctrl Pts',(-8.74847242949861,8.89468772120599,
11.7594724196399));
#112634=CARTESIAN_POINT('Ctrl Pts',(-8.7302311108433,8.89676245761913,11.7285644700424));
#112635=CARTESIAN_POINT('Ctrl Pts',(-8.7084402559117,8.8994536989981,11.6883336905298));
#112636=CARTESIAN_POINT('Ctrl Pts',(-8.70382339198042,8.90003742114885,
11.6795999097701));
#112637=CARTESIAN_POINT('Ctrl Pts',(-8.69462145491289,8.90122796725129,
11.6617575692998));
#112638=CARTESIAN_POINT('Ctrl Pts',(-8.69004243253148,8.90183489911153,
11.6526464534744));
#112639=CARTESIAN_POINT('Ctrl Pts',(-8.63897856300995,8.90876657860311,
11.5483392932407));
#112640=CARTESIAN_POINT('Ctrl Pts',(-8.60286173223419,8.91521933920611,
11.4484015389924));
#112641=CARTESIAN_POINT('Ctrl Pts',(-8.56670818222448,8.92411858355313,
11.2995593829959));
#112642=CARTESIAN_POINT('Ctrl Pts',(-8.55779018093599,8.92680278988726,
11.2531655512976));
#112643=CARTESIAN_POINT('Ctrl Pts',(-8.54951362092497,8.93005185553253,
11.1950714409487));
#112644=CARTESIAN_POINT('Ctrl Pts',(-8.54803043389354,8.93068228772016,
11.1837062669191));
#112645=CARTESIAN_POINT('Ctrl Pts',(-8.54588049215706,8.93168000932376,
11.1655744897553));
#112646=CARTESIAN_POINT('Ctrl Pts',(-8.54512713732619,8.9320499736209,11.1588187972773));
#112647=CARTESIAN_POINT('Ctrl Pts',(-8.54379218718497,8.93274650191618,
11.1460399543327));
#112648=CARTESIAN_POINT('Ctrl Pts',(-8.54320082802234,8.93307336205915,
11.1400179859969));
#112649=CARTESIAN_POINT('Ctrl Pts',(-8.54194655786245,8.9338107748212,11.1263760647004));
#112650=CARTESIAN_POINT('Ctrl Pts',(-8.54130599765319,8.93422062743271,
11.1187542015309));
#112651=CARTESIAN_POINT('Ctrl Pts',(-8.53980724165087,8.93527358788995,
11.0990732447401));
#112652=CARTESIAN_POINT('Ctrl Pts',(-8.53903865340875,8.93591392923553,
11.0870077847237));
#112653=CARTESIAN_POINT('Ctrl Pts',(-8.53364145529618,8.94145882479623,
10.9817358816986));
#112654=CARTESIAN_POINT('Ctrl Pts',(-8.53778769339262,8.94607392746065,
10.888291387662));
#112655=CARTESIAN_POINT('Ctrl Pts',(-8.56015387701888,8.95389287733966,
10.7295064786447));
#112656=CARTESIAN_POINT('Ctrl Pts',(-8.57404851758469,8.95712410389077,
10.6638671253848));
#112657=CARTESIAN_POINT('Ctrl Pts',(-8.60474886444194,8.96272212291293,
10.5559900325723));
#112658=CARTESIAN_POINT('Ctrl Pts',(-8.61910838052428,8.96502504122162,
10.5131651215242));
#112659=CARTESIAN_POINT('Ctrl Pts',(-8.63812836538541,8.9678304599192,10.4640951956629));
#112660=CARTESIAN_POINT('Ctrl Pts',(-8.64088779888032,8.96823239288008,
10.4571350734028));
#112661=CARTESIAN_POINT('Ctrl Pts',(-8.64521139180291,8.96885494346698,
10.4464692847369));
#112662=CARTESIAN_POINT('Ctrl Pts',(-8.64673766554276,8.96907338166948,
10.4427482804031));
#112663=CARTESIAN_POINT('Ctrl Pts',(-8.64957503619267,8.96947712342239,
10.4359112698022));
#112664=CARTESIAN_POINT('Ctrl Pts',(-8.65088160793411,8.9696621589135,10.4327934750273));
#112665=CARTESIAN_POINT('Ctrl Pts',(-8.65386219391348,8.97008228155642,
10.4257496427532));
#112666=CARTESIAN_POINT('Ctrl Pts',(-8.65554257793381,8.97031774180539,
10.4218264057545));
#112667=CARTESIAN_POINT('Ctrl Pts',(-8.65993479842792,8.97092951269295,
10.4116944605255));
#112668=CARTESIAN_POINT('Ctrl Pts',(-8.66267260126068,8.97130730002528,
10.4054972016335));
#112669=CARTESIAN_POINT('Ctrl Pts',(-8.68092221578194,8.97380155779059,
10.3649515955078));
#112670=CARTESIAN_POINT('Ctrl Pts',(-8.69771178667431,8.97598460022114,
10.33119686408));
#112671=CARTESIAN_POINT('Ctrl Pts',(-8.76536318953748,8.98429693210015,
10.2074145363756));
#112672=CARTESIAN_POINT('Ctrl Pts',(-8.82441523068524,8.99062442433493,
10.1222062472152));
#112673=CARTESIAN_POINT('Ctrl Pts',(-8.92055331120898,8.99931240625607,
10.0107865307667));
#112674=CARTESIAN_POINT('Ctrl Pts',(-8.95062428422832,9.00185631380975,
9.97894194674716));
#112675=CARTESIAN_POINT('Ctrl Pts',(-8.99547335236816,9.00540419184556,
9.93552549884425));
#112676=CARTESIAN_POINT('Ctrl Pts',(-9.00911384962417,9.00645347463193,
9.92281643604425));
#112677=CARTESIAN_POINT('Ctrl Pts',(-9.03386443242001,9.00830542903683,
9.900624046293));
#112678=CARTESIAN_POINT('Ctrl Pts',(-9.04488049422913,9.00911214541781,
9.89104004859289));
#112679=CARTESIAN_POINT('Ctrl Pts',(-9.06174108829313,9.01032102002174,
9.87680894188968));
#112680=CARTESIAN_POINT('Ctrl Pts',(-9.06748056118138,9.01072812214244,
9.8720392571041));
#112681=CARTESIAN_POINT('Ctrl Pts',(-9.07788395267128,9.01145823019151,
9.8635273889857));
#112682=CARTESIAN_POINT('Ctrl Pts',(-9.08253477084014,9.01178185911014,
9.85976951668824));
#112683=CARTESIAN_POINT('Ctrl Pts',(-9.09260340951733,9.01247662375643,
9.85173552149119));
#112684=CARTESIAN_POINT('Ctrl Pts',(-9.09802872746412,9.01284737616267,
9.84746899791573));
#112685=CARTESIAN_POINT('Ctrl Pts',(-9.11268086756289,9.01383916048615,
9.83611323901252));
#112686=CARTESIAN_POINT('Ctrl Pts',(-9.12196249051524,9.01445741524365,
9.82909531666123));
#112687=CARTESIAN_POINT('Ctrl Pts',(-9.1677059456582,9.01745740504885,9.79535807532475));
#112688=CARTESIAN_POINT('Ctrl Pts',(-9.2053102239292,9.0197786039421,9.77022594637324));
#112689=CARTESIAN_POINT('Ctrl Pts',(-9.3391211136247,9.02764206083292,9.68950121096527));
#112690=CARTESIAN_POINT('Ctrl Pts',(-9.44043796494813,9.03289712536169,
9.64314437965328));
#112691=CARTESIAN_POINT('Ctrl Pts',(-9.59527745331882,9.04097295544686,
9.59262071072323));
#112692=CARTESIAN_POINT('Ctrl Pts',(-9.64534851713804,9.04359684584337,
9.57917696428167));
#112693=CARTESIAN_POINT('Ctrl Pts',(-9.70355718614101,9.0467667935509,9.56681708944067));
#112694=CARTESIAN_POINT('Ctrl Pts',(-9.71110523292502,9.04718013548706,
9.56527654042919));
#112695=CARTESIAN_POINT('Ctrl Pts',(-9.72265669218006,9.0478166773709,9.56301374911531));
#112696=CARTESIAN_POINT('Ctrl Pts',(-9.72665165185683,9.0480375419899,9.56224846535303));
#112697=CARTESIAN_POINT('Ctrl Pts',(-9.73397012071315,9.04844355581598,
9.56087812709937));
#112698=CARTESIAN_POINT('Ctrl Pts',(-9.73729257994235,9.04862841496215,
9.56026791637773));
#112699=CARTESIAN_POINT('Ctrl Pts',(-9.74476413251379,9.04904532915929,
9.55892239723007));
#112700=CARTESIAN_POINT('Ctrl Pts',(-9.74891427580035,9.0492777318521,9.55819350693232));
#112701=CARTESIAN_POINT('Ctrl Pts',(-9.76110006292114,9.04996241823258,
9.55610752354358));
#112702=CARTESIAN_POINT('Ctrl Pts',(-9.76914383108824,9.05041730299622,
9.55479963789781));
#112703=CARTESIAN_POINT('Ctrl Pts',(-9.84509082859884,9.05473706674155,
9.54310116565416));
#112704=CARTESIAN_POINT('Ctrl Pts',(-9.91362943967456,9.05881898805314,
9.53743741322794));
#112705=CARTESIAN_POINT('Ctrl Pts',(-10.0644830973373,9.06787544526682,
9.53561326795602));
#112706=CARTESIAN_POINT('Ctrl Pts',(-10.1466056423097,9.0728468720453,9.54154360736761));
#112707=CARTESIAN_POINT('Ctrl Pts',(-10.2829361158806,9.08092925426571,
9.56302574385637));
#112708=CARTESIAN_POINT('Ctrl Pts',(-10.3375355136485,9.08412158034588,
9.57486184063684));
#112709=CARTESIAN_POINT('Ctrl Pts',(-10.4029015224438,9.0878818765142,9.59300077761915));
#112710=CARTESIAN_POINT('Ctrl Pts',(-10.4144328138846,9.08854297785567,
9.59635406766419));
#112711=CARTESIAN_POINT('Ctrl Pts',(-10.4325392255552,9.08957769580528,
9.60186198420036));
#112712=CARTESIAN_POINT('Ctrl Pts',(-10.4391423997892,9.08995433923746,
9.60392190481373));
#112713=CARTESIAN_POINT('Ctrl Pts',(-10.4514792438239,9.09065677850308,
9.60786668541154));
#112714=CARTESIAN_POINT('Ctrl Pts',(-10.4572163186318,9.09098292821465,
9.60974034343602));
#112715=CARTESIAN_POINT('Ctrl Pts',(-10.4700273770158,9.09171015477695,
9.61401215588393));
#112716=CARTESIAN_POINT('Ctrl Pts',(-10.4770949499233,9.09211061138931,
9.61642909442921));
#112717=CARTESIAN_POINT('Ctrl Pts',(-10.4949950746895,9.0931231428494,9.62270397302916));
#112718=CARTESIAN_POINT('Ctrl Pts',(-10.5058013361027,9.09373280304401,
9.62663570448953));
#112719=CARTESIAN_POINT('Ctrl Pts',(-10.5737487475284,9.09755788824588,
9.65226836083816));
#112720=CARTESIAN_POINT('Ctrl Pts',(-10.6295325247783,9.10065724523289,
9.67740478646118));
#112721=CARTESIAN_POINT('Ctrl Pts',(-10.770686464596,9.10857407175856,9.7519702463093));
#112722=CARTESIAN_POINT('Ctrl Pts',(-10.8529147033749,9.1132521137058,9.8066555115232));
#112723=CARTESIAN_POINT('Ctrl Pts',(-10.9535202924956,9.11973879195422,
9.88930814693232));
#112724=CARTESIAN_POINT('Ctrl Pts',(-10.977355019592,9.12134193643803,9.9102228244174));
#112725=CARTESIAN_POINT('Ctrl Pts',(-11.0140058537742,9.12394832660967,
9.94455350009359));
#112726=CARTESIAN_POINT('Ctrl Pts',(-11.0272791109758,9.12492361087835,
9.95746810547042));
#112727=CARTESIAN_POINT('Ctrl Pts',(-11.0443394244582,9.12622464198219,
9.97470962761396));
#112728=CARTESIAN_POINT('Ctrl Pts',(-11.0483516192572,9.12653416330093,
9.97881242594844));
#112729=CARTESIAN_POINT('Ctrl Pts',(-11.0548683111548,9.12704293878031,
9.98555515819117));
#112730=CARTESIAN_POINT('Ctrl Pts',(-11.0573873129517,9.12724110035875,
9.98818106324872));
#112731=CARTESIAN_POINT('Ctrl Pts',(-11.062275548278,9.1276286323657,9.99331493866138));
#112732=CARTESIAN_POINT('Ctrl Pts',(-11.0646457430461,9.12781792729118,
9.99582193102718));
#112733=CARTESIAN_POINT('Ctrl Pts',(-11.0704353729412,9.12828368277919,
10.0019892519744));
#112734=CARTESIAN_POINT('Ctrl Pts',(-11.0738449083667,9.12856087398673,
10.0056587848762));
#112735=CARTESIAN_POINT('Ctrl Pts',(-11.0853770600799,9.12950813445925,
10.0181988232992));
#112736=CARTESIAN_POINT('Ctrl Pts',(-11.0934089238754,9.1301844296147,10.0271516976484));
#112737=CARTESIAN_POINT('Ctrl Pts',(-11.1509120965089,9.13514147027932,
10.0928604280109));
#112738=CARTESIAN_POINT('Ctrl Pts',(-11.1960448076829,9.13965697341427,
10.1532557705715));
#112739=CARTESIAN_POINT('Ctrl Pts',(-11.2709985495337,9.14808450829513,
10.2715820004104));
#112740=CARTESIAN_POINT('Ctrl Pts',(-11.3019984404251,9.15198435365961,
10.3285604992716));
#112741=CARTESIAN_POINT('Ctrl Pts',(-11.3458115499405,9.1581367030656,10.4236204225296));
#112742=CARTESIAN_POINT('Ctrl Pts',(-11.3610158206485,9.160444404595,10.4605016510532));
#112743=CARTESIAN_POINT('Ctrl Pts',(-11.3836289358003,9.16418217027848,
10.5224213487448));
#112744=CARTESIAN_POINT('Ctrl Pts',(-11.3919080509611,9.16563842225506,
10.547117565857));
#112745=CARTESIAN_POINT('Ctrl Pts',(-11.4022628869522,9.16758946938339,
10.5809788094145));
#112746=CARTESIAN_POINT('Ctrl Pts',(-11.4049156834548,9.16810273015466,
10.58996111116));
#112747=CARTESIAN_POINT('Ctrl Pts',(-11.4092204660547,9.16895899714929,
10.6050694084826));
#112748=CARTESIAN_POINT('Ctrl Pts',(-11.4109191454895,9.16930349360786,
10.6111817124785));
#112749=CARTESIAN_POINT('Ctrl Pts',(-11.4141892089613,9.16998006981207,
10.6232519488273));
#112750=CARTESIAN_POINT('Ctrl Pts',(-11.415762815904,9.17031221466447,10.6292091377886));
#112751=CARTESIAN_POINT('Ctrl Pts',(-11.4191418914766,9.17104030793275,
10.6423364584381));
#112752=CARTESIAN_POINT('Ctrl Pts',(-11.4209307451835,9.17143572145567,
10.6495107174242));
#112753=CARTESIAN_POINT('Ctrl Pts',(-11.4270232309098,9.17281873590946,
10.6747583863271));
#112754=CARTESIAN_POINT('Ctrl Pts',(-11.4310371148213,9.17379718903327,
10.6929003002947));
#112755=CARTESIAN_POINT('Ctrl Pts',(-11.4538534043649,9.17982202874215,
10.8062137438306));
#112756=CARTESIAN_POINT('Ctrl Pts',(-11.4634999999959,9.18456812665941,
10.9029819768369));
#112757=CARTESIAN_POINT('Ctrl Pts',(-11.4635,9.18928959125266,10.9999999999375));
#112758=CARTESIAN_POINT('Origin',(-10.,3.5,11.));
#112759=CARTESIAN_POINT('',(-11.4634998211562,9.76065504584291,10.9992764838212));
#112760=CARTESIAN_POINT('',(-11.4634998339897,9.68830622417397,10.9993269840173));
#112761=CARTESIAN_POINT('',(-11.4635,3.5,11.));
#112762=CARTESIAN_POINT('Ctrl Pts',(-11.4634998211562,9.76065504584291,
10.9992764838212));
#112763=CARTESIAN_POINT('Ctrl Pts',(-11.4634788673927,9.758339008624,10.9568920423594));
#112764=CARTESIAN_POINT('Ctrl Pts',(-11.4616168184814,9.75602297140509,
10.9145549795653));
#112765=CARTESIAN_POINT('Ctrl Pts',(-11.4579250610406,9.75370693418618,
10.8723803839928));
#112766=CARTESIAN_POINT('Ctrl Pts',(-11.4531267995415,9.75069672769344,
10.8175650984766));
#112767=CARTESIAN_POINT('Ctrl Pts',(-11.4452227348698,9.74768652120071,
10.7629056994581));
#112768=CARTESIAN_POINT('Ctrl Pts',(-11.4342328984321,9.74467631470797,
10.708781451389));
#112769=CARTESIAN_POINT('Ctrl Pts',(-11.4232625847686,9.74167145566349,
10.6547533517458));
#112770=CARTESIAN_POINT('Ctrl Pts',(-11.4092174820364,9.738666596619,10.601259029792));
#112771=CARTESIAN_POINT('Ctrl Pts',(-11.3921693129869,9.73566173757451,
10.5486721214265));
#112772=CARTESIAN_POINT('Ctrl Pts',(-11.3751380014157,9.73265984977849,
10.4961372117633));
#112773=CARTESIAN_POINT('Ctrl Pts',(-11.3551096679902,9.72965796198248,
10.444508438124));
#112774=CARTESIAN_POINT('Ctrl Pts',(-11.3322065426073,9.72665607418646,
10.3941469007801));
#112775=CARTESIAN_POINT('Ctrl Pts',(-11.3093170193905,9.72365596921159,
10.3438152731531));
#112776=CARTESIAN_POINT('Ctrl Pts',(-11.2835563064641,9.72065586423672,
10.2947498698395));
#112777=CARTESIAN_POINT('Ctrl Pts',(-11.255094875594,9.71765575926185,10.2472921527859));
#112778=CARTESIAN_POINT('Ctrl Pts',(-11.2266391087995,9.7146562513343,10.1998438802362));
#112779=CARTESIAN_POINT('Ctrl Pts',(-11.1954839629081,9.71165674340675,
10.1540031111753));
#112780=CARTESIAN_POINT('Ctrl Pts',(-11.1618448678258,9.70865723547921,
10.1100849742212));
#112781=CARTESIAN_POINT('Ctrl Pts',(-11.128174854497,9.70565497065451,10.0661264713839));
#112782=CARTESIAN_POINT('Ctrl Pts',(-11.092016652586,9.70265270582982,10.0240945512531));
#112783=CARTESIAN_POINT('Ctrl Pts',(-11.0536269897426,9.69965044100512,
9.98427246936693));
#112784=CARTESIAN_POINT('Ctrl Pts',(-11.0152198424233,9.69664680880643,
9.94443225061321));
#112785=CARTESIAN_POINT('Ctrl Pts',(-10.9745795963937,9.69364317660773,
9.90680423581745));
#112786=CARTESIAN_POINT('Ctrl Pts',(-10.9319986021011,9.69063954440904,
9.87163354548196));
#112787=CARTESIAN_POINT('Ctrl Pts',(-10.889337309732,9.68763024804275,9.83639653121886));
#112788=CARTESIAN_POINT('Ctrl Pts',(-10.8447283847183,9.68462095167646,
9.80362641182894));
#112789=CARTESIAN_POINT('Ctrl Pts',(-10.7984949412382,9.68161165531017,
9.77352616056561));
#112790=CARTESIAN_POINT('Ctrl Pts',(-10.7632188166337,9.67931556171214,
9.75055966414512));
#112791=CARTESIAN_POINT('Ctrl Pts',(-10.7269975994523,9.67701946811412,
9.72914661305899));
#112792=CARTESIAN_POINT('Ctrl Pts',(-10.6899836595581,9.6747233745161,9.70935876420177));
#112793=CARTESIAN_POINT('Ctrl Pts',(-10.6414579364402,9.67171316802338,
9.68341665489134));
#112794=CARTESIAN_POINT('Ctrl Pts',(-10.591365224381,9.66870296153067,9.66016059465073));
#112795=CARTESIAN_POINT('Ctrl Pts',(-10.5400340736877,9.66569275503795,
9.63978110244849));
#112796=CARTESIAN_POINT('Ctrl Pts',(-10.488794109653,9.66268789599348,9.61943781317125));
#112797=CARTESIAN_POINT('Ctrl Pts',(-10.4363205597793,9.65968303694902,
9.6019611442763));
#112798=CARTESIAN_POINT('Ctrl Pts',(-10.3829655137402,9.65667817790455,
9.58749525123428));
#112799=CARTESIAN_POINT('Ctrl Pts',(-10.3296632259492,9.65367629010856,
9.57304366227838));
#112800=CARTESIAN_POINT('Ctrl Pts',(-10.2754816758471,9.65067440231256,
9.5615970891755));
#112801=CARTESIAN_POINT('Ctrl Pts',(-10.220790061141,9.64767251451656,9.55325054038325));
#112802=CARTESIAN_POINT('Ctrl Pts',(-10.1661309277846,9.64467240954171,
9.54490894860629));
#112803=CARTESIAN_POINT('Ctrl Pts',(-10.1109628512463,9.64167230456686,
9.5396638114467));
#112804=CARTESIAN_POINT('Ctrl Pts',(-10.0556649512334,9.63867219959201,
9.53755900522306));
#112805=CARTESIAN_POINT('Ctrl Pts',(-10.0003780559899,9.63567269166448,
9.53545461787439));
#112806=CARTESIAN_POINT('Ctrl Pts',(-9.94496191598655,9.63267318373695,
9.53648934039428));
#112807=CARTESIAN_POINT('Ctrl Pts',(-9.88979817165473,9.62967367580942,
9.54065500753613));
#112808=CARTESIAN_POINT('Ctrl Pts',(-9.83458372541682,9.62667141098474,
9.54482450341128));
#112809=CARTESIAN_POINT('Ctrl Pts',(-9.77962266602956,9.62366914616006,
9.55213065330776));
#112810=CARTESIAN_POINT('Ctrl Pts',(-9.72529251492394,9.62066688133539,
9.5625132878377));
#112811=CARTESIAN_POINT('Ctrl Pts',(-9.67093761928698,9.61766324913671,
9.57290065111255));
#112812=CARTESIAN_POINT('Ctrl Pts',(-9.61721471785987,9.61465961693804,
9.58636716354264));
#112813=CARTESIAN_POINT('Ctrl Pts',(-9.56448886747576,9.61165598473936,
9.60280198130421));
#112814=CARTESIAN_POINT('Ctrl Pts',(-9.51166358812249,9.60864668837309,
9.61926779139641));
#112815=CARTESIAN_POINT('Ctrl Pts',(-9.45983961144264,9.60563739200682,
9.63871290278073));
#112816=CARTESIAN_POINT('Ctrl Pts',(-9.40936351397626,9.60262809564055,
9.66097767330879));
#112817=CARTESIAN_POINT('Ctrl Pts',(-9.37085024371385,9.60033200204236,
9.6779656967044));
#112818=CARTESIAN_POINT('Ctrl Pts',(-9.33312129533429,9.59803590844418,
9.6965942174547));
#112819=CARTESIAN_POINT('Ctrl Pts',(-9.29632003954256,9.59573981484599,
9.71677485870537));
#112820=CARTESIAN_POINT('Ctrl Pts',(-9.2480731478601,9.59272960835328,9.74323192359506));
#112821=CARTESIAN_POINT('Ctrl Pts',(-9.20121912931898,9.58971940186056,
9.77246931550857));
#112822=CARTESIAN_POINT('Ctrl Pts',(-9.15609710226321,9.58670919536784,
9.80431603289521));
#112823=CARTESIAN_POINT('Ctrl Pts',(-9.11105523173663,9.58370433632337,
9.83610617653066));
#112824=CARTESIAN_POINT('Ctrl Pts',(-9.06773967475705,9.58069947727891,
9.87049614477097));
#112825=CARTESIAN_POINT('Ctrl Pts',(-9.02646359002306,9.57769461823444,
9.90726988306847));
#112826=CARTESIAN_POINT('Ctrl Pts',(-8.98522831968392,9.57469273043844,
9.94400725895696));
#112827=CARTESIAN_POINT('Ctrl Pts',(-8.94602891903112,9.57169084264244,
9.98312338601127));
#112828=CARTESIAN_POINT('Ctrl Pts',(-8.90914674100313,9.56868895484644,
10.0243610210042));
#112829=CARTESIAN_POINT('Ctrl Pts',(-8.87228646730048,9.56568884987159,
10.065574164966));
#112830=CARTESIAN_POINT('Ctrl Pts',(-8.83774103984014,9.56268874489674,
10.1089059266928));
#112831=CARTESIAN_POINT('Ctrl Pts',(-8.80575441577487,9.55968863992189,
10.1540628069657));
#112832=CARTESIAN_POINT('Ctrl Pts',(-8.77377415732961,9.55668913199436,
10.1992107006215));
#112833=CARTESIAN_POINT('Ctrl Pts',(-8.74435199604565,9.55368962406683,
10.2461825608034));
#112834=CARTESIAN_POINT('Ctrl Pts',(-8.71768968642659,9.55069011613929,
10.2946543331789));
#112835=CARTESIAN_POINT('Ctrl Pts',(-8.69100287103957,9.54768785131462,
10.3431706567589));
#112836=CARTESIAN_POINT('Ctrl Pts',(-8.66708123020108,9.54468558648994,
10.3931891830754));
#112837=CARTESIAN_POINT('Ctrl Pts',(-8.64608071804832,9.54168332166527,
10.4443608833429));
#112838=CARTESIAN_POINT('Ctrl Pts',(-8.62507064126487,9.53867968946659,
10.4955558896332));
#112839=CARTESIAN_POINT('Ctrl Pts',(-8.60698451801093,9.53567605726792,
10.5479046168425));
#112840=CARTESIAN_POINT('Ctrl Pts',(-8.59192905414153,9.53267242506924,
10.601040777235));
#112841=CARTESIAN_POINT('Ctrl Pts',(-8.57684519908939,9.52966312870297,
10.6542771403482));
#112842=CARTESIAN_POINT('Ctrl Pts',(-8.56480353540812,9.52665383233669,
10.7083033862982));
#112843=CARTESIAN_POINT('Ctrl Pts',(-8.55585980377181,9.52364453597042,
10.7627420314552));
#112844=CARTESIAN_POINT('Ctrl Pts',(-8.54903573513436,9.52134844237225,
10.804278726225));
#112845=CARTESIAN_POINT('Ctrl Pts',(-8.54401412856267,9.51905234877408,
10.8460552602913));
#112846=CARTESIAN_POINT('Ctrl Pts',(-8.54079933768928,9.51675625517591,
10.8879032689506));
#112847=CARTESIAN_POINT('Ctrl Pts',(-8.53658470795139,9.51374604868319,
10.9427665147148));
#112848=CARTESIAN_POINT('Ctrl Pts',(-8.53545966515834,9.51073584219047,
10.9979829834363));
#112849=CARTESIAN_POINT('Ctrl Pts',(-8.53746636104217,9.50772563569775,
11.053175228413));
#112850=CARTESIAN_POINT('Ctrl Pts',(-8.53946949215315,9.50472077665328,
11.1082694277325));
#112851=CARTESIAN_POINT('Ctrl Pts',(-8.54459330239428,9.50171591760881,
11.1633389652341));
#112852=CARTESIAN_POINT('Ctrl Pts',(-8.55282802674087,9.49871105856434,
11.2180035087178));
#112853=CARTESIAN_POINT('Ctrl Pts',(-8.56105460847188,9.49570917076833,
11.2726139991033));
#112854=CARTESIAN_POINT('Ctrl Pts',(-8.57238593237142,9.49270728297233,
11.3268197691464));
#112855=CARTESIAN_POINT('Ctrl Pts',(-8.58676035740054,9.48970539517632,
11.380244608884));
#112856=CARTESIAN_POINT('Ctrl Pts',(-8.6011262454587,9.48670529020147,11.4336377196096));
#112857=CARTESIAN_POINT('Ctrl Pts',(-8.61853151551821,9.48370518522661,
11.4862503103739));
#112858=CARTESIAN_POINT('Ctrl Pts',(-8.63886372590758,9.48070508025175,
11.5377176706691));
#112859=CARTESIAN_POINT('Ctrl Pts',(-8.65919189000795,9.47770557232422,
11.5891747885062));
#112860=CARTESIAN_POINT('Ctrl Pts',(-8.68244564371486,9.47470606439668,
11.6394866376286));
#112861=CARTESIAN_POINT('Ctrl Pts',(-8.70846389145155,9.47170655646915,
11.688307148238));
#112862=CARTESIAN_POINT('Ctrl Pts',(-8.73450605298833,9.46870429164447,
11.7371725305829));
#112863=CARTESIAN_POINT('Ctrl Pts',(-8.76331753600472,9.46570202681979,
11.7845433688876));
#112864=CARTESIAN_POINT('Ctrl Pts',(-8.79469129795319,9.46269976199511,
11.830098297053));
#112865=CARTESIAN_POINT('Ctrl Pts',(-8.82607934900303,9.45969612979643,
11.8756739730964));
#112866=CARTESIAN_POINT('Ctrl Pts',(-8.86003168099162,9.45669249759774,
11.9194316723883));
#112867=CARTESIAN_POINT('Ctrl Pts',(-8.89629988096166,9.45368886539906,
11.9610818369082));
#112868=CARTESIAN_POINT('Ctrl Pts',(-8.93263647451303,9.45067956903279,
12.0028105441711));
#112869=CARTESIAN_POINT('Ctrl Pts',(-8.97129729043019,9.44767027266651,
12.0424233985027));
#112870=CARTESIAN_POINT('Ctrl Pts',(-9.01199668423977,9.44466097630023,
12.0796674015857));
#112871=CARTESIAN_POINT('Ctrl Pts',(-9.04305032808208,9.44236488270209,
12.1080845817632));
#112872=CARTESIAN_POINT('Ctrl Pts',(-9.07528998392297,9.44006878910395,
12.1351234412503));
#112873=CARTESIAN_POINT('Ctrl Pts',(-9.10857704016443,9.43777269550581,
12.160688311597));
#112874=CARTESIAN_POINT('Ctrl Pts',(-9.15221677371128,9.4347624890131,12.194204165988));
#112875=CARTESIAN_POINT('Ctrl Pts',(-9.19784096890391,9.43175228252038,
12.2253258136369));
#112876=CARTESIAN_POINT('Ctrl Pts',(-9.24515658492047,9.42874207602766,
12.2538116559959));
#112877=CARTESIAN_POINT('Ctrl Pts',(-9.29238814763082,9.4257372169832,12.2822468949931));
#112878=CARTESIAN_POINT('Ctrl Pts',(-9.34130471952884,9.42273235793873,
12.308055350696));
#112879=CARTESIAN_POINT('Ctrl Pts',(-9.39158246742835,9.41972749889426,
12.3310373233157));
#112880=CARTESIAN_POINT('Ctrl Pts',(-9.44181049995711,9.41672561109826,
12.3539965710256));
#112881=CARTESIAN_POINT('Ctrl Pts',(-9.49339656428801,9.41372372330227,
12.3741346537078));
#112882=CARTESIAN_POINT('Ctrl Pts',(-9.54599192552215,9.41072183550627,
12.3912975664138));
#112883=CARTESIAN_POINT('Ctrl Pts',(-9.5985560503715,9.40772173053142,12.408450286066));
#112884=CARTESIAN_POINT('Ctrl Pts',(-9.65212778299837,9.40472162555657,
12.4226311744769));
#112885=CARTESIAN_POINT('Ctrl Pts',(-9.70634025235392,9.40172152058171,
12.4337350531435));
#112886=CARTESIAN_POINT('Ctrl Pts',(-9.76054193295044,9.39872201265418,
12.4448367220405));
#112887=CARTESIAN_POINT('Ctrl Pts',(-9.81538357998686,9.39572250472665,
12.4528624914055));
#112888=CARTESIAN_POINT('Ctrl Pts',(-9.87048733978993,9.39272299679912,
12.457758114656));
#112889=CARTESIAN_POINT('Ctrl Pts',(-9.92564174636634,9.38972073197445,
12.4626582375544));
#112890=CARTESIAN_POINT('Ctrl Pts',(-9.98105821987884,9.38671846714977,
12.4644224197221));
#112891=CARTESIAN_POINT('Ctrl Pts',(-10.0363544807912,9.3837162023251,12.4630483935012));
#112892=CARTESIAN_POINT('Ctrl Pts',(-10.0916759262472,9.38071257012642,
12.4616737414834));
#112893=CARTESIAN_POINT('Ctrl Pts',(-10.1468765227223,9.37770893792775,
12.4571580750236));
#112894=CARTESIAN_POINT('Ctrl Pts',(-10.2015780155307,9.37470530572907,
12.4495511559289));
#112895=CARTESIAN_POINT('Ctrl Pts',(-10.2563826629209,9.3716960093628,12.4419298919137));
#112896=CARTESIAN_POINT('Ctrl Pts',(-10.3106858071257,9.36868671299653,
12.4312058327413));
#112897=CARTESIAN_POINT('Ctrl Pts',(-10.3641194595772,9.36567741663025,
12.4174799007948));
#112898=CARTESIAN_POINT('Ctrl Pts',(-10.4048893447556,9.36338132303208,
12.4070070125726));
#112899=CARTESIAN_POINT('Ctrl Pts',(-10.4451532387728,9.36108522943391,
12.3947875948399));
#112900=CARTESIAN_POINT('Ctrl Pts',(-10.4847552668445,9.35878913583574,
12.3808854337948));
#112901=CARTESIAN_POINT('Ctrl Pts',(-10.5366740048791,9.35577892934302,
12.3626595324316));
#112902=CARTESIAN_POINT('Ctrl Pts',(-10.5876724399118,9.3527687228503,12.3414632175733));
#112903=CARTESIAN_POINT('Ctrl Pts',(-10.6373880871114,9.34975851635758,
12.317409836159));
#112904=CARTESIAN_POINT('Ctrl Pts',(-10.6870154174957,9.34675365731311,
12.2933991841099));
#112905=CARTESIAN_POINT('Ctrl Pts',(-10.7353640108114,9.34374879826863,
12.2665417658343));
#112906=CARTESIAN_POINT('Ctrl Pts',(-10.7820896387808,9.34074393922416,
12.2369996147581));
#112907=CARTESIAN_POINT('Ctrl Pts',(-10.8287690637675,9.33774205142816,
12.2074866753919));
#112908=CARTESIAN_POINT('Ctrl Pts',(-10.8738282583114,9.33474016363216,
12.1752945429008));
#112909=CARTESIAN_POINT('Ctrl Pts',(-10.9169476492224,9.33173827583616,
12.1406310790898));
#112910=CARTESIAN_POINT('Ctrl Pts',(-10.9600414315273,9.3287381708613,12.1059882019098));
#112911=CARTESIAN_POINT('Ctrl Pts',(-11.0011972828855,9.32573806588645,
12.068877232753));
#112912=CARTESIAN_POINT('Ctrl Pts',(-11.040126605484,9.32273796091159,12.0295479078529));
#112913=CARTESIAN_POINT('Ctrl Pts',(-11.0790481808044,9.31973845298405,
11.9902264098349));
#112914=CARTESIAN_POINT('Ctrl Pts',(-11.1157437360589,9.31673894505652,
11.948687807931));
#112915=CARTESIAN_POINT('Ctrl Pts',(-11.1499613218517,9.31373943712899,
11.9052188731158));
#112916=CARTESIAN_POINT('Ctrl Pts',(-11.1842103575913,9.31073717230431,
11.8617099852867));
#112917=CARTESIAN_POINT('Ctrl Pts',(-11.2159765463204,9.30773490747963,
11.8162676357775));
#112918=CARTESIAN_POINT('Ctrl Pts',(-11.2450490475493,9.30473264265495,
11.7692107118316));
#112919=CARTESIAN_POINT('Ctrl Pts',(-11.2741347897762,9.30172901045627,
11.7221323559276));
#112920=CARTESIAN_POINT('Ctrl Pts',(-11.3005241468463,9.29872537825759,
11.6734384248046));
#112921=CARTESIAN_POINT('Ctrl Pts',(-11.3240520483837,9.29572174605891,
11.6234728728428));
#112922=CARTESIAN_POINT('Ctrl Pts',(-11.3476243181955,9.29271244969263,
11.5734130972074));
#112923=CARTESIAN_POINT('Ctrl Pts',(-11.368324155093,9.28970315332636,11.5220774013604));
#112924=CARTESIAN_POINT('Ctrl Pts',(-11.386034942466,9.28669385696008,11.4698291053811));
#112925=CARTESIAN_POINT('Ctrl Pts',(-11.3995482760017,9.28439776336194,
11.4299636473769));
#112926=CARTESIAN_POINT('Ctrl Pts',(-11.411322481028,9.2821016697638,11.3895673180003));
#112927=CARTESIAN_POINT('Ctrl Pts',(-11.421325777003,9.27980557616565,11.3488055126096));
#112928=CARTESIAN_POINT('Ctrl Pts',(-11.4384553450834,9.2758737629206,11.2790053065305));
#112929=CARTESIAN_POINT('Ctrl Pts',(-11.4504497976639,9.27194194967556,
11.2078990836009));
#112930=CARTESIAN_POINT('Ctrl Pts',(-11.4571541790753,9.26801013643051,
11.1361394447004));
#112931=CARTESIAN_POINT('Ctrl Pts',(-11.4613346856349,9.26555846042148,
11.0913938339238));
#112932=CARTESIAN_POINT('Ctrl Pts',(-11.4634592272291,9.26310678441244,
11.0463945317134));
#112933=CARTESIAN_POINT('Ctrl Pts',(-11.4634994186103,9.26065510840341,
11.0013045026646));
#112934=CARTESIAN_POINT('Ctrl Pts',(-11.4635,9.18928959125266,10.9999999999375));
#112935=CARTESIAN_POINT('Ctrl Pts',(-11.4635,9.18931070478979,11.0004338470187));
#112936=CARTESIAN_POINT('Ctrl Pts',(-11.4634998070825,9.18933181826334,
11.0008676990741));
#112937=CARTESIAN_POINT('Ctrl Pts',(-11.4634162934266,9.19390164597574,
11.0947723710105));
#112938=CARTESIAN_POINT('Ctrl Pts',(-11.4543786882082,9.19841535153124,
11.1880093984724));
#112939=CARTESIAN_POINT('Ctrl Pts',(-11.4343089561222,9.20394569799821,
11.2910729990247));
#112940=CARTESIAN_POINT('Ctrl Pts',(-11.4319670270922,9.20456026192431,
11.3023840097753));
#112941=CARTESIAN_POINT('Ctrl Pts',(-11.4285379422702,9.20542139636589,
11.3180116245272));
#112942=CARTESIAN_POINT('Ctrl Pts',(-11.427564552336,9.20566191668663,11.3223530575614));
#112943=CARTESIAN_POINT('Ctrl Pts',(-11.4258579286926,9.20607711447965,
11.329805446705));
#112944=CARTESIAN_POINT('Ctrl Pts',(-11.4251342665793,9.20625125777558,
11.3329185896152));
#112945=CARTESIAN_POINT('Ctrl Pts',(-11.4235983581644,9.20661695972425,
11.3394291782735));
#112946=CARTESIAN_POINT('Ctrl Pts',(-11.4227841411512,9.20680863386454,
11.342826106506));
#112947=CARTESIAN_POINT('Ctrl Pts',(-11.420762385351,9.20727923823071,11.3511296450391));
#112948=CARTESIAN_POINT('Ctrl Pts',(-11.419541585996,9.20755890652332,11.3560329582264));
#112949=CARTESIAN_POINT('Ctrl Pts',(-11.4150332432856,9.20857552668693,
11.3737487642164));
#112950=CARTESIAN_POINT('Ctrl Pts',(-11.4115975208428,9.20932024748357,
11.3865224864759));
#112951=CARTESIAN_POINT('Ctrl Pts',(-11.402570587407,9.21120258237549,11.4183569449842));
#112952=CARTESIAN_POINT('Ctrl Pts',(-11.3967636649921,9.21234965395902,
11.4373533841521));
#112953=CARTESIAN_POINT('Ctrl Pts',(-11.3695441099538,9.21744767387213,
11.5203185100442));
#112954=CARTESIAN_POINT('Ctrl Pts',(-11.344110804997,9.22152106032847,11.5828789216155));
#112955=CARTESIAN_POINT('Ctrl Pts',(-11.2697294680659,9.23169700736126,
11.7348247048393));
#112956=CARTESIAN_POINT('Ctrl Pts',(-11.2155934171519,9.23773363401411,
11.8212909808977));
#112957=CARTESIAN_POINT('Ctrl Pts',(-11.1415253723073,9.24447707203091,
11.9160208072718));
#112958=CARTESIAN_POINT('Ctrl Pts',(-11.1298581114288,9.2455036517799,11.9303735737946));
#112959=CARTESIAN_POINT('Ctrl Pts',(-11.1131584311969,9.24692483478562,
11.9501394779548));
#112960=CARTESIAN_POINT('Ctrl Pts',(-11.1083526820278,9.24732845915661,
11.9557411027778));
#112961=CARTESIAN_POINT('Ctrl Pts',(-11.0994597763015,9.24806569146908,
11.9659494663672));
#112962=CARTESIAN_POINT('Ctrl Pts',(-11.0953855429715,9.24839981501118,
11.9705671976394));
#112963=CARTESIAN_POINT('Ctrl Pts',(-11.0870522488457,9.24907594924944,
11.979892830405));
#112964=CARTESIAN_POINT('Ctrl Pts',(-11.0827914562261,9.24941787754999,
11.9845990122182));
#112965=CARTESIAN_POINT('Ctrl Pts',(-11.0721547751027,9.25026226759842,
11.9961950137961));
#112966=CARTESIAN_POINT('Ctrl Pts',(-11.0657429157468,9.25076321014763,
12.0030515491843));
#112967=CARTESIAN_POINT('Ctrl Pts',(-11.0411857703223,9.25265209448541,
12.0288104613804));
#112968=CARTESIAN_POINT('Ctrl Pts',(-11.0225994332753,9.25402118331006,
12.0472866288312));
#112969=CARTESIAN_POINT('Ctrl Pts',(-10.9742545206584,9.25744360974625,
12.0928300974333));
#112970=CARTESIAN_POINT('Ctrl Pts',(-10.9438574363473,9.25946949343498,
12.1191885146192));
#112971=CARTESIAN_POINT('Ctrl Pts',(-10.8620329652188,9.2646643176182,12.1844336850034));
#112972=CARTESIAN_POINT('Ctrl Pts',(-10.8090552544612,9.2677790510141,12.2212345419651));
#112973=CARTESIAN_POINT('Ctrl Pts',(-10.6894606284566,9.27458120824155,
12.2931028859242));
#112974=CARTESIAN_POINT('Ctrl Pts',(-10.6222214494893,9.27826846510201,
12.3267664158778));
#112975=CARTESIAN_POINT('Ctrl Pts',(-10.541561872582,9.28285134077685,12.3596645983925));
#112976=CARTESIAN_POINT('Ctrl Pts',(-10.5303632025621,9.28349113156792,
12.3640718225078));
#112977=CARTESIAN_POINT('Ctrl Pts',(-10.5144274840568,9.28440818493755,
12.3701174091051));
#112978=CARTESIAN_POINT('Ctrl Pts',(-10.5097341265907,9.28467908148262,
12.3718704274806));
#112979=CARTESIAN_POINT('Ctrl Pts',(-10.5017936211981,9.28513890719721,
12.3747899170307));
#112980=CARTESIAN_POINT('Ctrl Pts',(-10.4985511317041,9.28532709887036,
12.3759690850817));
#112981=CARTESIAN_POINT('Ctrl Pts',(-10.491880727274,9.28571516672002,12.3783681797009));
#112982=CARTESIAN_POINT('Ctrl Pts',(-10.4884523992187,9.28591511282023,
12.3795868011033));
#112983=CARTESIAN_POINT('Ctrl Pts',(-10.479606675768,9.2864322164833,12.3826939652239));
#112984=CARTESIAN_POINT('Ctrl Pts',(-10.4741827075524,9.28675045271687,
12.3845634411398));
#112985=CARTESIAN_POINT('Ctrl Pts',(-10.4512170148637,9.28810237555627,
12.3923282382564));
#112986=CARTESIAN_POINT('Ctrl Pts',(-10.4335760114101,9.28915183384186,
12.3979222063333));
#112987=CARTESIAN_POINT('Ctrl Pts',(-10.3854680990713,9.2920344924298,12.4121790612834));
#112988=CARTESIAN_POINT('Ctrl Pts',(-10.3548190891514,9.29389315160753,
12.4201896183692));
#112989=CARTESIAN_POINT('Ctrl Pts',(-10.2281329114532,9.30160436492201,
12.4489440044418));
#112990=CARTESIAN_POINT('Ctrl Pts',(-10.1303818483636,9.30760009445275,
12.4609879686413));
#112991=CARTESIAN_POINT('Ctrl Pts',(-10.0029387493462,9.31510437547275,
12.463788803362));
#112992=CARTESIAN_POINT('Ctrl Pts',(-9.97370791366097,9.3168062485537,12.4635556591013));
#112993=CARTESIAN_POINT('Ctrl Pts',(-9.90883508549313,9.32053474383792,
12.4610938357323));
#112994=CARTESIAN_POINT('Ctrl Pts',(-9.87322733151111,9.32254849869958,
12.458435887098));
#112995=CARTESIAN_POINT('Ctrl Pts',(-9.82694574265264,9.32512362994786,
12.4532730854023));
#112996=CARTESIAN_POINT('Ctrl Pts',(-9.81615495523334,9.32572105737832,
12.4519474663954));
#112997=CARTESIAN_POINT('Ctrl Pts',(-9.79877083918716,9.32667889503289,
12.4496149621946));
#112998=CARTESIAN_POINT('Ctrl Pts',(-9.79216800988718,9.32704162117717,
12.4486830501215));
#112999=CARTESIAN_POINT('Ctrl Pts',(-9.77955896126588,9.32773230034248,
12.4468154494086));
#113000=CARTESIAN_POINT('Ctrl Pts',(-9.7735517648403,9.32806048393344,12.4458874072798));
#113001=CARTESIAN_POINT('Ctrl Pts',(-9.75976705402127,9.32881163979397,
12.4436698136899));
#113002=CARTESIAN_POINT('Ctrl Pts',(-9.75199379129647,9.32923380719507,
12.4423547840332));
#113003=CARTESIAN_POINT('Ctrl Pts',(-9.72773079402021,9.33054736285011,
12.4380481835979));
#113004=CARTESIAN_POINT('Ctrl Pts',(-9.71128126793625,9.33143185376321,
12.4348360961403));
#113005=CARTESIAN_POINT('Ctrl Pts',(-9.62993138743596,9.33578064760873,
12.4174952693153));
#113006=CARTESIAN_POINT('Ctrl Pts',(-9.56598752164667,9.33911357766149,
12.3992419509615));
#113007=CARTESIAN_POINT('Ctrl Pts',(-9.42983710549426,9.34623614843183,
12.3501401484218));
#113008=CARTESIAN_POINT('Ctrl Pts',(-9.35842794888089,9.34998806402997,
12.3177059411876));
#113009=CARTESIAN_POINT('Ctrl Pts',(-9.28291642515852,9.35425842926083,
12.275808858601));
#113010=CARTESIAN_POINT('Ctrl Pts',(-9.27590734334583,9.35465791541158,
12.2718439052434));
#113011=CARTESIAN_POINT('Ctrl Pts',(-9.25760927934127,9.35570986764527,
12.2612926236925));
#113012=CARTESIAN_POINT('Ctrl Pts',(-9.24637531821011,9.35636483054804,
12.2546126459496));
#113013=CARTESIAN_POINT('Ctrl Pts',(-9.20580473223473,9.35876890977939,
12.2297468975157));
#113014=CARTESIAN_POINT('Ctrl Pts',(-9.17702627751852,9.36054894780729,
12.2106764471404));
#113015=CARTESIAN_POINT('Ctrl Pts',(-9.14356918399046,9.36274229331912,
12.1867612523143));
#113016=CARTESIAN_POINT('Ctrl Pts',(-9.13821362696425,9.36309730717949,
12.1828779550769));
#113017=CARTESIAN_POINT('Ctrl Pts',(-9.12948555959472,9.36368265598932,
12.1764585259247));
#113018=CARTESIAN_POINT('Ctrl Pts',(-9.12609730860128,9.36391158083808,
12.1739438399));
#113019=CARTESIAN_POINT('Ctrl Pts',(-9.12001594450787,9.36432561183346,
12.1693894668398));
#113020=CARTESIAN_POINT('Ctrl Pts',(-9.11731897034202,9.36451035657473,
12.1673550713338));
#113021=CARTESIAN_POINT('Ctrl Pts',(-9.11139422199671,9.36491871437721,
12.1628536131513));
#113022=CARTESIAN_POINT('Ctrl Pts',(-9.1081697048281,9.36514260308794,12.1603824706177));
#113023=CARTESIAN_POINT('Ctrl Pts',(-9.09887963399047,9.36579229968712,
12.1532013315938));
#113024=CARTESIAN_POINT('Ctrl Pts',(-9.09284090357253,9.36622039108618,
12.1484570491762));
#113025=CARTESIAN_POINT('Ctrl Pts',(-9.04700269876655,9.36951246213953,
12.1118575224423));
#113026=CARTESIAN_POINT('Ctrl Pts',(-9.00885816539702,9.37249805186184,
12.0779925298275));
#113027=CARTESIAN_POINT('Ctrl Pts',(-8.89503119094708,9.38201322418886,
11.9657789385272));
#113028=CARTESIAN_POINT('Ctrl Pts',(-8.82626172405252,9.38865873790665,
11.8809242442921));
#113029=CARTESIAN_POINT('Ctrl Pts',(-8.74172123076185,9.39777969282462,
11.7489053036056));
#113030=CARTESIAN_POINT('Ctrl Pts',(-8.71789397169585,9.40050555926008,
11.7073397160796));
#113031=CARTESIAN_POINT('Ctrl Pts',(-8.69076981891896,9.40381589248003,
11.6541320055381));
#113032=CARTESIAN_POINT('Ctrl Pts',(-8.68552215720694,9.40446754798275,
11.6435218411537));
#113033=CARTESIAN_POINT('Ctrl Pts',(-8.67739932184916,9.40549468991658,
11.6265843657826));
#113034=CARTESIAN_POINT('Ctrl Pts',(-8.67443957646659,9.40587306025991,
11.6202983855893));
#113035=CARTESIAN_POINT('Ctrl Pts',(-8.6689938842059,9.40657709237264,11.6085157014111));
#113036=CARTESIAN_POINT('Ctrl Pts',(-8.66649695178861,9.40690312262903,
11.6030242624107));
#113037=CARTESIAN_POINT('Ctrl Pts',(-8.66100150152525,9.40762802784437,
11.5907372000281));
#113038=CARTESIAN_POINT('Ctrl Pts',(-8.6580206091867,9.40802630112904,11.5839338454001));
#113039=CARTESIAN_POINT('Ctrl Pts',(-8.64940198222725,9.40919317617536,
11.5638487596563));
#113040=CARTESIAN_POINT('Ctrl Pts',(-8.64390862909211,9.40995694614799,
11.550505806135));
#113041=CARTESIAN_POINT('Ctrl Pts',(-8.60151729682826,9.41602161482387,
11.4430532479255));
#113042=CARTESIAN_POINT('Ctrl Pts',(-8.57426149988435,9.42098098231308,
11.3454310961212));
#113043=CARTESIAN_POINT('Ctrl Pts',(-8.54108168023866,9.43059822153739,
11.1506589601929));
#113044=CARTESIAN_POINT('Ctrl Pts',(-8.53432621167576,9.43524501531815,
11.0541906260235));
#113045=CARTESIAN_POINT('Ctrl Pts',(-8.53743741546067,9.44092691352552,
10.9464066532307));
#113046=CARTESIAN_POINT('Ctrl Pts',(-8.53789797794449,9.44153212453165,
10.9350444613398));
#113047=CARTESIAN_POINT('Ctrl Pts',(-8.53872145120537,9.44238225341211,
10.9192732637801));
#113048=CARTESIAN_POINT('Ctrl Pts',(-8.53897202985836,9.44262132283926,
10.9148585144847));
#113049=CARTESIAN_POINT('Ctrl Pts',(-8.53943775171228,9.44303468400678,
10.9072619890059));
#113050=CARTESIAN_POINT('Ctrl Pts',(-8.53964329634233,9.44320845230994,
10.904079629436));
#113051=CARTESIAN_POINT('Ctrl Pts',(-8.5400962386056,9.44357415971811,10.8974061066962));
#113052=CARTESIAN_POINT('Ctrl Pts',(-8.54034575996971,9.44376621945698,
10.8939151366112));
#113053=CARTESIAN_POINT('Ctrl Pts',(-8.54098868169338,9.44423911521611,
10.8853522689456));
#113054=CARTESIAN_POINT('Ctrl Pts',(-8.54139600815837,9.44452070550036,
10.8802814859852));
#113055=CARTESIAN_POINT('Ctrl Pts',(-8.54297716284364,9.44555212077781,
10.8618052597239));
#113056=CARTESIAN_POINT('Ctrl Pts',(-8.54430939767145,9.44631000629406,
10.8484144521639));
#113057=CARTESIAN_POINT('Ctrl Pts',(-8.54811723558188,9.44823272578966,
10.8148462717941));
#113058=CARTESIAN_POINT('Ctrl Pts',(-8.55082890820206,9.44940751090486,
10.7946989051811));
#113059=CARTESIAN_POINT('Ctrl Pts',(-8.57495946714656,9.45856346935995,
10.6398800551122));
#113060=CARTESIAN_POINT('Ctrl Pts',(-8.61468658402728,9.46699182855886,
10.5087347512731));
#113061=CARTESIAN_POINT('Ctrl Pts',(-8.69019306789367,9.47739765970247,
10.345697823823));
#113062=CARTESIAN_POINT('Ctrl Pts',(-8.71011628315959,9.47985374951358,
10.3072474643031));
#113063=CARTESIAN_POINT('Ctrl Pts',(-8.73751678925365,9.48289522273003,
10.2596598589567));
#113064=CARTESIAN_POINT('Ctrl Pts',(-8.74343724761085,9.48353482422218,
10.2496551179159));
#113065=CARTESIAN_POINT('Ctrl Pts',(-8.75302621417252,9.48454361499292,
10.2338829591029));
#113066=CARTESIAN_POINT('Ctrl Pts',(-8.75661691528472,9.48491558250808,
10.2280690123213));
#113067=CARTESIAN_POINT('Ctrl Pts',(-8.7631394858567,9.48558105935513,10.2176714759101));
#113068=CARTESIAN_POINT('Ctrl Pts',(-8.76605642901196,9.48587510325263,
10.2130787105629));
#113069=CARTESIAN_POINT('Ctrl Pts',(-8.77294942199925,9.48656173445071,
10.2023581722921));
#113070=CARTESIAN_POINT('Ctrl Pts',(-8.77694589167756,9.48695356404656,
10.1962436581768));
#113071=CARTESIAN_POINT('Ctrl Pts',(-8.78864100191446,9.48808244242097,
10.1786396053198));
#113072=CARTESIAN_POINT('Ctrl Pts',(-8.79645705016204,9.48881513428449,
10.1672287797503));
#113073=CARTESIAN_POINT('Ctrl Pts',(-8.81447299691252,9.49045702066079,
10.1417104447309));
#113074=CARTESIAN_POINT('Ctrl Pts',(-8.82476527647107,9.49136272780874,
10.1276705828222));
#113075=CARTESIAN_POINT('Ctrl Pts',(-8.85926040377859,9.49429942271809,
10.0823342515621));
#113076=CARTESIAN_POINT('Ctrl Pts',(-8.88448260680557,9.49629387093512,
10.0518341470824));
#113077=CARTESIAN_POINT('Ctrl Pts',(-8.95441360035844,9.50149456009104,
9.97392859580813));
#113078=CARTESIAN_POINT('Ctrl Pts',(-9.00110352457218,9.50464286327012,
9.92842194881521));
#113079=CARTESIAN_POINT('Ctrl Pts',(-9.10812604573773,9.51149769172588,
9.83720482956861));
#113080=CARTESIAN_POINT('Ctrl Pts',(-9.16928038899626,9.51520348125991,
9.79275757381452));
#113081=CARTESIAN_POINT('Ctrl Pts',(-9.24381078696519,9.51980641726203,
9.74694202233806));
#113082=CARTESIAN_POINT('Ctrl Pts',(-9.25411645731182,9.52044477589274,
9.74078034331006));
#113083=CARTESIAN_POINT('Ctrl Pts',(-9.26839525790908,9.52133344313662,
9.73247994542628));
#113084=CARTESIAN_POINT('Ctrl Pts',(-9.27230447559931,9.52157716849879,
9.73023159194743));
#113085=CARTESIAN_POINT('Ctrl Pts',(-9.27901583539317,9.5219964355525,9.72641278174015));
#113086=CARTESIAN_POINT('Ctrl Pts',(-9.28181289518627,9.52217141916658,
9.72483340296241));
#113087=CARTESIAN_POINT('Ctrl Pts',(-9.28765047246164,9.52253717952849,
9.72156247444341));
#113088=CARTESIAN_POINT('Ctrl Pts',(-9.29069183704921,9.5227280606743,9.71987255116799));
#113089=CARTESIAN_POINT('Ctrl Pts',(-9.29810219848745,9.52319387554117,
9.71578952597999));
#113090=CARTESIAN_POINT('Ctrl Pts',(-9.30247742725874,9.52346951352522,
9.71340786400986));
#113091=CARTESIAN_POINT('Ctrl Pts',(-9.31809998108202,9.52445566578656,
9.70500681470163));
#113092=CARTESIAN_POINT('Ctrl Pts',(-9.32941343204,9.5251733661015,9.69911237297404));
#113093=CARTESIAN_POINT('Ctrl Pts',(-9.35769505325932,9.52697356322383,
9.6848442635865));
#113094=CARTESIAN_POINT('Ctrl Pts',(-9.37475102590782,9.52806455354686,
9.67665049341641));
#113095=CARTESIAN_POINT('Ctrl Pts',(-9.44822723652618,9.53277263575836,
9.64308970759946));
#113096=CARTESIAN_POINT('Ctrl Pts',(-9.50606437777582,9.53649611259197,
9.62098382475941));
#113097=CARTESIAN_POINT('Ctrl Pts',(-9.66955476782688,9.54680031869225,
9.57010477517453));
#113098=CARTESIAN_POINT('Ctrl Pts',(-9.77731701196726,9.55331885509914,
9.54940907622033));
#113099=CARTESIAN_POINT('Ctrl Pts',(-9.90451971688929,9.56047026406354,
9.53950475170611));
#113100=CARTESIAN_POINT('Ctrl Pts',(-9.92267265321241,9.5614791845174,9.53843119292253));
#113101=CARTESIAN_POINT('Ctrl Pts',(-9.94889081625855,9.5629200926222,9.53737051880413));
#113102=CARTESIAN_POINT('Ctrl Pts',(-9.95694281729685,9.56336041164563,
9.53711134033965));
#113103=CARTESIAN_POINT('Ctrl Pts',(-9.97111918697271,9.56413185226006,
9.53677217925446));
#113104=CARTESIAN_POINT('Ctrl Pts',(-9.97724263371884,9.56446383164643,
9.53666413266765));
#113105=CARTESIAN_POINT('Ctrl Pts',(-9.98989743207178,9.56514739856308,
9.53652029572315));
#113106=CARTESIAN_POINT('Ctrl Pts',(-9.99642871485747,9.56549881586043,
9.5364897832541));
#113107=CARTESIAN_POINT('Ctrl Pts',(-10.0132051061119,9.56639803826055,
9.53652371503839));
#113108=CARTESIAN_POINT('Ctrl Pts',(-10.0234498226951,9.5669438671373,9.53665201527382));
#113109=CARTESIAN_POINT('Ctrl Pts',(-10.0670375144166,9.56925297804632,
9.53765575202187));
#113110=CARTESIAN_POINT('Ctrl Pts',(-10.1003479287124,9.57098445121748,
9.53956333932139));
#113111=CARTESIAN_POINT('Ctrl Pts',(-10.1903777585356,9.57559922970326,
9.54781431494368));
#113112=CARTESIAN_POINT('Ctrl Pts',(-10.2468391260356,9.57842135079891,
9.55633867188869));
#113113=CARTESIAN_POINT('Ctrl Pts',(-10.3722729210377,9.58469100852929,
9.5828523652751));
#113114=CARTESIAN_POINT('Ctrl Pts',(-10.4407164520063,9.58811121128971,
9.6026228326214));
#113115=CARTESIAN_POINT('Ctrl Pts',(-10.5533534782184,9.59407825330123,
9.64426129612588));
#113116=CARTESIAN_POINT('Ctrl Pts',(-10.5983744617336,9.59656224368481,
9.66352155691888));
#113117=CARTESIAN_POINT('Ctrl Pts',(-10.6488093458091,9.59954971718296,
9.68815759582505));
#113118=CARTESIAN_POINT('Ctrl Pts',(-10.6552534176226,9.59993539176993,
9.6913644452502));
#113119=CARTESIAN_POINT('Ctrl Pts',(-10.6655516101131,9.60055852464694,
9.69658440675131));
#113120=CARTESIAN_POINT('Ctrl Pts',(-10.6694209489156,9.60079420496739,
9.69856742525034));
#113121=CARTESIAN_POINT('Ctrl Pts',(-10.6762939100976,9.60121570209106,
9.70212854674182));
#113122=CARTESIAN_POINT('Ctrl Pts',(-10.6793009511628,9.60140110108965,
9.70369988831467));
#113123=CARTESIAN_POINT('Ctrl Pts',(-10.6823205747863,9.60158828401621,
9.70529119735832));
#113124=CARTESIAN_POINT('Ctrl Pts',(-10.682338588012,9.60158940067085,9.7053006906141));
#113125=CARTESIAN_POINT('Ctrl Pts',(-10.6823743791361,9.60159161946332,
9.70531955405881));
#113126=CARTESIAN_POINT('Ctrl Pts',(-10.6823921570856,9.60159272160339,
9.70532892426227));
#113127=CARTESIAN_POINT('Ctrl Pts',(-10.6824274812581,9.60159491158719,
9.70534754346307));
#113128=CARTESIAN_POINT('Ctrl Pts',(-10.6824450274407,9.60159599942749,
9.70535679242699));
#113129=CARTESIAN_POINT('Ctrl Pts',(-10.6824798915461,9.60159816102398,
9.70537517094006));
#113130=CARTESIAN_POINT('Ctrl Pts',(-10.682497209407,9.60159923477544,9.70538430044477));
#113131=CARTESIAN_POINT('Ctrl Pts',(-10.6825316202207,9.6016013683994,9.70540244177105));
#113132=CARTESIAN_POINT('Ctrl Pts',(-10.682548713134,9.6016024282686,9.70541145356042));
#113133=CARTESIAN_POINT('Ctrl Pts',(-10.682582677389,9.60160453433238,9.70542936118101));
#113134=CARTESIAN_POINT('Ctrl Pts',(-10.6825995487072,9.60160558052466,
9.7054382569887));
#113135=CARTESIAN_POINT('Ctrl Pts',(-10.6826330728645,9.60160765942387,
9.70545593424326));
#113136=CARTESIAN_POINT('Ctrl Pts',(-10.6826497257856,9.60160869213508,
9.70546471572255));
#113137=CARTESIAN_POINT('Ctrl Pts',(-10.682682816523,9.60161074427897,9.70548216606737));
#113138=CARTESIAN_POINT('Ctrl Pts',(-10.6826992543128,9.60161176370923,
9.70549083490844));
#113139=CARTESIAN_POINT('Ctrl Pts',(-10.6827319179129,9.60161378948269,
9.70550806159347));
#113140=CARTESIAN_POINT('Ctrl Pts',(-10.6827481437337,9.60161479582579,
9.70551661943282));
#113141=CARTESIAN_POINT('Ctrl Pts',(-10.6827803864486,9.60161679561196,
9.70553362569396));
#113142=CARTESIAN_POINT('Ctrl Pts',(-10.68279640338,9.60161778905661,9.70554207412551));
#113143=CARTESIAN_POINT('Ctrl Pts',(-10.6828282314985,9.60161976324108,
9.70555886322003));
#113144=CARTESIAN_POINT('Ctrl Pts',(-10.6828440426436,9.60162074397757,
9.70556720385115));
#113145=CARTESIAN_POINT('Ctrl Pts',(-10.6828754621327,9.60162269292609,
9.70558377886846));
#113146=CARTESIAN_POINT('Ctrl Pts',(-10.6828910704704,9.60162366113703,
9.70559201324188));
#113147=CARTESIAN_POINT('Ctrl Pts',(-10.6829220875001,9.60162558522809,
9.70560837738032));
#113148=CARTESIAN_POINT('Ctrl Pts',(-10.6829374961114,9.60162654110252,
9.7056165070936));
#113149=CARTESIAN_POINT('Ctrl Pts',(-10.6829681161778,9.60162844067294,
9.70563266319781));
#113150=CARTESIAN_POINT('Ctrl Pts',(-10.6829833278201,9.60162938437988,
9.70564068967862));
#113151=CARTESIAN_POINT('Ctrl Pts',(-10.6830135570897,9.60163125980822,
9.70565664094877));
#113152=CARTESIAN_POINT('Ctrl Pts',(-10.6830285746875,9.60163219152713,
9.70566456571385));
#113153=CARTESIAN_POINT('Ctrl Pts',(-10.6830584187838,9.60163404315836,
9.70568031506526));
#113154=CARTESIAN_POINT('Ctrl Pts',(-10.6830732451936,9.60163496306454,
9.70568813959627));
#113155=CARTESIAN_POINT('Ctrl Pts',(-10.68310270972,9.60163679124254,9.7057036899353));
#113156=CARTESIAN_POINT('Ctrl Pts',(-10.6831173477817,9.60163769951032,
9.70571141570603));
#113157=CARTESIAN_POINT('Ctrl Pts',(-10.683146437956,9.60163950455514,9.70572676973713));
#113158=CARTESIAN_POINT('Ctrl Pts',(-10.6831608902278,9.60164040134144,
9.70573439807348));
#113159=CARTESIAN_POINT('Ctrl Pts',(-10.6831896120403,9.60164218362119,
9.70574955891043));
#113160=CARTESIAN_POINT('Ctrl Pts',(-10.6832038814252,9.60164306910437,
9.70575709132099));
#113161=CARTESIAN_POINT('Ctrl Pts',(-10.6832322396096,9.6016448289093,9.70577206141581));
#113162=CARTESIAN_POINT('Ctrl Pts',(-10.683246328575,9.60164570324076,9.70577949918005));
#113163=CARTESIAN_POINT('Ctrl Pts',(-10.6832743288134,9.60164744092008,
9.7057942814869));
#113164=CARTESIAN_POINT('Ctrl Pts',(-10.683288240036,9.60164830426425,9.70580162599546));
#113165=CARTESIAN_POINT('Ctrl Pts',(-10.6833158874056,9.60165002012975,
9.70581622315054));
#113166=CARTESIAN_POINT('Ctrl Pts',(-10.6833296235036,9.60165087264749,
9.70582347576395));
#113167=CARTESIAN_POINT('Ctrl Pts',(-10.6833569228363,9.60165256699583,
9.70583789027534));
#113168=CARTESIAN_POINT('Ctrl Pts',(-10.6833704861922,9.60165340883343,
9.70584505223036));
#113169=CARTESIAN_POINT('Ctrl Pts',(-10.6833974428782,9.60165508199603,
9.70585928690236));
#113170=CARTESIAN_POINT('Ctrl Pts',(-10.6834108360869,9.60165591331299,
9.70586635954843));
#113171=CARTESIAN_POINT('Ctrl Pts',(-10.6834374548406,9.60165756557941,
9.70588041682977));
#113172=CARTESIAN_POINT('Ctrl Pts',(-10.6834506803668,9.60165838652722,
9.70588740144846));
#113173=CARTESIAN_POINT('Ctrl Pts',(-10.68347696589,9.60166001818636,9.70590128378244));
#113174=CARTESIAN_POINT('Ctrl Pts',(-10.6834900260471,9.60166082890715,
9.70590818157588));
#113175=CARTESIAN_POINT('Ctrl Pts',(-10.6835159832055,9.60166244025814,
9.70592189149365));
#113176=CARTESIAN_POINT('Ctrl Pts',(-10.6835288802863,9.60166324089282,
9.70592870365374));
#113177=CARTESIAN_POINT('Ctrl Pts',(-10.6835545141058,9.60166483224487,
9.70594224377232));
#113178=CARTESIAN_POINT('Ctrl Pts',(-10.6835672506391,9.60166562294903,
9.70594897161618));
#113179=CARTESIAN_POINT('Ctrl Pts',(-10.6835925651352,9.60166719454868,
9.70596234401999));
#113180=CARTESIAN_POINT('Ctrl Pts',(-10.6836051432246,9.60166797545158,
9.70596898864081));
#113181=CARTESIAN_POINT('Ctrl Pts',(-10.6836301434222,9.60166952760812,
9.70598219594861));
#113182=CARTESIAN_POINT('Ctrl Pts',(-10.6836425654444,9.601670298856,9.70598875858437));
#113183=CARTESIAN_POINT('Ctrl Pts',(-10.6836672554069,9.60167183181913,
9.70600180290815));
#113184=CARTESIAN_POINT('Ctrl Pts',(-10.6836795234334,9.60167259353931,
9.70600828463608));
#113185=CARTESIAN_POINT('Ctrl Pts',(-10.6837039079859,9.60167410760609,
9.7060211684913));
#113186=CARTESIAN_POINT('Ctrl Pts',(-10.6837160243483,9.60167485994211,
9.70602757052664));
#113187=CARTESIAN_POINT('Ctrl Pts',(-10.6837401074538,9.60167635535615,
9.7060402959743));
#113188=CARTESIAN_POINT('Ctrl Pts',(-10.6837520742491,9.60167709843701,
9.70604661940887));
#113189=CARTESIAN_POINT('Ctrl Pts',(-10.6837758601558,9.6016785754597,9.70605918866168));
#113190=CARTESIAN_POINT('Ctrl Pts',(-10.6837876794018,9.60167930940951,
9.70606543454586));
#113191=CARTESIAN_POINT('Ctrl Pts',(-10.6838111725248,9.6016807683127,9.70607784990575));
#113192=CARTESIAN_POINT('Ctrl Pts',(-10.6838228463518,9.60168149326259,
9.70608401934992));
#113193=CARTESIAN_POINT('Ctrl Pts',(-10.6838460506931,9.60168293429252,
9.70609628290143));
#113194=CARTESIAN_POINT('Ctrl Pts',(-10.6838575811444,9.60168365036827,
9.7061023769705));
#113195=CARTESIAN_POINT('Ctrl Pts',(-10.6838805007578,9.60168507377448,
9.70611449082648));
#113196=CARTESIAN_POINT('Ctrl Pts',(-10.6838918898546,9.60168578110053,
9.70612051057408));
#113197=CARTESIAN_POINT('Ctrl Pts',(-10.6839145287203,9.60168718712807,
9.70613247680945));
#113198=CARTESIAN_POINT('Ctrl Pts',(-10.6839257784642,9.60168788582765,
9.70613842327933));
#113199=CARTESIAN_POINT('Ctrl Pts',(-10.6839481403683,9.60168927470957,
9.70615024386725));
#113200=CARTESIAN_POINT('Ctrl Pts',(-10.6839592526239,9.60168996489747,
9.70615611803117));
#113201=CARTESIAN_POINT('Ctrl Pts',(-10.6839813416535,9.60169133688556,
9.70616779510476));
#113202=CARTESIAN_POINT('Ctrl Pts',(-10.6839923184077,9.60169201868418,
9.70617359799954));
#113203=CARTESIAN_POINT('Ctrl Pts',(-10.6840141381392,9.60169337399861,
9.70618513342284));
#113204=CARTESIAN_POINT('Ctrl Pts',(-10.6840249812056,9.60169404751961,
9.70619086599411));
#113205=CARTESIAN_POINT('Ctrl Pts',(-10.684046535537,9.60169538640055,9.70620226180188));
#113206=CARTESIAN_POINT('Ctrl Pts',(-10.6840572467956,9.60169605175976,
9.70620792503078));
#113207=CARTESIAN_POINT('Ctrl Pts',(-10.6876846865737,9.60192138442477,
9.70812587323267));
#113208=CARTESIAN_POINT('Ctrl Pts',(-10.6912933359568,9.60214699436492,
9.7100532916476));
#113209=CARTESIAN_POINT('Ctrl Pts',(-10.7019458556196,9.60281715643344,
9.71580045453595));
#113210=CARTESIAN_POINT('Ctrl Pts',(-10.7089663747763,9.60326425049677,
9.71966288409624));
#113211=CARTESIAN_POINT('Ctrl Pts',(-10.7250712541704,9.60430180392394,
9.72869626468675));
#113212=CARTESIAN_POINT('Ctrl Pts',(-10.7341325621673,9.60489442810374,
9.73390723858346));
#113213=CARTESIAN_POINT('Ctrl Pts',(-10.7642988113322,9.60689520666466,
9.75168794748396));
#113214=CARTESIAN_POINT('Ctrl Pts',(-10.7851422150384,9.60832381613623,
9.76469143997631));
#113215=CARTESIAN_POINT('Ctrl Pts',(-10.8500329308914,9.61289692380356,
9.80748042237717));
#113216=CARTESIAN_POINT('Ctrl Pts',(-10.8927890585302,9.61609758061416,
9.83914417751405));
#113217=CARTESIAN_POINT('Ctrl Pts',(-11.0175058511338,9.62584439482827,
9.94247850071633));
#113218=CARTESIAN_POINT('Ctrl Pts',(-11.0932968305378,9.63232684168418,
10.0210315914217));
#113219=CARTESIAN_POINT('Ctrl Pts',(-11.1707943135816,9.63944823031381,
10.1217035790922));
#113220=CARTESIAN_POINT('Ctrl Pts',(-11.18163353811,9.64045881947979,10.1363414151755));
#113221=CARTESIAN_POINT('Ctrl Pts',(-11.1968724706293,9.64190165442275,
10.1577449789388));
#113222=CARTESIAN_POINT('Ctrl Pts',(-11.2014935956771,9.64234226250431,
10.164350327813));
#113223=CARTESIAN_POINT('Ctrl Pts',(-11.2095295857406,9.64311403958962,
10.1760412944275));
#113224=CARTESIAN_POINT('Ctrl Pts',(-11.212967509226,9.64344606869018,10.181110758155));
#113225=CARTESIAN_POINT('Ctrl Pts',(-11.2200041662266,9.64412957746605,
10.1916283563145));
#113226=CARTESIAN_POINT('Ctrl Pts',(-11.2235984741443,9.64448088808905,
10.1970792966405));
#113227=CARTESIAN_POINT('Ctrl Pts',(-11.2327335125077,9.64537950511583,
10.211136827257));
#113228=CARTESIAN_POINT('Ctrl Pts',(-11.2382206989335,9.64592484054412,
10.2197778995714));
#113229=CARTESIAN_POINT('Ctrl Pts',(-11.2611537838395,9.64822883442018,
10.2567436589376));
#113230=CARTESIAN_POINT('Ctrl Pts',(-11.2777225527412,9.64995586451404,
10.2856022464121));
#113231=CARTESIAN_POINT('Ctrl Pts',(-11.3198893303148,9.65455493175708,
10.3652142298304));
#113232=CARTESIAN_POINT('Ctrl Pts',(-11.3435388003032,9.65736634004851,
10.4169348788187));
#113233=CARTESIAN_POINT('Ctrl Pts',(-11.3921468751536,9.6639299332138,10.5420199676267));
#113234=CARTESIAN_POINT('Ctrl Pts',(-11.414407470614,9.66764188557768,10.616243322208));
#113235=CARTESIAN_POINT('Ctrl Pts',(-11.4364117936173,9.67286491853837,
10.7184144295653));
#113236=CARTESIAN_POINT('Ctrl Pts',(-11.4413877359852,9.67424030752079,
10.7451068204224));
#113237=CARTESIAN_POINT('Ctrl Pts',(-11.4486330472466,9.67664764207889,
10.7910292703301));
#113238=CARTESIAN_POINT('Ctrl Pts',(-11.4512685332935,9.67766447007054,
10.8101947175152));
#113239=CARTESIAN_POINT('Ctrl Pts',(-11.4542288615562,9.67902503192416,
10.8354177730152));
#113240=CARTESIAN_POINT('Ctrl Pts',(-11.4548971399276,9.67935121356271,
10.8414339226088));
#113241=CARTESIAN_POINT('Ctrl Pts',(-11.4559146112561,9.67988049819796,
10.851142190841));
#113242=CARTESIAN_POINT('Ctrl Pts',(-11.4562871324289,9.68008233526669,
10.8548318564051));
#113243=CARTESIAN_POINT('Ctrl Pts',(-11.4569580544429,9.68046155306436,
10.8617396549847));
#113244=CARTESIAN_POINT('Ctrl Pts',(-11.4572598236306,9.68063874615317,
10.8649574100434));
#113245=CARTESIAN_POINT('Ctrl Pts',(-11.4578576466569,9.68100383610441,
10.871567421347));
#113246=CARTESIAN_POINT('Ctrl Pts',(-11.4581525251255,9.68119179577398,
10.8749597737987));
#113247=CARTESIAN_POINT('Ctrl Pts',(-11.4588160875583,9.68163391969058,
10.8829152824278));
#113248=CARTESIAN_POINT('Ctrl Pts',(-11.4591752024302,9.68188858426316,
10.8874791756721));
#113249=CARTESIAN_POINT('Ctrl Pts',(-11.4604393785231,9.68284592504264,
10.9045703226372));
#113250=CARTESIAN_POINT('Ctrl Pts',(-11.4612045497126,9.68355550289127,
10.9171070285735));
#113251=CARTESIAN_POINT('Ctrl Pts',(-11.4629244220802,9.68559627130138,
10.9528452079629));
#113252=CARTESIAN_POINT('Ctrl Pts',(-11.4634883795329,9.68694349692706,
10.976060848177));
#113253=CARTESIAN_POINT('Ctrl Pts',(-11.4634998222634,9.68830623016798,
10.9992787267827));
#113254=CARTESIAN_POINT('Origin',(-10.,3.5,11.));
#113255=CARTESIAN_POINT('',(-11.4634998963973,10.2594509413108,10.9994493226066));
#113256=CARTESIAN_POINT('',(-11.4634998672782,10.1905769185068,10.9993767206508));
#113257=CARTESIAN_POINT('',(-11.4635,3.5,11.));
#113258=CARTESIAN_POINT('Ctrl Pts',(-11.4634998963974,10.2594509413502,
10.9994493233677));
#113259=CARTESIAN_POINT('Ctrl Pts',(-11.4634862943792,10.2575830488448,
10.9633000642476));
#113260=CARTESIAN_POINT('Ctrl Pts',(-11.462133348461,10.255752951935,10.927162368284));
#113261=CARTESIAN_POINT('Ctrl Pts',(-11.4542405240509,10.2504599843605,
10.8213753825262));
#113262=CARTESIAN_POINT('Ctrl Pts',(-11.4440460393546,10.2470799500598,
10.752101545193));
#113263=CARTESIAN_POINT('Ctrl Pts',(-11.4124588144446,10.2399541673378,
10.6093459547505));
#113264=CARTESIAN_POINT('Ctrl Pts',(-11.3901840202895,10.2362127256549,
10.5362798243507));
#113265=CARTESIAN_POINT('Ctrl Pts',(-11.3579340662727,10.2315686396017,
10.454114030765));
#113266=CARTESIAN_POINT('Ctrl Pts',(-11.3534098793377,10.2309302831277,
10.4429918312827));
#113267=CARTESIAN_POINT('Ctrl Pts',(-11.3469993328789,10.2300416617662,
10.427771569031));
#113268=CARTESIAN_POINT('Ctrl Pts',(-11.3452299929797,10.2297979805115,
10.4236243890496));
#113269=CARTESIAN_POINT('Ctrl Pts',(-11.3421677002724,10.2293788004034,
10.4165375526681));
#113270=CARTESIAN_POINT('Ctrl Pts',(-11.3408841728556,10.2292038594952,
10.4135938287509));
#113271=CARTESIAN_POINT('Ctrl Pts',(-11.3381902921116,10.2288382031425,
10.4074705994657));
#113272=CARTESIAN_POINT('Ctrl Pts',(-11.3367782861009,10.2286473834548,
10.4042918824162));
#113273=CARTESIAN_POINT('Ctrl Pts',(-11.3333173556612,10.2281817472528,
10.3965748816269));
#113274=CARTESIAN_POINT('Ctrl Pts',(-11.3312565827084,10.2279062271955,
10.3920419801395));
#113275=CARTESIAN_POINT('Ctrl Pts',(-11.3238374368099,10.2269206578529,
10.3759413359653));
#113276=CARTESIAN_POINT('Ctrl Pts',(-11.3183512448256,10.2262034320483,
10.3644335219093));
#113277=CARTESIAN_POINT('Ctrl Pts',(-11.3043574104275,10.2244045891495,
10.3360410895325));
#113278=CARTESIAN_POINT('Ctrl Pts',(-11.2956717191823,10.2233144924664,
10.3192471625397));
#113279=CARTESIAN_POINT('Ctrl Pts',(-11.2572250079121,10.2186120366431,
10.2483124170297));
#113280=CARTESIAN_POINT('Ctrl Pts',(-11.2243781907875,10.2148935063949,
10.1959189869045));
#113281=CARTESIAN_POINT('Ctrl Pts',(-11.1244119287705,10.2045868898192,
10.0568572490605));
#113282=CARTESIAN_POINT('Ctrl Pts',(-11.0507174687013,10.1980608497323,
9.97539246817712));
#113283=CARTESIAN_POINT('Ctrl Pts',(-10.9549894127951,10.190903302578,9.89087521219069));
#113284=CARTESIAN_POINT('Ctrl Pts',(-10.9411415869911,10.189894821308,9.87910075015727));
#113285=CARTESIAN_POINT('Ctrl Pts',(-10.9208462259254,10.1884544941744,
9.86248545826009));
#113286=CARTESIAN_POINT('Ctrl Pts',(-10.9145727904991,10.1880143243531,
9.85743546398245));
#113287=CARTESIAN_POINT('Ctrl Pts',(-10.9034571294003,10.1872431300614,
9.84863778500781));
#113288=CARTESIAN_POINT('Ctrl Pts',(-10.898632511624,10.1869112484666,9.84486825625668));
#113289=CARTESIAN_POINT('Ctrl Pts',(-10.8886139335851,10.1862278699084,
9.8371413836111));
#113290=CARTESIAN_POINT('Ctrl Pts',(-10.883416852644,10.1858765431702,9.83318829667214));
#113291=CARTESIAN_POINT('Ctrl Pts',(-10.8699996346552,10.1849775282995,
9.82312371004521));
#113292=CARTESIAN_POINT('Ctrl Pts',(-10.8617414038642,10.1844318156519,
9.81706343106077));
#113293=CARTESIAN_POINT('Ctrl Pts',(-10.8263276494325,10.1821230309942,
9.79164282259333));
#113294=CARTESIAN_POINT('Ctrl Pts',(-10.7985772390656,10.180391760713,9.77312630466797));
#113295=CARTESIAN_POINT('Ctrl Pts',(-10.7217121316134,10.1757774778639,
9.72555194852045));
#113296=CARTESIAN_POINT('Ctrl Pts',(-10.671491497365,10.1729556392773,9.69839098215427));
#113297=CARTESIAN_POINT('Ctrl Pts',(-10.6046300439122,10.1693461943471,
9.66713256544891));
#113298=CARTESIAN_POINT('Ctrl Pts',(-10.5893280728218,10.1685294806238,
9.66029648186219));
#113299=CARTESIAN_POINT('Ctrl Pts',(-10.4837723358048,10.1629431597651,
9.61529847656086));
#113300=CARTESIAN_POINT('Ctrl Pts',(-10.3900122293105,10.1582301446143,
9.58602696272213));
#113301=CARTESIAN_POINT('Ctrl Pts',(-10.2829623046903,10.1524710192988,
9.56407082770563));
#113302=CARTESIAN_POINT('Ctrl Pts',(-10.2718534910464,10.151868810434,9.56192631699846));
#113303=CARTESIAN_POINT('Ctrl Pts',(-10.2563800130152,10.1510222810881,
9.55912491756782));
#113304=CARTESIAN_POINT('Ctrl Pts',(-10.2520352808938,10.1507837456512,
9.55835859853328));
#113305=CARTESIAN_POINT('Ctrl Pts',(-10.244547337332,10.1503710908606,9.55707276715072));
#113306=CARTESIAN_POINT('Ctrl Pts',(-10.2414057464927,10.1501974912041,
9.55654384733852));
#113307=CARTESIAN_POINT('Ctrl Pts',(-10.2348080594086,10.1498318824792,
9.55545519862289));
#113308=CARTESIAN_POINT('Ctrl Pts',(-10.231351658652,10.1496397511864,9.55489761013364));
#113309=CARTESIAN_POINT('Ctrl Pts',(-10.2228587572847,10.1491662472596,
9.55355878057596));
#113310=CARTESIAN_POINT('Ctrl Pts',(-10.2178201357117,10.1488841155311,
9.55279144079065));
#113311=CARTESIAN_POINT('Ctrl Pts',(-10.1993938024115,10.1478481798891,
9.55008367203305));
#113312=CARTESIAN_POINT('Ctrl Pts',(-10.1859837709318,10.1470862237061,
9.54830262902944));
#113313=CARTESIAN_POINT('Ctrl Pts',(-10.1522205497791,10.1451508804495,
9.54429387307351));
#113314=CARTESIAN_POINT('Ctrl Pts',(-10.1318420632849,10.1439673835021,
9.54230695244723));
#113315=CARTESIAN_POINT('Ctrl Pts',(-9.97255185211468,10.1346298881146,
9.53014343409202));
#113316=CARTESIAN_POINT('Ctrl Pts',(-9.83286472504538,10.1260166633179,
9.53941567275816));
#113317=CARTESIAN_POINT('Ctrl Pts',(-9.65686146692039,10.1156266212034,
9.57671633511999));
#113318=CARTESIAN_POINT('Ctrl Pts',(-9.6175107082053,10.1133274195974,9.58678280707845));
#113319=CARTESIAN_POINT('Ctrl Pts',(-9.56773157055176,10.1104498628845,
9.60174906156194));
#113320=CARTESIAN_POINT('Ctrl Pts',(-9.55687487753494,10.1098241412488,
9.60515168638234));
#113321=CARTESIAN_POINT('Ctrl Pts',(-9.53961524541052,10.108832173874,9.61078293053293));
#113322=CARTESIAN_POINT('Ctrl Pts',(-9.53318635401791,10.1084633052205,
9.6129299907974));
#113323=CARTESIAN_POINT('Ctrl Pts',(-9.52161827207353,10.1078006232038,
9.61688292583138));
#113324=CARTESIAN_POINT('Ctrl Pts',(-9.51647383609122,10.1075063012531,
9.61867296834161));
#113325=CARTESIAN_POINT('Ctrl Pts',(-9.50438429093902,10.1068154796893,
9.62295542436544));
#113326=CARTESIAN_POINT('Ctrl Pts',(-9.49744776455892,10.1064197700455,
9.62547173630032));
#113327=CARTESIAN_POINT('Ctrl Pts',(-9.47722316546002,10.1052677542921,
9.63298202820936));
#113328=CARTESIAN_POINT('Ctrl Pts',(-9.46398816403667,10.1045160927794,
9.63811708132038));
#113329=CARTESIAN_POINT('Ctrl Pts',(-9.36378414404764,10.0988379025878,
9.67868236315272));
#113330=CARTESIAN_POINT('Ctrl Pts',(-9.28032948398277,10.094201951275,9.72221758349777));
#113331=CARTESIAN_POINT('Ctrl Pts',(-9.11364814108016,10.0845087558652,
9.83071417379565));
#113332=CARTESIAN_POINT('Ctrl Pts',(-9.03210816717216,10.0794904899148,
9.89726308525945));
#113333=CARTESIAN_POINT('Ctrl Pts',(-8.95085077461707,10.0733851975957,
9.97959148694501));
#113334=CARTESIAN_POINT('Ctrl Pts',(-8.94338986138299,10.0728128427596,
9.98731908660913));
#113335=CARTESIAN_POINT('Ctrl Pts',(-8.93305208019201,10.07200191329,9.99826500199554));
#113336=CARTESIAN_POINT('Ctrl Pts',(-8.93010318396578,10.0717685095511,
10.0014151653953));
#113337=CARTESIAN_POINT('Ctrl Pts',(-8.92501816567224,10.0713623123091,
10.0068956253172));
#113338=CARTESIAN_POINT('Ctrl Pts',(-8.92287556638294,10.0711900009472,
10.0092199046892));
#113339=CARTESIAN_POINT('Ctrl Pts',(-8.91835774106767,10.0708241653642,
10.0141527906046));
#113340=CARTESIAN_POINT('Ctrl Pts',(-8.91598439574228,10.0706304999293,
10.0167630674057));
#113341=CARTESIAN_POINT('Ctrl Pts',(-8.91011713487109,10.0701480970889,
10.0232631222595));
#113342=CARTESIAN_POINT('Ctrl Pts',(-8.9066346044091,10.0698585374223,10.0271630670737));
#113343=CARTESIAN_POINT('Ctrl Pts',(-8.89360817409079,10.0687635040853,
10.0419091366168));
#113344=CARTESIAN_POINT('Ctrl Pts',(-8.8842044636374,10.0679486503046,10.0528773765514));
#113345=CARTESIAN_POINT('Ctrl Pts',(-8.8154564322845,10.0618188517994,10.1355082531234));
#113346=CARTESIAN_POINT('Ctrl Pts',(-8.76290817778324,10.0561683490377,
10.2125412660766));
#113347=CARTESIAN_POINT('Ctrl Pts',(-8.67258339270342,10.0449193983551,
10.3765629510643));
#113348=CARTESIAN_POINT('Ctrl Pts',(-8.63520563135311,10.0393527951374,
10.4632973500904));
#113349=CARTESIAN_POINT('Ctrl Pts',(-8.60073450430408,10.0330218748626,
10.5707735292916));
#113350=CARTESIAN_POINT('Ctrl Pts',(-8.59538408780555,10.031987675413,10.5886200362395));
#113351=CARTESIAN_POINT('Ctrl Pts',(-8.58838619787018,10.0305578976472,
10.6136924917161));
#113352=CARTESIAN_POINT('Ctrl Pts',(-8.58645077902293,10.0301531512991,
10.6208356293082));
#113353=CARTESIAN_POINT('Ctrl Pts',(-8.58300330503894,10.0294145787647,
10.633952754895));
#113354=CARTESIAN_POINT('Ctrl Pts',(-8.58147464678666,10.0290802291361,
10.6399221708042));
#113355=CARTESIAN_POINT('Ctrl Pts',(-8.57844995758247,10.0284043537728,
10.6520518561747));
#113356=CARTESIAN_POINT('Ctrl Pts',(-8.57695615861035,10.0280629052112,
10.6582125498181));
#113357=CARTESIAN_POINT('Ctrl Pts',(-8.57335856940373,10.0272210336467,
10.6734822006574));
#113358=CARTESIAN_POINT('Ctrl Pts',(-8.57130192460902,10.0267221107228,
10.6826020485465));
#113359=CARTESIAN_POINT('Ctrl Pts',(-8.56387157716686,10.0248496232155,
10.7170872014899));
#113360=CARTESIAN_POINT('Ctrl Pts',(-8.55908470370161,10.0234944839752,
10.7425748377645));
#113361=CARTESIAN_POINT('Ctrl Pts',(-8.54869891533128,10.020114708801,10.8073126652342));
#113362=CARTESIAN_POINT('Ctrl Pts',(-8.54401265956118,10.0181166172646,
10.8466885520205));
#113363=CARTESIAN_POINT('Ctrl Pts',(-8.53587294428252,10.0129164816629,
10.9510580080868));
#113364=CARTESIAN_POINT('Ctrl Pts',(-8.53514438064214,10.0097719489477,
11.0161743293147));
#113365=CARTESIAN_POINT('Ctrl Pts',(-8.54293164515807,10.0029236483346,
11.1564443509342));
#113366=CARTESIAN_POINT('Ctrl Pts',(-8.55293028183017,9.99922055924571,
11.2313219634186));
#113367=CARTESIAN_POINT('Ctrl Pts',(-8.57115868811284,9.99462010144775,
11.3168426215016));
#113368=CARTESIAN_POINT('Ctrl Pts',(-8.57380918105517,9.99398104737646,
11.3285673005787));
#113369=CARTESIAN_POINT('Ctrl Pts',(-8.57765241213885,9.99309161963148,
11.3446446504495));
#113370=CARTESIAN_POINT('Ctrl Pts',(-8.57872137691247,9.99284784554781,
11.3490267471933));
#113371=CARTESIAN_POINT('Ctrl Pts',(-8.58058616533332,9.99242854739396,
11.3565205913516));
#113372=CARTESIAN_POINT('Ctrl Pts',(-8.58137201327883,9.99225358196518,
11.3596348161468));
#113373=CARTESIAN_POINT('Ctrl Pts',(-8.58303013768096,9.99188792258592,
11.3661157672652));
#113374=CARTESIAN_POINT('Ctrl Pts',(-8.5839041677126,9.99169712470755,11.3694819869559));
#113375=CARTESIAN_POINT('Ctrl Pts',(-8.58605822908163,9.99123162189138,
11.3776581694534));
#113376=CARTESIAN_POINT('Ctrl Pts',(-8.58735081158651,9.990956214351,11.3824647611288));
#113377=CARTESIAN_POINT('Ctrl Pts',(-8.59203790097204,9.98997148480037,
11.3995462087035));
#113378=CARTESIAN_POINT('Ctrl Pts',(-8.59556798989298,9.98925500199196,
11.4117828939991));
#113379=CARTESIAN_POINT('Ctrl Pts',(-8.60472678743104,9.98745840314594,
11.4420422845281));
#113380=CARTESIAN_POINT('Ctrl Pts',(-8.6105453388387,9.98636983308172,11.4600047874608));
#113381=CARTESIAN_POINT('Ctrl Pts',(-8.63683323579494,9.98167765091917,
11.5361037314702));
#113382=CARTESIAN_POINT('Ctrl Pts',(-8.66061589532994,9.97796828124458,
11.5930264293615));
#113383=CARTESIAN_POINT('Ctrl Pts',(-8.73650629985609,9.96765803100651,
11.7466253520187));
#113384=CARTESIAN_POINT('Ctrl Pts',(-8.79600954596482,9.96111891418536,
11.8392139967933));
#113385=CARTESIAN_POINT('Ctrl Pts',(-8.87678302920461,9.95395052159352,
11.9383740233353));
#113386=CARTESIAN_POINT('Ctrl Pts',(-8.88851607342498,9.95294266699089,
11.9522424552714));
#113387=CARTESIAN_POINT('Ctrl Pts',(-8.90581836444586,9.95150306357661,
11.9719380749385));
#113388=CARTESIAN_POINT('Ctrl Pts',(-8.91118199119699,9.95106300240495,
11.9779429535603));
#113389=CARTESIAN_POINT('Ctrl Pts',(-8.92071087035814,9.95029193455262,
11.9884354837182));
#113390=CARTESIAN_POINT('Ctrl Pts',(-8.92485520611861,9.94996007161204,
11.9929417931585));
#113391=CARTESIAN_POINT('Ctrl Pts',(-8.93347834672682,9.94927667103424,
12.0022008071594));
#113392=CARTESIAN_POINT('Ctrl Pts',(-8.93796093584425,9.94892530406674,
12.0069498114931));
#113393=CARTESIAN_POINT('Ctrl Pts',(-8.94955821806162,9.94802606094409,
12.0190727657173));
#113394=CARTESIAN_POINT('Ctrl Pts',(-8.9567189016098,9.94748016225432,12.0264023557685));
#113395=CARTESIAN_POINT('Ctrl Pts',(-8.98753419436374,9.94516944491471,
12.0572888286523));
#113396=CARTESIAN_POINT('Ctrl Pts',(-9.01191499026243,9.94343649631223,
12.0801087480284));
#113397=CARTESIAN_POINT('Ctrl Pts',(-9.08007794747757,9.93881627062336,
12.1396664304062));
#113398=CARTESIAN_POINT('Ctrl Pts',(-9.12526573037847,9.93599037839805,
12.1747070886251));
#113399=CARTESIAN_POINT('Ctrl Pts',(-9.17977839071617,9.9327582061639,12.2120845864152));
#113400=CARTESIAN_POINT('Ctrl Pts',(-9.18721459082728,9.93232084037367,
12.2170835685018));
#113401=CARTESIAN_POINT('Ctrl Pts',(-9.28010780959744,9.92689662383859,
12.2782999369494));
#113402=CARTESIAN_POINT('Ctrl Pts',(-9.37117488225281,9.92200733388753,
12.3254695675598));
#113403=CARTESIAN_POINT('Ctrl Pts',(-9.47923849118508,9.91592716793035,
12.3677827906596));
#113404=CARTESIAN_POINT('Ctrl Pts',(-9.49214568724392,9.91519641757728,
12.3726275100879));
#113405=CARTESIAN_POINT('Ctrl Pts',(-9.51010225466513,9.91417108554198,
12.3790795803178));
#113406=CARTESIAN_POINT('Ctrl Pts',(-9.51509518492441,9.91388506218078,
12.3808430788164));
#113407=CARTESIAN_POINT('Ctrl Pts',(-9.52311088004403,9.91342423775376,
12.3836253798561));
#113408=CARTESIAN_POINT('Ctrl Pts',(-9.52612764408092,9.91325043250034,
12.3846614800775));
#113409=CARTESIAN_POINT('Ctrl Pts',(-9.53245912566061,9.91288483316092,
12.3868128973142));
#113410=CARTESIAN_POINT('Ctrl Pts',(-9.53577447484118,9.91269291971138,
12.3879262020452));
#113411=CARTESIAN_POINT('Ctrl Pts',(-9.54391295698816,9.91222070352063,
12.3906267081038));
#113412=CARTESIAN_POINT('Ctrl Pts',(-9.54874039953616,9.91193965079142,
12.3922007051873));
#113413=CARTESIAN_POINT('Ctrl Pts',(-9.56633532318243,9.9109120742867,12.3978364370677));
#113414=CARTESIAN_POINT('Ctrl Pts',(-9.57914985334231,9.91015756467046,
12.401747796461));
#113415=CARTESIAN_POINT('Ctrl Pts',(-9.61142430397616,9.90824513808985,
12.4111164407753));
#113416=CARTESIAN_POINT('Ctrl Pts',(-9.63094661017167,9.90707739531486,
12.4163474876122));
#113417=CARTESIAN_POINT('Ctrl Pts',(-9.71818855211159,9.90182874953775,
12.4377980485015));
#113418=CARTESIAN_POINT('Ctrl Pts',(-9.78690466530693,9.89761902283037,
12.449576000437));
#113419=CARTESIAN_POINT('Ctrl Pts',(-9.95459581624042,9.88748715181938,
12.4661336363236));
#113420=CARTESIAN_POINT('Ctrl Pts',(-10.0537414793066,9.88162907834498,
12.4658535856989));
#113421=CARTESIAN_POINT('Ctrl Pts',(-10.1705691530577,9.87504117984222,
12.4536446488069));
#113422=CARTESIAN_POINT('Ctrl Pts',(-10.1889875434898,9.87401107687879,
12.4513649966937));
#113423=CARTESIAN_POINT('Ctrl Pts',(-10.2146727253466,9.87258595522523,
12.4476886644436));
#113424=CARTESIAN_POINT('Ctrl Pts',(-10.2219792960107,9.87218184729995,
12.4465863413923));
#113425=CARTESIAN_POINT('Ctrl Pts',(-10.2353602561993,9.87144407460977,
12.4444638220382));
#113426=CARTESIAN_POINT('Ctrl Pts',(-10.2414371237853,9.87110989060074,
12.4434605295051));
#113427=CARTESIAN_POINT('Ctrl Pts',(-10.2537590579502,9.87043398150606,
12.4413461841859));
#113428=CARTESIAN_POINT('Ctrl Pts',(-10.2600035998408,9.87009233625453,
12.4402328325524));
#113429=CARTESIAN_POINT('Ctrl Pts',(-10.2754514035148,9.86924929458444,
12.4373748688961));
#113430=CARTESIAN_POINT('Ctrl Pts',(-10.2846455989532,9.86874940759867,
12.4355824176591));
#113431=CARTESIAN_POINT('Ctrl Pts',(-10.3193552214165,9.86686881083936,
12.428469045712));
#113432=CARTESIAN_POINT('Ctrl Pts',(-10.3447449176104,9.86550673874607,
12.4225549628151));
#113433=CARTESIAN_POINT('Ctrl Pts',(-10.4085919418975,9.86210571696722,
12.4058729816874));
#113434=CARTESIAN_POINT('Ctrl Pts',(-10.446792107829,9.86009376431832,12.3942034720116));
#113435=CARTESIAN_POINT('Ctrl Pts',(-10.5455648683247,9.85489603500823,
12.3595526119834));
#113436=CARTESIAN_POINT('Ctrl Pts',(-10.6051721444239,9.85176612869738,
12.3340881673152));
#113437=CARTESIAN_POINT('Ctrl Pts',(-10.7300072059253,9.84494011717332,
12.2706643951548));
#113438=CARTESIAN_POINT('Ctrl Pts',(-10.7943798039771,9.84124443254299,
12.2314450292451));
#113439=CARTESIAN_POINT('Ctrl Pts',(-10.8651946002799,9.83665261940266,
12.1804300023848));
#113440=CARTESIAN_POINT('Ctrl Pts',(-10.8748587119894,9.83601368342828,
12.1732855162519));
#113441=CARTESIAN_POINT('Ctrl Pts',(-10.8880269731594,9.83512439223558,
12.1632973343212));
#113442=CARTESIAN_POINT('Ctrl Pts',(-10.8916078498252,9.83488063390505,
12.160555054339));
#113443=CARTESIAN_POINT('Ctrl Pts',(-10.8977168392171,9.83446135578417,
12.1558317534044));
#113444=CARTESIAN_POINT('Ctrl Pts',(-10.900251233902,9.8342863945172,12.1538588653047));
#113445=CARTESIAN_POINT('Ctrl Pts',(-10.9054619442421,9.83392452363076,
12.1497749938534));
#113446=CARTESIAN_POINT('Ctrl Pts',(-10.9081373936128,9.8337375375289,12.1476629916818));
#113447=CARTESIAN_POINT('Ctrl Pts',(-10.9145223683666,9.83328850242657,
12.1425863807602));
#113448=CARTESIAN_POINT('Ctrl Pts',(-10.9182248792449,9.83302584722511,
12.1396130350241));
#113449=CARTESIAN_POINT('Ctrl Pts',(-10.9261735409754,9.83245718425941,
12.1331658832771));
#113450=CARTESIAN_POINT('Ctrl Pts',(-10.9304147494144,9.83215078366186,
12.1296861242071));
#113451=CARTESIAN_POINT('Ctrl Pts',(-10.9421570453954,9.83129440296373,
12.1199410130196));
#113452=CARTESIAN_POINT('Ctrl Pts',(-10.9496149639325,9.8307412323541,12.1136243448397));
#113453=CARTESIAN_POINT('Ctrl Pts',(-10.9738749966481,9.82891277645808,
12.0926558103169));
#113454=CARTESIAN_POINT('Ctrl Pts',(-10.9904050895021,9.8276205057281,12.0776951777825));
#113455=CARTESIAN_POINT('Ctrl Pts',(-11.0644092223474,9.82164344265169,
12.0075764884374));
#113456=CARTESIAN_POINT('Ctrl Pts',(-11.1176612007506,9.8168040787014,11.9481615623249));
#113457=CARTESIAN_POINT('Ctrl Pts',(-11.2223438010768,9.80642700587287,
11.8102177226744));
#113458=CARTESIAN_POINT('Ctrl Pts',(-11.2716120844529,9.80094566884931,
11.73046889136));
#113459=CARTESIAN_POINT('Ctrl Pts',(-11.3182656332789,9.79507576618525,
11.6357306500799));
#113460=CARTESIAN_POINT('Ctrl Pts',(-11.323460518529,9.79440986951528,11.624843986457));
#113461=CARTESIAN_POINT('Ctrl Pts',(-11.3317247335049,9.79332974258818,
11.6069595053183));
#113462=CARTESIAN_POINT('Ctrl Pts',(-11.3348748313196,9.79291278315802,
11.5999998289309));
#113463=CARTESIAN_POINT('Ctrl Pts',(-11.3404211610531,9.79216900387095,
11.5874861223305));
#113464=CARTESIAN_POINT('Ctrl Pts',(-11.3428377104716,9.79184150328524,
11.5819413353436));
#113465=CARTESIAN_POINT('Ctrl Pts',(-11.3478978920332,9.79114826628413,
11.5701313541925));
#113466=CARTESIAN_POINT('Ctrl Pts',(-11.3505323785172,9.79078284274585,
11.5638623813337));
#113467=CARTESIAN_POINT('Ctrl Pts',(-11.3574959711797,9.78980450487223,
11.5469631395508));
#113468=CARTESIAN_POINT('Ctrl Pts',(-11.3617439224967,9.78919429769688,
11.5362998110006));
#113469=CARTESIAN_POINT('Ctrl Pts',(-11.3829166876477,9.78608060602992,
11.4812772567377));
#113470=CARTESIAN_POINT('Ctrl Pts',(-11.3978019122915,9.78364474708211,
11.4361613868698));
#113471=CARTESIAN_POINT('Ctrl Pts',(-11.4457360101786,9.77461698310313,
11.2629805251056));
#113472=CARTESIAN_POINT('Ctrl Pts',(-11.4635701272462,9.76846159256352,
11.1313942033913));
#113473=CARTESIAN_POINT('Ctrl Pts',(-11.4634997927887,9.76174222740085,
10.9992212140726));
#113474=CARTESIAN_POINT('Ctrl Pts',(-11.4634998220212,9.68830620133612,
10.9992782355534));
#113475=CARTESIAN_POINT('Ctrl Pts',(-11.4635429469811,9.69343852619092,
11.0867214055635));
#113476=CARTESIAN_POINT('Ctrl Pts',(-11.4557491548704,9.69876645421532,
11.173991636853));
#113477=CARTESIAN_POINT('Ctrl Pts',(-11.4300728543198,9.70739539864329,
11.316195617827));
#113478=CARTESIAN_POINT('Ctrl Pts',(-11.416658284113,9.71075321983715,11.3717100266276));
#113479=CARTESIAN_POINT('Ctrl Pts',(-11.390318033565,9.7159285351877,11.4582147519796));
#113480=CARTESIAN_POINT('Ctrl Pts',(-11.3795125452969,9.71780551448472,
11.4897860587433));
#113481=CARTESIAN_POINT('Ctrl Pts',(-11.3639897141292,9.72021344075026,
11.5305367850858));
#113482=CARTESIAN_POINT('Ctrl Pts',(-11.3602421131619,9.72077586490582,
11.5400727928912));
#113483=CARTESIAN_POINT('Ctrl Pts',(-11.3539419976944,9.72169138470325,
11.5556221511588));
#113484=CARTESIAN_POINT('Ctrl Pts',(-11.3514488604297,9.72204643757071,
11.5616590491941));
#113485=CARTESIAN_POINT('Ctrl Pts',(-11.346539826344,9.72273179772204,11.5733238633946));
#113486=CARTESIAN_POINT('Ctrl Pts',(-11.3441288548648,9.72306226077398,
11.5789536936174));
#113487=CARTESIAN_POINT('Ctrl Pts',(-11.338464895733,9.7238246716408,11.5919534330316));
#113488=CARTESIAN_POINT('Ctrl Pts',(-11.335186238294,9.72425574569722,11.5993119859952));
#113489=CARTESIAN_POINT('Ctrl Pts',(-11.3243105692131,9.72565315847926,
11.6231888328617));
#113490=CARTESIAN_POINT('Ctrl Pts',(-11.3164663239234,9.7266111240623,11.6395930435499));
#113491=CARTESIAN_POINT('Ctrl Pts',(-11.2592852667694,9.73326631203767,
11.7536607779819));
#113492=CARTESIAN_POINT('Ctrl Pts',(-11.1994388078099,9.73856815202739,
11.8456671707993));
#113493=CARTESIAN_POINT('Ctrl Pts',(-11.0905891970258,9.74690665917458,
11.977891282018));
#113494=CARTESIAN_POINT('Ctrl Pts',(-11.0483033289548,9.74992553095584,
12.0230910591678));
#113495=CARTESIAN_POINT('Ctrl Pts',(-10.9895166896113,9.75404501277318,
12.0784464899131));
#113496=CARTESIAN_POINT('Ctrl Pts',(-10.975494703158,9.75502257273336,12.0911462496094));
#113497=CARTESIAN_POINT('Ctrl Pts',(-10.9546584559813,9.75647462664689,
12.1092950266589));
#113498=CARTESIAN_POINT('Ctrl Pts',(-10.9480349614829,9.75693613029575,
12.1149609539311));
#113499=CARTESIAN_POINT('Ctrl Pts',(-10.9361223498875,9.75776682627462,
12.1249684503344));
#113500=CARTESIAN_POINT('Ctrl Pts',(-10.9308525993667,9.75813452659437,
12.1293327688653));
#113501=CARTESIAN_POINT('Ctrl Pts',(-10.9225259901414,9.75871622076786,
12.1361308521409));
#113502=CARTESIAN_POINT('Ctrl Pts',(-10.9194895916721,9.75892848693532,
12.1385896564424));
#113503=CARTESIAN_POINT('Ctrl Pts',(-10.9139896395615,9.75931330680082,
12.1430070401583));
#113504=CARTESIAN_POINT('Ctrl Pts',(-10.9115295793716,9.75948555673964,
12.1449698600876));
#113505=CARTESIAN_POINT('Ctrl Pts',(-10.9057789791387,9.75988849185047,
12.1495278392403));
#113506=CARTESIAN_POINT('Ctrl Pts',(-10.9024836357942,9.76011960113006,
12.1521167902901));
#113507=CARTESIAN_POINT('Ctrl Pts',(-10.8928314675794,9.76079702390766,
12.1596330922909));
#113508=CARTESIAN_POINT('Ctrl Pts',(-10.8864451905178,9.76124585872733,
12.1645221580183));
#113509=CARTESIAN_POINT('Ctrl Pts',(-10.8362239141879,9.76477816533409,
12.2023169765479));
#113510=CARTESIAN_POINT('Ctrl Pts',(-10.7906156643839,9.7680005774255,12.2327863858057));
#113511=CARTESIAN_POINT('Ctrl Pts',(-10.687479380953,9.77514723503009,12.2936076255848));
#113512=CARTESIAN_POINT('Ctrl Pts',(-10.6294141741077,9.77908159320722,
12.322832774934));
#113513=CARTESIAN_POINT('Ctrl Pts',(-10.5169954982628,9.78636945884805,
12.3703317460775));
#113514=CARTESIAN_POINT('Ctrl Pts',(-10.4631320092967,9.78973020310004,
12.3894614726743));
#113515=CARTESIAN_POINT('Ctrl Pts',(-10.3762331927796,9.79490937830925,
12.4147066087068));
#113516=CARTESIAN_POINT('Ctrl Pts',(-10.3438715931174,9.79678740572847,
12.4229191068024));
#113517=CARTESIAN_POINT('Ctrl Pts',(-10.3012424951101,9.79919645198739,
12.4321976886779));
#113518=CARTESIAN_POINT('Ctrl Pts',(-10.2912066951425,9.79975898453359,
12.4342719158109));
#113519=CARTESIAN_POINT('Ctrl Pts',(-10.2747396865461,9.80067463530868,
12.4374953975996));
#113520=CARTESIAN_POINT('Ctrl Pts',(-10.2683212197175,9.8010297118396,12.4387072803223));
#113521=CARTESIAN_POINT('Ctrl Pts',(-10.2558695753907,9.80171508660512,
12.4409720727719));
#113522=CARTESIAN_POINT('Ctrl Pts',(-10.2498374885065,9.80204554084979,
12.4420301609263));
#113523=CARTESIAN_POINT('Ctrl Pts',(-10.2358568034387,9.80280788678733,
12.4443921542127));
#113524=CARTESIAN_POINT('Ctrl Pts',(-10.2279036872808,9.8032389051946,12.4456683712739));
#113525=CARTESIAN_POINT('Ctrl Pts',(-10.2019716093904,9.80463594455662,
12.4496103113135));
#113526=CARTESIAN_POINT('Ctrl Pts',(-10.1839530810802,9.80559359873114,
12.4520068484133));
#113527=CARTESIAN_POINT('Ctrl Pts',(-10.0570708613357,9.81225447752986,
12.4664827987086));
#113528=CARTESIAN_POINT('Ctrl Pts',(-9.94719826427292,9.8175613665428,12.4666435572833));
#113529=CARTESIAN_POINT('Ctrl Pts',(-9.77694941808122,9.8259016078335,12.4477204837495));
#113530=CARTESIAN_POINT('Ctrl Pts',(-9.71606765643149,9.82891675932577,
12.4370203953792));
#113531=CARTESIAN_POINT('Ctrl Pts',(-9.63767457849472,9.83303153034887,
12.4180655362463));
#113532=CARTESIAN_POINT('Ctrl Pts',(-9.61938948424919,9.83400838726915,
12.4132675453968));
#113533=CARTESIAN_POINT('Ctrl Pts',(-9.58893787359339,9.83567157807621,
12.4046432582679));
#113534=CARTESIAN_POINT('Ctrl Pts',(-9.57671886680961,9.83634888157252,
12.401009570026));
#113535=CARTESIAN_POINT('Ctrl Pts',(-9.55979474875185,9.837302817685,12.3957350709302));
#113536=CARTESIAN_POINT('Ctrl Pts',(-9.55504786047416,9.83757212262337,
12.3942290498799));
#113537=CARTESIAN_POINT('Ctrl Pts',(-9.54699805697024,9.83803192262449,
12.3916298335306));
#113538=CARTESIAN_POINT('Ctrl Pts',(-9.54369113488434,9.83822170800693,
12.3905490186924));
#113539=CARTESIAN_POINT('Ctrl Pts',(-9.53733812669189,9.83858808635694,
12.3884475363546));
#113540=CARTESIAN_POINT('Ctrl Pts',(-9.53429150890127,9.83876456972674,
12.3874286183912));
#113541=CARTESIAN_POINT('Ctrl Pts',(-9.52697502377209,9.83919024236874,
12.384954862183));
#113542=CARTESIAN_POINT('Ctrl Pts',(-9.52270850650006,9.83943998368531,
12.383490306276));
#113543=CARTESIAN_POINT('Ctrl Pts',(-9.50710151365549,9.84035892421729,
12.3780521501353));
#113544=CARTESIAN_POINT('Ctrl Pts',(-9.49580363399297,9.84103458417673,
12.3739587519168));
#113545=CARTESIAN_POINT('Ctrl Pts',(-9.41261059788289,9.84608072569973,
12.3426523637845));
#113546=CARTESIAN_POINT('Ctrl Pts',(-9.34291418490526,9.85069586025734,
12.30995342135));
#113547=CARTESIAN_POINT('Ctrl Pts',(-9.2189234356124,9.85928053045996,12.2393877085059));
#113548=CARTESIAN_POINT('Ctrl Pts',(-9.16398945000605,9.86323843381767,
12.2030169539097));
#113549=CARTESIAN_POINT('Ctrl Pts',(-9.06569624426849,9.87049425980762,
12.1279440729478));
#113550=CARTESIAN_POINT('Ctrl Pts',(-9.02182512190009,9.87380861048452,
12.0901176590184));
#113551=CARTESIAN_POINT('Ctrl Pts',(-8.97161104040798,9.87768991826784,
12.0413430321092));
#113552=CARTESIAN_POINT('Ctrl Pts',(-8.96302173434888,9.87835732588763,
12.0327900327079));
#113553=CARTESIAN_POINT('Ctrl Pts',(-8.94968210782994,9.87939964046026,
12.0191725843584));
#113554=CARTESIAN_POINT('Ctrl Pts',(-8.9448600084295,9.8797776488194,12.0141794869829));
#113555=CARTESIAN_POINT('Ctrl Pts',(-8.93591359088611,9.880481345071,12.0047829416177));
#113556=CARTESIAN_POINT('Ctrl Pts',(-8.93178063984191,9.88080739839743,
12.0003879477035));
#113557=CARTESIAN_POINT('Ctrl Pts',(-8.92261436664782,9.88153278063923,
11.9905189262006));
#113558=CARTESIAN_POINT('Ctrl Pts',(-8.91759533169696,9.88193150405114,
11.9850318182257));
#113559=CARTESIAN_POINT('Ctrl Pts',(-8.90499464957722,9.88293662058158,
11.9710433967644));
#113560=CARTESIAN_POINT('Ctrl Pts',(-8.89746995658573,9.8835406612028,11.9624913032657));
#113561=CARTESIAN_POINT('Ctrl Pts',(-8.85183475573293,9.88722952750027,
11.9093876956457));
#113562=CARTESIAN_POINT('Ctrl Pts',(-8.81632804306537,9.890208133278,11.8626651151827));
#113563=CARTESIAN_POINT('Ctrl Pts',(-8.78168562879809,9.89330338755409,
11.8108980757707));
#113564=CARTESIAN_POINT('Ctrl Pts',(-8.77966521118386,9.89348467383459,
11.8078543183925));
#113565=CARTESIAN_POINT('Ctrl Pts',(-8.72391876214443,9.89850852208393,
11.7231859901556));
#113566=CARTESIAN_POINT('Ctrl Pts',(-8.67849356435907,9.90315067663834,
11.6363966667992));
#113567=CARTESIAN_POINT('Ctrl Pts',(-8.62462901023069,9.91034824039895,
11.5023656581116));
#113568=CARTESIAN_POINT('Ctrl Pts',(-8.60928983286015,9.91272809556236,
11.4581932536058));
#113569=CARTESIAN_POINT('Ctrl Pts',(-8.59396044537834,9.91562070779918,
11.4061304372609));
#113570=CARTESIAN_POINT('Ctrl Pts',(-8.59188567973241,9.91602563134109,
11.3988774466754));
#113571=CARTESIAN_POINT('Ctrl Pts',(-8.58878771090022,9.91665185139239,
11.3877220624297));
#113572=CARTESIAN_POINT('Ctrl Pts',(-8.58772438426416,9.91687092808195,
11.3838308312346));
#113573=CARTESIAN_POINT('Ctrl Pts',(-8.58579974831586,9.91727526022663,
11.3766713703653));
#113574=CARTESIAN_POINT('Ctrl Pts',(-8.58493366099531,9.91746024180222,
11.3734045108452));
#113575=CARTESIAN_POINT('Ctrl Pts',(-8.58300320454476,9.91787948662472,
11.3660197012764));
#113576=CARTESIAN_POINT('Ctrl Pts',(-8.58194547233547,9.91811411606763,
11.3619001183897));
#113577=CARTESIAN_POINT('Ctrl Pts',(-8.57926135294477,9.91872231905239,
11.3512537417045));
#113578=CARTESIAN_POINT('Ctrl Pts',(-8.57766199614514,9.91909734166273,
11.3447203121438));
#113579=CARTESIAN_POINT('Ctrl Pts',(-8.5676318837832,9.92153192026289,11.3024884863029));
#113580=CARTESIAN_POINT('Ctrl Pts',(-8.56050132560197,9.92365455854974,
11.2664973740121));
#113581=CARTESIAN_POINT('Ctrl Pts',(-8.53885626972182,9.93175253910585,
11.1306497032781));
#113582=CARTESIAN_POINT('Ctrl Pts',(-8.53332596227692,9.9379243020373,11.0296452501177));
#113583=CARTESIAN_POINT('Ctrl Pts',(-8.54130347976066,9.94763752349695,
10.8656975168665));
#113584=CARTESIAN_POINT('Ctrl Pts',(-8.54846979039542,9.95129669376925,
10.8027835502904));
#113585=CARTESIAN_POINT('Ctrl Pts',(-8.56258476452079,9.95574547976785,
10.7244332899017));
#113586=CARTESIAN_POINT('Ctrl Pts',(-8.56575310042201,9.95665081479642,
10.708391645769));
#113587=CARTESIAN_POINT('Ctrl Pts',(-8.57083036558007,9.95797594845148,
10.6847741395887));
#113588=CARTESIAN_POINT('Ctrl Pts',(-8.5725321095842,9.95840222216736,10.6771554365603));
#113589=CARTESIAN_POINT('Ctrl Pts',(-8.57566499203983,9.95915644999239,
10.6636387920155));
#113590=CARTESIAN_POINT('Ctrl Pts',(-8.5770720021878,9.9594851584985,10.6577354945192));
#113591=CARTESIAN_POINT('Ctrl Pts',(-8.58011142853446,9.96017474539921,
10.6453259416234));
#113592=CARTESIAN_POINT('Ctrl Pts',(-8.58175194198266,9.96053535807072,
10.6388218015498));
#113593=CARTESIAN_POINT('Ctrl Pts',(-8.58621362830064,9.9614863892437,10.6216318115937));
#113594=CARTESIAN_POINT('Ctrl Pts',(-8.58911125472945,9.96207436368118,
10.6109661349416));
#113595=CARTESIAN_POINT('Ctrl Pts',(-8.60233052175095,9.96463330963514,
10.5643996986256));
#113596=CARTESIAN_POINT('Ctrl Pts',(-8.61390406095152,9.96656408278289,
10.5288673865308));
#113597=CARTESIAN_POINT('Ctrl Pts',(-8.67625315595973,9.97571408849073,
10.3597273146995));
#113598=CARTESIAN_POINT('Ctrl Pts',(-8.74504551395334,9.98232925048296,
10.2336208292813));
#113599=CARTESIAN_POINT('Ctrl Pts',(-8.843431449092,9.99063955110981,10.1030007509666));
#113600=CARTESIAN_POINT('Ctrl Pts',(-8.85619945949582,9.99170285182257,
10.0867756476086));
#113601=CARTESIAN_POINT('Ctrl Pts',(-8.87794811720875,9.99349936051039,
10.0603100982597));
#113602=CARTESIAN_POINT('Ctrl Pts',(-8.88673640826825,9.99422155671268,
10.0499149047499));
#113603=CARTESIAN_POINT('Ctrl Pts',(-8.89902131959352,9.99522839606229,
10.0357882454523));
#113604=CARTESIAN_POINT('Ctrl Pts',(-8.90239466250804,9.99550459446113,
10.0319499579769));
#113605=CARTESIAN_POINT('Ctrl Pts',(-8.90811519392663,9.99597267122059,
10.0255093117909));
#113606=CARTESIAN_POINT('Ctrl Pts',(-8.9104517893094,9.99616377734365,10.0228975348321));
#113607=CARTESIAN_POINT('Ctrl Pts',(-8.91492944366567,9.99652989306577,
10.0179285779094));
#113608=CARTESIAN_POINT('Ctrl Pts',(-8.91706885022544,9.99670477428029,
10.0155699543599));
#113609=CARTESIAN_POINT('Ctrl Pts',(-8.92218539782627,9.99712286147057,
10.0099659960374));
#113610=CARTESIAN_POINT('Ctrl Pts',(-8.92516950622037,9.99736657795279,
10.006727099794));
#113611=CARTESIAN_POINT('Ctrl Pts',(-8.93583702345718,9.99823721170144,
9.99525313592193));
#113612=CARTESIAN_POINT('Ctrl Pts',(-8.94360062944579,9.99886974609392,
9.98709356021656));
#113613=CARTESIAN_POINT('Ctrl Pts',(-9.02052780910603,10.0051194244367,
9.90808927631429));
#113614=CARTESIAN_POINT('Ctrl Pts',(-9.09661340340824,10.0111427820746,
9.84435080480534));
#113615=CARTESIAN_POINT('Ctrl Pts',(-9.23489428455426,10.0211756763731,
9.75056755286459));
#113616=CARTESIAN_POINT('Ctrl Pts',(-9.29384748122678,10.0252189596186,
9.71632622467873));
#113617=CARTESIAN_POINT('Ctrl Pts',(-9.37716974242864,10.0305560874737,
9.67541476174027));
#113618=CARTESIAN_POINT('Ctrl Pts',(-9.39963731902107,10.0319606905992,
9.66508115047922));
#113619=CARTESIAN_POINT('Ctrl Pts',(-9.43908455854085,10.0343672126787,
9.64813552162616));
#113620=CARTESIAN_POINT('Ctrl Pts',(-9.45594533499729,10.0353774484928,
9.6412622535473));
#113621=CARTESIAN_POINT('Ctrl Pts',(-9.48053192370348,10.036824716506,9.63177064775783));
#113622=CARTESIAN_POINT('Ctrl Pts',(-9.48815780350037,10.0372700589915,
9.62889963450686));
#113623=CARTESIAN_POINT('Ctrl Pts',(-9.50154938097836,10.0380460182381,
9.62398523216919));
#113624=CARTESIAN_POINT('Ctrl Pts',(-9.50730460175746,10.0383775429948,
9.62191404222653));
#113625=CARTESIAN_POINT('Ctrl Pts',(-9.51925010262383,10.0390616755179,
9.6176994912034));
#113626=CARTESIAN_POINT('Ctrl Pts',(-9.52544213627317,10.0394141019826,
9.61556148698245));
#113627=CARTESIAN_POINT('Ctrl Pts',(-9.54143913332729,10.0403190439857,
9.61015793066456));
#113628=CARTESIAN_POINT('Ctrl Pts',(-9.5512647964227,10.0408695334523,9.60695449804873));
#113629=CARTESIAN_POINT('Ctrl Pts',(-9.59075090794574,10.043061231024,9.59454209002999));
#113630=CARTESIAN_POINT('Ctrl Pts',(-9.6206682177543,10.0446754280182,9.58617386746621));
#113631=CARTESIAN_POINT('Ctrl Pts',(-9.77282805911964,10.0526907339707,
9.54879123799847));
#113632=CARTESIAN_POINT('Ctrl Pts',(-9.89816789410017,10.0586147550827,
9.53465255419911));
#113633=CARTESIAN_POINT('Ctrl Pts',(-10.0778929076538,10.0675091968103,
9.53757231172584));
#113634=CARTESIAN_POINT('Ctrl Pts',(-10.1319178438482,10.0702435540323,
9.54145326544586));
#113635=CARTESIAN_POINT('Ctrl Pts',(-10.1933019074375,10.0735394864808,
9.54930122177673));
#113636=CARTESIAN_POINT('Ctrl Pts',(-10.2009978286706,10.073956150462,9.55034747605381));
#113637=CARTESIAN_POINT('Ctrl Pts',(-10.2127240431901,10.0745967623492,
9.55203681510023));
#113638=CARTESIAN_POINT('Ctrl Pts',(-10.2167606962006,10.0748183286146,
9.552635601122));
#113639=CARTESIAN_POINT('Ctrl Pts',(-10.2241337399032,10.0752250132131,
9.55376083402037));
#113640=CARTESIAN_POINT('Ctrl Pts',(-10.227470859399,10.0754098351782,9.55428195482394));
#113641=CARTESIAN_POINT('Ctrl Pts',(-10.2349524776899,10.0758258832384,
9.55547682136548));
#113642=CARTESIAN_POINT('Ctrl Pts',(-10.2390958657187,10.0760574499858,
9.55615684837898));
#113643=CARTESIAN_POINT('Ctrl Pts',(-10.2512043440916,10.0767374377372,
9.55819768269092));
#113644=CARTESIAN_POINT('Ctrl Pts',(-10.2591610304336,10.0771884080902,
9.55960661658563));
#113645=CARTESIAN_POINT('Ctrl Pts',(-10.3249658310771,10.0809501261909,
9.57182191523864));
#113646=CARTESIAN_POINT('Ctrl Pts',(-10.3821203951458,10.0844208780651,
9.58604169478641));
#113647=CARTESIAN_POINT('Ctrl Pts',(-10.4532103132402,10.0888772009644,
9.60835411530643));
#113648=CARTESIAN_POINT('Ctrl Pts',(-10.4680864791138,10.0898178078741,
9.61328701753133));
#113649=CARTESIAN_POINT('Ctrl Pts',(-10.5262830611944,10.0935236503403,
9.63362804655819));
#113650=CARTESIAN_POINT('Ctrl Pts',(-10.5689475221038,10.0962969222659,
9.65083543288455));
#113651=CARTESIAN_POINT('Ctrl Pts',(-10.6621165046477,10.1024168949535,
9.69361905306786));
#113652=CARTESIAN_POINT('Ctrl Pts',(-10.7120943129398,10.1057428651567,
9.72017496845359));
#113653=CARTESIAN_POINT('Ctrl Pts',(-10.7887456925683,10.1108760738997,
9.76678792277443));
#113654=CARTESIAN_POINT('Ctrl Pts',(-10.8164853688777,10.1127415912754,
9.78497584981021));
#113655=CARTESIAN_POINT('Ctrl Pts',(-10.8519396333987,10.1151372642407,
9.80998502274923));
#113656=CARTESIAN_POINT('Ctrl Pts',(-10.8602325895159,10.1156984989772,
9.81596592769202));
#113657=CARTESIAN_POINT('Ctrl Pts',(-10.8737156475717,10.1166125815493,
9.82590638584195));
#113658=CARTESIAN_POINT('Ctrl Pts',(-10.8789430466826,10.1169673748126,
9.82981455733642));
#113659=CARTESIAN_POINT('Ctrl Pts',(-10.8890260497643,10.1176525754766,
9.83745861885132));
#113660=CARTESIAN_POINT('Ctrl Pts',(-10.8938846763555,10.1179831359847,
9.8411902800779));
#113661=CARTESIAN_POINT('Ctrl Pts',(-10.9050868590331,10.1187462632,9.84990647754119));
#113662=CARTESIAN_POINT('Ctrl Pts',(-10.911412949548,10.1191779509325,9.85491320341774));
#113663=CARTESIAN_POINT('Ctrl Pts',(-10.9319119848368,10.1205794862349,
9.87141447559486));
#113664=CARTESIAN_POINT('Ctrl Pts',(-10.9459116995941,10.1215408902521,
9.88312206190239));
#113665=CARTESIAN_POINT('Ctrl Pts',(-11.0412972961293,10.1281298732351,
9.96597082458304));
#113666=CARTESIAN_POINT('Ctrl Pts',(-11.1148018409877,10.1333730258618,
10.0456752531836));
#113667=CARTESIAN_POINT('Ctrl Pts',(-11.216066620657,10.141691799218,10.1833263494909));
#113668=CARTESIAN_POINT('Ctrl Pts',(-11.249975355087,10.144754103187,10.2362366285427));
#113669=CARTESIAN_POINT('Ctrl Pts',(-11.2896219527467,10.1489285484622,
10.3078500452822));
#113670=CARTESIAN_POINT('Ctrl Pts',(-11.2985361556874,10.1499142631211,
10.3247221792628));
#113671=CARTESIAN_POINT('Ctrl Pts',(-11.3128914673595,10.1515911684447,
10.3532287540284));
#113672=CARTESIAN_POINT('Ctrl Pts',(-11.3185140424906,10.1522731350291,
10.3647695321754));
#113673=CARTESIAN_POINT('Ctrl Pts',(-11.3261118520167,10.1532325786207,
10.3809002140401));
#113674=CARTESIAN_POINT('Ctrl Pts',(-11.3282166523921,10.1535026155764,
10.3854288390449));
#113675=CARTESIAN_POINT('Ctrl Pts',(-11.3317494841296,10.1539632907507,
10.3931328944634));
#113676=CARTESIAN_POINT('Ctrl Pts',(-11.3331894586537,10.1541532127041,
10.396302857886));
#113677=CARTESIAN_POINT('Ctrl Pts',(-11.3359349899429,10.1545195476271,
10.4024046081798));
#113678=CARTESIAN_POINT('Ctrl Pts',(-11.3372422321661,10.1546958489397,
10.4053355889402));
#113679=CARTESIAN_POINT('Ctrl Pts',(-11.3403588329447,10.1551206673123,
10.4123855948063));
#113680=CARTESIAN_POINT('Ctrl Pts',(-11.3421588480684,10.155369731712,10.4165086841163));
#113681=CARTESIAN_POINT('Ctrl Pts',(-11.3486599108059,10.1562827690098,
10.4315891802221));
#113682=CARTESIAN_POINT('Ctrl Pts',(-11.3532458881252,10.1569530946779,
10.4425953329252));
#113683=CARTESIAN_POINT('Ctrl Pts',(-11.3890690174472,10.1623996076468,
10.5316178874271));
#113684=CARTESIAN_POINT('Ctrl Pts',(-11.4136654823685,10.1674677008347,
10.6121311288679));
#113685=CARTESIAN_POINT('Ctrl Pts',(-11.4526326753921,10.1786934254206,
10.7945677441922));
#113686=CARTESIAN_POINT('Ctrl Pts',(-11.4634561904881,10.1848010301259,
10.8968206735927));
#113687=CARTESIAN_POINT('Ctrl Pts',(-11.4634998672784,10.1905769185562,
10.9993767215278));
#113688=CARTESIAN_POINT('Origin',(-10.,3.5,11.));
#113689=CARTESIAN_POINT('',(-11.4635,10.7604277254418,11.0000000000833));
#113690=CARTESIAN_POINT('',(-11.463499418515,10.6893450235318,11.0013046096532));
#113691=CARTESIAN_POINT('',(-11.4635,3.5,11.));
#113692=CARTESIAN_POINT('Ctrl Pts',(-11.4635,10.7604277254418,11.0000000000833));
#113693=CARTESIAN_POINT('Ctrl Pts',(-11.4635000000053,10.7547997906437,
10.9061827223186));
#113694=CARTESIAN_POINT('Ctrl Pts',(-11.4544789754102,10.749283903319,10.8125691096008));
#113695=CARTESIAN_POINT('Ctrl Pts',(-11.4345115940165,10.743453902123,10.7099604418026));
#113696=CARTESIAN_POINT('Ctrl Pts',(-11.4323553763509,10.7428614340804,
10.6994928570103));
#113697=CARTESIAN_POINT('Ctrl Pts',(-11.428576935905,10.7418815432258,10.6821155188989));
#113698=CARTESIAN_POINT('Ctrl Pts',(-11.4270187869678,10.7414921283556,
10.6751923811775));
#113699=CARTESIAN_POINT('Ctrl Pts',(-11.4238625334524,10.7407311075056,
10.6616298383438));
#113700=CARTESIAN_POINT('Ctrl Pts',(-11.4222681923137,10.740359393331,10.6549897511698));
#113701=CARTESIAN_POINT('Ctrl Pts',(-11.4191752228267,10.7396614638034,
10.6424941034062));
#113702=CARTESIAN_POINT('Ctrl Pts',(-11.4176866857666,10.7393349362192,
10.6366362130144));
#113703=CARTESIAN_POINT('Ctrl Pts',(-11.4142462240952,10.7386007706892,
10.6234398757249));
#113704=CARTESIAN_POINT('Ctrl Pts',(-11.4122733801302,10.7381938087947,
10.6161070301772));
#113705=CARTESIAN_POINT('Ctrl Pts',(-11.4070597360085,10.7371531327239,
10.5973127670552));
#113706=CARTESIAN_POINT('Ctrl Pts',(-11.4037358977619,10.7365220768464,
10.5858748394572));
#113707=CARTESIAN_POINT('Ctrl Pts',(-11.3790129158789,10.7320474974723,
10.5045183856098));
#113708=CARTESIAN_POINT('Ctrl Pts',(-11.3525391369504,10.7283742235854,
10.4362463170501));
#113709=CARTESIAN_POINT('Ctrl Pts',(-11.297519344144,10.7220857438647,10.3208306435393));
#113710=CARTESIAN_POINT('Ctrl Pts',(-11.2712159816375,10.7194398415474,
10.2727879009053));
#113711=CARTESIAN_POINT('Ctrl Pts',(-11.203493963091,10.7131861618418,10.1640462662085));
#113712=CARTESIAN_POINT('Ctrl Pts',(-11.1600786676837,10.7095673986135,
10.104772935813));
#113713=CARTESIAN_POINT('Ctrl Pts',(-11.1057233052021,10.7051458763059,
10.0411913265861));
#113714=CARTESIAN_POINT('Ctrl Pts',(-11.0989558077283,10.704597031036,10.0334420758216));
#113715=CARTESIAN_POINT('Ctrl Pts',(-11.0890178418926,10.703792353166,10.0223017184476));
#113716=CARTESIAN_POINT('Ctrl Pts',(-11.0859119080876,10.7035410446066,
10.0188531626722));
#113717=CARTESIAN_POINT('Ctrl Pts',(-11.0804887171331,10.7031024318616,
10.0128890235853));
#113718=CARTESIAN_POINT('Ctrl Pts',(-11.0781789272478,10.702915679546,10.0103666596512));
#113719=CARTESIAN_POINT('Ctrl Pts',(-11.0732921319586,10.7025206472851,
10.0050675397512));
#113720=CARTESIAN_POINT('Ctrl Pts',(-11.0707131849895,10.7023122270468,
10.0022926903127));
#113721=CARTESIAN_POINT('Ctrl Pts',(-11.0637374129124,10.7017486940809,
9.99484521988085));
#113722=CARTESIAN_POINT('Ctrl Pts',(-11.0593206371623,10.7013921225682,
9.99019150319104));
#113723=CARTESIAN_POINT('Ctrl Pts',(-11.0391466323553,10.6997651433688,
9.96921325798015));
#113724=CARTESIAN_POINT('Ctrl Pts',(-11.0230424470121,10.698471047192,9.95322826347696));
#113725=CARTESIAN_POINT('Ctrl Pts',(-10.9419777833616,10.6920086190878,
9.87642149131234));
#113726=CARTESIAN_POINT('Ctrl Pts',(-10.8719367980879,10.686595600217,9.82123965520631));
#113727=CARTESIAN_POINT('Ctrl Pts',(-10.7429753074925,10.6773729660338,
9.73745492201226));
#113728=CARTESIAN_POINT('Ctrl Pts',(-10.6863399904447,10.6735343819576,
9.70579322690261));
#113729=CARTESIAN_POINT('Ctrl Pts',(-10.6061086226439,10.6684341491352,
9.66769352429766));
#113730=CARTESIAN_POINT('Ctrl Pts',(-10.5841789489759,10.6670721982255,
9.65793321504449));
#113731=CARTESIAN_POINT('Ctrl Pts',(-10.5457162266694,10.6647387806049,
9.64193601883193));
#113732=CARTESIAN_POINT('Ctrl Pts',(-10.5292923931357,10.6637594423995,
9.63545114499648));
#113733=CARTESIAN_POINT('Ctrl Pts',(-10.5051469880933,10.6623438921197,
9.62641900613032));
#113734=CARTESIAN_POINT('Ctrl Pts',(-10.4975155991831,10.6618999752809,
9.623636509283));
#113735=CARTESIAN_POINT('Ctrl Pts',(-10.484102711134,10.6611257335106,9.6188721417314));
#113736=CARTESIAN_POINT('Ctrl Pts',(-10.4783312763615,10.6607945116493,
9.6168627011633));
#113737=CARTESIAN_POINT('Ctrl Pts',(-10.4663405450099,10.66011029016,9.61277191687501));
#113738=CARTESIAN_POINT('Ctrl Pts',(-10.4601194965109,10.6597574769935,
9.61069610618399));
#113739=CARTESIAN_POINT('Ctrl Pts',(-10.4440220735393,10.6588500421336,
9.60544477704503));
#113740=CARTESIAN_POINT('Ctrl Pts',(-10.4341254186934,10.6582974694394,
9.60233229990579));
#113741=CARTESIAN_POINT('Ctrl Pts',(-10.3941506688643,10.6560860361381,
9.59022589019884));
#113742=CARTESIAN_POINT('Ctrl Pts',(-10.3638187791932,10.654454826036,9.58209525359855));
#113743=CARTESIAN_POINT('Ctrl Pts',(-10.210611033843,10.6464094247904,9.54626778635204));
#113744=CARTESIAN_POINT('Ctrl Pts',(-10.0847950563064,10.6404733768689,
9.53354066210397));
#113745=CARTESIAN_POINT('Ctrl Pts',(-9.90550159441945,10.6315925785157,
9.53857726136514));
#113746=CARTESIAN_POINT('Ctrl Pts',(-9.85222588322448,10.6288917342299,
9.54300032109587));
#113747=CARTESIAN_POINT('Ctrl Pts',(-9.79164345380039,10.6256341319354,
9.55138693564193));
#113748=CARTESIAN_POINT('Ctrl Pts',(-9.78397870311705,10.6252185273544,
9.55251008478071));
#113749=CARTESIAN_POINT('Ctrl Pts',(-9.77229532635904,10.6245792502028,
9.55431696245804));
#113750=CARTESIAN_POINT('Ctrl Pts',(-9.76826992439674,10.6243579447619,
9.55495673605292));
#113751=CARTESIAN_POINT('Ctrl Pts',(-9.76091458126963,10.6239515657501,
9.55615727468522));
#113752=CARTESIAN_POINT('Ctrl Pts',(-9.75758386182619,10.623766786603,9.55671275613981));
#113753=CARTESIAN_POINT('Ctrl Pts',(-9.75011299774511,10.6233506200677,
9.55798530150694));
#113754=CARTESIAN_POINT('Ctrl Pts',(-9.74597403330262,10.6231188902979,
9.55870866515151));
#113755=CARTESIAN_POINT('Ctrl Pts',(-9.7338682322749,10.6224378141069,9.5608781517215));
#113756=CARTESIAN_POINT('Ctrl Pts',(-9.72591034288388,10.6219859056689,
9.56237255667462));
#113757=CARTESIAN_POINT('Ctrl Pts',(-9.64613387633493,10.6174162300859,
9.57804015296798));
#113758=CARTESIAN_POINT('Ctrl Pts',(-9.57546875835911,10.6130521952094,
9.59751572274386));
#113759=CARTESIAN_POINT('Ctrl Pts',(-9.43477622288705,10.6040712484098,
9.64790202351978));
#113760=CARTESIAN_POINT('Ctrl Pts',(-9.36510187618191,10.5994671019091,
9.67918487573041));
#113761=CARTESIAN_POINT('Ctrl Pts',(-9.24799583018466,10.5916426884488,
9.74318155588011));
#113762=CARTESIAN_POINT('Ctrl Pts',(-9.19945797605669,10.5883689035972,
9.77352677922071));
#113763=CARTESIAN_POINT('Ctrl Pts',(-9.14296437931245,10.5845278802939,
9.81363236433785));
#113764=CARTESIAN_POINT('Ctrl Pts',(-9.13319939791361,10.5838626515886,
9.82074813948062));
#113765=CARTESIAN_POINT('Ctrl Pts',(-9.11797237170055,10.5828230270341,
9.83213546994633));
#113766=CARTESIAN_POINT('Ctrl Pts',(-9.11245079897331,10.5824455551042,
9.83632619875833));
#113767=CARTESIAN_POINT('Ctrl Pts',(-9.10218044643509,10.581742454745,9.84423675316168));
#113768=CARTESIAN_POINT('Ctrl Pts',(-9.0974245043081,10.5814164647094,9.8479470022687));
#113769=CARTESIAN_POINT('Ctrl Pts',(-9.08685053275288,10.5806907157047,
9.85630173647957));
#113770=CARTESIAN_POINT('Ctrl Pts',(-9.08104470595801,10.5802915664637,
9.86096144146016));
#113771=CARTESIAN_POINT('Ctrl Pts',(-9.06642252352293,10.5792844352352,
9.87288164750657));
#113772=CARTESIAN_POINT('Ctrl Pts',(-9.05765505251029,10.5786788235582,
9.88020149367515));
#113773=CARTESIAN_POINT('Ctrl Pts',(-9.00385929888975,10.5749502684628,
9.92619415363525));
#113774=CARTESIAN_POINT('Ctrl Pts',(-8.96113039516,10.5719363718953,9.96747578191413));
#113775=CARTESIAN_POINT('Ctrl Pts',(-8.85340019644995,10.5640174156504,
10.0850357735143));
#113776=CARTESIAN_POINT('Ctrl Pts',(-8.79352916509664,10.5592671757975,
10.1655676053775));
#113777=CARTESIAN_POINT('Ctrl Pts',(-8.72601741250604,10.5526923763829,
10.2790144626755));
#113778=CARTESIAN_POINT('Ctrl Pts',(-8.71059178427471,10.5510782929004,
10.3069790668705));
#113779=CARTESIAN_POINT('Ctrl Pts',(-8.69042051100301,10.5487732323348,
10.3465553555071));
#113780=CARTESIAN_POINT('Ctrl Pts',(-8.68489007457613,10.548118464817,10.3577584511645));
#113781=CARTESIAN_POINT('Ctrl Pts',(-8.67549826833073,10.5469634886149,
10.3774136740671));
#113782=CARTESIAN_POINT('Ctrl Pts',(-8.67157264501839,10.5464667068261,
10.3858344488774));
#113783=CARTESIAN_POINT('Ctrl Pts',(-8.66591256486667,10.5457285695778,
10.3982839566248));
#113784=CARTESIAN_POINT('Ctrl Pts',(-8.66411554168054,10.5454908392508,
10.4022841858802));
#113785=CARTESIAN_POINT('Ctrl Pts',(-8.66097425502319,10.5450691478249,
10.4093617173169));
#113786=CARTESIAN_POINT('Ctrl Pts',(-8.65962256978433,10.5448856363975,
10.4124356452021));
#113787=CARTESIAN_POINT('Ctrl Pts',(-8.65671542884547,10.544486423175,10.4191091440517));
#113788=CARTESIAN_POINT('Ctrl Pts',(-8.65516388054255,10.5442705023026,
10.4227102662513));
#113789=CARTESIAN_POINT('Ctrl Pts',(-8.65094696472251,10.5436758260625,
10.4326069297103));
#113790=CARTESIAN_POINT('Ctrl Pts',(-8.64831124327319,10.543295374688,10.4389148999977));
#113791=CARTESIAN_POINT('Ctrl Pts',(-8.63499914609308,10.541328980494,10.4714124494827));
#113792=CARTESIAN_POINT('Ctrl Pts',(-8.62504000210766,10.5397058963187,
10.4978875382606));
#113793=CARTESIAN_POINT('Ctrl Pts',(-8.60700287756042,10.536467589061,10.5504069223544));
#113794=CARTESIAN_POINT('Ctrl Pts',(-8.59887299529019,10.5348548222039,
10.5764224727577));
#113795=CARTESIAN_POINT('Ctrl Pts',(-8.56242015342782,10.5268469986105,
10.7056400258164));
#113796=CARTESIAN_POINT('Ctrl Pts',(-8.54474635359602,10.5203248068903,
10.81152067943));
#113797=CARTESIAN_POINT('Ctrl Pts',(-8.53613325584113,10.5113496713486,
10.9657262283736));
#113798=CARTESIAN_POINT('Ctrl Pts',(-8.53579108875596,10.5086535053874,
11.0131722768093));
#113799=CARTESIAN_POINT('Ctrl Pts',(-8.53822806765231,10.5053923791101,
11.0720187922413));
#113800=CARTESIAN_POINT('Ctrl Pts',(-8.53883760063605,10.5047612489473,
11.0834765943436));
#113801=CARTESIAN_POINT('Ctrl Pts',(-8.54002281901201,10.5037627499132,
11.1017108967944));
#113802=CARTESIAN_POINT('Ctrl Pts',(-8.54051109335387,10.5033926978334,
11.1084924378788));
#113803=CARTESIAN_POINT('Ctrl Pts',(-8.54152301812002,10.5026962021431,
11.1213001571628));
#113804=CARTESIAN_POINT('Ctrl Pts',(-8.5420368031537,10.502369460854,11.1273269529748));
#113805=CARTESIAN_POINT('Ctrl Pts',(-8.54328414426527,10.5016325807481,
11.1409593773818));
#113806=CARTESIAN_POINT('Ctrl Pts',(-8.54403993195253,10.5012231390261,
11.1485628273439));
#113807=CARTESIAN_POINT('Ctrl Pts',(-8.54614282808425,10.5001717564433,
11.1681582176433));
#113808=CARTESIAN_POINT('Ctrl Pts',(-8.54757878212707,10.4995325689911,
11.1801401670374));
#113809=CARTESIAN_POINT('Ctrl Pts',(-8.56142465634995,10.493983624911,11.2847095162364));
#113810=CARTESIAN_POINT('Ctrl Pts',(-8.58252471416636,10.4893640179191,
11.3759322176457));
#113811=CARTESIAN_POINT('Ctrl Pts',(-8.63349335585492,10.4815342436606,
11.5282051175993));
#113812=CARTESIAN_POINT('Ctrl Pts',(-8.65916283878904,10.4782967890616,
11.5903355746889));
#113813=CARTESIAN_POINT('Ctrl Pts',(-8.70249735519559,10.4734297386707,
11.6776728785523));
#113814=CARTESIAN_POINT('Ctrl Pts',(-8.7168310180172,10.4718916897755,11.7044365231716));
#113815=CARTESIAN_POINT('Ctrl Pts',(-8.73801513088745,10.4696872486856,
11.7411965099131));
#113816=CARTESIAN_POINT('Ctrl Pts',(-8.74417376612101,10.4690537202878,
11.7515840137387));
#113817=CARTESIAN_POINT('Ctrl Pts',(-8.75517052594085,10.4679329897077,
11.7696191918838));
#113818=CARTESIAN_POINT('Ctrl Pts',(-8.75995242070123,10.4674489422033,
11.7773005293559));
#113819=CARTESIAN_POINT('Ctrl Pts',(-8.76713211262178,10.4667262338022,
11.7885986597269));
#113820=CARTESIAN_POINT('Ctrl Pts',(-8.76947535368254,10.4664909841474,
11.7922500663805));
#113821=CARTESIAN_POINT('Ctrl Pts',(-8.77367535751717,10.4660703233456,
11.7987312290063));
#113822=CARTESIAN_POINT('Ctrl Pts',(-8.77552574034814,10.4658853288083,
11.801565026762));
#113823=CARTESIAN_POINT('Ctrl Pts',(-8.77956574666803,10.4654821230287,
11.8077055226295));
#113824=CARTESIAN_POINT('Ctrl Pts',(-8.7817589544364,10.4652636830626,11.8110096991619));
#113825=CARTESIAN_POINT('Ctrl Pts',(-8.78787844200941,10.464655522755,11.8201481778294));
#113826=CARTESIAN_POINT('Ctrl Pts',(-8.79183333351764,10.4642639819811,
11.8259630784298));
#113827=CARTESIAN_POINT('Ctrl Pts',(-8.81346592532299,10.462131347131,11.8572818010132));
#113828=CARTESIAN_POINT('Ctrl Pts',(-8.83190838480165,10.4603454650886,
11.8822453771999));
#113829=CARTESIAN_POINT('Ctrl Pts',(-8.86304368663352,10.4574046766675,
11.9217008884223));
#113830=CARTESIAN_POINT('Ctrl Pts',(-8.87525467564313,10.456268190878,11.9365629185263));
#113831=CARTESIAN_POINT('Ctrl Pts',(-8.94208266334871,10.450153672356,12.014707070443));
#113832=CARTESIAN_POINT('Ctrl Pts',(-9.00175375946532,10.4450682431004,
12.0734638825186));
#113833=CARTESIAN_POINT('Ctrl Pts',(-9.11756677632043,10.4361436807626,
12.1694482867504));
#113834=CARTESIAN_POINT('Ctrl Pts',(-9.17188182685075,10.4322672649661,
12.2085196839747));
#113835=CARTESIAN_POINT('Ctrl Pts',(-9.24296794176158,10.4275894007463,
12.2526041813151));
#113836=CARTESIAN_POINT('Ctrl Pts',(-9.25740438863672,10.4266581803532,
12.261216303078));
#113837=CARTESIAN_POINT('Ctrl Pts',(-9.27883228470759,10.4253028364607,
12.2735036916358));
#113838=CARTESIAN_POINT('Ctrl Pts',(-9.28570987031505,10.4248718040947,
12.2773739234167));
#113839=CARTESIAN_POINT('Ctrl Pts',(-9.29793935008301,10.4241122860226,
12.2841261759115));
#113840=CARTESIAN_POINT('Ctrl Pts',(-9.30327848434095,10.4237830073013,
12.2870308166398));
#113841=CARTESIAN_POINT('Ctrl Pts',(-9.31450663810641,10.4230953029959,
12.2930489054275));
#113842=CARTESIAN_POINT('Ctrl Pts',(-9.32039914104527,10.4227371198028,
12.2961555830748));
#113843=CARTESIAN_POINT('Ctrl Pts',(-9.33594046880033,10.4217994311675,
12.3042142483516));
#113844=CARTESIAN_POINT('Ctrl Pts',(-9.34562358085017,10.4212222468204,
12.3090994526976));
#113845=CARTESIAN_POINT('Ctrl Pts',(-9.38719995650233,10.4187729317251,
12.329498462767));
#113846=CARTESIAN_POINT('Ctrl Pts',(-9.41959836327716,10.4169367678432,
12.3439584273586));
#113847=CARTESIAN_POINT('Ctrl Pts',(-9.56443809814606,10.4089912704893,
12.402387027644));
#113848=CARTESIAN_POINT('Ctrl Pts',(-9.68153353201755,10.4032927241331,
12.4335207006078));
#113849=CARTESIAN_POINT('Ctrl Pts',(-9.85424200343877,10.3946628512953,
12.4572102741142));
#113850=CARTESIAN_POINT('Ctrl Pts',(-9.90771828257885,10.3919527417577,
12.4615711186602));
#113851=CARTESIAN_POINT('Ctrl Pts',(-9.96905649915228,10.3886845667216,
12.4631933708788));
#113852=CARTESIAN_POINT('Ctrl Pts',(-9.976806955096,10.3882686893503,12.4633367412465));
#113853=CARTESIAN_POINT('Ctrl Pts',(-9.98863483075482,10.3876290780289,
12.4634615489339));
#113854=CARTESIAN_POINT('Ctrl Pts',(-9.99271175871203,10.387407715019,12.4634875308665));
#113855=CARTESIAN_POINT('Ctrl Pts',(-10.0001654646229,10.3870012808454,
12.4635038863192));
#113856=CARTESIAN_POINT('Ctrl Pts',(-10.0035421478281,10.3868165046222,
12.4634996089111));
#113857=CARTESIAN_POINT('Ctrl Pts',(-10.011119285522,10.386400408587,12.4634637870096));
#113858=CARTESIAN_POINT('Ctrl Pts',(-10.0153196039819,10.3861687469633,
12.4634258448017));
#113859=CARTESIAN_POINT('Ctrl Pts',(-10.02761034898,10.3854880534732,12.4632619005959));
#113860=CARTESIAN_POINT('Ctrl Pts',(-10.0356998323165,10.3850364637911,
12.4630868863626));
#113861=CARTESIAN_POINT('Ctrl Pts',(-10.1175056331756,10.3804363962512,
12.4606381974949));
#113862=CARTESIAN_POINT('Ctrl Pts',(-10.1909448198655,10.3760379929665,
12.4528625011414));
#113863=CARTESIAN_POINT('Ctrl Pts',(-10.3094856413223,10.3687950031995,
12.4311668677988));
#113864=CARTESIAN_POINT('Ctrl Pts',(-10.3550651548998,10.3659732394667,
12.420545262272));
#113865=CARTESIAN_POINT('Ctrl Pts',(-10.4544347575514,10.359806687048,12.3923063254228));
#113866=CARTESIAN_POINT('Ctrl Pts',(-10.5078740813945,10.3564815985431,
12.3737149439448));
#113867=CARTESIAN_POINT('Ctrl Pts',(-10.5907360588929,10.3513496616357,
12.3393887524389));
#113868=CARTESIAN_POINT('Ctrl Pts',(-10.6209258391924,10.3494845621877,
12.3256631064033));
#113869=CARTESIAN_POINT('Ctrl Pts',(-10.659781195264,10.347089435138,12.3063787764712));
#113870=CARTESIAN_POINT('Ctrl Pts',(-10.6688895339176,10.3465283414083,
12.3017386573591));
#113871=CARTESIAN_POINT('Ctrl Pts',(-10.6837312892492,10.3456144948202,
12.2939808146894));
#113872=CARTESIAN_POINT('Ctrl Pts',(-10.6894936865504,10.3452597974355,
12.2909195493149));
#113873=CARTESIAN_POINT('Ctrl Pts',(-10.700624712586,10.344574787597,12.2849104134184));
#113874=CARTESIAN_POINT('Ctrl Pts',(-10.7059956805918,10.3442443220705,
12.2819671832572));
#113875=CARTESIAN_POINT('Ctrl Pts',(-10.718396166965,10.3434814239076,12.2750702880158));
#113876=CARTESIAN_POINT('Ctrl Pts',(-10.7254118313522,10.343049869637,12.271092038578));
#113877=CARTESIAN_POINT('Ctrl Pts',(-10.7481869493952,10.3416488211784,
12.2579273730278));
#113878=CARTESIAN_POINT('Ctrl Pts',(-10.763807928455,10.3406877640882,12.2485040945486));
#113879=CARTESIAN_POINT('Ctrl Pts',(-10.8708379990983,10.3340933506595,
12.1811778933719));
#113880=CARTESIAN_POINT('Ctrl Pts',(-10.9557555153073,10.3288453255794,
12.1135860558942));
#113881=CARTESIAN_POINT('Ctrl Pts',(-11.0768961338526,10.3205246851005,
11.9930052524465));
#113882=CARTESIAN_POINT('Ctrl Pts',(-11.1184488281583,10.3174657284237,
11.9459576809373));
#113883=CARTESIAN_POINT('Ctrl Pts',(-11.1685322343153,10.3132955653407,
11.8813218668758));
#113884=CARTESIAN_POINT('Ctrl Pts',(-11.1799148916231,10.3123105324518,
11.8660234444216));
#113885=CARTESIAN_POINT('Ctrl Pts',(-11.1984509536745,10.3106347181775,
11.8400667626018));
#113886=CARTESIAN_POINT('Ctrl Pts',(-11.2057690825715,10.3099531468485,
11.8295286320316));
#113887=CARTESIAN_POINT('Ctrl Pts',(-11.2157406684736,10.3089942145375,
11.8147587348675));
#113888=CARTESIAN_POINT('Ctrl Pts',(-11.2185126380754,10.3087242845307,
11.8106072528732));
#113889=CARTESIAN_POINT('Ctrl Pts',(-11.2231812164023,10.3082637762265,
11.8035372278182));
#113890=CARTESIAN_POINT('Ctrl Pts',(-11.2250887802904,10.3080739135103,
11.8006259081846));
#113891=CARTESIAN_POINT('Ctrl Pts',(-11.2287347902593,10.3077076823169,
11.7950178360897));
#113892=CARTESIAN_POINT('Ctrl Pts',(-11.2304747764753,10.307531425358,11.792322136851));
#113893=CARTESIAN_POINT('Ctrl Pts',(-11.2346327304216,10.3071067022195,
11.7858336356913));
#113894=CARTESIAN_POINT('Ctrl Pts',(-11.2370420894708,10.3068576888654,
11.7820353891011));
#113895=CARTESIAN_POINT('Ctrl Pts',(-11.2457737834779,10.3059447443888,
11.7681289464596));
#113896=CARTESIAN_POINT('Ctrl Pts',(-11.2519898722347,10.305274460854,11.7579549718576));
#113897=CARTESIAN_POINT('Ctrl Pts',(-11.3009618699232,10.2998339891384,
11.6755553593478));
#113898=CARTESIAN_POINT('Ctrl Pts',(-11.3375533695938,10.2947725968978,
11.5998546784398));
#113899=CARTESIAN_POINT('Ctrl Pts',(-11.3953964881368,10.2850034904056,
11.4481645267125));
#113900=CARTESIAN_POINT('Ctrl Pts',(-11.4174063857041,10.2803105400422,
11.3727520379573));
#113901=CARTESIAN_POINT('Ctrl Pts',(-11.4386922612988,10.2742363175254,
11.2696600436006));
#113902=CARTESIAN_POINT('Ctrl Pts',(-11.4433937934071,10.2727078712792,
11.2432415382901));
#113903=CARTESIAN_POINT('Ctrl Pts',(-11.450236806506,10.2701126482664,11.1975377718739));
#113904=CARTESIAN_POINT('Ctrl Pts',(-11.4527259661506,10.269035697827,11.1783123212896));
#113905=CARTESIAN_POINT('Ctrl Pts',(-11.4557401997089,10.2675116182542,
11.150739771814));
#113906=CARTESIAN_POINT('Ctrl Pts',(-11.4565767683192,10.2670549005589,
11.1424293855986));
#113907=CARTESIAN_POINT('Ctrl Pts',(-11.4579055805771,10.2662658104847,
11.1279897257452));
#113908=CARTESIAN_POINT('Ctrl Pts',(-11.4584304183583,10.2659324363664,
11.121863727897));
#113909=CARTESIAN_POINT('Ctrl Pts',(-11.4593673763403,10.2652923167664,
11.1100527023862));
#113910=CARTESIAN_POINT('Ctrl Pts',(-11.4597849193632,10.264985409241,11.1043682273761));
#113911=CARTESIAN_POINT('Ctrl Pts',(-11.4607975261001,10.2641794680605,
11.0893848852245));
#113912=CARTESIAN_POINT('Ctrl Pts',(-11.4613370172568,10.2636821573072,
11.0800824409014));
#113913=CARTESIAN_POINT('Ctrl Pts',(-11.4629378830962,10.2619249084422,
11.0470182948696));
#113914=CARTESIAN_POINT('Ctrl Pts',(-11.4635088466797,10.260680035812,11.0232359460211));
#113915=CARTESIAN_POINT('Ctrl Pts',(-11.4634998963974,10.2594509413502,
10.9994493233677));
#113916=CARTESIAN_POINT('Ctrl Pts',(-11.4634998672784,10.1905769185562,
10.9993767215278));
#113917=CARTESIAN_POINT('Ctrl Pts',(-11.4635087402576,10.1917502954767,
11.0202110747467));
#113918=CARTESIAN_POINT('Ctrl Pts',(-11.4630727178984,10.1929103982478,
11.0410439404734));
#113919=CARTESIAN_POINT('Ctrl Pts',(-11.4618180918408,10.1945436224955,
11.0706991190408));
#113920=CARTESIAN_POINT('Ctrl Pts',(-11.4613640568745,10.1950278809764,
11.0795336226862));
#113921=CARTESIAN_POINT('Ctrl Pts',(-11.4604569612154,10.1958461096992,
11.094529757153));
#113922=CARTESIAN_POINT('Ctrl Pts',(-11.4600449380559,10.1961813381255,
11.1006935500792));
#113923=CARTESIAN_POINT('Ctrl Pts',(-11.4591321939684,10.1968572818914,
11.113161291302));
#113924=CARTESIAN_POINT('Ctrl Pts',(-11.4586296167857,10.1971979323305,
11.119464974271));
#113925=CARTESIAN_POINT('Ctrl Pts',(-11.4572898380598,10.1980346966816,
11.1349979815483));
#113926=CARTESIAN_POINT('Ctrl Pts',(-11.4564057957963,10.1985293522045,
11.14422305779));
#113927=CARTESIAN_POINT('Ctrl Pts',(-11.4527793613769,10.2003657298693,
11.1786212723831));
#113928=CARTESIAN_POINT('Ctrl Pts',(-11.4494713520886,10.2016899589236,
11.2037310262968));
#113929=CARTESIAN_POINT('Ctrl Pts',(-11.4395178835776,10.2049754559772,
11.2666306570856));
#113930=CARTESIAN_POINT('Ctrl Pts',(-11.4320349842601,10.2069121359247,
11.304269147967));
#113931=CARTESIAN_POINT('Ctrl Pts',(-11.4075888170012,10.2121232551803,
11.4061185327691));
#113932=CARTESIAN_POINT('Ctrl Pts',(-11.3877222970212,10.2153327069813,
11.4695376944518));
#113933=CARTESIAN_POINT('Ctrl Pts',(-11.3359554807644,10.2222813590908,
11.6023785995309));
#113934=CARTESIAN_POINT('Ctrl Pts',(-11.302793136757,10.2260187699642,11.6710920949111));
#113935=CARTESIAN_POINT('Ctrl Pts',(-11.2583919615321,10.230658257944,11.7472791459426));
#113936=CARTESIAN_POINT('Ctrl Pts',(-11.2522182138101,10.2312966806352,
11.7575790239711));
#113937=CARTESIAN_POINT('Ctrl Pts',(-11.2435525950672,10.2321854218951,
11.7716408051306));
#113938=CARTESIAN_POINT('Ctrl Pts',(-11.2411688673024,10.2324291557478,
11.7754691680555));
#113939=CARTESIAN_POINT('Ctrl Pts',(-11.2370570634862,10.2328484335978,
11.7820053644841));
#113940=CARTESIAN_POINT('Ctrl Pts',(-11.2353376823465,10.2330234194541,
11.7847186620506));
#113941=CARTESIAN_POINT('Ctrl Pts',(-11.2317373574746,10.2333891800879,
11.7903590564388));
#113942=CARTESIAN_POINT('Ctrl Pts',(-11.2298548992932,10.2335800592346,
11.7932851200699));
#113943=CARTESIAN_POINT('Ctrl Pts',(-11.225252012212,10.2340458618815,11.8003840141447));
#113944=CARTESIAN_POINT('Ctrl Pts',(-11.2225206881745,10.2343214895584,
11.8045497057596));
#113945=CARTESIAN_POINT('Ctrl Pts',(-11.2127196948706,10.2353075648476,
11.8193325925128));
#113946=CARTESIAN_POINT('Ctrl Pts',(-11.2055327481338,10.2360251970548,
11.8298709093419));
#113947=CARTESIAN_POINT('Ctrl Pts',(-11.1873464865875,10.2378251884096,
11.8558028320513));
#113948=CARTESIAN_POINT('Ctrl Pts',(-11.1761848564835,10.2389160387255,
11.8710793824369));
#113949=CARTESIAN_POINT('Ctrl Pts',(-11.1272841915869,10.2436231772408,
11.9353541618816));
#113950=CARTESIAN_POINT('Ctrl Pts',(-11.086757147,10.2473458123594,11.9821482813872));
#113951=CARTESIAN_POINT('Ctrl Pts',(-10.9666762283056,10.2576512976286,
12.1042368700797));
#113952=CARTESIAN_POINT('Ctrl Pts',(-10.8814413221291,10.2641719474604,
12.1734012675663));
#113953=CARTESIAN_POINT('Ctrl Pts',(-10.7739794202707,10.2713245145159,
12.2422231232295));
#113954=CARTESIAN_POINT('Ctrl Pts',(-10.7584959635955,10.2723327750234,
12.2517373309323));
#113955=CARTESIAN_POINT('Ctrl Pts',(-10.73589956152,10.2737729209937,12.2650489912396));
#113956=CARTESIAN_POINT('Ctrl Pts',(-10.7289265713706,10.2742131256107,
12.2690796555173));
#113957=CARTESIAN_POINT('Ctrl Pts',(-10.7165935438463,10.2749844330836,
12.2760734483298));
#113958=CARTESIAN_POINT('Ctrl Pts',(-10.7112475599466,10.2753163928242,
12.2790608518209));
#113959=CARTESIAN_POINT('Ctrl Pts',(-10.7001609224506,10.2759999829107,
12.2851652033948));
#113960=CARTESIAN_POINT('Ctrl Pts',(-10.6944178292519,10.2763514425556,
12.2882774536759));
#113961=CARTESIAN_POINT('Ctrl Pts',(-10.6796107600734,10.277250905233,12.2961737935304));
#113962=CARTESIAN_POINT('Ctrl Pts',(-10.6705169363113,10.2777969299543,
12.3009013542479));
#113963=CARTESIAN_POINT('Ctrl Pts',(-10.6315890813982,10.2801080752409,
12.3206219367596));
#113964=CARTESIAN_POINT('Ctrl Pts',(-10.6012952121128,10.2818413150216,
12.3346877368311));
#113965=CARTESIAN_POINT('Ctrl Pts',(-10.5179247329741,10.2864623492634,
12.3699822511231));
#113966=CARTESIAN_POINT('Ctrl Pts',(-10.4640425903194,10.2892887374912,
12.3891589193271));
#113967=CARTESIAN_POINT('Ctrl Pts',(-10.4020283082121,10.2924472338555,
12.4072174278449));
#113968=CARTESIAN_POINT('Ctrl Pts',(-10.3948662362419,10.2928106623411,
12.4092438773955));
#113969=CARTESIAN_POINT('Ctrl Pts',(-10.2925469536391,10.2979863632561,
12.437353019407));
#113970=CARTESIAN_POINT('Ctrl Pts',(-10.1950157221062,10.3027032357727,
12.453799253202));
#113971=CARTESIAN_POINT('Ctrl Pts',(-10.0788969638044,10.3087485491173,
12.4614792935148));
#113972=CARTESIAN_POINT('Ctrl Pts',(-10.061190717498,10.3096824403585,12.4623276299303));
#113973=CARTESIAN_POINT('Ctrl Pts',(-10.0376230241181,10.3109465687501,
12.4630280328475));
#113974=CARTESIAN_POINT('Ctrl Pts',(-10.0317709270593,10.311262192774,12.4631668130179));
#113975=CARTESIAN_POINT('Ctrl Pts',(-10.0222545753738,10.311778475196,12.4633353718921));
#113976=CARTESIAN_POINT('Ctrl Pts',(-10.0185907066386,10.3119779786252,
12.4633865045774));
#113977=CARTESIAN_POINT('Ctrl Pts',(-10.0114518446186,10.3123681900871,
12.4634593200052));
#113978=CARTESIAN_POINT('Ctrl Pts',(-10.0079769178361,10.3125588224461,
12.463482385946));
#113979=CARTESIAN_POINT('Ctrl Pts',(-9.99954340099898,10.3130231103691,
12.4635083291254));
#113980=CARTESIAN_POINT('Ctrl Pts',(-9.99458483299467,10.3132974594287,
12.4634983814178));
#113981=CARTESIAN_POINT('Ctrl Pts',(-9.9770178232458,10.3142740228842,12.4633738606046));
#113982=CARTESIAN_POINT('Ctrl Pts',(-9.96441126698918,10.314983244761,12.4631215454226));
#113983=CARTESIAN_POINT('Ctrl Pts',(-9.93319129921668,10.3167578755444,
12.4620929790299));
#113984=CARTESIAN_POINT('Ctrl Pts',(-9.9145867634661,10.3178314888808,12.4611241575624));
#113985=CARTESIAN_POINT('Ctrl Pts',(-9.83595563669678,10.3224235074177,
12.4555226258912));
#113986=CARTESIAN_POINT('Ctrl Pts',(-9.77622873261292,10.3260436527171,
12.4475435700484));
#113987=CARTESIAN_POINT('Ctrl Pts',(-9.60754611631345,10.3363898988575,
12.4143178542094));
#113988=CARTESIAN_POINT('Ctrl Pts',(-9.50074091015564,10.3430574924025,
12.3802402714164));
#113989=CARTESIAN_POINT('Ctrl Pts',(-9.38402417628157,10.3502312912186,
12.3276559137121));
#113990=CARTESIAN_POINT('Ctrl Pts',(-9.36931665886675,10.3511339744866,
12.3207327487295));
#113991=CARTESIAN_POINT('Ctrl Pts',(-9.34679748656298,10.3525144765691,
12.3096704847812));
#113992=CARTESIAN_POINT('Ctrl Pts',(-9.33890319326492,10.3529981139995,
12.3057033810059));
#113993=CARTESIAN_POINT('Ctrl Pts',(-9.32555274362245,10.35381560688,12.2988422855884));
#113994=CARTESIAN_POINT('Ctrl Pts',(-9.32007816719641,10.3541507151379,
12.295984832999));
#113995=CARTESIAN_POINT('Ctrl Pts',(-9.30903225092473,10.3548266738485,
12.2901301638649));
#113996=CARTESIAN_POINT('Ctrl Pts',(-9.30346192932136,10.3551674575417,
12.2871313016904));
#113997=CARTESIAN_POINT('Ctrl Pts',(-9.28976911730005,10.3560050211665,
12.2796446592993));
#113998=CARTESIAN_POINT('Ctrl Pts',(-9.28166947103459,10.3565003363637,
12.2751155309557));
#113999=CARTESIAN_POINT('Ctrl Pts',(-9.25155178745401,10.3583421595042,
12.2578963898265));
#114000=CARTESIAN_POINT('Ctrl Pts',(-9.22982174722013,10.3596710359274,
12.2447102531085));
#114001=CARTESIAN_POINT('Ctrl Pts',(-9.17602124379907,10.3629706246461,
12.2101145761539));
#114002=CARTESIAN_POINT('Ctrl Pts',(-9.14443239848515,10.3649164627707,
12.1879910044656));
#114003=CARTESIAN_POINT('Ctrl Pts',(-9.0610844848641,10.370126005813,12.1245666241999));
#114004=CARTESIAN_POINT('Ctrl Pts',(-9.01119467476569,10.3733258543988,
12.0809610257993));
#114005=CARTESIAN_POINT('Ctrl Pts',(-8.9106718461047,10.3802595405064,11.9802978259537));
#114006=CARTESIAN_POINT('Ctrl Pts',(-8.86120083578663,10.3839917521697,
11.9223630849978));
#114007=CARTESIAN_POINT('Ctrl Pts',(-8.80939790475063,10.3886252686737,
11.8511422430614));
#114008=CARTESIAN_POINT('Ctrl Pts',(-8.80245402167343,10.3892637267956,
11.8413442093914));
#114009=CARTESIAN_POINT('Ctrl Pts',(-8.79306947405171,10.3901525089944,
11.8277507445931));
#114010=CARTESIAN_POINT('Ctrl Pts',(-8.7905244279565,10.3903962475449,11.8240275657979));
#114011=CARTESIAN_POINT('Ctrl Pts',(-8.78619619663323,10.3908155313687,
11.8176324941483));
#114012=CARTESIAN_POINT('Ctrl Pts',(-8.78440450906698,10.3909905184656,
11.8149663616191));
#114013=CARTESIAN_POINT('Ctrl Pts',(-8.7806904779767,10.3913562792501,11.8094001762187));
#114014=CARTESIAN_POINT('Ctrl Pts',(-8.77876968961178,10.3915471572909,
11.8064991530652));
#114015=CARTESIAN_POINT('Ctrl Pts',(-8.77412416440732,10.3920129531775,
11.7994282320693));
#114016=CARTESIAN_POINT('Ctrl Pts',(-8.77141034735266,10.3922885751524,
11.7952512348007));
#114017=CARTESIAN_POINT('Ctrl Pts',(-8.76182355985369,10.3932746078615,
11.7803294443974));
#114018=CARTESIAN_POINT('Ctrl Pts',(-8.75506998902289,10.3939922023927,
11.7695090538862));
#114019=CARTESIAN_POINT('Ctrl Pts',(-8.7386531600432,10.3957920799232,11.7424245864894));
#114020=CARTESIAN_POINT('Ctrl Pts',(-8.72916236292778,10.3968828527923,
11.7260590596319));
#114021=CARTESIAN_POINT('Ctrl Pts',(-8.69001256888584,10.4015894693512,
11.6554304425494));
#114022=CARTESIAN_POINT('Ctrl Pts',(-8.66349268225899,10.4053116389298,
11.599502803005));
#114023=CARTESIAN_POINT('Ctrl Pts',(-8.60006938422499,10.4156163611572,
11.4404487695174));
#114024=CARTESIAN_POINT('Ctrl Pts',(-8.57106396768715,10.4221367599141,
11.3345893074705));
#114025=CARTESIAN_POINT('Ctrl Pts',(-8.55131577385237,10.4292897153516,
11.2085109377557));
#114026=CARTESIAN_POINT('Ctrl Pts',(-8.5488371839734,10.4302985478611,11.1904975623334));
#114027=CARTESIAN_POINT('Ctrl Pts',(-8.54574562402567,10.4317393544073,
11.1644425537456));
#114028=CARTESIAN_POINT('Ctrl Pts',(-8.54486249019697,10.4321796581879,
11.156435209291));
#114029=CARTESIAN_POINT('Ctrl Pts',(-8.54342441442566,10.4329510810623,
11.1423282112598));
#114030=CARTESIAN_POINT('Ctrl Pts',(-8.54284156857864,10.4332830578301,
11.1362316539053));
#114031=CARTESIAN_POINT('Ctrl Pts',(-8.54171625039937,10.4339666278286,
11.1236261047494));
#114032=CARTESIAN_POINT('Ctrl Pts',(-8.54117904739401,10.4343180507639,
11.1171167718596));
#114033=CARTESIAN_POINT('Ctrl Pts',(-8.53991112343057,10.4352173051551,
11.1003877194206));
#114034=CARTESIAN_POINT('Ctrl Pts',(-8.53924410535028,10.4357631601072,
11.0901634352357));
#114035=CARTESIAN_POINT('Ctrl Pts',(-8.53686253841685,10.4380725417661,
11.0466241103748));
#114036=CARTESIAN_POINT('Ctrl Pts',(-8.53617986339711,10.4398042500448,
11.0132614341371));
#114037=CARTESIAN_POINT('Ctrl Pts',(-8.53742159065321,10.4444198607817,
10.9228460019067));
#114038=CARTESIAN_POINT('Ctrl Pts',(-8.54154151089922,10.4472425495139,
10.8658813647854));
#114039=CARTESIAN_POINT('Ctrl Pts',(-8.55090612133398,10.4507570759175,
10.7946266489073));
#114040=CARTESIAN_POINT('Ctrl Pts',(-8.55305706585009,10.4514786364106,
10.7799831094522));
#114041=CARTESIAN_POINT('Ctrl Pts',(-8.57147646227741,10.457073659183,10.6665763026729));
#114042=CARTESIAN_POINT('Ctrl Pts',(-8.59761445844416,10.4618789871233,
10.569696980072));
#114043=CARTESIAN_POINT('Ctrl Pts',(-8.63743209187229,10.4677444811539,
10.4658031631833));
#114044=CARTESIAN_POINT('Ctrl Pts',(-8.64155792519702,10.4683404620168,
10.455396769011));
#114045=CARTESIAN_POINT('Ctrl Pts',(-8.64746820164726,10.4691796015083,
10.4409747076588));
#114046=CARTESIAN_POINT('Ctrl Pts',(-8.64915206613876,10.4694171062503,
10.4369179441515));
#114047=CARTESIAN_POINT('Ctrl Pts',(-8.65208698238771,10.4698284912014,
10.4299360841979));
#114048=CARTESIAN_POINT('Ctrl Pts',(-8.65332936700261,10.4700018595023,
10.4270073499827));
#114049=CARTESIAN_POINT('Ctrl Pts',(-8.65596156618187,10.470367597016,10.4208581855653));
#114050=CARTESIAN_POINT('Ctrl Pts',(-8.65735341860562,10.4705600925052,
10.4176386778777));
#114051=CARTESIAN_POINT('Ctrl Pts',(-8.66080752490595,10.4710355519655,
10.4097271539162));
#114052=CARTESIAN_POINT('Ctrl Pts',(-8.66288286874368,10.4713192883491,
10.4050409309285));
#114053=CARTESIAN_POINT('Ctrl Pts',(-8.67060270317975,10.472367432314,10.387853599491));
#114054=CARTESIAN_POINT('Ctrl Pts',(-8.67639807441659,10.4731402368784,
10.375421499448));
#114055=CARTESIAN_POINT('Ctrl Pts',(-8.71822423839432,10.4786128343341,
10.2888942466231));
#114056=CARTESIAN_POINT('Ctrl Pts',(-8.76027875785401,10.4835825371276,
10.2178812410391));
#114057=CARTESIAN_POINT('Ctrl Pts',(-8.86974678993304,10.4949344521506,
10.0642360190502));
#114058=CARTESIAN_POINT('Ctrl Pts',(-8.94066745975049,10.5012573896226,
9.98464396843344));
#114059=CARTESIAN_POINT('Ctrl Pts',(-9.03320343366227,10.5082450353975,
9.90114940024882));
#114060=CARTESIAN_POINT('Ctrl Pts',(-9.04704243294261,10.5092623069535,
9.88912639814773));
#114061=CARTESIAN_POINT('Ctrl Pts',(-9.06730356186042,10.5107128541953,
9.87218134444256));
#114062=CARTESIAN_POINT('Ctrl Pts',(-9.07354594457713,10.5111546165914,
9.86704790375476));
#114063=CARTESIAN_POINT('Ctrl Pts',(-9.08459627017407,10.5119277384135,
9.85811304372277));
#114064=CARTESIAN_POINT('Ctrl Pts',(-9.0893861276056,10.5122599671348,9.85428965856194));
#114065=CARTESIAN_POINT('Ctrl Pts',(-9.09932186413509,10.5129432493903,
9.84646037356761));
#114066=CARTESIAN_POINT('Ctrl Pts',(-9.10447079039932,10.5132941385571,
9.84245854898995));
#114067=CARTESIAN_POINT('Ctrl Pts',(-9.11774025550072,10.5141903622623,
9.83228685079056));
#114068=CARTESIAN_POINT('Ctrl Pts',(-9.12589892344178,10.5147337465359,
9.82616714538261));
#114069=CARTESIAN_POINT('Ctrl Pts',(-9.16066052573272,10.5170176290588,
9.80065635205338));
#114070=CARTESIAN_POINT('Ctrl Pts',(-9.18785073186588,10.518727202849,9.7820797579534));
#114071=CARTESIAN_POINT('Ctrl Pts',(-9.26286072789059,10.5232648462859,
9.73446234385364));
#114072=CARTESIAN_POINT('Ctrl Pts',(-9.31175694967316,10.5260344279026,
9.70721928502519));
#114073=CARTESIAN_POINT('Ctrl Pts',(-9.42756736872976,10.5323314608391,
9.6511318714039));
#114074=CARTESIAN_POINT('Ctrl Pts',(-9.49531067441672,10.5358258931188,
9.62435019068098));
#114075=CARTESIAN_POINT('Ctrl Pts',(-9.58394257400059,10.5404384128553,
9.5967423385813));
#114076=CARTESIAN_POINT('Ctrl Pts',(-9.60324376205152,10.541445604914,9.59116349853737));
#114077=CARTESIAN_POINT('Ctrl Pts',(-9.6520692012048,10.5440134904584,9.57813385293057));
#114078=CARTESIAN_POINT('Ctrl Pts',(-9.68172119537227,10.5455911574977,
9.57120416570205));
#114079=CARTESIAN_POINT('Ctrl Pts',(-9.71842248126392,10.547589436078,9.56382617077153));
#114080=CARTESIAN_POINT('Ctrl Pts',(-9.72528901580081,10.5479652438603,
9.56249694326973));
#114081=CARTESIAN_POINT('Ctrl Pts',(-9.73605562565912,10.5485579113282,
9.56049269492433));
#114082=CARTESIAN_POINT('Ctrl Pts',(-9.73994944954854,10.5487729497922,
9.55978417430872));
#114083=CARTESIAN_POINT('Ctrl Pts',(-9.74718033446681,10.5491736482781,
9.55849872164477));
#114084=CARTESIAN_POINT('Ctrl Pts',(-9.75051656309215,10.549359071667,9.55791757074044));
#114085=CARTESIAN_POINT('Ctrl Pts',(-9.75814559843241,10.5497843195902,
9.55661590504471));
#114086=CARTESIAN_POINT('Ctrl Pts',(-9.76243960950503,10.5500245567199,
9.55590296136369));
#114087=CARTESIAN_POINT('Ctrl Pts',(-9.77573787928642,10.5507711583569,
9.55375593873383));
#114088=CARTESIAN_POINT('Ctrl Pts',(-9.78475223407125,10.5512809367453,
9.55238686996278));
#114089=CARTESIAN_POINT('Ctrl Pts',(-9.80585124718539,10.5524817984529,
9.54938385014964));
#114090=CARTESIAN_POINT('Ctrl Pts',(-9.81794458374595,10.5531759606489,
9.54781655433849));
#114091=CARTESIAN_POINT('Ctrl Pts',(-9.86064193252219,10.5556441655955,
9.54282469042827));
#114092=CARTESIAN_POINT('Ctrl Pts',(-9.89133182094211,10.5574494886226,
9.54021522945709));
#114093=CARTESIAN_POINT('Ctrl Pts',(-10.0298816845532,10.565677567142,9.53282798844815));
#114094=CARTESIAN_POINT('Ctrl Pts',(-10.1380019555013,10.5722797398151,
9.53902589850794));
#114095=CARTESIAN_POINT('Ctrl Pts',(-10.2974345101372,10.5817390468098,
9.56603615990242));
#114096=CARTESIAN_POINT('Ctrl Pts',(-10.3498829700813,10.5848107273916,
9.57792317168964));
#114097=CARTESIAN_POINT('Ctrl Pts',(-10.4133282668786,10.5884707795145,
9.59602647142961));
#114098=CARTESIAN_POINT('Ctrl Pts',(-10.4250505772105,10.5891447511397,
9.59953081267335));
#114099=CARTESIAN_POINT('Ctrl Pts',(-10.443445483883,10.5901990097299,9.60528214637818));
#114100=CARTESIAN_POINT('Ctrl Pts',(-10.450147985461,10.5905824414117,9.60743094175544));
#114101=CARTESIAN_POINT('Ctrl Pts',(-10.4625053676953,10.5912881396837,
9.61149120941357));
#114102=CARTESIAN_POINT('Ctrl Pts',(-10.4681645331558,10.5916108390277,
9.61338907835271));
#114103=CARTESIAN_POINT('Ctrl Pts',(-10.4807084634067,10.592325117948,9.61768138496508));
#114104=CARTESIAN_POINT('Ctrl Pts',(-10.4875872948824,10.5927161363647,
9.62009275212421));
#114105=CARTESIAN_POINT('Ctrl Pts',(-10.5073945686856,10.5938402718558,
9.62720277703443));
#114106=CARTESIAN_POINT('Ctrl Pts',(-10.5202753378402,10.5945690895984,
9.63203251008392));
#114107=CARTESIAN_POINT('Ctrl Pts',(-10.5491868593215,10.596201072058,9.64334052751265));
#114108=CARTESIAN_POINT('Ctrl Pts',(-10.5651748641215,10.5971008121415,
9.64992276708801));
#114109=CARTESIAN_POINT('Ctrl Pts',(-10.6169903147784,10.6000118822921,
9.67233693302531));
#114110=CARTESIAN_POINT('Ctrl Pts',(-10.6523004538226,10.6019874194546,
9.68932434755603));
#114111=CARTESIAN_POINT('Ctrl Pts',(-10.7767544931489,10.6089925087812,
9.75547507805603));
#114112=CARTESIAN_POINT('Ctrl Pts',(-10.8613880590976,10.613818545891,9.8124820050933));
#114113=CARTESIAN_POINT('Ctrl Pts',(-10.948413448068,10.6194743121055,9.88533335293958));
#114114=CARTESIAN_POINT('Ctrl Pts',(-10.957315593808,10.6200620881367,9.89296944599265));
#114115=CARTESIAN_POINT('Ctrl Pts',(-10.9925372238763,10.6224290755521,
9.92392446333581));
#114116=CARTESIAN_POINT('Ctrl Pts',(-11.0181025219248,10.6242411757766,
9.94808004553598));
#114117=CARTESIAN_POINT('Ctrl Pts',(-11.0474368771963,10.6264706148856,
9.97786867090394));
#114118=CARTESIAN_POINT('Ctrl Pts',(-11.0520700761582,10.6268274276144,
9.98263820732939));
#114119=CARTESIAN_POINT('Ctrl Pts',(-11.0595970869691,10.6274151464101,
9.99049311281253));
#114120=CARTESIAN_POINT('Ctrl Pts',(-11.0625103580291,10.6276446230026,
9.99355979801825));
#114121=CARTESIAN_POINT('Ctrl Pts',(-11.0677266801538,10.6280592247461,
9.99909870501392));
#114122=CARTESIAN_POINT('Ctrl Pts',(-11.0700345072656,10.6282439836777,
10.0015663173252));
#114123=CARTESIAN_POINT('Ctrl Pts',(-11.0750923831634,10.6286518538625,
10.007012059954));
#114124=CARTESIAN_POINT('Ctrl Pts',(-11.0778385787115,10.6288752364172,
10.0099935965649));
#114125=CARTESIAN_POINT('Ctrl Pts',(-11.0857227775879,10.6295220387791,
10.0186251368294));
#114126=CARTESIAN_POINT('Ctrl Pts',(-11.0908289105967,10.6299477116908,
10.0243039128229));
#114127=CARTESIAN_POINT('Ctrl Pts',(-11.1286789884811,10.6331524387183,
10.0670672978851));
#114128=CARTESIAN_POINT('Ctrl Pts',(-11.1595653745561,10.6360461089173,
10.1057478429604));
#114129=CARTESIAN_POINT('Ctrl Pts',(-11.2312174537644,10.6433477311361,
10.205449198514));
#114130=CARTESIAN_POINT('Ctrl Pts',(-11.2694694780741,10.647798701241,10.268115548723));
#114131=CARTESIAN_POINT('Ctrl Pts',(-11.3404236409246,10.6570914808106,
10.4067918290544));
#114132=CARTESIAN_POINT('Ctrl Pts',(-11.3717157056356,10.661892724109,10.4832496120246));
#114133=CARTESIAN_POINT('Ctrl Pts',(-11.4000168564154,10.6671485043266,
10.5734665098075));
#114134=CARTESIAN_POINT('Ctrl Pts',(-11.403488030209,10.6678150472914,10.5850308712938));
#114135=CARTESIAN_POINT('Ctrl Pts',(-11.408922509258,10.6688960676021,10.6039847986157));
#114136=CARTESIAN_POINT('Ctrl Pts',(-11.4109716716786,10.6693132805952,
10.6113489719169));
#114137=CARTESIAN_POINT('Ctrl Pts',(-11.41453930508,10.6700574193959,10.6245703649181));
#114138=CARTESIAN_POINT('Ctrl Pts',(-11.4160793145276,10.6703850273874,
10.6304215468959));
#114139=CARTESIAN_POINT('Ctrl Pts',(-11.4192730698448,10.6710783970174,
10.642869144821));
#114140=CARTESIAN_POINT('Ctrl Pts',(-11.4209172168043,10.6714438463253,
10.6494678907394));
#114141=CARTESIAN_POINT('Ctrl Pts',(-11.424173231385,10.6721854758231,10.662935275096));
#114142=CARTESIAN_POINT('Ctrl Pts',(-11.4257815460902,10.6725615359051,
10.669804592818));
#114143=CARTESIAN_POINT('Ctrl Pts',(-11.4296786106541,10.6734979943037,
10.6870089995984));
#114144=CARTESIAN_POINT('Ctrl Pts',(-11.4319050426638,10.67405644641,10.6973578805117));
#114145=CARTESIAN_POINT('Ctrl Pts',(-11.4537097882804,10.6797822166669,
10.8043426556033));
#114146=CARTESIAN_POINT('Ctrl Pts',(-11.4635870590518,10.6846245035735,
10.9026959679584));
#114147=CARTESIAN_POINT('Ctrl Pts',(-11.4634994219804,10.6894249952545,
11.0013007162982));
#114148=CARTESIAN_POINT('Origin',(-10.,3.5,11.));
#114149=CARTESIAN_POINT('',(-11.4634998199575,11.2617878196045,10.9992740621286));
#114150=CARTESIAN_POINT('',(-11.4634998222683,11.1893449541571,10.999278736866));
#114151=CARTESIAN_POINT('',(-11.4635,3.5,11.));
#114152=CARTESIAN_POINT('',(-11.4634993682568,10.7605065214977,11.001312182958));
#114153=CARTESIAN_POINT('Ctrl Pts',(-11.463499819958,11.2617878197064,10.9992740641209));
#114154=CARTESIAN_POINT('Ctrl Pts',(-11.463486688228,11.2604341920573,10.9728002597134));
#114155=CARTESIAN_POINT('Ctrl Pts',(-11.4627552163876,11.2590556290495,
10.946333239001));
#114156=CARTESIAN_POINT('Ctrl Pts',(-11.4609407851069,11.257284080159,10.9132306704544));
#114157=CARTESIAN_POINT('Ctrl Pts',(-11.4605294202421,11.2569247662569,
10.9065617671658));
#114158=CARTESIAN_POINT('Ctrl Pts',(-11.4598066339438,11.2563526182091,
10.8960195233276));
#114159=CARTESIAN_POINT('Ctrl Pts',(-11.4595254219672,11.2561414065003,
10.8921441241544));
#114160=CARTESIAN_POINT('Ctrl Pts',(-11.458995493785,11.2557625509528,10.8852231000926));
#114161=CARTESIAN_POINT('Ctrl Pts',(-11.458752668362,11.2555952341647,10.8821770835459));
#114162=CARTESIAN_POINT('Ctrl Pts',(-11.4581475455987,11.255192765732,10.8748751451752));
#114163=CARTESIAN_POINT('Ctrl Pts',(-11.4577761565212,11.2549571182771,
10.8706200534682));
#114164=CARTESIAN_POINT('Ctrl Pts',(-11.4565913163249,11.2542382503158,
10.8576983509844));
#114165=CARTESIAN_POINT('Ctrl Pts',(-11.4557191796975,11.2537519611746,
10.8490374731997));
#114166=CARTESIAN_POINT('Ctrl Pts',(-11.4535165464869,11.2526152206947,
10.828962125839));
#114167=CARTESIAN_POINT('Ctrl Pts',(-11.4521287737384,11.2519621027094,
10.8175546258698));
#114168=CARTESIAN_POINT('Ctrl Pts',(-11.435861274341,11.2449234509118,10.6958132230162));
#114169=CARTESIAN_POINT('Ctrl Pts',(-11.4085727377921,11.2380905037844,
10.5875083579516));
#114170=CARTESIAN_POINT('Ctrl Pts',(-11.3407520148659,11.2266394173485,
10.4077650713213));
#114171=CARTESIAN_POINT('Ctrl Pts',(-11.3060214706851,11.2219404602744,
10.3346659737906));
#114172=CARTESIAN_POINT('Ctrl Pts',(-11.2593717792556,11.2167788150277,
10.2543725024596));
#114173=CARTESIAN_POINT('Ctrl Pts',(-11.2531856402008,11.2161131419785,
10.2440215566316));
#114174=CARTESIAN_POINT('Ctrl Pts',(-11.2428730993153,11.2150333031189,
10.2272406276176));
#114175=CARTESIAN_POINT('Ctrl Pts',(-11.2388231157101,11.2146164105612,
10.220764554406));
#114176=CARTESIAN_POINT('Ctrl Pts',(-11.2314755565732,11.2138727050138,
10.2092176120861));
#114177=CARTESIAN_POINT('Ctrl Pts',(-11.2281969143172,11.2135452118272,
10.2041349532428));
#114178=CARTESIAN_POINT('Ctrl Pts',(-11.2211650595449,11.212851943327,10.1933808855717));
#114179=CARTESIAN_POINT('Ctrl Pts',(-11.2174036261162,11.2124864812542,
10.1877150058878));
#114180=CARTESIAN_POINT('Ctrl Pts',(-11.2071862182944,11.2115079268949,
10.1725548359386));
#114181=CARTESIAN_POINT('Ctrl Pts',(-11.2006577174758,11.2108975438894,
10.163109851544));
#114182=CARTESIAN_POINT('Ctrl Pts',(-11.166537641028,11.2077811865274,10.1149684690307));
#114183=CARTESIAN_POINT('Ctrl Pts',(-11.1371828998453,11.2053429818794,
10.0775540605704));
#114184=CARTESIAN_POINT('Ctrl Pts',(-11.0355975914252,11.1975496823898,
9.96031396779354));
#114185=CARTESIAN_POINT('Ctrl Pts',(-10.9563891946588,11.192449698844,9.88701832105989));
#114186=CARTESIAN_POINT('Ctrl Pts',(-10.8478650472762,11.1857680377002,
9.80680872110096));
#114187=CARTESIAN_POINT('Ctrl Pts',(-10.8254154028199,11.1843985897977,
9.79117004353052));
#114188=CARTESIAN_POINT('Ctrl Pts',(-10.7794629744942,11.1815939499171,
9.76103616325597));
#114189=CARTESIAN_POINT('Ctrl Pts',(-10.7559622234764,11.1801588411624,
9.74655879875568));
#114190=CARTESIAN_POINT('Ctrl Pts',(-10.7262018665948,11.1783228534056,
9.72936669680408));
#114191=CARTESIAN_POINT('Ctrl Pts',(-10.7203125849238,11.1779586412921,
9.72601887034836));
#114192=CARTESIAN_POINT('Ctrl Pts',(-10.7109905627091,11.177380407447,9.72080496644957));
#114193=CARTESIAN_POINT('Ctrl Pts',(-10.7075731557772,11.1771680662359,
9.71891150086287));
#114194=CARTESIAN_POINT('Ctrl Pts',(-10.7014723129851,11.1767882703901,
9.71556309546341));
#114195=CARTESIAN_POINT('Ctrl Pts',(-10.6987918618229,11.1766211533441,
9.71410284200062));
#114196=CARTESIAN_POINT('Ctrl Pts',(-10.6923764086864,11.1762205830398,
9.7106338208467));
#114197=CARTESIAN_POINT('Ctrl Pts',(-10.6886372509974,11.1759866475075,
9.70863290623313));
#114198=CARTESIAN_POINT('Ctrl Pts',(-10.6773317683744,11.1752780470676,
9.70264613070868));
#114199=CARTESIAN_POINT('Ctrl Pts',(-10.6697392854091,11.174800437032,9.69871038231332));
#114200=CARTESIAN_POINT('Ctrl Pts',(-10.5893245488687,11.1697271998879,
9.65791561526222));
#114201=CARTESIAN_POINT('Ctrl Pts',(-10.5135813304267,11.1648299550675,
9.62714689682599));
#114202=CARTESIAN_POINT('Ctrl Pts',(-10.3256076031161,11.1529822048455,
9.56853033538366));
#114203=CARTESIAN_POINT('Ctrl Pts',(-10.2118479877965,11.1460881788344,
9.54732842820739));
#114204=CARTESIAN_POINT('Ctrl Pts',(-10.079020286721,11.138631551582,9.53852665513824));
#114205=CARTESIAN_POINT('Ctrl Pts',(-10.0612540913168,11.1376451475261,
9.53767427748808));
#114206=CARTESIAN_POINT('Ctrl Pts',(-10.0354956237449,11.1362303488594,
9.53690873264133));
#114207=CARTESIAN_POINT('Ctrl Pts',(-10.0275131285929,11.1357940343046,
9.53673685647315));
#114208=CARTESIAN_POINT('Ctrl Pts',(-10.0134188038962,11.1350273166918,
9.53654875956377));
#114209=CARTESIAN_POINT('Ctrl Pts',(-10.0073075799973,11.1346960871203,
9.5365054840304));
#114210=CARTESIAN_POINT('Ctrl Pts',(-9.99463846173659,11.1340118762913,
9.53649512885722));
#114211=CARTESIAN_POINT('Ctrl Pts',(-9.9880806911095,11.1336590812989,9.53653384530509));
#114212=CARTESIAN_POINT('Ctrl Pts',(-9.97115167042587,11.1327517492285,
9.53674759104382));
#114213=CARTESIAN_POINT('Ctrl Pts',(-9.96078152694503,11.1321992602464,
9.53698880483284));
#114214=CARTESIAN_POINT('Ctrl Pts',(-9.91584923270393,11.1298189020828,
9.53851204623405));
#114215=CARTESIAN_POINT('Ctrl Pts',(-9.88133471590067,11.1280254194898,
9.54090878174838));
#114216=CARTESIAN_POINT('Ctrl Pts',(-9.7869369309863,11.1231877165366,9.55083609028697));
#114217=CARTESIAN_POINT('Ctrl Pts',(-9.72738316798507,11.1202129159283,
9.56085002104142));
#114218=CARTESIAN_POINT('Ctrl Pts',(-9.57780438989927,11.1127159867484,
9.59562279055109));
#114219=CARTESIAN_POINT('Ctrl Pts',(-9.48922683467326,11.1082579249049,
9.62536100537308));
#114220=CARTESIAN_POINT('Ctrl Pts',(-9.381671753301,11.1022174118941,9.67331059672294));
#114221=CARTESIAN_POINT('Ctrl Pts',(-9.35951195405144,11.1009362820014,
9.68386569087924));
#114222=CARTESIAN_POINT('Ctrl Pts',(-9.33175289958555,11.0992718114994,
9.69795488141136));
#114223=CARTESIAN_POINT('Ctrl Pts',(-9.32589681106973,11.0989172385231,
9.70097707277241));
#114224=CARTESIAN_POINT('Ctrl Pts',(-9.31667281868704,11.0983529907968,
9.70581652888809));
#114225=CARTESIAN_POINT('Ctrl Pts',(-9.31329121891552,11.0981449001671,
9.70760766679776));
#114226=CARTESIAN_POINT('Ctrl Pts',(-9.30691021542978,11.0977498304209,
9.71101961847261));
#114227=CARTESIAN_POINT('Ctrl Pts',(-9.30390941756315,11.0975630210812,
9.71263766808647));
#114228=CARTESIAN_POINT('Ctrl Pts',(-9.29690441403648,11.0971245766201,
9.71644646388222));
#114229=CARTESIAN_POINT('Ctrl Pts',(-9.292904776117,11.0968724308582,9.7186454720495));
#114230=CARTESIAN_POINT('Ctrl Pts',(-9.27995131019711,11.096050096812,9.7258464279553));
#114231=CARTESIAN_POINT('Ctrl Pts',(-9.27103995960337,11.0954754543274,
9.73092368695006));
#114232=CARTESIAN_POINT('Ctrl Pts',(-9.22356472910915,11.0923690084629,
9.75863780076442));
#114233=CARTESIAN_POINT('Ctrl Pts',(-9.18600300180205,11.089751104733,9.78293793436466));
#114234=CARTESIAN_POINT('Ctrl Pts',(-9.06307401566891,11.0807723093504,
9.87070415891188));
#114235=CARTESIAN_POINT('Ctrl Pts',(-8.98351406272645,11.0742780520504,
9.94174716314356));
#114236=CARTESIAN_POINT('Ctrl Pts',(-8.90500709897132,11.0674243361306,
10.0289472606158));
#114237=CARTESIAN_POINT('Ctrl Pts',(-8.89775048206228,11.0667856677941,
10.037192187484));
#114238=CARTESIAN_POINT('Ctrl Pts',(-8.86291326084977,11.0636947874948,
10.0776841649977));
#114239=CARTESIAN_POINT('Ctrl Pts',(-8.83664955989742,11.0612883614971,
10.1110404866213));
#114240=CARTESIAN_POINT('Ctrl Pts',(-8.80512367001447,11.0582981947217,
10.1548749576329));
#114241=CARTESIAN_POINT('Ctrl Pts',(-8.79848783667515,11.0576624613002,
10.1643360045507));
#114242=CARTESIAN_POINT('Ctrl Pts',(-8.78811656242673,11.0566584047046,
10.179501825627));
#114243=CARTESIAN_POINT('Ctrl Pts',(-8.7843078245752,11.0562873465705,10.1851556852933));
#114244=CARTESIAN_POINT('Ctrl Pts',(-8.77753033831777,11.0556227662621,
10.1953697858876));
#114245=CARTESIAN_POINT('Ctrl Pts',(-8.77454727205529,11.0553287166808,
10.199920336548));
#114246=CARTESIAN_POINT('Ctrl Pts',(-8.76760944743998,11.0546411425273,
10.2106335501222));
#114247=CARTESIAN_POINT('Ctrl Pts',(-8.76367540416524,11.0542483837425,
10.2168094978812));
#114248=CARTESIAN_POINT('Ctrl Pts',(-8.75239663559079,11.0531137380059,
10.2348124995559));
#114249=CARTESIAN_POINT('Ctrl Pts',(-8.74517400192465,11.0523762798636,
10.2467153275152));
#114250=CARTESIAN_POINT('Ctrl Pts',(-8.68669847874528,11.0463091978923,
10.3462579244345));
#114251=CARTESIAN_POINT('Ctrl Pts',(-8.644521627876,11.0413258428021,10.438910970078));
#114252=CARTESIAN_POINT('Ctrl Pts',(-8.58149710500079,11.0316662114003,
10.6270770134347));
#114253=CARTESIAN_POINT('Ctrl Pts',(-8.5599268650995,11.0270009487026,10.7217791812591));
#114254=CARTESIAN_POINT('Ctrl Pts',(-8.54645992899512,11.0212975155907,
10.829171233828));
#114255=CARTESIAN_POINT('Ctrl Pts',(-8.54517820889322,11.0206931183749,
10.8404545646537));
#114256=CARTESIAN_POINT('Ctrl Pts',(-8.54358036214461,11.0198439921769,
10.8561472523417));
#114257=CARTESIAN_POINT('Ctrl Pts',(-8.54315268042422,11.0196050946766,
10.860545129269));
#114258=CARTESIAN_POINT('Ctrl Pts',(-8.54245076777175,11.0191919822457,
10.8681188170028));
#114259=CARTESIAN_POINT('Ctrl Pts',(-8.54216698201834,11.0190182896834,
10.8712937372095));
#114260=CARTESIAN_POINT('Ctrl Pts',(-8.54159341537822,11.0186526860205,
10.8779560335453));
#114261=CARTESIAN_POINT('Ctrl Pts',(-8.54130576819757,11.0184606539934,
10.8814435445598));
#114262=CARTESIAN_POINT('Ctrl Pts',(-8.54063058711665,11.0179877360115,
10.8900042957124));
#114263=CARTESIAN_POINT('Ctrl Pts',(-8.54025699883146,11.0177060951066,
10.8950785665774));
#114264=CARTESIAN_POINT('Ctrl Pts',(-8.53899101008997,11.016673968829,10.9135917653415));
#114265=CARTESIAN_POINT('Ctrl Pts',(-8.53825770550112,11.0159154072524,
10.9270404920041));
#114266=CARTESIAN_POINT('Ctrl Pts',(-8.53688261837224,11.0139905204385,
10.9608332978521));
#114267=CARTESIAN_POINT('Ctrl Pts',(-8.53647945555567,11.0128142154581,
10.981183866438));
#114268=CARTESIAN_POINT('Ctrl Pts',(-8.53664439499977,11.0036263761541,
11.1384106828293));
#114269=CARTESIAN_POINT('Ctrl Pts',(-8.55598728674533,10.9951654956004,
11.2745952142894));
#114270=CARTESIAN_POINT('Ctrl Pts',(-8.60585611403407,10.984762845462,11.447243828349));
#114271=CARTESIAN_POINT('Ctrl Pts',(-8.6195324964374,10.9823348338308,11.4878260064324));
#114272=CARTESIAN_POINT('Ctrl Pts',(-8.63914739316766,10.9793223389284,
11.538559808752));
#114273=CARTESIAN_POINT('Ctrl Pts',(-8.64345368037679,10.9786849015235,
11.5493164649263));
#114274=CARTESIAN_POINT('Ctrl Pts',(-8.65049843866856,10.9776787880916,
11.5663253015064));
#114275=CARTESIAN_POINT('Ctrl Pts',(-8.65315362717664,10.9773073578466,
11.5726112654904));
#114276=CARTESIAN_POINT('Ctrl Pts',(-8.65800453759039,10.9766424503777,
11.5838750073932));
#114277=CARTESIAN_POINT('Ctrl Pts',(-8.66018422395008,10.9763484425683,
11.588859518675));
#114278=CARTESIAN_POINT('Ctrl Pts',(-8.66535903324808,10.9756613984166,
11.6005157956232));
#114279=CARTESIAN_POINT('Ctrl Pts',(-8.66837648625373,10.9752691238937,
11.6071775285671));
#114280=CARTESIAN_POINT('Ctrl Pts',(-8.67726408030995,10.9741373172945,
11.6264140094053));
#114281=CARTESIAN_POINT('Ctrl Pts',(-8.68326338402909,10.9734021792358,
11.638928420044));
#114282=CARTESIAN_POINT('Ctrl Pts',(-8.73771368267025,10.9669722345414,
11.748485097245));
#114283=CARTESIAN_POINT('Ctrl Pts',(-8.7966351241764,10.9616788967025,11.839948049353));
#114284=CARTESIAN_POINT('Ctrl Pts',(-8.92164338210987,10.9520450975817,
11.9934738906188));
#114285=CARTESIAN_POINT('Ctrl Pts',(-8.98439921637841,10.947707690103,12.0575418234643));
#114286=CARTESIAN_POINT('Ctrl Pts',(-9.06155335046782,10.9423785132384,
12.1230707989617));
#114287=CARTESIAN_POINT('Ctrl Pts',(-9.07059419437932,10.9417539596014,
12.1305640029925));
#114288=CARTESIAN_POINT('Ctrl Pts',(-9.08320336986207,10.9408812575007,
12.1407612428869));
#114289=CARTESIAN_POINT('Ctrl Pts',(-9.08669564218362,10.9406393802955,
12.1435591035216));
#114290=CARTESIAN_POINT('Ctrl Pts',(-9.0927090094764,10.9402224924739,12.1483316435585));
#114291=CARTESIAN_POINT('Ctrl Pts',(-9.09522387665814,10.9400480263199,
12.1503141620051));
#114292=CARTESIAN_POINT('Ctrl Pts',(-9.10048980960202,10.9396824145588,
12.1544374468385));
#114293=CARTESIAN_POINT('Ctrl Pts',(-9.10324203174723,10.9394911585174,
12.1565766497872));
#114294=CARTESIAN_POINT('Ctrl Pts',(-9.10997556710577,10.9390228725697,
12.1617719007692));
#114295=CARTESIAN_POINT('Ctrl Pts',(-9.11396499369372,10.9387451204313,
12.1648173275915));
#114296=CARTESIAN_POINT('Ctrl Pts',(-9.12834970683843,10.9377427734411,
12.1756815951264));
#114297=CARTESIAN_POINT('Ctrl Pts',(-9.13883316314712,10.9370106842262,
12.1833820608782));
#114298=CARTESIAN_POINT('Ctrl Pts',(-9.16522244570663,10.9351667905506,
12.2022295545922));
#114299=CARTESIAN_POINT('Ctrl Pts',(-9.18124989695634,10.934045984839,12.2132014144969));
#114300=CARTESIAN_POINT('Ctrl Pts',(-9.2516714441834,10.9291332178608,12.2593786031975));
#114301=CARTESIAN_POINT('Ctrl Pts',(-9.30814976191267,10.9252265134849,
12.2912678320341));
#114302=CARTESIAN_POINT('Ctrl Pts',(-9.46142865058808,10.9149957445417,
12.3648625864945));
#114303=CARTESIAN_POINT('Ctrl Pts',(-9.56095668223373,10.9087372911465,
12.4000558950807));
#114304=CARTESIAN_POINT('Ctrl Pts',(-9.67955646900472,10.9019039766204,
12.4280838216257));
#114305=CARTESIAN_POINT('Ctrl Pts',(-9.69576530343403,10.9009822691528,
12.4316245105298));
#114306=CARTESIAN_POINT('Ctrl Pts',(-9.72077986417247,10.8995781108575,
12.4366446970227));
#114307=CARTESIAN_POINT('Ctrl Pts',(-9.72954441626644,10.8990895471695,
12.4383204274033));
#114308=CARTESIAN_POINT('Ctrl Pts',(-9.74386139923743,10.8982969299803,
12.4409222546615));
#114309=CARTESIAN_POINT('Ctrl Pts',(-9.74940472577557,10.8979913686292,
12.4418966455825));
#114310=CARTESIAN_POINT('Ctrl Pts',(-9.76107425792123,10.897350860781,12.4438785554664));
#114311=CARTESIAN_POINT('Ctrl Pts',(-9.76720154189295,10.8970161377078,
12.4448791204439));
#114312=CARTESIAN_POINT('Ctrl Pts',(-9.7819178952353,10.8962159280863,12.447186208087));
#114313=CARTESIAN_POINT('Ctrl Pts',(-9.79051264885204,10.8957516170809,
12.448455308037));
#114314=CARTESIAN_POINT('Ctrl Pts',(-9.82033863693388,10.8941504550591,
12.4525883771122));
#114315=CARTESIAN_POINT('Ctrl Pts',(-9.84162161506871,10.8930256838134,
12.4550627297469));
#114316=CARTESIAN_POINT('Ctrl Pts',(-9.98122805657438,10.8857496251962,
12.4681937372834));
#114317=CARTESIAN_POINT('Ctrl Pts',(-10.1004149022225,10.8800618910277,
12.4648766738575));
#114318=CARTESIAN_POINT('Ctrl Pts',(-10.2905829711886,10.8706621499727,
12.4362440704026));
#114319=CARTESIAN_POINT('Ctrl Pts',(-10.3623346248171,10.8670237781975,
12.4198403453594));
#114320=CARTESIAN_POINT('Ctrl Pts',(-10.4402736824534,10.8626843353073,
12.3957280706299));
#114321=CARTESIAN_POINT('Ctrl Pts',(-10.4479859292538,10.8622505778353,
12.3932718198192));
#114322=CARTESIAN_POINT('Ctrl Pts',(-10.4596694780708,10.8615862739666,
12.3894437268116));
#114323=CARTESIAN_POINT('Ctrl Pts',(-10.4636560249375,10.8613583279926,
12.3881185067185));
#114324=CARTESIAN_POINT('Ctrl Pts',(-10.4708365224507,10.8609453545981,
12.3856971609403));
#114325=CARTESIAN_POINT('Ctrl Pts',(-10.4740324410999,10.8607606803902,
12.3846071273428));
#114326=CARTESIAN_POINT('Ctrl Pts',(-10.4810783263755,10.8603516107149,
12.3821767297007));
#114327=CARTESIAN_POINT('Ctrl Pts',(-10.4849264332692,10.860126932439,12.3808313516597));
#114328=CARTESIAN_POINT('Ctrl Pts',(-10.4960733290925,10.8594725318554,
12.3768818236513));
#114329=CARTESIAN_POINT('Ctrl Pts',(-10.5033570048102,10.8590404755058,
12.3742357965485));
#114330=CARTESIAN_POINT('Ctrl Pts',(-10.5524208213832,10.8561015739289,
12.3559694179628));
#114331=CARTESIAN_POINT('Ctrl Pts',(-10.5934856823278,10.8535021285129,
12.3385050893608));
#114332=CARTESIAN_POINT('Ctrl Pts',(-10.7403409264512,10.8438446787764,
12.2679620747211));
#114333=CARTESIAN_POINT('Ctrl Pts',(-10.8404063684241,10.8365963249241,
12.2039746619075));
#114334=CARTESIAN_POINT('Ctrl Pts',(-10.9664515190271,10.8271130626593,
12.0999261247623));
#114335=CARTESIAN_POINT('Ctrl Pts',(-10.9998867756579,10.824550616811,12.069622861117));
#114336=CARTESIAN_POINT('Ctrl Pts',(-11.0401159386909,10.8214075610566,
12.0296243202608));
#114337=CARTESIAN_POINT('Ctrl Pts',(-11.0482623384985,10.8207677107044,
12.0213292747129));
#114338=CARTESIAN_POINT('Ctrl Pts',(-11.0610838036623,10.819754997594,12.0079588281649));
#114339=CARTESIAN_POINT('Ctrl Pts',(-11.0658231988062,10.8193793845616,
12.0029460348501));
#114340=CARTESIAN_POINT('Ctrl Pts',(-11.0746029278732,10.8186811055779,
11.9935273169167));
#114341=CARTESIAN_POINT('Ctrl Pts',(-11.0786520382124,10.8183580718146,
11.9891298013773));
#114342=CARTESIAN_POINT('Ctrl Pts',(-11.0876951689677,10.8176343012436,
11.9791869876923));
#114343=CARTESIAN_POINT('Ctrl Pts',(-11.0926739677109,10.8172342031675,
11.9736280298675));
#114344=CARTESIAN_POINT('Ctrl Pts',(-11.1066701655776,10.8161046484279,
11.9577583258368));
#114345=CARTESIAN_POINT('Ctrl Pts',(-11.1155857627045,10.8153793567944,
11.9473585851255));
#114346=CARTESIAN_POINT('Ctrl Pts',(-11.164933030371,10.8113291240717,11.888133842599));
#114347=CARTESIAN_POINT('Ctrl Pts',(-11.2023069099331,10.8081272035812,
11.8368452430039));
#114348=CARTESIAN_POINT('Ctrl Pts',(-11.2661724462096,10.802227944451,11.7360484391955));
#114349=CARTESIAN_POINT('Ctrl Pts',(-11.2933729088438,10.7995195818688,
11.6871292739145));
#114350=CARTESIAN_POINT('Ctrl Pts',(-11.3295642918049,10.7954671879514,
11.6122366278136));
#114351=CARTESIAN_POINT('Ctrl Pts',(-11.3407336662317,10.7941360479663,
11.5873738865482));
#114352=CARTESIAN_POINT('Ctrl Pts',(-11.3729925052898,10.7899912941477,
11.5098443459131));
#114353=CARTESIAN_POINT('Ctrl Pts',(-11.3917176598579,10.7871356946076,
11.4562568800924));
#114354=CARTESIAN_POINT('Ctrl Pts',(-11.4094933035069,10.783690734242,11.3939868318368));
#114355=CARTESIAN_POINT('Ctrl Pts',(-11.4116381353588,10.7832594743773,
11.3862314918515));
#114356=CARTESIAN_POINT('Ctrl Pts',(-11.4148026004861,10.7825982482181,
11.3744107566704));
#114357=CARTESIAN_POINT('Ctrl Pts',(-11.4158689356968,10.782370846197,11.3703578932564));
#114358=CARTESIAN_POINT('Ctrl Pts',(-11.4177629442364,10.7819584288677,
11.363031520339));
#114359=CARTESIAN_POINT('Ctrl Pts',(-11.418596711397,10.7817737620087,11.3597596708969));
#114360=CARTESIAN_POINT('Ctrl Pts',(-11.4204143973771,10.781364182019,11.3525221746251));
#114361=CARTESIAN_POINT('Ctrl Pts',(-11.4213930240943,10.7811389816206,
11.3485553243097));
#114362=CARTESIAN_POINT('Ctrl Pts',(-11.4241900704397,10.7804815795621,
11.3370098451807));
#114363=CARTESIAN_POINT('Ctrl Pts',(-11.4259645492666,10.7800470117977,
11.3294208422403));
#114364=CARTESIAN_POINT('Ctrl Pts',(-11.4317882136537,10.77856014688,11.3035853885632));
#114365=CARTESIAN_POINT('Ctrl Pts',(-11.4355483030422,10.7774938560526,
11.2852763272408));
#114366=CARTESIAN_POINT('Ctrl Pts',(-11.4552056333645,10.771268744215,11.1792968508592));
#114367=CARTESIAN_POINT('Ctrl Pts',(-11.4634195301979,10.765851273268,11.0903985669709));
#114368=CARTESIAN_POINT('Ctrl Pts',(-11.4634994116541,10.7605064521335,
11.0013122835481));
#114369=CARTESIAN_POINT('Ctrl Pts',(-11.4634994117402,10.7605064463713,
11.0013121875042));
#114370=CARTESIAN_POINT('Ctrl Pts',(-11.4634998039174,10.7604802041083,
11.0008747873294));
#114371=CARTESIAN_POINT('Ctrl Pts',(-11.4635,10.7604539637884,11.0004373914791));
#114372=CARTESIAN_POINT('Ctrl Pts',(-11.4635,10.7604277254418,11.0000000000833));
#114373=CARTESIAN_POINT('Ctrl Pts',(-11.463499418515,10.6893450235318,11.0013046096532));
#114374=CARTESIAN_POINT('Ctrl Pts',(-11.4634349907531,10.6932747544557,
11.0735790956281));
#114375=CARTESIAN_POINT('Ctrl Pts',(-11.4580128964482,10.6972044853797,
11.1456191271162));
#114376=CARTESIAN_POINT('Ctrl Pts',(-11.4473590059667,10.7011342163037,
11.2167582936063));
#114377=CARTESIAN_POINT('Ctrl Pts',(-11.4406841404891,10.7035962676385,
11.2613283375106));
#114378=CARTESIAN_POINT('Ctrl Pts',(-11.4319566126795,10.7060583189733,
11.3055453362204));
#114379=CARTESIAN_POINT('Ctrl Pts',(-11.4212166274608,10.7085203703081,
11.3492499789963));
#114380=CARTESIAN_POINT('Ctrl Pts',(-11.4080854742713,10.7115305768008,
11.4026850953113));
#114381=CARTESIAN_POINT('Ctrl Pts',(-11.3919089668557,10.7145407832936,
11.4554908217744));
#114382=CARTESIAN_POINT('Ctrl Pts',(-11.3727649466491,10.7175509897864,
11.5072954279822));
#114383=CARTESIAN_POINT('Ctrl Pts',(-11.3536549346268,10.7205558488309,
11.5590080064665));
#114384=CARTESIAN_POINT('Ctrl Pts',(-11.3315880529432,10.7235607078754,
11.609722502667));
#114385=CARTESIAN_POINT('Ctrl Pts',(-11.3066923639379,10.72656556692,11.6590806597272));
#114386=CARTESIAN_POINT('Ctrl Pts',(-11.2818212921532,10.729567454716,11.7083900107215));
#114387=CARTESIAN_POINT('Ctrl Pts',(-11.2541271907677,10.732569342512,11.7563452101873));
#114388=CARTESIAN_POINT('Ctrl Pts',(-11.2237861156574,10.7355712303081,
11.8026081192737));
#114389=CARTESIAN_POINT('Ctrl Pts',(-11.1934630601116,10.738571335283,11.8488435528187));
#114390=CARTESIAN_POINT('Ctrl Pts',(-11.1604964357665,10.7415714402579,
11.8933882473642));
#114391=CARTESIAN_POINT('Ctrl Pts',(-11.125106966386,10.7445715452328,11.9359308543849));
#114392=CARTESIAN_POINT('Ctrl Pts',(-11.0897245398217,10.7475710531603,
11.9784649950521));
#114393=CARTESIAN_POINT('Ctrl Pts',(-11.0519205633224,10.7505705610879,
12.0189974337215));
#114394=CARTESIAN_POINT('Ctrl Pts',(-11.011956158834,10.7535700690155,12.0572497257498));
#114395=CARTESIAN_POINT('Ctrl Pts',(-10.9719550224031,10.7565723338402,
12.0955371760898));
#114396=CARTESIAN_POINT('Ctrl Pts',(-10.9297898731728,10.7595745986649,
12.131539926898));
#114397=CARTESIAN_POINT('Ctrl Pts',(-10.8857577661469,10.7625768634896,
12.1650173516778));
#114398=CARTESIAN_POINT('Ctrl Pts',(-10.841705604808,10.7655804956883,12.198510023667));
#114399=CARTESIAN_POINT('Ctrl Pts',(-10.7957852292608,10.768584127887,12.2294747811257));
#114400=CARTESIAN_POINT('Ctrl Pts',(-10.748323061093,10.7715877600857,12.2577141353409));
#114401=CARTESIAN_POINT('Ctrl Pts',(-10.7007713900644,10.774597056452,12.2860067425593));
#114402=CARTESIAN_POINT('Ctrl Pts',(-10.6516725878829,10.7776063528183,
12.3115634352269));
#114403=CARTESIAN_POINT('Ctrl Pts',(-10.6013770268355,10.7806156491846,
12.3342330836831));
#114404=CARTESIAN_POINT('Ctrl Pts',(-10.5630015058961,10.7829117427824,
12.351530028998));
#114405=CARTESIAN_POINT('Ctrl Pts',(-10.5239297800624,10.7852078363802,
12.3671471852995));
#114406=CARTESIAN_POINT('Ctrl Pts',(-10.4843234063868,10.787503929978,12.3810369611368));
#114407=CARTESIAN_POINT('Ctrl Pts',(-10.4323989712049,10.7905141364707,
12.3992466253454));
#114408=CARTESIAN_POINT('Ctrl Pts',(-10.3793371053808,10.7935243429634,
12.414562059867));
#114409=CARTESIAN_POINT('Ctrl Pts',(-10.32549164717,10.7965345494561,12.426845274591));
#114410=CARTESIAN_POINT('Ctrl Pts',(-10.2717418421318,10.7995394085005,
12.4391066689331));
#114411=CARTESIAN_POINT('Ctrl Pts',(-10.217211717851,10.8025442675449,12.4483464166516));
#114412=CARTESIAN_POINT('Ctrl Pts',(-10.1622712787386,10.8055491265894,
12.4544759475827));
#114413=CARTESIAN_POINT('Ctrl Pts',(-10.107385165534,10.8085510143854,12.4605994175441));
#114414=CARTESIAN_POINT('Ctrl Pts',(-10.0520900634723,10.8115529021813,
12.4636187047463));
#114415=CARTESIAN_POINT('Ctrl Pts',(-9.99676536154247,10.8145547899773,
12.4634964253848));
#114416=CARTESIAN_POINT('Ctrl Pts',(-9.94147351695289,10.8175548949522,
12.463374218645));
#114417=CARTESIAN_POINT('Ctrl Pts',(-9.88615263436755,10.820554999927,12.4601141446112));
#114418=CARTESIAN_POINT('Ctrl Pts',(-9.83118408216089,10.8235551049018,
12.453730867762));
#114419=CARTESIAN_POINT('Ctrl Pts',(-9.77622646918038,10.8265546128293,
12.4473488612412));
#114420=CARTESIAN_POINT('Ctrl Pts',(-9.72162157159207,10.8295541207569,
12.4378449471583));
#114421=CARTESIAN_POINT('Ctrl Pts',(-9.66774528388968,10.8325536286844,
12.425285604229));
#114422=CARTESIAN_POINT('Ctrl Pts',(-9.61381947760378,10.835555893509,12.4127147178008));
#114423=CARTESIAN_POINT('Ctrl Pts',(-9.56062413452305,10.8385581583337,
12.3970829120905));
#114424=CARTESIAN_POINT('Ctrl Pts',(-9.50852311948919,10.8415604231584,
12.3785074268655));
#114425=CARTESIAN_POINT('Ctrl Pts',(-9.45639837517843,10.844564055357,12.3599234814823));
#114426=CARTESIAN_POINT('Ctrl Pts',(-9.40536943985125,10.8475676875557,
12.3383933896544));
#114427=CARTESIAN_POINT('Ctrl Pts',(-9.35578010493267,10.8505713197543,
12.3140825608764));
#114428=CARTESIAN_POINT('Ctrl Pts',(-9.30609725580016,10.8535806161206,
12.2897258874011));
#114429=CARTESIAN_POINT('Ctrl Pts',(-9.25785989153677,10.8565899124869,
12.2625782612703));
#114430=CARTESIAN_POINT('Ctrl Pts',(-9.21138607246561,10.8595992088531,
12.2328504870011));
#114431=CARTESIAN_POINT('Ctrl Pts',(-9.17592654124189,10.8618953024515,
12.2101681905818));
#114432=CARTESIAN_POINT('Ctrl Pts',(-9.14149316789575,10.8641913960498,
12.185984763789));
#114433=CARTESIAN_POINT('Ctrl Pts',(-9.10821410804107,10.8664874896482,
12.1604094850108));
#114434=CARTESIAN_POINT('Ctrl Pts',(-9.06458485785984,10.8694976961408,
12.1268799850447));
#114435=CARTESIAN_POINT('Ctrl Pts',(-9.02275759696782,10.8725079026334,
12.0908160919466));
#114436=CARTESIAN_POINT('Ctrl Pts',(-8.98304127681541,10.875518109126,12.0524386943375));
#114437=CARTESIAN_POINT('Ctrl Pts',(-8.94339551028357,10.8785229681704,
12.0141294718347));
#114438=CARTESIAN_POINT('Ctrl Pts',(-8.9058536193491,10.8815278272147,11.9735152647533));
#114439=CARTESIAN_POINT('Ctrl Pts',(-8.8706920063438,10.8845326862591,11.9308575108276));
#114440=CARTESIAN_POINT('Ctrl Pts',(-8.8355651616545,10.887534574055,11.8882419375115));
#114441=CARTESIAN_POINT('Ctrl Pts',(-8.80281426664224,10.8905364618508,
11.8435872257451));
#114442=CARTESIAN_POINT('Ctrl Pts',(-8.77267798871069,10.8935383496467,
11.7971906488443));
#114443=CARTESIAN_POINT('Ctrl Pts',(-8.74255960871446,10.8965384546215,
11.7508216268702));
#114444=CARTESIAN_POINT('Ctrl Pts',(-8.7150530550755,10.8995385595962,11.7027132321823));
#114445=CARTESIAN_POINT('Ctrl Pts',(-8.69035449104467,10.9025386645709,
11.6531928435563));
#114446=CARTESIAN_POINT('Ctrl Pts',(-8.66566084224569,10.9055381724983,
11.6036823099239));
#114447=CARTESIAN_POINT('Ctrl Pts',(-8.64377430882604,10.9085376804257,
11.5527608127128));
#114448=CARTESIAN_POINT('Ctrl Pts',(-8.62484467216533,10.9115371883532,
11.5007794667595));
#114449=CARTESIAN_POINT('Ctrl Pts',(-8.60589763696374,10.9145394531777,
11.4487503438948));
#114450=CARTESIAN_POINT('Ctrl Pts',(-8.58991310925893,10.9175417180023,
11.3956599233924));
#114451=CARTESIAN_POINT('Ctrl Pts',(-8.57699178734229,10.9205439828268,
11.3418769906102));
#114452=CARTESIAN_POINT('Ctrl Pts',(-8.56406458044193,10.9235476150254,
11.2880695625259));
#114453=CARTESIAN_POINT('Ctrl Pts',(-8.55420345460581,10.9265512472239,
11.2335695139773));
#114454=CARTESIAN_POINT('Ctrl Pts',(-8.54745779859224,10.9295548794225,
11.1787551485399));
#114455=CARTESIAN_POINT('Ctrl Pts',(-8.54069942180473,10.9325641757886,
11.1238374156686));
#114456=CARTESIAN_POINT('Ctrl Pts',(-8.53706828588017,10.9355734721548,
11.0686047100736));
#114457=CARTESIAN_POINT('Ctrl Pts',(-8.5365617013168,10.938582768521,11.0134385991544));
#114458=CARTESIAN_POINT('Ctrl Pts',(-8.53617517721555,10.9408788621201,
10.9713468478755));
#114459=CARTESIAN_POINT('Ctrl Pts',(-8.5376065868234,10.9431749557192,10.9292939478672));
#114460=CARTESIAN_POINT('Ctrl Pts',(-8.54083446443999,10.9454710493182,
10.8874469465813));
#114461=CARTESIAN_POINT('Ctrl Pts',(-8.54506625105535,10.9484812558113,
10.832585021512));
#114462=CARTESIAN_POINT('Ctrl Pts',(-8.55240528538672,10.9514914623044,
10.7778468929808));
#114463=CARTESIAN_POINT('Ctrl Pts',(-8.56283545473865,10.9545016687974,
10.7236120121211));
#114464=CARTESIAN_POINT('Ctrl Pts',(-8.57324709553083,10.9575065278422,
10.6694734762196));
#114465=CARTESIAN_POINT('Ctrl Pts',(-8.58673887504706,10.960511386887,10.6158369282496));
#114466=CARTESIAN_POINT('Ctrl Pts',(-8.60324293386438,10.9635162459319,
10.5630767250418));
#114467=CARTESIAN_POINT('Ctrl Pts',(-8.61973067322752,10.9665181337282,
10.5103686918928));
#114468=CARTESIAN_POINT('Ctrl Pts',(-8.63922463455454,10.9695200215245,
10.4585357884465));
#114469=CARTESIAN_POINT('Ctrl Pts',(-8.66160632448387,10.9725219093209,
10.4079403582928));
#114470=CARTESIAN_POINT('Ctrl Pts',(-8.68397472192765,10.9755220142961,
10.3573749767649));
#114471=CARTESIAN_POINT('Ctrl Pts',(-8.70922723546476,10.9785221192713,
10.3080460938113));
#114472=CARTESIAN_POINT('Ctrl Pts',(-8.73719692958272,10.9815222242465,
10.260296914063));
#114473=CARTESIAN_POINT('Ctrl Pts',(-8.76516105748513,10.9845217321743,
10.2125572368222));
#114474=CARTESIAN_POINT('Ctrl Pts',(-8.79584102530502,10.9875212401022,
10.1663970938549));
#114475=CARTESIAN_POINT('Ctrl Pts',(-8.82902466977638,10.9905207480301,
10.1221338222669));
#114476=CARTESIAN_POINT('Ctrl Pts',(-8.86223881388195,10.9935230128551,
10.077829867577));
#114477=CARTESIAN_POINT('Ctrl Pts',(-8.89796091461215,10.9965252776801,
10.0354266908642));
#114478=CARTESIAN_POINT('Ctrl Pts',(-8.93593718392468,10.9995275425051,
9.9952101844436));
#114479=CARTESIAN_POINT('Ctrl Pts',(-8.97393074943399,11.0025311747041,
9.95497536151579));
#114480=CARTESIAN_POINT('Ctrl Pts',(-9.01418014565303,11.0055348069031,
9.91692955754966));
#114481=CARTESIAN_POINT('Ctrl Pts',(-9.05639556972368,11.0085384391021,
9.88132089982743));
#114482=CARTESIAN_POINT('Ctrl Pts',(-9.09869060248836,11.0115477354687,
9.84564509227075));
#114483=CARTESIAN_POINT('Ctrl Pts',(-9.14295864597717,11.0145570318353,
9.8124159297475));
#114484=CARTESIAN_POINT('Ctrl Pts',(-9.18887869987918,11.0175663282019,
9.78183971231602));
#114485=CARTESIAN_POINT('Ctrl Pts',(-9.22391570814423,11.0198624217974,
9.75851005366304));
#114486=CARTESIAN_POINT('Ctrl Pts',(-9.25991380500009,11.0221585153929,
9.73672399505271));
#114487=CARTESIAN_POINT('Ctrl Pts',(-9.29672136993095,11.0244546089884,
9.71655486346778));
#114488=CARTESIAN_POINT('Ctrl Pts',(-9.34497653302352,11.0274648154808,
9.69011288786048));
#114489=CARTESIAN_POINT('Ctrl Pts',(-9.39482634721519,11.0304750219732,
9.66634063167969));
#114490=CARTESIAN_POINT('Ctrl Pts',(-9.44594424770867,11.0334852284657,
9.64543199751622));
#114491=CARTESIAN_POINT('Ctrl Pts',(-9.49697134036953,11.0364900875099,
9.62456050626616));
#114492=CARTESIAN_POINT('Ctrl Pts',(-9.54926156404086,11.039494946554,9.60654274003543));
#114493=CARTESIAN_POINT('Ctrl Pts',(-9.60246433689903,11.0424998055982,
9.59152648354225));
#114494=CARTESIAN_POINT('Ctrl Pts',(-9.65561450207914,11.045501693394,9.57652507534258));
#114495=CARTESIAN_POINT('Ctrl Pts',(-9.70967492321259,11.0485035811897,
9.56451944026266));
#114496=CARTESIAN_POINT('Ctrl Pts',(-9.76427740368708,11.0515054689854,
9.55560839534858));
#114497=CARTESIAN_POINT('Ctrl Pts',(-9.81884745574875,11.05450557396,9.54670264270402));
#114498=CARTESIAN_POINT('Ctrl Pts',(-9.87395840891588,11.0575056789346,
9.54088792230632));
#114499=CARTESIAN_POINT('Ctrl Pts',(-9.92923161693159,11.0605057839091,
9.53821202428058));
#114500=CARTESIAN_POINT('Ctrl Pts',(-9.984493825092,11.0635052918364,9.53553665878212));
#114501=CARTESIAN_POINT('Ctrl Pts',(-10.0399176968041,11.0665047997637,
9.53599890063128));
#114502=CARTESIAN_POINT('Ctrl Pts',(-10.0951215276541,11.0695043076909,
9.53959452720255));
#114503=CARTESIAN_POINT('Ctrl Pts',(-10.1503760972545,11.0725065725153,
9.54319345857343));
#114504=CARTESIAN_POINT('Ctrl Pts',(-10.2054096938424,11.0755088373398,
9.54993149399967));
#114505=CARTESIAN_POINT('Ctrl Pts',(-10.2598441946035,11.0785111021642,
9.55975236694141));
#114506=CARTESIAN_POINT('Ctrl Pts',(-10.3143034874218,11.0815147343626,
9.56957771277516));
#114507=CARTESIAN_POINT('Ctrl Pts',(-10.3681626260665,11.084518366561,9.58248857172123));
#114508=CARTESIAN_POINT('Ctrl Pts',(-10.4210554282106,11.0875219987594,
9.59837787675339));
#114509=CARTESIAN_POINT('Ctrl Pts',(-10.4740479741572,11.0905312951255,
9.61429714540322));
#114510=CARTESIAN_POINT('Ctrl Pts',(-10.5260700457833,11.0935405914915,
9.63320589943068));
#114511=CARTESIAN_POINT('Ctrl Pts',(-10.576773436003,11.0965498878575,9.65494808519475));
#114512=CARTESIAN_POINT('Ctrl Pts',(-10.6154601307107,11.0988459814578,
9.67153737635038));
#114513=CARTESIAN_POINT('Ctrl Pts',(-10.6533794910279,11.1011420750581,
9.6897751790565));
#114514=CARTESIAN_POINT('Ctrl Pts',(-10.6903872410026,11.1034381686584,
9.70957460213277));
#114515=CARTESIAN_POINT('Ctrl Pts',(-10.7389048490023,11.1064483751505,
9.73553188535293));
#114516=CARTESIAN_POINT('Ctrl Pts',(-10.7860583777846,11.1094585816426,
9.76428373505595));
#114517=CARTESIAN_POINT('Ctrl Pts',(-10.8315069607238,11.1124687881346,
9.79566266176466));
#114518=CARTESIAN_POINT('Ctrl Pts',(-10.8768748070272,11.1154736471784,
9.82698584572369));
#114519=CARTESIAN_POINT('Ctrl Pts',(-10.9205432869829,11.1184785062222,
9.86092654767628));
#114520=CARTESIAN_POINT('Ctrl Pts',(-10.9621970268473,11.121483365266,9.8972719593997));
#114521=CARTESIAN_POINT('Ctrl Pts',(-11.0038095788859,11.1244852530614,
9.93358143224962));
#114522=CARTESIAN_POINT('Ctrl Pts',(-11.0434109413571,11.1274871408567,
9.97229055903382));
#114523=CARTESIAN_POINT('Ctrl Pts',(-11.0807171191185,11.1304890286521,
10.0131450165074));
#114524=CARTESIAN_POINT('Ctrl Pts',(-11.1180011407411,11.1334891336262,
10.0539752105188));
#114525=CARTESIAN_POINT('Ctrl Pts',(-11.1529923240554,11.1364892386004,
10.0969478206531));
#114526=CARTESIAN_POINT('Ctrl Pts',(-11.1854436932004,11.1394893435746,
10.1417718833251));
#114527=CARTESIAN_POINT('Ctrl Pts',(-11.2178886042371,11.1424888515015,
10.1865870256137));
#114528=CARTESIAN_POINT('Ctrl Pts',(-11.2477943954007,11.1454883594283,
10.2332524611863));
#114529=CARTESIAN_POINT('Ctrl Pts',(-11.2749559756063,11.1484878673552,
10.2814462370387));
#114530=CARTESIAN_POINT('Ctrl Pts',(-11.3021425204678,11.1514901321792,
10.3296843085845));
#114531=CARTESIAN_POINT('Ctrl Pts',(-11.326579555432,11.1544923970032,10.3794530658141));
#114532=CARTESIAN_POINT('Ctrl Pts',(-11.3481075293614,11.1574946618272,
10.4304051095039));
#114533=CARTESIAN_POINT('Ctrl Pts',(-11.3696453081526,11.1604982940252,
10.4813803591746));
#114534=CARTESIAN_POINT('Ctrl Pts',(-11.3882712068658,11.1635019262232,
10.5335394714238));
#114535=CARTESIAN_POINT('Ctrl Pts',(-11.4038747417405,11.1665055584212,
10.5865172802847));
#114536=CARTESIAN_POINT('Ctrl Pts',(-11.4195077013352,11.1695148547868,
10.6395949932514));
#114537=CARTESIAN_POINT('Ctrl Pts',(-11.4321067910242,11.1725241511524,
10.6934939714734));
#114538=CARTESIAN_POINT('Ctrl Pts',(-11.4416123738597,11.175533447518,10.7478373272378));
#114539=CARTESIAN_POINT('Ctrl Pts',(-11.4488651350685,11.1778295411215,
10.7893013162918));
#114540=CARTESIAN_POINT('Ctrl Pts',(-11.4543180078065,11.180125634725,10.8310237505242));
#114541=CARTESIAN_POINT('Ctrl Pts',(-11.4579648995368,11.1824217283285,
10.8728363191844));
#114542=CARTESIAN_POINT('Ctrl Pts',(-11.4616302923563,11.1847294702714,
10.9148610076761));
#114543=CARTESIAN_POINT('Ctrl Pts',(-11.4634790087263,11.1870372122142,
10.9570464174956));
#114544=CARTESIAN_POINT('Ctrl Pts',(-11.4634998222683,11.1893449541571,
10.999278736866));
#114545=CARTESIAN_POINT('Origin',(-10.,3.5,11.));
#114546=CARTESIAN_POINT('',(-11.4634998686003,11.759483043376,10.9993798331215));
#114547=CARTESIAN_POINT('',(-11.4634998405534,11.6905473354117,10.9993168449445));
#114548=CARTESIAN_POINT('',(-11.4635,3.5,11.));
#114549=CARTESIAN_POINT('Ctrl Pts',(-11.4634998686003,11.759483043376,10.9993798331215));
#114550=CARTESIAN_POINT('Ctrl Pts',(-11.4634424942562,11.7525188724877,
10.863985074265));
#114551=CARTESIAN_POINT('Ctrl Pts',(-11.4445984465822,11.7461686400878,
10.7292564909312));
#114552=CARTESIAN_POINT('Ctrl Pts',(-11.3938575632165,11.7369685184196,
10.5511426273315));
#114553=CARTESIAN_POINT('Ctrl Pts',(-11.3777805713092,11.7344413008791,
10.5039842588742));
#114554=CARTESIAN_POINT('Ctrl Pts',(-11.3565020214225,11.7313814454091,
10.4506431739692));
#114555=CARTESIAN_POINT('Ctrl Pts',(-11.3536148451146,11.7309713329516,
10.443567162624));
#114556=CARTESIAN_POINT('Ctrl Pts',(-11.3491115253287,11.730338786047,10.4327727284323));
#114557=CARTESIAN_POINT('Ctrl Pts',(-11.3475350862997,11.7301186425966,
10.4290377632698));
#114558=CARTESIAN_POINT('Ctrl Pts',(-11.3446168045301,11.7297133682378,
10.4222030565607));
#114559=CARTESIAN_POINT('Ctrl Pts',(-11.3432797318978,11.7295285212857,
10.4191013684297));
#114560=CARTESIAN_POINT('Ctrl Pts',(-11.3402453023586,11.729110892674,10.4121287177449));
#114561=CARTESIAN_POINT('Ctrl Pts',(-11.3385419179345,11.7288777568964,
10.4082604897329));
#114562=CARTESIAN_POINT('Ctrl Pts',(-11.334119134539,11.7282758431147,10.398333574308));
#114563=CARTESIAN_POINT('Ctrl Pts',(-11.3313752384149,11.727905663636,10.3922859849185));
#114564=CARTESIAN_POINT('Ctrl Pts',(-11.3139025398083,11.7255694592676,
10.354462215987));
#114565=CARTESIAN_POINT('Ctrl Pts',(-11.2980791811996,11.7235458891817,
10.3232068399372));
#114566=CARTESIAN_POINT('Ctrl Pts',(-11.2752789935019,11.7207739495255,
10.2819169122308));
#114567=CARTESIAN_POINT('Ctrl Pts',(-11.2692744583298,11.7200559390253,
10.2713559364059));
#114568=CARTESIAN_POINT('Ctrl Pts',(-11.2006257645169,11.711987347571,10.1540382899813));
#114569=CARTESIAN_POINT('Ctrl Pts',(-11.1247988889472,11.7044068157916,
10.0555488463371));
#114570=CARTESIAN_POINT('Ctrl Pts',(-11.0190471673143,11.6957650675023,
9.94925841761822));
#114571=CARTESIAN_POINT('Ctrl Pts',(-11.0001243080575,11.6942777935473,
9.93123132143435));
#114572=CARTESIAN_POINT('Ctrl Pts',(-10.9710413142432,11.6920787460667,
9.90497427782668));
#114573=CARTESIAN_POINT('Ctrl Pts',(-10.9612378316976,11.6913515348915,
9.89635856708299));
#114574=CARTESIAN_POINT('Ctrl Pts',(-10.945185979161,11.6901831422179,9.88262769097901));
#114575=CARTESIAN_POINT('Ctrl Pts',(-10.9390083765175,11.6897386948096,
9.87743121161688));
#114576=CARTESIAN_POINT('Ctrl Pts',(-10.9272282591607,11.6889008938301,
9.86768729378933));
#114577=CARTESIAN_POINT('Ctrl Pts',(-10.9216345112152,11.6885071384502,
9.86312967337223));
#114578=CARTESIAN_POINT('Ctrl Pts',(-10.9159158980214,11.6881086647101,
9.85854026288203));
#114579=CARTESIAN_POINT('Ctrl Pts',(-10.9158245712297,11.6881023020954,
9.85846698758125));
#114580=CARTESIAN_POINT('Ctrl Pts',(-10.9156395850463,11.6880894164798,
9.85831860192528));
#114581=CARTESIAN_POINT('Ctrl Pts',(-10.9155459251939,11.6880828935006,
9.8582434921252));
#114582=CARTESIAN_POINT('Ctrl Pts',(-10.91535610056,11.6880696753179,9.85809130209254));
#114583=CARTESIAN_POINT('Ctrl Pts',(-10.9152599352929,11.6880629801397,
9.85801422248929));
#114584=CARTESIAN_POINT('Ctrl Pts',(-10.9150649131779,11.6880494047442,
9.85785794635015));
#114585=CARTESIAN_POINT('Ctrl Pts',(-10.9149660557833,11.6880425245542,
9.85777875050008));
#114586=CARTESIAN_POINT('Ctrl Pts',(-10.9103385841818,11.6877205232028,
9.85407261347046));
#114587=CARTESIAN_POINT('Ctrl Pts',(-10.9057884079304,11.687406471117,9.85047258647511));
#114588=CARTESIAN_POINT('Ctrl Pts',(-10.895814345535,11.686723589641,9.84267725991775));
#114589=CARTESIAN_POINT('Ctrl Pts',(-10.8903821247848,11.6863551896471,
9.83849281516649));
#114590=CARTESIAN_POINT('Ctrl Pts',(-10.8755712654802,11.6853601156105,
9.82724896207685));
#114591=CARTESIAN_POINT('Ctrl Pts',(-10.8661366720745,11.6847363147741,
9.82026387959406));
#114592=CARTESIAN_POINT('Ctrl Pts',(-10.8204839211805,11.6817642436415,
9.78730688070494));
#114593=CARTESIAN_POINT('Ctrl Pts',(-10.7831744819301,11.6794745936183,
9.76288372335997));
#114594=CARTESIAN_POINT('Ctrl Pts',(-10.648064197173,11.6715717947472,9.68300522338928));
#114595=CARTESIAN_POINT('Ctrl Pts',(-10.5450626399567,11.666257996532,9.63714713233808));
#114596=CARTESIAN_POINT('Ctrl Pts',(-10.3931199970811,11.6583583565572,
9.58950913556167));
#114597=CARTESIAN_POINT('Ctrl Pts',(-10.3477653502953,11.6559880039351,
9.57764760496075));
#114598=CARTESIAN_POINT('Ctrl Pts',(-10.2916510011308,11.6529573775868,
9.56581654810985));
#114599=CARTESIAN_POINT('Ctrl Pts',(-10.2813550799387,11.652397319608,9.56376123619725));
#114600=CARTESIAN_POINT('Ctrl Pts',(-10.2665102913943,11.6515829486251,
9.56096360539452));
#114601=CARTESIAN_POINT('Ctrl Pts',(-10.2619784080785,11.6513334156389,
9.56013167513231));
#114602=CARTESIAN_POINT('Ctrl Pts',(-10.2540806978368,11.6508968408326,
9.55872039034368));
#114603=CARTESIAN_POINT('Ctrl Pts',(-10.2507166054712,11.6507103356166,
9.55813138676255));
#114604=CARTESIAN_POINT('Ctrl Pts',(-10.2436006556844,11.6503146401129,
9.55691114442579));
#114605=CARTESIAN_POINT('Ctrl Pts',(-10.239848397897,11.6501053008798,9.55628275971959));
#114606=CARTESIAN_POINT('Ctrl Pts',(-10.2296891584629,11.6495367342492,
9.55462210628225));
#114607=CARTESIAN_POINT('Ctrl Pts',(-10.2232777677505,11.649176004278,9.55361782353091));
#114608=CARTESIAN_POINT('Ctrl Pts',(-10.1936538664019,11.6475010936978,
9.54917918195676));
#114609=CARTESIAN_POINT('Ctrl Pts',(-10.1703687125812,11.646161532245,9.54626094421371));
#114610=CARTESIAN_POINT('Ctrl Pts',(-10.0534673905235,11.6393543889882,
9.53445718900411));
#114611=CARTESIAN_POINT('Ctrl Pts',(-9.95922065802072,11.6336199679331,
9.53404955545915));
#114612=CARTESIAN_POINT('Ctrl Pts',(-9.80520023455023,11.6243634832209,
9.54825513208688));
#114613=CARTESIAN_POINT('Ctrl Pts',(-9.74521144150929,11.6207837092217,
9.55757354901897));
#114614=CARTESIAN_POINT('Ctrl Pts',(-9.65207574211328,11.6153174881503,
9.57803474818691));
#114615=CARTESIAN_POINT('Ctrl Pts',(-9.61845600041192,11.6133628021498,
9.58668442067806));
#114616=CARTESIAN_POINT('Ctrl Pts',(-9.57521487396315,11.6108721633427,
9.59946521493751));
#114617=CARTESIAN_POINT('Ctrl Pts',(-9.56528772308476,11.6103019693183,
9.60251463995475));
#114618=CARTESIAN_POINT('Ctrl Pts',(-9.54914339413789,11.6093771243343,
9.60766253759527));
#114619=CARTESIAN_POINT('Ctrl Pts',(-9.5429065039128,11.6090204379554,9.60969757748716));
#114620=CARTESIAN_POINT('Ctrl Pts',(-9.53088745208363,11.6083341680599,
9.61370890405043));
#114621=CARTESIAN_POINT('Ctrl Pts',(-9.52510357960061,11.6080044113381,
9.61567959750339));
#114622=CARTESIAN_POINT('Ctrl Pts',(-9.51179683587907,11.6072468187616,
9.62030671261641));
#114623=CARTESIAN_POINT('Ctrl Pts',(-9.50428296762525,11.6068198226367,
9.62298855345223));
#114624=CARTESIAN_POINT('Ctrl Pts',(-9.48012368217048,11.6054491929746,
9.6318348339827));
#114625=CARTESIAN_POINT('Ctrl Pts',(-9.46356803220921,11.6045134845507,
9.63824081169274));
#114626=CARTESIAN_POINT('Ctrl Pts',(-9.33997749788962,11.5975463788458,
9.68866626711206));
#114627=CARTESIAN_POINT('Ctrl Pts',(-9.23838775952141,11.591965677738,9.74494023042731));
#114628=CARTESIAN_POINT('Ctrl Pts',(-9.07848775998065,11.5823594252192,
9.86014756995489));
#114629=CARTESIAN_POINT('Ctrl Pts',(-9.01657999458253,11.5783670579818,
9.91310982224851));
#114630=CARTESIAN_POINT('Ctrl Pts',(-8.9534226984433,11.5735939322803,9.97697485353089));
#114631=CARTESIAN_POINT('Ctrl Pts',(-8.94749884260123,11.5731386873473,
9.98307040296981));
#114632=CARTESIAN_POINT('Ctrl Pts',(-8.93870673871934,11.5724509858833,
9.99227644642512));
#114633=CARTESIAN_POINT('Ctrl Pts',(-8.93579823325915,11.5722214795905,
9.99534844566566));
#114634=CARTESIAN_POINT('Ctrl Pts',(-8.93081485720318,11.5718246858552,
10.0006578706696));
#114635=CARTESIAN_POINT('Ctrl Pts',(-8.92873360968667,11.5716578848684,
10.0028892329251));
#114636=CARTESIAN_POINT('Ctrl Pts',(-8.92399828930383,11.5712758709605,
10.0079980384012));
#114637=CARTESIAN_POINT('Ctrl Pts',(-8.92134881802128,11.571060327158,10.0108795825991));
#114638=CARTESIAN_POINT('Ctrl Pts',(-8.91412361622041,11.5704676618925,
10.018801208185));
#114639=CARTESIAN_POINT('Ctrl Pts',(-8.9095714985369,11.570088862648,10.0238625765528));
#114640=CARTESIAN_POINT('Ctrl Pts',(-8.88654011679276,11.5681454355156,
10.0498326483015));
#114641=CARTESIAN_POINT('Ctrl Pts',(-8.86862732873863,11.5665446624375,
10.0712338376494));
#114642=CARTESIAN_POINT('Ctrl Pts',(-8.83441132044706,11.5633261337647,
10.1145727068805));
#114643=CARTESIAN_POINT('Ctrl Pts',(-8.81808847498346,11.5617100395966,
10.1364819094037));
#114644=CARTESIAN_POINT('Ctrl Pts',(-8.7629388345888,11.5559882812125,10.2150012825382));
#114645=CARTESIAN_POINT('Ctrl Pts',(-8.72748877255023,11.5518262476291,
10.2738741785106));
#114646=CARTESIAN_POINT('Ctrl Pts',(-8.66194377399587,11.5432199472893,
10.4023753854391));
#114647=CARTESIAN_POINT('Ctrl Pts',(-8.63285497269362,11.5388050167115,
10.4723005416013));
#114648=CARTESIAN_POINT('Ctrl Pts',(-8.60373125867463,11.5335665810548,
10.5611545243207));
#114649=CARTESIAN_POINT('Ctrl Pts',(-8.59847542299494,11.5325750906874,
10.5782410058611));
#114650=CARTESIAN_POINT('Ctrl Pts',(-8.59129799792309,11.5311496087261,
10.603192330531));
#114651=CARTESIAN_POINT('Ctrl Pts',(-8.5891266756742,11.5307076496595,10.6109831320211));
#114652=CARTESIAN_POINT('Ctrl Pts',(-8.5854295984133,11.5299356609608,10.6246866515785));
#114653=CARTESIAN_POINT('Ctrl Pts',(-8.58387607265188,11.5296047502809,
10.6305916155493));
#114654=CARTESIAN_POINT('Ctrl Pts',(-8.58072709578384,11.5289200809813,
10.6428727519618));
#114655=CARTESIAN_POINT('Ctrl Pts',(-8.57913754992648,11.5285665168862,
10.6492503060187));
#114656=CARTESIAN_POINT('Ctrl Pts',(-8.57513442405915,11.5276548381275,
10.6657854906743));
#114657=CARTESIAN_POINT('Ctrl Pts',(-8.57278645417067,11.5270988098742,
10.6759587219705));
#114658=CARTESIAN_POINT('Ctrl Pts',(-8.56369899359542,11.5248555106611,
10.7173490598808));
#114659=CARTESIAN_POINT('Ctrl Pts',(-8.5578730292936,11.523196933513,10.7487588251569));
#114660=CARTESIAN_POINT('Ctrl Pts',(-8.53218269435429,11.5144510085156,
10.917980104887));
#114661=CARTESIAN_POINT('Ctrl Pts',(-8.53103444530728,11.5079672197986,
11.0578857983742));
#114662=CARTESIAN_POINT('Ctrl Pts',(-8.55505583806701,11.4989583218038,
11.2357818294622));
#114663=CARTESIAN_POINT('Ctrl Pts',(-8.56209649598592,11.4968914165499,
11.2754808220132));
#114664=CARTESIAN_POINT('Ctrl Pts',(-8.57233387995621,11.4943529938332,
11.3219547280457));
#114665=CARTESIAN_POINT('Ctrl Pts',(-8.57395532951994,11.4939614496551,
11.3290622899376));
#114666=CARTESIAN_POINT('Ctrl Pts',(-8.57654376880891,11.4933516931382,
11.340030059812));
#114667=CARTESIAN_POINT('Ctrl Pts',(-8.57747353757602,11.4931355227729,
11.3438990355231));
#114668=CARTESIAN_POINT('Ctrl Pts',(-8.57922297926627,11.4927338909099,
11.3510503567288));
#114669=CARTESIAN_POINT('Ctrl Pts',(-8.58003826458599,11.4925486770264,
11.354333691432));
#114670=CARTESIAN_POINT('Ctrl Pts',(-8.58192065730371,11.4921254452299,
11.3618036681155));
#114671=CARTESIAN_POINT('Ctrl Pts',(-8.58299492022926,11.4918870294069,
11.3659884142591));
#114672=CARTESIAN_POINT('Ctrl Pts',(-8.58584592001532,11.4912624017895,
11.3768936318395));
#114673=CARTESIAN_POINT('Ctrl Pts',(-8.58765201643302,11.4908746112489,
11.3836062318812));
#114674=CARTESIAN_POINT('Ctrl Pts',(-8.60055284734017,11.4881594522332,
11.4302275151662));
#114675=CARTESIAN_POINT('Ctrl Pts',(-8.6132889125125,11.4857518383235,11.4696592716363));
#114676=CARTESIAN_POINT('Ctrl Pts',(-8.64096512073443,11.481041905672,11.5443516599621));
#114677=CARTESIAN_POINT('Ctrl Pts',(-8.65565148326296,11.4787474078218,
11.5796735577058));
#114678=CARTESIAN_POINT('Ctrl Pts',(-8.69706546661657,11.4728132613263,
11.6692112389772));
#114679=CARTESIAN_POINT('Ctrl Pts',(-8.72579928695462,11.4691728498757,
11.7224231519741));
#114680=CARTESIAN_POINT('Ctrl Pts',(-8.7810844752932,11.4629966844251,11.8111885712552));
#114681=CARTESIAN_POINT('Ctrl Pts',(-8.80611374901831,11.4604296359684,
11.8475954727107));
#114682=CARTESIAN_POINT('Ctrl Pts',(-8.84406263891625,11.4568531892661,
11.8977709006743));
#114683=CARTESIAN_POINT('Ctrl Pts',(-8.85565908674962,11.4557976658339,
11.9125062695176));
#114684=CARTESIAN_POINT('Ctrl Pts',(-8.87682574403533,11.453935834131,11.9383639680648));
#114685=CARTESIAN_POINT('Ctrl Pts',(-8.88628591673415,11.4531254187194,
11.9495726978218));
#114686=CARTESIAN_POINT('Ctrl Pts',(-8.90081947171254,11.4519122266862,
11.9662765051693));
#114687=CARTESIAN_POINT('Ctrl Pts',(-8.90576890541274,11.4515044515295,
11.9718777869328));
#114688=CARTESIAN_POINT('Ctrl Pts',(-8.91479107840204,11.4507706865977,
11.9819318996718));
#114689=CARTESIAN_POINT('Ctrl Pts',(-8.91884883412423,11.4504440891259,
11.9863979000073));
#114690=CARTESIAN_POINT('Ctrl Pts',(-8.92761212326882,11.449745971754,11.995923809079));
#114691=CARTESIAN_POINT('Ctrl Pts',(-8.93232611606177,11.4493748178274,
12.0009757596638));
#114692=CARTESIAN_POINT('Ctrl Pts',(-8.94510061040143,11.44838058073,12.014473173132));
#114693=CARTESIAN_POINT('Ctrl Pts',(-8.9532267699252,11.4477602998774,12.0228559802902));
#114694=CARTESIAN_POINT('Ctrl Pts',(-8.99356461553095,11.4447387857988,
12.0634835714805));
#114695=CARTESIAN_POINT('Ctrl Pts',(-9.02717160273462,11.4423991512414,
12.0943102458646));
#114696=CARTESIAN_POINT('Ctrl Pts',(-9.07591485195291,11.4392055914501,
12.1349976569982));
#114697=CARTESIAN_POINT('Ctrl Pts',(-9.08987453997787,11.4383121002684,
12.1462219298007));
#114698=CARTESIAN_POINT('Ctrl Pts',(-9.18149871929675,11.432568204177,12.2171627984452));
#114699=CARTESIAN_POINT('Ctrl Pts',(-9.26478235065502,11.4279148031777,
12.2692057770446));
#114700=CARTESIAN_POINT('Ctrl Pts',(-9.38100134151841,11.421458148884,12.3265267261546));
#114701=CARTESIAN_POINT('Ctrl Pts',(-9.40981020434452,11.4198586877313,
12.3395925824074));
#114702=CARTESIAN_POINT('Ctrl Pts',(-9.45609249157997,11.4172577598147,
12.3588004355484));
#114703=CARTESIAN_POINT('Ctrl Pts',(-9.47329892573647,11.4162841147581,
12.3655621250389));
#114704=CARTESIAN_POINT('Ctrl Pts',(-9.49600347830573,11.4149850240082,
12.3739914973173));
#114705=CARTESIAN_POINT('Ctrl Pts',(-9.50139054316824,11.4146757460125,
12.3759555719406));
#114706=CARTESIAN_POINT('Ctrl Pts',(-9.51021329099656,11.4141673059653,
12.3791136495742));
#114707=CARTESIAN_POINT('Ctrl Pts',(-9.51364218039606,11.413969234299,12.3803266097115));
#114708=CARTESIAN_POINT('Ctrl Pts',(-9.52033180486485,11.4135818247282,
12.3826650250974));
#114709=CARTESIAN_POINT('Ctrl Pts',(-9.52359204767646,11.4133925618799,
12.3837917513907));
#114710=CARTESIAN_POINT('Ctrl Pts',(-9.53159678254224,11.4129268077977,
12.3865265133184));
#114711=CARTESIAN_POINT('Ctrl Pts',(-9.53634558633175,11.412649585399,12.3881217271715));
#114712=CARTESIAN_POINT('Ctrl Pts',(-9.55253278709311,11.4117017429061,
12.3934669868706));
#114713=CARTESIAN_POINT('Ctrl Pts',(-9.56400892420642,11.4110248850594,
12.3971001800116));
#114714=CARTESIAN_POINT('Ctrl Pts',(-9.64733843275038,11.406081637634,12.422354533796));
#114715=CARTESIAN_POINT('Ctrl Pts',(-9.72071029128511,11.4015821084823,
12.4385610814297));
#114716=CARTESIAN_POINT('Ctrl Pts',(-9.85869333012996,11.3931975413301,
12.4580821391088));
#114717=CARTESIAN_POINT('Ctrl Pts',(-9.92292114403549,11.3893247174424,
12.4628843995483));
#114718=CARTESIAN_POINT('Ctrl Pts',(-10.0275671328543,11.3831704423263,
12.4637954694185));
#114719=CARTESIAN_POINT('Ctrl Pts',(-10.0678748107872,11.3808364026854,
12.4624809510527));
#114720=CARTESIAN_POINT('Ctrl Pts',(-10.1256605894001,11.3775499753839,
12.4582017898254));
#114721=CARTESIAN_POINT('Ctrl Pts',(-10.1432173253624,11.3765593255652,
12.4565822594953));
#114722=CARTESIAN_POINT('Ctrl Pts',(-10.1746259480028,11.3748009529641,
12.4531115485322));
#114723=CARTESIAN_POINT('Ctrl Pts',(-10.1884884755116,11.374029740693,12.4513784853414));
#114724=CARTESIAN_POINT('Ctrl Pts',(-10.2095861661059,11.3728631336376,
12.4484335157498));
#114725=CARTESIAN_POINT('Ctrl Pts',(-10.2168402905223,11.3724632995181,
12.4473652965648));
#114726=CARTESIAN_POINT('Ctrl Pts',(-10.2300407460209,11.3717379805044,
12.4453199691868));
#114727=CARTESIAN_POINT('Ctrl Pts',(-10.2359896230982,11.3714119512394,
12.444360570442));
#114728=CARTESIAN_POINT('Ctrl Pts',(-10.2488558160518,11.3707085760832,
12.442203977344));
#114729=CARTESIAN_POINT('Ctrl Pts',(-10.2557708053247,11.3703316480437,
12.4409936942706));
#114730=CARTESIAN_POINT('Ctrl Pts',(-10.2746377429737,11.3693061056603,
12.4375514543835));
#114731=CARTESIAN_POINT('Ctrl Pts',(-10.2865711526202,11.3686606082065,
12.4352202131067));
#114732=CARTESIAN_POINT('Ctrl Pts',(-10.3500158759908,11.3652438766463,
12.4220031483192));
#114733=CARTESIAN_POINT('Ctrl Pts',(-10.4009431512887,11.3625564372787,
12.408491892493));
#114734=CARTESIAN_POINT('Ctrl Pts',(-10.5517992938335,11.3546352794877,
12.3596208081135));
#114735=CARTESIAN_POINT('Ctrl Pts',(-10.6487158848414,11.3496190955654,
12.3161373578487));
#114736=CARTESIAN_POINT('Ctrl Pts',(-10.7821001760998,11.3419303981839,
12.2379511348052));
#114737=CARTESIAN_POINT('Ctrl Pts',(-10.8228529943803,11.3394559791379,
12.211245545055));
#114738=CARTESIAN_POINT('Ctrl Pts',(-10.8683425189849,11.3364561228357,
12.1780795385852));
#114739=CARTESIAN_POINT('Ctrl Pts',(-10.8744547735832,11.3360478311921,
12.1735497320214));
#114740=CARTESIAN_POINT('Ctrl Pts',(-10.8837636605859,11.3354175169901,
12.1665377913031));
#114741=CARTESIAN_POINT('Ctrl Pts',(-10.8869858677704,11.3351977604464,
12.1640896425475));
#114742=CARTESIAN_POINT('Ctrl Pts',(-10.8928791169897,11.3347928504524,
12.1595734317947));
#114743=CARTESIAN_POINT('Ctrl Pts',(-10.8955531883116,11.3346079774608,
12.1575094589641));
#114744=CARTESIAN_POINT('Ctrl Pts',(-10.9015638265741,11.3341898464147,
12.1528368721524));
#114745=CARTESIAN_POINT('Ctrl Pts',(-10.9048962080823,11.333956230238,12.1502230387444));
#114746=CARTESIAN_POINT('Ctrl Pts',(-10.9134466631671,11.3333522600879,
12.1434561294621));
#114747=CARTESIAN_POINT('Ctrl Pts',(-10.9186477226205,11.3329804889804,
12.1392818285136));
#114748=CARTESIAN_POINT('Ctrl Pts',(-10.9514035971639,11.3306121508043,
12.1126222637292));
#114749=CARTESIAN_POINT('Ctrl Pts',(-10.9781576964593,11.3285562560528,
12.0891759450938));
#114750=CARTESIAN_POINT('Ctrl Pts',(-11.0119533995221,11.3258248614941,
12.0573084661654));
#114751=CARTESIAN_POINT('Ctrl Pts',(-11.0197938353524,11.3251811905767,
12.0497482562144));
#114752=CARTESIAN_POINT('Ctrl Pts',(-11.1160937526781,11.3171570681968,
11.9547931104636));
#114753=CARTESIAN_POINT('Ctrl Pts',(-11.1931654580102,11.3095387455601,
11.856538667084));
#114754=CARTESIAN_POINT('Ctrl Pts',(-11.270294152291,11.3008603254226,11.7272348183555));
#114755=CARTESIAN_POINT('Ctrl Pts',(-11.2831010585926,11.2993699947618,
11.7043930054864));
#114756=CARTESIAN_POINT('Ctrl Pts',(-11.3041442646358,11.2968326329587,
11.6643808577152));
#114757=CARTESIAN_POINT('Ctrl Pts',(-11.3126708161345,11.2957760194702,
11.6473712715336));
#114758=CARTESIAN_POINT('Ctrl Pts',(-11.3244335666525,11.2942753146663,
11.622717199005));
#114759=CARTESIAN_POINT('Ctrl Pts',(-11.3279399550492,11.2938220332981,
11.6152044067964));
#114760=CARTESIAN_POINT('Ctrl Pts',(-11.3339309244136,11.2930369474052,
11.6020782454489));
#114761=CARTESIAN_POINT('Ctrl Pts',(-11.3364443555855,11.2927041694526,
11.5964783405632));
#114762=CARTESIAN_POINT('Ctrl Pts',(-11.3412298601791,11.2920638432507,
11.5856341638999));
#114763=CARTESIAN_POINT('Ctrl Pts',(-11.343506586619,11.2917561425349,11.5803920784616));
#114764=CARTESIAN_POINT('Ctrl Pts',(-11.3488420787001,11.2910276090775,
11.5679076522584));
#114765=CARTESIAN_POINT('Ctrl Pts',(-11.351873326542,11.2906077021265,11.560653696133));
#114766=CARTESIAN_POINT('Ctrl Pts',(-11.3608518716564,11.2893451986867,
11.5386712546625));
#114767=CARTESIAN_POINT('Ctrl Pts',(-11.3666180901469,11.2885085790709,
11.5238697914193));
#114768=CARTESIAN_POINT('Ctrl Pts',(-11.4128432419754,11.2815697369377,
11.399252198799));
#114769=CARTESIAN_POINT('Ctrl Pts',(-11.440236324836,11.275931943562,11.28504386706));
#114770=CARTESIAN_POINT('Ctrl Pts',(-11.4602677332692,11.2674633686444,
11.112514165549));
#114771=CARTESIAN_POINT('Ctrl Pts',(-11.4635279155575,11.2646839331958,
11.0559152993318));
#114772=CARTESIAN_POINT('Ctrl Pts',(-11.463499819958,11.2617878197064,10.9992740641209));
#114773=CARTESIAN_POINT('Ctrl Pts',(-11.4634998522255,11.1882569054959,
10.99934232525));
#114774=CARTESIAN_POINT('Ctrl Pts',(-11.4635338577437,11.1926793304679,
11.0750135760492));
#114775=CARTESIAN_POINT('Ctrl Pts',(-11.4576989133034,11.1972663920743,
11.1505728907243));
#114776=CARTESIAN_POINT('Ctrl Pts',(-11.4355453177886,11.2059062555568,
11.2927357097168));
#114777=CARTESIAN_POINT('Ctrl Pts',(-11.4203436720628,11.2099570437846,
11.3593187447778));
#114778=CARTESIAN_POINT('Ctrl Pts',(-11.3897135834784,11.2160275233218,
11.4603518144949));
#114779=CARTESIAN_POINT('Ctrl Pts',(-11.3775105646457,11.2181359984491,
11.4956739190319));
#114780=CARTESIAN_POINT('Ctrl Pts',(-11.3601086820031,11.2207893666858,
11.5404165078517));
#114781=CARTESIAN_POINT('Ctrl Pts',(-11.3561407329977,11.2213742944607,
11.5502980551487));
#114782=CARTESIAN_POINT('Ctrl Pts',(-11.3495318268785,11.2223170183909,
11.5662507495036));
#114783=CARTESIAN_POINT('Ctrl Pts',(-11.3469569498686,11.2226769998052,
11.5723487051358));
#114784=CARTESIAN_POINT('Ctrl Pts',(-11.3419328037563,11.2233656542342,
11.5840254429781));
#114785=CARTESIAN_POINT('Ctrl Pts',(-11.3394898997157,11.223694531822,11.5896067994388));
#114786=CARTESIAN_POINT('Ctrl Pts',(-11.3338187661337,11.2244446177062,
11.6023465865331));
#114787=CARTESIAN_POINT('Ctrl Pts',(-11.3305676181248,11.2248650421615,
11.6094946497238));
#114788=CARTESIAN_POINT('Ctrl Pts',(-11.3203355243064,11.226159339565,11.6315191068243));
#114789=CARTESIAN_POINT('Ctrl Pts',(-11.3131613173344,11.2270266441307,
11.646304620224));
#114790=CARTESIAN_POINT('Ctrl Pts',(-11.2487837638936,11.2344807689899,
11.7734824723576));
#114791=CARTESIAN_POINT('Ctrl Pts',(-11.177527444974,11.2405144428455,11.8781611834126));
#114792=CARTESIAN_POINT('Ctrl Pts',(-11.0598518892127,11.2491721620616,
12.0105175878392));
#114793=CARTESIAN_POINT('Ctrl Pts',(-11.0240084805301,11.2516885334046,
12.046822719719));
#114794=CARTESIAN_POINT('Ctrl Pts',(-10.9738768593859,11.2551675984063,
12.0925571003518));
#114795=CARTESIAN_POINT('Ctrl Pts',(-10.9612117502599,11.2560434589762,
12.1037160341963));
#114796=CARTESIAN_POINT('Ctrl Pts',(-10.9422286974817,11.2573565504918,
12.119866988916));
#114797=CARTESIAN_POINT('Ctrl Pts',(-10.9360576667886,11.2577834597663,
12.1250302352685));
#114798=CARTESIAN_POINT('Ctrl Pts',(-10.9248992325891,11.2585561192119,
12.1342110343685));
#114799=CARTESIAN_POINT('Ctrl Pts',(-10.9199273977997,11.258900644706,12.1382472669462));
#114800=CARTESIAN_POINT('Ctrl Pts',(-10.9119542999476,11.2594538329858,
12.1446336243853));
#114801=CARTESIAN_POINT('Ctrl Pts',(-10.9089700115832,11.2596610406498,
12.1470049244167));
#114802=CARTESIAN_POINT('Ctrl Pts',(-10.9033089076799,11.2600544659016,
12.1514672400781));
#114803=CARTESIAN_POINT('Ctrl Pts',(-10.900634052081,11.2602405154443,12.1535606144061));
#114804=CARTESIAN_POINT('Ctrl Pts',(-10.8944920312796,11.2606680618265,
12.1583330499074));
#114805=CARTESIAN_POINT('Ctrl Pts',(-10.8910201047251,11.2609099821988,
12.1610058658297));
#114806=CARTESIAN_POINT('Ctrl Pts',(-10.8817212241847,11.2615584358344,
12.1680982058668));
#114807=CARTESIAN_POINT('Ctrl Pts',(-10.8758731302221,11.2619667878203,
12.172489654982));
#114808=CARTESIAN_POINT('Ctrl Pts',(-10.8264733175058,11.265418962106,12.2090091273422));
#114809=CARTESIAN_POINT('Ctrl Pts',(-10.781206944492,11.2685988583441,12.2387396063636));
#114810=CARTESIAN_POINT('Ctrl Pts',(-10.6422796541326,11.2781817087353,
12.3193378189134));
#114811=CARTESIAN_POINT('Ctrl Pts',(-10.5445850578446,11.2846710858472,
12.3625734969083));
#114812=CARTESIAN_POINT('Ctrl Pts',(-10.3979600770254,11.2936104666671,
12.4091484437394));
#114813=CARTESIAN_POINT('Ctrl Pts',(-10.3521880454408,11.2963010748327,
12.4212796503466));
#114814=CARTESIAN_POINT('Ctrl Pts',(-10.2946893415239,11.2995566599851,
12.4335696611234));
#114815=CARTESIAN_POINT('Ctrl Pts',(-10.2834459614915,11.3001875278057,
12.4358350109554));
#114816=CARTESIAN_POINT('Ctrl Pts',(-10.2654963904741,11.3011857754426,
12.4392324845373));
#114817=CARTESIAN_POINT('Ctrl Pts',(-10.2588070893192,11.3015558350145,
12.4404504054594));
#114818=CARTESIAN_POINT('Ctrl Pts',(-10.2461493823004,11.3022524445173,
12.4426639735371));
#114819=CARTESIAN_POINT('Ctrl Pts',(-10.2401828341048,11.3025792914326,
12.4436693065458));
#114820=CARTESIAN_POINT('Ctrl Pts',(-10.2266629668339,11.3033165438201,
12.4458611989896));
#114821=CARTESIAN_POINT('Ctrl Pts',(-10.2191062065598,11.3037262505235,
12.4470256322978));
#114822=CARTESIAN_POINT('Ctrl Pts',(-10.1995874378448,11.3047785799762,
12.4498769019648));
#114823=CARTESIAN_POINT('Ctrl Pts',(-10.1876129218288,11.3054184418868,
12.4514749667877));
#114824=CARTESIAN_POINT('Ctrl Pts',(-10.0829394314003,11.3109647745834,
12.4641271939158));
#114825=CARTESIAN_POINT('Ctrl Pts',(-9.98939683332163,11.3155815356956,
12.4664370591649));
#114826=CARTESIAN_POINT('Ctrl Pts',(-9.82937065051905,11.3234042208506,
12.4550652823896));
#114827=CARTESIAN_POINT('Ctrl Pts',(-9.76288738159231,11.3266374998875,
12.4457199905939));
#114828=CARTESIAN_POINT('Ctrl Pts',(-9.65316561131281,11.3322351874399,
12.4225229040288));
#114829=CARTESIAN_POINT('Ctrl Pts',(-9.60950750941634,11.3345353776697,
12.4111627843756));
#114830=CARTESIAN_POINT('Ctrl Pts',(-9.55929835679746,11.3373377064522,
12.3955896026911));
#114831=CARTESIAN_POINT('Ctrl Pts',(-9.55216646471291,11.3377395301958,
12.3933174072764));
#114832=CARTESIAN_POINT('Ctrl Pts',(-9.54123025632845,11.3383619467455,
12.3897405313191));
#114833=CARTESIAN_POINT('Ctrl Pts',(-9.53741326040538,11.338580361597,12.3884746773582));
#114834=CARTESIAN_POINT('Ctrl Pts',(-9.53039721874848,11.3389840818613,
12.3861157622858));
#114835=CARTESIAN_POINT('Ctrl Pts',(-9.52719670209757,11.3391691194281,
12.3850273352827));
#114836=CARTESIAN_POINT('Ctrl Pts',(-9.51996352002133,11.3395892746415,
12.382539492501));
#114837=CARTESIAN_POINT('Ctrl Pts',(-9.51593321050209,11.3398247656405,
12.3811335246087));
#114838=CARTESIAN_POINT('Ctrl Pts',(-9.5055202373898,11.3404366687097,12.3774497962112));
#114839=CARTESIAN_POINT('Ctrl Pts',(-9.49914721181735,11.3408145585016,
12.3751453224019));
#114840=CARTESIAN_POINT('Ctrl Pts',(-9.45740217733963,11.3433110638844,
12.3597217160524));
#114841=CARTESIAN_POINT('Ctrl Pts',(-9.42253529966939,11.3454963847404,
12.3452842113327));
#114842=CARTESIAN_POINT('Ctrl Pts',(-9.29438587855687,11.3538090634982,
12.2863206353601));
#114843=CARTESIAN_POINT('Ctrl Pts',(-9.2053421834017,11.3601341771834,12.2333015328602));
#114844=CARTESIAN_POINT('Ctrl Pts',(-9.08758944111155,11.3688197762693,
12.1451005107877));
#114845=CARTESIAN_POINT('Ctrl Pts',(-9.05374878703321,11.3713635216003,
12.1172991313714));
#114846=CARTESIAN_POINT('Ctrl Pts',(-9.00734496610683,11.3749111987279,
12.0755536735094));
#114847=CARTESIAN_POINT('Ctrl Pts',(-8.99372590804323,11.375960437172,12.0628227588898));
#114848=CARTESIAN_POINT('Ctrl Pts',(-8.96988012686894,11.3778123210649,
12.0396626643827));
#114849=CARTESIAN_POINT('Ctrl Pts',(-8.95955946815754,11.37861901084,12.0293342168726));
#114850=CARTESIAN_POINT('Ctrl Pts',(-8.94419970191335,11.3798278538856,
12.0134957659249));
#114851=CARTESIAN_POINT('Ctrl Pts',(-8.93904556594582,11.3802349506662,
12.0080990173196));
#114852=CARTESIAN_POINT('Ctrl Pts',(-8.92983647158431,11.3809650529399,
11.9983075791992));
#114853=CARTESIAN_POINT('Ctrl Pts',(-8.92576676618197,11.3812886813808,
11.9939270401103));
#114854=CARTESIAN_POINT('Ctrl Pts',(-8.91705738379454,11.3819834491744,
11.9844364763555));
#114855=CARTESIAN_POINT('Ctrl Pts',(-8.91242676692383,11.3823542051727,
11.9793183092796));
#114856=CARTESIAN_POINT('Ctrl Pts',(-8.90008718501891,11.3833460089234,
11.9654840452408));
#114857=CARTESIAN_POINT('Ctrl Pts',(-8.89244558790739,11.3839642793259,
11.9567083551246));
#114858=CARTESIAN_POINT('Ctrl Pts',(-8.85563077471804,11.3869644970278,
11.9133975051337));
#114859=CARTESIAN_POINT('Ctrl Pts',(-8.82796245483918,11.3892858965692,
11.8776129115956));
#114860=CARTESIAN_POINT('Ctrl Pts',(-8.73820138827559,11.397149338335,11.7496875480694));
#114861=CARTESIAN_POINT('Ctrl Pts',(-8.68496898238816,11.40240423267,11.6518124315955));
#114862=CARTESIAN_POINT('Ctrl Pts',(-8.62388760927176,11.4104798418267,
11.5008307100602));
#114863=CARTESIAN_POINT('Ctrl Pts',(-8.60702257077679,11.4131036899311,
11.4518069977571));
#114864=CARTESIAN_POINT('Ctrl Pts',(-8.5906774498911,11.4162735894621,11.3945903526116));
#114865=CARTESIAN_POINT('Ctrl Pts',(-8.58861995127858,11.4166869300703,
11.3871665656652));
#114866=CARTESIAN_POINT('Ctrl Pts',(-8.58556579661784,11.4173234703266,
11.3757987225679));
#114867=CARTESIAN_POINT('Ctrl Pts',(-8.58452678498911,11.4175443346645,
11.3718660677663));
#114868=CARTESIAN_POINT('Ctrl Pts',(-8.58265492112876,11.4179503482263,
11.3646595523714));
#114869=CARTESIAN_POINT('Ctrl Pts',(-8.58181699741172,11.418135207392,11.3613870948667));
#114870=CARTESIAN_POINT('Ctrl Pts',(-8.5799593317833,11.4185521219528,11.354026137339));
#114871=CARTESIAN_POINT('Ctrl Pts',(-8.57894592034459,11.4187845249927,
11.3499361471693));
#114872=CARTESIAN_POINT('Ctrl Pts',(-8.57602438381154,11.4194692133065,
11.3379232286568));
#114873=CARTESIAN_POINT('Ctrl Pts',(-8.57416478900355,11.4199240996775,
11.3299888011569));
#114874=CARTESIAN_POINT('Ctrl Pts',(-8.55726624375546,11.4242411825554,
11.2550761046984));
#114875=CARTESIAN_POINT('Ctrl Pts',(-8.54689245103548,11.4283201241921,
11.1871392351558));
#114876=CARTESIAN_POINT('Ctrl Pts',(-8.5346551527919,11.4373747604101,11.0368000541727));
#114877=CARTESIAN_POINT('Ctrl Pts',(-8.53490063362485,11.4423474610716,
10.9544444929529));
#114878=CARTESIAN_POINT('Ctrl Pts',(-8.54692419697573,11.4504326588445,
10.8169114196226));
#114879=CARTESIAN_POINT('Ctrl Pts',(-8.55496806311521,11.4536265045182,
10.7616000036699));
#114880=CARTESIAN_POINT('Ctrl Pts',(-8.56856024749333,11.4573883116653,
10.6951119579994));
#114881=CARTESIAN_POINT('Ctrl Pts',(-8.57111044210045,11.4580494938647,
10.6833754169989));
#114882=CARTESIAN_POINT('Ctrl Pts',(-8.5753567021834,11.4590843092491,10.6649304979668));
#114883=CARTESIAN_POINT('Ctrl Pts',(-8.57695632193355,11.4594609702094,
10.6582006585649));
#114884=CARTESIAN_POINT('Ctrl Pts',(-8.58004081992036,11.4601634255311,
10.6456208249245));
#114885=CARTESIAN_POINT('Ctrl Pts',(-8.58151428331777,11.4604895739194,
10.6397682053318));
#114886=CARTESIAN_POINT('Ctrl Pts',(-8.58489214075479,11.4612167763679,
10.6266934511137));
#114887=CARTESIAN_POINT('Ctrl Pts',(-8.5868157103419,11.4616172103819,10.6194764146541));
#114888=CARTESIAN_POINT('Ctrl Pts',(-8.59184044717048,11.4626296450614,
10.601187874811));
#114889=CARTESIAN_POINT('Ctrl Pts',(-8.59501701784213,11.46323923189,10.5901375021112));
#114890=CARTESIAN_POINT('Ctrl Pts',(-8.6158914852719,11.4670624821144,10.5206173732966));
#114891=CARTESIAN_POINT('Ctrl Pts',(-8.63710635422932,11.4701602134969,
10.4632634777758));
#114892=CARTESIAN_POINT('Ctrl Pts',(-8.70174583024231,11.4780770733069,
10.3173009905806));
#114893=CARTESIAN_POINT('Ctrl Pts',(-8.75064043438508,11.4827564871018,
10.2314681731663));
#114894=CARTESIAN_POINT('Ctrl Pts',(-8.82617550680336,11.4892448366329,
10.1253722688021));
#114895=CARTESIAN_POINT('Ctrl Pts',(-8.84539872465434,11.4908481850891,
10.1001481844332));
#114896=CARTESIAN_POINT('Ctrl Pts',(-8.87712323574395,11.4934548748436,
10.0612119401588));
#114897=CARTESIAN_POINT('Ctrl Pts',(-8.88909263149134,11.4944302468442,
10.0470781748281));
#114898=CARTESIAN_POINT('Ctrl Pts',(-8.90511759946581,11.495731378972,10.0288678193027));
#114899=CARTESIAN_POINT('Ctrl Pts',(-8.90893401068924,11.4960409104457,
10.0245820443698));
#114900=CARTESIAN_POINT('Ctrl Pts',(-8.91521134998595,11.4965496984126,
10.0176156169505));
#114901=CARTESIAN_POINT('Ctrl Pts',(-8.91765728071185,11.4967478622209,
10.0149214606584));
#114902=CARTESIAN_POINT('Ctrl Pts',(-8.92244177286516,11.4971353949788,
10.0096907451988));
#114903=CARTESIAN_POINT('Ctrl Pts',(-8.9247792919548,11.4973246883982,10.007153294208));
#114904=CARTESIAN_POINT('Ctrl Pts',(-8.93053247137639,11.4977904346543,
10.000952180998));
#114905=CARTESIAN_POINT('Ctrl Pts',(-8.93395799604242,11.4980676180705,
9.99729775918687));
#114906=CARTESIAN_POINT('Ctrl Pts',(-8.94567198399762,11.499014817498,9.98492890645159));
#114907=CARTESIAN_POINT('Ctrl Pts',(-8.95404886379648,11.4996910583094,
9.97629931520783));
#114908=CARTESIAN_POINT('Ctrl Pts',(-9.01565166136431,11.5046494570885,
9.91438359564765));
#114909=CARTESIAN_POINT('Ctrl Pts',(-9.07281033988419,11.5091665324305,
9.86517751281857));
#114910=CARTESIAN_POINT('Ctrl Pts',(-9.18574523258869,11.5175982913541,
9.7822048250766));
#114911=CARTESIAN_POINT('Ctrl Pts',(-9.24049110956728,11.521500790821,9.74732964846882));
#114912=CARTESIAN_POINT('Ctrl Pts',(-9.33231177819378,11.5276529684802,
9.69707590664529));
#114913=CARTESIAN_POINT('Ctrl Pts',(-9.36802000449302,11.5299581016063,
9.67938634490512));
#114914=CARTESIAN_POINT('Ctrl Pts',(-9.42038182505174,11.5332083615117,
9.65605772394456));
#114915=CARTESIAN_POINT('Ctrl Pts',(-9.43648259885476,11.5341908190591,
9.64922753758803));
#114916=CARTESIAN_POINT('Ctrl Pts',(-9.46557641200887,11.5359361131764,
9.63749628791977));
#114917=CARTESIAN_POINT('Ctrl Pts',(-9.47852390074208,11.5367023642279,
9.6324885253499));
#114918=CARTESIAN_POINT('Ctrl Pts',(-9.49840045758861,11.5378631279315,
9.62512412911922));
#114919=CARTESIAN_POINT('Ctrl Pts',(-9.50527895969779,11.5382620106919,
9.62263408773687));
#114920=CARTESIAN_POINT('Ctrl Pts',(-9.51730642667266,11.5389546655555,
9.61838182685496));
#114921=CARTESIAN_POINT('Ctrl Pts',(-9.52244704619107,11.5392491872347,
9.61659657384115));
#114922=CARTESIAN_POINT('Ctrl Pts',(-9.53405769521518,11.5399110166898,
9.6126368153354));
#114923=CARTESIAN_POINT('Ctrl Pts',(-9.54053324506639,11.5402777811637,
9.61047880879388));
#114924=CARTESIAN_POINT('Ctrl Pts',(-9.55804397950657,11.5412633547282,
9.60477907161012));
#114925=CARTESIAN_POINT('Ctrl Pts',(-9.5691066486116,11.5418793865342,9.60132294899019));
#114926=CARTESIAN_POINT('Ctrl Pts',(-9.6212384049464,11.5447527602802,9.58571353580589));
#114927=CARTESIAN_POINT('Ctrl Pts',(-9.66278887903261,11.5469562561097,
9.57523488124948));
#114928=CARTESIAN_POINT('Ctrl Pts',(-9.81567343986054,11.5548302545749,
9.54374318844541));
#114929=CARTESIAN_POINT('Ctrl Pts',(-9.92887569317197,11.5601862287449,
9.53384843766438));
#114930=CARTESIAN_POINT('Ctrl Pts',(-10.0943802268656,11.5683921616117,
9.53860965573711));
#114931=CARTESIAN_POINT('Ctrl Pts',(-10.1465529279434,11.5710401837991,
9.54291711010381));
#114932=CARTESIAN_POINT('Ctrl Pts',(-10.2060242161885,11.5742376277456,
9.55105354171047));
#114933=CARTESIAN_POINT('Ctrl Pts',(-10.213662366315,11.574651720035,9.55216015916214));
#114934=CARTESIAN_POINT('Ctrl Pts',(-10.2253150581689,11.5752891813678,
9.55394262059777));
#114935=CARTESIAN_POINT('Ctrl Pts',(-10.2293362415998,11.575510204658,9.55457490424558));
#114936=CARTESIAN_POINT('Ctrl Pts',(-10.2366894778973,11.5759163696421,
9.55576257076315));
#114937=CARTESIAN_POINT('Ctrl Pts',(-10.2400222918119,11.5761012198466,
9.55631272090408));
#114938=CARTESIAN_POINT('Ctrl Pts',(-10.2475048866822,11.5765179358098,
9.55757450529623));
#114939=CARTESIAN_POINT('Ctrl Pts',(-10.2516534879026,11.5767501476157,
9.55829250614975));
#114940=CARTESIAN_POINT('Ctrl Pts',(-10.2622826857882,11.5773480023673,
9.56017938365066));
#114941=CARTESIAN_POINT('Ctrl Pts',(-10.2687585278728,11.5777150155759,
9.56137410528359));
#114942=CARTESIAN_POINT('Ctrl Pts',(-10.3085748111801,11.5799877157225,
9.56899798864811));
#114943=CARTESIAN_POINT('Ctrl Pts',(-10.3416889610966,11.5819474996295,
9.5765417177384));
#114944=CARTESIAN_POINT('Ctrl Pts',(-10.3882638754592,11.5847757388921,
9.58887070363993));
#114945=CARTESIAN_POINT('Ctrl Pts',(-10.401965451617,11.5856167567329,9.59271236512463));
#114946=CARTESIAN_POINT('Ctrl Pts',(-10.4227529164756,11.586904490152,9.5988691206094));
#114947=CARTESIAN_POINT('Ctrl Pts',(-10.4298809735023,11.587348186084,9.6010396301536));
#114948=CARTESIAN_POINT('Ctrl Pts',(-10.5385004210813,11.5941392658103,
9.63502304186722));
#114949=CARTESIAN_POINT('Ctrl Pts',(-10.6362569208829,11.6006193198647,
9.6777572439905));
#114950=CARTESIAN_POINT('Ctrl Pts',(-10.769536815379,11.609548489495,9.75425442627853));
#114951=CARTESIAN_POINT('Ctrl Pts',(-10.8093919713453,11.6122374739243,
9.77977285531112));
#114952=CARTESIAN_POINT('Ctrl Pts',(-10.8572905478218,11.6154914056674,
9.81382267231472));
#114953=CARTESIAN_POINT('Ctrl Pts',(-10.8665582505874,11.6161221631041,
9.82057618096684));
#114954=CARTESIAN_POINT('Ctrl Pts',(-10.8811929403732,11.6171202774378,
9.83150632270964));
#114955=CARTESIAN_POINT('Ctrl Pts',(-10.8866117158469,11.6174903128553,
9.83561254750769));
#114956=CARTESIAN_POINT('Ctrl Pts',(-10.8967985845378,11.6181869017374,
9.84344426914289));
#114957=CARTESIAN_POINT('Ctrl Pts',(-10.9015725559512,11.6185137519738,
9.84716185538678));
#114958=CARTESIAN_POINT('Ctrl Pts',(-10.9123271126009,11.6192510448913,
9.85564430457269));
#114959=CARTESIAN_POINT('Ctrl Pts',(-10.91829371158,11.6196607884903,9.86042666742356));
#114960=CARTESIAN_POINT('Ctrl Pts',(-10.9335908280592,11.6207132775376,
9.87288580951611));
#114961=CARTESIAN_POINT('Ctrl Pts',(-10.9428643493104,11.6213532607155,
9.88063184658284));
#114962=CARTESIAN_POINT('Ctrl Pts',(-11.022830065191,11.6268918776169,9.94912496147416));
#114963=CARTESIAN_POINT('Ctrl Pts',(-11.0876675785056,11.631501820198,10.0163834043436));
#114964=CARTESIAN_POINT('Ctrl Pts',(-11.1953770397652,11.6399426892902,
10.1518922052661));
#114965=CARTESIAN_POINT('Ctrl Pts',(-11.2398750237063,11.6437824786447,
10.2183853352463));
#114966=CARTESIAN_POINT('Ctrl Pts',(-11.2949577015895,11.6495171981335,
10.3173354497481));
#114967=CARTESIAN_POINT('Ctrl Pts',(-11.3101887256513,11.6512424445273,
10.3470440138117));
#114968=CARTESIAN_POINT('Ctrl Pts',(-11.3273431482387,11.6533953435391,
10.3835256803938));
#114969=CARTESIAN_POINT('Ctrl Pts',(-11.3302517077373,11.653768429802,10.3898272292362));
#114970=CARTESIAN_POINT('Ctrl Pts',(-11.3347261776431,11.6543555201815,
10.3997054694105));
#114971=CARTESIAN_POINT('Ctrl Pts',(-11.3363228208845,11.6545677174694,
10.4032682257474));
#114972=CARTESIAN_POINT('Ctrl Pts',(-11.339280855516,11.6549660212945,10.4099402058511));
#114973=CARTESIAN_POINT('Ctrl Pts',(-11.3406457019655,11.6551519181444,
10.4130478114445));
#114974=CARTESIAN_POINT('Ctrl Pts',(-11.34373882174,11.6555780695504,10.4201575790975));
#114975=CARTESIAN_POINT('Ctrl Pts',(-11.345460031113,11.6558187375606,10.4241627332253));
#114976=CARTESIAN_POINT('Ctrl Pts',(-11.3499910108855,11.6564616516842,
10.4348372833239));
#114977=CARTESIAN_POINT('Ctrl Pts',(-11.3527692127832,11.6568656693083,
10.4415198495659));
#114978=CARTESIAN_POINT('Ctrl Pts',(-11.3743479126688,11.6600811132635,
10.4945301359121));
#114979=CARTESIAN_POINT('Ctrl Pts',(-11.3908111221768,11.663008888266,10.5417691952744));
#114980=CARTESIAN_POINT('Ctrl Pts',(-11.4131984756936,11.6677619763251,
10.6184310231344));
#114981=CARTESIAN_POINT('Ctrl Pts',(-11.4206929841681,11.669556070806,10.6473582611478));
#114982=CARTESIAN_POINT('Ctrl Pts',(-11.4432326409644,11.6756901368494,
10.7468024114972));
#114983=CARTESIAN_POINT('Ctrl Pts',(-11.453952661775,11.6800311954178,10.81819682255));
#114984=CARTESIAN_POINT('Ctrl Pts',(-11.4621041968615,11.6863840911647,
10.9264352976285));
#114985=CARTESIAN_POINT('Ctrl Pts',(-11.4634828265411,11.6884853094528,
10.9628682430287));
#114986=CARTESIAN_POINT('Ctrl Pts',(-11.4634998405537,11.690547335478,10.9993168461169));
#114987=CARTESIAN_POINT('Origin',(-10.,3.5,11.));
#114988=CARTESIAN_POINT('',(-11.4635,12.2603577583743,11.0000000000809));
#114989=CARTESIAN_POINT('',(-11.4634994198187,12.1893450843268,11.0013031462968));
#114990=CARTESIAN_POINT('',(-11.4635,3.5,11.));
#114991=CARTESIAN_POINT('Ctrl Pts',(-11.4635,12.2603577583743,11.0000000000809));
#114992=CARTESIAN_POINT('Ctrl Pts',(-11.4635000000051,12.2548059746649,
10.9073254685672));
#114993=CARTESIAN_POINT('Ctrl Pts',(-11.4546974320718,12.2493769166143,
10.8148476026833));
#114994=CARTESIAN_POINT('Ctrl Pts',(-11.4349328125928,12.2435558897438,
10.711998698516));
#114995=CARTESIAN_POINT('Ctrl Pts',(-11.4325173017963,12.2428918921651,
10.7002148795474));
#114996=CARTESIAN_POINT('Ctrl Pts',(-11.4283326869135,12.2418141969465,
10.6810075377871));
#114997=CARTESIAN_POINT('Ctrl Pts',(-11.4266503480007,12.2413977910046,
10.6735658671736));
#114998=CARTESIAN_POINT('Ctrl Pts',(-11.4235302230986,12.2406546022506,
10.6602493131919));
#114999=CARTESIAN_POINT('Ctrl Pts',(-11.4221140747212,12.240327143294,10.6543695828532));
#115000=CARTESIAN_POINT('Ctrl Pts',(-11.4190266597989,12.239633582581,10.6418911880217));
#115001=CARTESIAN_POINT('Ctrl Pts',(-11.4173457178811,12.2392677969016,
10.6352950499755));
#115002=CARTESIAN_POINT('Ctrl Pts',(-11.4126992279587,12.2382874969709,
10.6175793218541));
#115003=CARTESIAN_POINT('Ctrl Pts',(-11.4096484108479,12.2376757086318,
10.6064824634673));
#115004=CARTESIAN_POINT('Ctrl Pts',(-11.3932251538891,12.2345382837069,
10.5493889029438));
#115005=CARTESIAN_POINT('Ctrl Pts',(-11.3777306688271,12.2320815545049,
10.5040307602516));
#115006=CARTESIAN_POINT('Ctrl Pts',(-11.3195491799641,12.224170028088,10.3576280633855));
#115007=CARTESIAN_POINT('Ctrl Pts',(-11.2677430341436,12.2189814486879,
10.2606231323323));
#115008=CARTESIAN_POINT('Ctrl Pts',(-11.1769872196089,12.2110382755514,
10.128748398086));
#115009=CARTESIAN_POINT('Ctrl Pts',(-11.1462536186344,12.2084814995651,
10.0886932687176));
#115010=CARTESIAN_POINT('Ctrl Pts',(-11.1088113422629,12.2054110500189,
10.0447920471613));
#115011=CARTESIAN_POINT('Ctrl Pts',(-11.1040652484266,12.2050225902678,
10.039310274393));
#115012=CARTESIAN_POINT('Ctrl Pts',(-11.0963984611413,12.2043958392435,
10.0305869300754));
#115013=CARTESIAN_POINT('Ctrl Pts',(-11.0935036073444,12.204159359192,10.0273226920158));
#115014=CARTESIAN_POINT('Ctrl Pts',(-11.0883310000833,12.2037370111398,
10.0215423345221));
#115015=CARTESIAN_POINT('Ctrl Pts',(-11.0860590368975,12.2035515679007,
10.0190211332302));
#115016=CARTESIAN_POINT('Ctrl Pts',(-11.0811572689418,12.2031515810018,
10.0136195350622));
#115017=CARTESIAN_POINT('Ctrl Pts',(-11.0785247560787,12.2029368416973,
10.010741787198));
#115018=CARTESIAN_POINT('Ctrl Pts',(-11.0711861694832,12.2023385143601,
10.0027836755638));
#115019=CARTESIAN_POINT('Ctrl Pts',(-11.0664555535178,12.2019531539081,
9.9977262070975));
#115020=CARTESIAN_POINT('Ctrl Pts',(-11.038882781628,12.1997099873192,9.96866456397212));
#115021=CARTESIAN_POINT('Ctrl Pts',(-11.0152680514787,12.1978005197452,
9.9454097122866));
#115022=CARTESIAN_POINT('Ctrl Pts',(-10.932943887834,12.1912433901656,9.86966947375594));
#115023=CARTESIAN_POINT('Ctrl Pts',(-10.8707955870396,12.1864618595326,
9.82112513581298));
#115024=CARTESIAN_POINT('Ctrl Pts',(-10.7259178908006,12.1760619507911,
9.72569494404273));
#115025=CARTESIAN_POINT('Ctrl Pts',(-10.6419046781459,12.1705043963497,
9.68137431195839));
#115026=CARTESIAN_POINT('Ctrl Pts',(-10.5430705873411,12.164569381805,9.64093754359289));
#115027=CARTESIAN_POINT('Ctrl Pts',(-10.5319017711133,12.1639065613599,
9.63652761628501));
#115028=CARTESIAN_POINT('Ctrl Pts',(-10.5135558057522,12.1628303988043,
9.62954358365076));
#115029=CARTESIAN_POINT('Ctrl Pts',(-10.5064107323465,12.1624143607992,
9.62688728504845));
#115030=CARTESIAN_POINT('Ctrl Pts',(-10.4935611252204,12.161671597705,9.62222417336057));
#115031=CARTESIAN_POINT('Ctrl Pts',(-10.4878643279251,12.1613441992047,
9.62019667638689));
#115032=CARTESIAN_POINT('Ctrl Pts',(-10.4757251913483,12.1606505269177,
9.6159609220166));
#115033=CARTESIAN_POINT('Ctrl Pts',(-10.4692796600842,12.1602845710383,
9.61376220299878));
#115034=CARTESIAN_POINT('Ctrl Pts',(-10.4518860353491,12.1593032379807,
9.60796405518009));
#115035=CARTESIAN_POINT('Ctrl Pts',(-10.4409102653362,12.1586905974093,
9.60444877965924));
#115036=CARTESIAN_POINT('Ctrl Pts',(-10.383876467884,12.1555397068102,9.58692226507335));
#115037=CARTESIAN_POINT('Ctrl Pts',(-10.3371869458659,12.1530711108834,
9.57505951298429));
#115038=CARTESIAN_POINT('Ctrl Pts',(-10.181226427311,12.145082463203,9.54353058818045));
#115039=CARTESIAN_POINT('Ctrl Pts',(-10.070317629146,12.1398361262459,9.5339849224058));
#115040=CARTESIAN_POINT('Ctrl Pts',(-9.93941505871758,12.1333293657368,
9.53761791554359));
#115041=CARTESIAN_POINT('Ctrl Pts',(-9.91944561469846,12.1323271295369,
9.53858190722312));
#115042=CARTESIAN_POINT('Ctrl Pts',(-9.8690636967917,12.1297611654952,9.54204977377601));
#115043=CARTESIAN_POINT('Ctrl Pts',(-9.83869956372696,12.1281802200906,
9.54509618940577));
#115044=CARTESIAN_POINT('Ctrl Pts',(-9.80151793989404,12.1261782967226,
9.55000479907706));
#115045=CARTESIAN_POINT('Ctrl Pts',(-9.79458771849976,12.1258023228816,
9.55097032410739));
#115046=CARTESIAN_POINT('Ctrl Pts',(-9.78374890645254,12.1252094877737,
9.55255971498088));
#115047=CARTESIAN_POINT('Ctrl Pts',(-9.77983537985621,12.1249944501264,
9.55314981651763));
#115048=CARTESIAN_POINT('Ctrl Pts',(-9.77257887999176,12.1245938178299,
9.55427411140282));
#115049=CARTESIAN_POINT('Ctrl Pts',(-9.76923532733898,12.1244084602799,
9.55480403545743));
#115050=CARTESIAN_POINT('Ctrl Pts',(-9.76159997108689,12.1239834531014,
9.55604134547359));
#115051=CARTESIAN_POINT('Ctrl Pts',(-9.75730947576301,12.1237433919598,
9.55675626513817));
#115052=CARTESIAN_POINT('Ctrl Pts',(-9.74404741984771,12.1229976556589,
9.55902691344309));
#115053=CARTESIAN_POINT('Ctrl Pts',(-9.73508731533925,12.1224885767231,
9.56064722167714));
#115054=CARTESIAN_POINT('Ctrl Pts',(-9.71418407045161,12.1212895864138,
9.56462906759807));
#115055=CARTESIAN_POINT('Ctrl Pts',(-9.70225423868412,12.1205966079204,
9.56705621084313));
#115056=CARTESIAN_POINT('Ctrl Pts',(-9.66033000443401,12.1181338657539,
9.57613189438323));
#115057=CARTESIAN_POINT('Ctrl Pts',(-9.63051722765552,12.1163329555175,
9.58357549943435));
#115058=CARTESIAN_POINT('Ctrl Pts',(-9.53674198267762,12.1105532686362,
9.61015116941723));
#115059=CARTESIAN_POINT('Ctrl Pts',(-9.47384269054574,12.1065077713021,
9.63272309724021));
#115060=CARTESIAN_POINT('Ctrl Pts',(-9.32735953324229,12.0969250660342,
9.69690027953282));
#115061=CARTESIAN_POINT('Ctrl Pts',(-9.24576967904837,12.091464213834,9.74236109430823));
#115062=CARTESIAN_POINT('Ctrl Pts',(-9.15908229161052,12.0856101219716,
9.8021535144291));
#115063=CARTESIAN_POINT('Ctrl Pts',(-9.1492027114298,12.0849417668494,9.80915039515757));
#115064=CARTESIAN_POINT('Ctrl Pts',(-9.13322143189497,12.0838584770434,
9.82076901274582));
#115065=CARTESIAN_POINT('Ctrl Pts',(-9.12706730216103,12.0834407863807,
9.82531735538098));
#115066=CARTESIAN_POINT('Ctrl Pts',(-9.1161122930673,12.0826962046614,9.83354752794579));
#115067=CARTESIAN_POINT('Ctrl Pts',(-9.11129806775944,12.0823686270161,
9.83721122933819));
#115068=CARTESIAN_POINT('Ctrl Pts',(-9.1011276182116,12.0816757453845,9.84505116206975));
#115069=CARTESIAN_POINT('Ctrl Pts',(-9.09577745751848,12.0813107502746,
9.84923504886328));
#115070=CARTESIAN_POINT('Ctrl Pts',(-9.08149370477378,12.0803348016928,
9.86056622723117));
#115071=CARTESIAN_POINT('Ctrl Pts',(-9.07261437602079,12.0797265321294,
9.86778135893339));
#115072=CARTESIAN_POINT('Ctrl Pts',(-9.02772556506568,12.0766419107304,
9.90513933710712));
#115073=CARTESIAN_POINT('Ctrl Pts',(-8.99309559981289,12.074231625155,9.93690003354028));
#115074=CARTESIAN_POINT('Ctrl Pts',(-8.88640550605975,12.0666095479148,
10.0446493225219));
#115075=CARTESIAN_POINT('Ctrl Pts',(-8.82095494826308,12.0616373535182,
10.1267074767315));
#115076=CARTESIAN_POINT('Ctrl Pts',(-8.73459889633989,12.0536880857346,
10.2625947504823));
#115077=CARTESIAN_POINT('Ctrl Pts',(-8.7071545206653,12.0508506118036,10.3118461270923));
#115078=CARTESIAN_POINT('Ctrl Pts',(-8.67911761104667,12.0474262492691,
10.3697884399054));
#115079=CARTESIAN_POINT('Ctrl Pts',(-8.67567533345731,12.0469953178371,
10.3770545226679));
#115080=CARTESIAN_POINT('Ctrl Pts',(-8.67053080171456,12.046334498301,10.3881491584753));
#115081=CARTESIAN_POINT('Ctrl Pts',(-8.66878477456983,12.0461071697904,
10.391957382938));
#115082=CARTESIAN_POINT('Ctrl Pts',(-8.66566112536145,12.0456948283028,
10.3988482570086));
#115083=CARTESIAN_POINT('Ctrl Pts',(-8.66427779567627,12.0455101631393,
10.401928229283));
#115084=CARTESIAN_POINT('Ctrl Pts',(-8.6612435286354,12.0451005162417,10.4087470386492));
#115085=CARTESIAN_POINT('Ctrl Pts',(-8.65959760765169,12.0448752466374,
10.4124879748611));
#115086=CARTESIAN_POINT('Ctrl Pts',(-8.65485628996998,12.0442174497102,
10.423387927128));
#115087=CARTESIAN_POINT('Ctrl Pts',(-8.65180247527174,12.0437825520738,
10.4305647428377));
#115088=CARTESIAN_POINT('Ctrl Pts',(-8.62749121198827,12.0402296517615,
10.4889909422773));
#115089=CARTESIAN_POINT('Ctrl Pts',(-8.60910842535902,12.0369679878286,
10.5413824395642));
#115090=CARTESIAN_POINT('Ctrl Pts',(-8.55399259994106,12.0250888368134,
10.7326087439801));
#115091=CARTESIAN_POINT('Ctrl Pts',(-8.53473776357802,12.0163479269612,
10.8756691694954));
#115092=CARTESIAN_POINT('Ctrl Pts',(-8.53685348325511,12.0073464281386,
11.0364960509889));
#115093=CARTESIAN_POINT('Ctrl Pts',(-8.53738516658651,12.0063904543788,
11.0537361687143));
#115094=CARTESIAN_POINT('Ctrl Pts',(-8.53860391863576,12.0050109499559,
11.0788413030466));
#115095=CARTESIAN_POINT('Ctrl Pts',(-8.53905004193811,12.0045800409144,
11.0867160949721));
#115096=CARTESIAN_POINT('Ctrl Pts',(-8.53995381605657,12.0038195608795,
11.1006705281967));
#115097=CARTESIAN_POINT('Ctrl Pts',(-8.54038583399948,12.0034892061035,
11.1067515923067));
#115098=CARTESIAN_POINT('Ctrl Pts',(-8.54136469399968,12.0028036323156,
11.1194104580995));
#115099=CARTESIAN_POINT('Ctrl Pts',(-8.54191806356541,12.0024486230723,
11.1259876263951));
#115100=CARTESIAN_POINT('Ctrl Pts',(-8.54347304899,12.0015288021931,11.1430844211263));
#115101=CARTESIAN_POINT('Ctrl Pts',(-8.54454414567865,12.0009661493641,
11.1535974430187));
#115102=CARTESIAN_POINT('Ctrl Pts',(-8.54982498712061,11.9984736826175,
11.2003973328238));
#115103=CARTESIAN_POINT('Ctrl Pts',(-8.55527874288746,11.9965825318892,
11.2365320918327));
#115104=CARTESIAN_POINT('Ctrl Pts',(-8.57432477963348,11.9913799573634,
11.3370606429539));
#115105=CARTESIAN_POINT('Ctrl Pts',(-8.59091464485725,11.9881528734285,
11.4007978902761));
#115106=CARTESIAN_POINT('Ctrl Pts',(-8.64423644301081,11.9799453178317,
11.5606075965663));
#115107=CARTESIAN_POINT('Ctrl Pts',(-8.68689202115462,11.9750266073954,
11.6543071253193));
#115108=CARTESIAN_POINT('Ctrl Pts',(-8.74456251159488,11.9690328458795,
11.7522163493403));
#115109=CARTESIAN_POINT('Ctrl Pts',(-8.75023915335709,11.9684482528034,
11.7616104881095));
#115110=CARTESIAN_POINT('Ctrl Pts',(-8.758314866178,11.967622719986,11.7746413650166));
#115111=CARTESIAN_POINT('Ctrl Pts',(-8.76062546216422,11.9673871987733,
11.7783328143804));
#115112=CARTESIAN_POINT('Ctrl Pts',(-8.76464702000663,11.9669783423139,
11.7846944129708));
#115113=CARTESIAN_POINT('Ctrl Pts',(-8.76635026159977,11.966805504622,11.7873694364642));
#115114=CARTESIAN_POINT('Ctrl Pts',(-8.76996041578092,11.9664397960954,
11.7929988879357));
#115115=CARTESIAN_POINT('Ctrl Pts',(-8.77186929701796,11.966246792018,11.7959520027421));
#115116=CARTESIAN_POINT('Ctrl Pts',(-8.77661225173234,11.9657681937331,
11.8032318596183));
#115117=CARTESIAN_POINT('Ctrl Pts',(-8.77945864011871,11.9654818043323,
11.8075504876417));
#115118=CARTESIAN_POINT('Ctrl Pts',(-8.79012115710668,11.9644123341662,
11.8235428365423));
#115119=CARTESIAN_POINT('Ctrl Pts',(-8.79808211699375,11.9636204154628,
11.8351185490441));
#115120=CARTESIAN_POINT('Ctrl Pts',(-8.85658456097778,11.95785762137,11.9176151265116));
#115121=CARTESIAN_POINT('Ctrl Pts',(-8.9131975903255,11.952588506484,11.9840095898735));
#115122=CARTESIAN_POINT('Ctrl Pts',(-9.04738992528469,11.9412851037012,
12.1155893772728));
#115123=CARTESIAN_POINT('Ctrl Pts',(-9.12652587627735,11.9353026248179,
12.1785815153733));
#115124=CARTESIAN_POINT('Ctrl Pts',(-9.22712181784205,11.9286061533182,
12.2429136713676));
#115125=CARTESIAN_POINT('Ctrl Pts',(-9.24290884947954,11.9275783753904,
12.2525925565333));
#115126=CARTESIAN_POINT('Ctrl Pts',(-9.26524176343757,11.9261558976793,
12.2657081360948));
#115127=CARTESIAN_POINT('Ctrl Pts',(-9.2716359759257,11.9257521532284,12.2693985202424));
#115128=CARTESIAN_POINT('Ctrl Pts',(-9.28341395702334,11.9250148360302,
12.2760778212882));
#115129=CARTESIAN_POINT('Ctrl Pts',(-9.28878916259913,11.924680746424,12.2790814318645));
#115130=CARTESIAN_POINT('Ctrl Pts',(-9.29974159867636,11.9240048179416,
12.2851111551536));
#115131=CARTESIAN_POINT('Ctrl Pts',(-9.30531987602035,11.9236630604178,
12.2881351003707));
#115132=CARTESIAN_POINT('Ctrl Pts',(-9.31919064809662,11.9228193499423,
12.2955380400237));
#115133=CARTESIAN_POINT('Ctrl Pts',(-9.32750596275297,11.9223189117851,
12.2998738254677));
#115134=CARTESIAN_POINT('Ctrl Pts',(-9.35915766562077,11.920433661042,12.3159926872941));
#115135=CARTESIAN_POINT('Ctrl Pts',(-9.38276733800983,11.9190676086697,
12.3272300482196));
#115136=CARTESIAN_POINT('Ctrl Pts',(-9.44331449664166,11.9156543676327,
12.3540829978543));
#115137=CARTESIAN_POINT('Ctrl Pts',(-9.4806165080502,11.9136344385394,12.3688245319763));
#115138=CARTESIAN_POINT('Ctrl Pts',(-9.57945121937701,11.9084383659812,
12.4032604703767));
#115139=CARTESIAN_POINT('Ctrl Pts',(-9.64176408505081,11.9053171411273,
12.4204465781561));
#115140=CARTESIAN_POINT('Ctrl Pts',(-9.7786354195135,11.8985047848275,12.4486133100641));
#115141=CARTESIAN_POINT('Ctrl Pts',(-9.85331323675533,11.8948139309531,
12.4580683829241));
#115142=CARTESIAN_POINT('Ctrl Pts',(-9.94039336046036,11.8902271089276,
12.4623351281179));
#115143=CARTESIAN_POINT('Ctrl Pts',(-9.95241568093956,11.889587541225,12.4627756809019));
#115144=CARTESIAN_POINT('Ctrl Pts',(-9.96944876114729,11.8886707976507,
12.4631896519195));
#115145=CARTESIAN_POINT('Ctrl Pts',(-9.97445636122614,11.8883999833124,
12.4632856374339));
#115146=CARTESIAN_POINT('Ctrl Pts',(-9.98291319048334,11.8879402948549,
12.4634043146915));
#115147=CARTESIAN_POINT('Ctrl Pts',(-9.98636223924958,11.8877521577671,
12.4634405210253));
#115148=CARTESIAN_POINT('Ctrl Pts',(-9.99344872588289,11.8873642028206,
12.4634898570841));
#115149=CARTESIAN_POINT('Ctrl Pts',(-9.99708612032296,11.8871643150776,
12.4635016192993));
#115150=CARTESIAN_POINT('Ctrl Pts',(-10.0064588771287,11.8866473675899,
12.4634969858861));
#115151=CARTESIAN_POINT('Ctrl Pts',(-10.0121941120456,11.8863292298372,
12.4634604354747));
#115152=CARTESIAN_POINT('Ctrl Pts',(-10.0364267107871,11.8849777835674,
12.4631635471214));
#115153=CARTESIAN_POINT('Ctrl Pts',(-10.0549177208273,11.883928714258,12.4625862196702));
#115154=CARTESIAN_POINT('Ctrl Pts',(-10.1050100814931,11.8810472718436,
12.4600710127188));
#115155=CARTESIAN_POINT('Ctrl Pts',(-10.1365667759029,11.8791894598557,
12.4574579846259));
#115156=CARTESIAN_POINT('Ctrl Pts',(-10.2655120137174,11.8714846040999,
12.442556350046));
#115157=CARTESIAN_POINT('Ctrl Pts',(-10.3616331145905,11.865494497724,12.4215093552516));
#115158=CARTESIAN_POINT('Ctrl Pts',(-10.5133055760395,11.8560994955007,
12.3719045139553));
#115159=CARTESIAN_POINT('Ctrl Pts',(-10.5704274783732,11.8525701630846,
12.3491547706635));
#115160=CARTESIAN_POINT('Ctrl Pts',(-10.6364068692296,11.8485172306536,
12.3179348270918));
#115161=CARTESIAN_POINT('Ctrl Pts',(-10.64679846414,11.84787949189,12.3128662038372));
#115162=CARTESIAN_POINT('Ctrl Pts',(-10.6638191353195,11.8468357002052,
12.3043130237419));
#115163=CARTESIAN_POINT('Ctrl Pts',(-10.6704833373149,11.8464272162831,
12.3008998445705));
#115164=CARTESIAN_POINT('Ctrl Pts',(-10.682349601798,11.8457001434379,12.2947069372998));
#115165=CARTESIAN_POINT('Ctrl Pts',(-10.6875615727535,11.8453808890408,
12.2919466388532));
#115166=CARTESIAN_POINT('Ctrl Pts',(-10.6986504977495,11.8447017924644,
12.2859877521747));
#115167=CARTESIAN_POINT('Ctrl Pts',(-10.704522503127,11.8443422730469,12.2827802077367));
#115168=CARTESIAN_POINT('Ctrl Pts',(-10.7165546524216,11.8436056795521,
12.2761001846483));
#115169=CARTESIAN_POINT('Ctrl Pts',(-10.7227120459811,11.8432287788758,
12.272623098998));
#115170=CARTESIAN_POINT('Ctrl Pts',(-10.7380589061946,11.8422893440294,
12.2638094081906));
#115171=CARTESIAN_POINT('Ctrl Pts',(-10.7472159814269,11.8417287759056,
12.2584170429673));
#115172=CARTESIAN_POINT('Ctrl Pts',(-10.7730028698787,11.84014939064,12.242851090319));
#115173=CARTESIAN_POINT('Ctrl Pts',(-10.7894895581006,11.8391387027473,
12.2324441370172));
#115174=CARTESIAN_POINT('Ctrl Pts',(-10.8448405796337,11.8357359084201,
12.1959380648638));
#115175=CARTESIAN_POINT('Ctrl Pts',(-10.8826599310488,11.8333954347197,
12.1683044681025));
#115176=CARTESIAN_POINT('Ctrl Pts',(-10.9755601415778,11.8275113879887,
12.0933343409568));
#115177=CARTESIAN_POINT('Ctrl Pts',(-11.0285603759722,11.8240255258427,
12.0436287391181));
#115178=CARTESIAN_POINT('Ctrl Pts',(-11.1199840400863,11.8173834963673,
11.9441302713563));
#115179=CARTESIAN_POINT('Ctrl Pts',(-11.1593112561158,11.8142528259374,
11.8954004525021));
#115180=CARTESIAN_POINT('Ctrl Pts',(-11.2000847119548,11.8104939784547,
11.8376723589042));
#115181=CARTESIAN_POINT('Ctrl Pts',(-11.2047177453511,11.8100584889564,
11.8309954541469));
#115182=CARTESIAN_POINT('Ctrl Pts',(-11.2116649693189,11.8093920516097,
11.8208032412061));
#115183=CARTESIAN_POINT('Ctrl Pts',(-11.2140200761227,11.8091637293957,
11.8173158584814));
#115184=CARTESIAN_POINT('Ctrl Pts',(-11.2182379568744,11.8087503699657,
11.811011673547));
#115185=CARTESIAN_POINT('Ctrl Pts',(-11.2201060554532,11.8085656892533,
11.8081985320733));
#115186=CARTESIAN_POINT('Ctrl Pts',(-11.2242043130961,11.8081569661181,
11.8019804340152));
#115187=CARTESIAN_POINT('Ctrl Pts',(-11.2264299852938,11.8079326439324,
11.7985726686392));
#115188=CARTESIAN_POINT('Ctrl Pts',(-11.2328354766852,11.8072802874163,
11.7886751708793));
#115189=CARTESIAN_POINT('Ctrl Pts',(-11.2369781376446,11.8068499407652,
11.7821616964879));
#115190=CARTESIAN_POINT('Ctrl Pts',(-11.2688508272659,11.8034742444762,
11.7311619600476));
#115191=CARTESIAN_POINT('Ctrl Pts',(-11.2942216581094,11.8004004055587,
11.6852514067206));
#115192=CARTESIAN_POINT('Ctrl Pts',(-11.369044800095,11.7901749755661,11.5308085307833));
#115193=CARTESIAN_POINT('Ctrl Pts',(-11.407723773277,11.7828982666145,11.4175664497123));
#115194=CARTESIAN_POINT('Ctrl Pts',(-11.4399883204299,11.7738639909726,
11.2639840358877));
#115195=CARTESIAN_POINT('Ctrl Pts',(-11.4463117504704,11.7717332821447,
11.2267964202192));
#115196=CARTESIAN_POINT('Ctrl Pts',(-11.4526286991968,11.7690328257708,
11.1783965519156));
#115197=CARTESIAN_POINT('Ctrl Pts',(-11.4539400364801,11.7684225837634,
11.1673733768493));
#115198=CARTESIAN_POINT('Ctrl Pts',(-11.4558434087634,11.7674493197095,
11.1496574067769));
#115199=CARTESIAN_POINT('Ctrl Pts',(-11.4565149777432,11.7670838442857,
11.1429737456393));
#115200=CARTESIAN_POINT('Ctrl Pts',(-11.4576884218097,11.7664009218756,
11.1304274997349));
#115201=CARTESIAN_POINT('Ctrl Pts',(-11.4582010022206,11.7660831495338,
11.1245660719387));
#115202=CARTESIAN_POINT('Ctrl Pts',(-11.459153545937,11.7654510448967,11.1128606344265));
#115203=CARTESIAN_POINT('Ctrl Pts',(-11.4595937819835,11.7651367098116,
11.1070167574441));
#115204=CARTESIAN_POINT('Ctrl Pts',(-11.4605169322783,11.7644228827377,
11.0936946861254));
#115205=CARTESIAN_POINT('Ctrl Pts',(-11.4609775380424,11.7640240816738,
11.0862150786803));
#115206=CARTESIAN_POINT('Ctrl Pts',(-11.4628044140944,11.7622246781202,
11.0523056692109));
#115207=CARTESIAN_POINT('Ctrl Pts',(-11.4635111105567,11.7608442923582,
11.025844731747));
#115208=CARTESIAN_POINT('Ctrl Pts',(-11.4634998679599,11.7594829657366,
10.9993783236864));
#115209=CARTESIAN_POINT('Ctrl Pts',(-11.4634998405537,11.690547335478,10.9993168461169));
#115210=CARTESIAN_POINT('Ctrl Pts',(-11.4635110117752,11.6919012400444,
11.023248614949));
#115211=CARTESIAN_POINT('Ctrl Pts',(-11.4629351707176,11.693237851355,11.0471779657481));
#115212=CARTESIAN_POINT('Ctrl Pts',(-11.4613190077038,11.6950711538873,
11.0804130227707));
#115213=CARTESIAN_POINT('Ctrl Pts',(-11.4607760139058,11.6955830245042,
11.0897381711136));
#115214=CARTESIAN_POINT('Ctrl Pts',(-11.4597576234224,11.6964030878732,
11.1047495986055));
#115215=CARTESIAN_POINT('Ctrl Pts',(-11.4593381917171,11.6967130012465,
11.1104393092238));
#115216=CARTESIAN_POINT('Ctrl Pts',(-11.4583977047227,11.6973547198214,
11.1222545545916));
#115217=CARTESIAN_POINT('Ctrl Pts',(-11.457871301458,11.6976863529116,11.1283795592229));
#115218=CARTESIAN_POINT('Ctrl Pts',(-11.4565399129737,11.6984650497468,
11.1428050205016));
#115219=CARTESIAN_POINT('Ctrl Pts',(-11.4557025398489,11.6989111016444,
11.151102320701));
#115220=CARTESIAN_POINT('Ctrl Pts',(-11.4526923246627,11.7003823114869,
11.1785769763488));
#115221=CARTESIAN_POINT('Ctrl Pts',(-11.4502110205741,11.70139792342,11.1977189114103));
#115222=CARTESIAN_POINT('Ctrl Pts',(-11.4434001245814,11.7037915102701,
11.243186872661));
#115223=CARTESIAN_POINT('Ctrl Pts',(-11.4387278955424,11.7051591633226,
11.2694548588893));
#115224=CARTESIAN_POINT('Ctrl Pts',(-11.4176628825599,11.7104392807719,
11.3716037768903));
#115225=CARTESIAN_POINT('Ctrl Pts',(-11.3959617091636,11.7142074138894,
11.4462613099121));
#115226=CARTESIAN_POINT('Ctrl Pts',(-11.3382945830485,11.7221239245019,
11.5983565033105));
#115227=CARTESIAN_POINT('Ctrl Pts',(-11.3012792295772,11.7262611852359,
11.6750792636379));
#115228=CARTESIAN_POINT('Ctrl Pts',(-11.2517321146167,11.7313617765336,
11.7583803635228));
#115229=CARTESIAN_POINT('Ctrl Pts',(-11.2455199461069,11.7319949932516,
11.7685402452513));
#115230=CARTESIAN_POINT('Ctrl Pts',(-11.2367921393787,11.7328777297301,
11.782430621376));
#115231=CARTESIAN_POINT('Ctrl Pts',(-11.2343820864251,11.7331207834384,
11.7862272807159));
#115232=CARTESIAN_POINT('Ctrl Pts',(-11.2302224556582,11.7335391966889,
11.7927138550937));
#115233=CARTESIAN_POINT('Ctrl Pts',(-11.2284814442481,11.7337140031849,
11.795409257675));
#115234=CARTESIAN_POINT('Ctrl Pts',(-11.2248326494808,11.7340797439245,
11.8010177003377));
#115235=CARTESIAN_POINT('Ctrl Pts',(-11.2229233244739,11.7342707848579,
11.803929671737));
#115236=CARTESIAN_POINT('Ctrl Pts',(-11.2182492911315,11.7347375739999,
11.8110030058457));
#115237=CARTESIAN_POINT('Ctrl Pts',(-11.2154736412383,11.7350140333436,
11.8151570626571));
#115238=CARTESIAN_POINT('Ctrl Pts',(-11.2054821914291,11.7360063349114,
11.8299458426191));
#115239=CARTESIAN_POINT('Ctrl Pts',(-11.1981478517334,11.736729478913,11.8404993265583));
#115240=CARTESIAN_POINT('Ctrl Pts',(-11.1795644907716,11.7385461431458,
11.866501607227));
#115241=CARTESIAN_POINT('Ctrl Pts',(-11.1681502456499,11.739648345848,11.8818289889599));
#115242=CARTESIAN_POINT('Ctrl Pts',(-11.1178625270516,11.7444324664026,
11.9466666622002));
#115243=CARTESIAN_POINT('Ctrl Pts',(-11.0761184031524,11.7482238468011,
11.9938625965223));
#115244=CARTESIAN_POINT('Ctrl Pts',(-10.9549528328743,11.7585020099576,
12.1142399248257));
#115245=CARTESIAN_POINT('Ctrl Pts',(-10.8702564604242,11.7649248297365,
12.1815778704343));
#115246=CARTESIAN_POINT('Ctrl Pts',(-10.7634618307599,11.7719962085118,
12.2487159501406));
#115247=CARTESIAN_POINT('Ctrl Pts',(-10.7478263365112,11.7730092245914,
12.2581420045889));
#115248=CARTESIAN_POINT('Ctrl Pts',(-10.7250312781815,11.7744548611267,
12.2713091671595));
#115249=CARTESIAN_POINT('Ctrl Pts',(-10.7180111394805,11.7748958889714,
12.2752871676856));
#115250=CARTESIAN_POINT('Ctrl Pts',(-10.7056034514141,11.7756681548096,
12.2821831194939));
#115251=CARTESIAN_POINT('Ctrl Pts',(-10.7002298511229,11.7760002562438,
12.285125651342));
#115252=CARTESIAN_POINT('Ctrl Pts',(-10.6890941349368,11.7766836814334,
12.2911328802317));
#115253=CARTESIAN_POINT('Ctrl Pts',(-10.6833296715704,11.7770348378461,
12.2941929543368));
#115254=CARTESIAN_POINT('Ctrl Pts',(-10.6684843208565,11.7779325796945,
12.3019467929988));
#115255=CARTESIAN_POINT('Ctrl Pts',(-10.6593742949861,11.7784772017356,
12.3065842051738));
#115256=CARTESIAN_POINT('Ctrl Pts',(-10.6205278844389,11.7807738206129,
12.3258489980042));
#115257=CARTESIAN_POINT('Ctrl Pts',(-10.5903467332848,11.7824944482346,
12.3395601405463));
#115258=CARTESIAN_POINT('Ctrl Pts',(-10.5075283757096,11.7870709311126,
12.3738407552375));
#115259=CARTESIAN_POINT('Ctrl Pts',(-10.4541228284109,11.7898669502416,
12.3924067467507));
#115260=CARTESIAN_POINT('Ctrl Pts',(-10.3532740435257,11.7949954785566,
12.4210441280469));
#115261=CARTESIAN_POINT('Ctrl Pts',(-10.3061475759296,11.7973340620579,
12.4319366592589));
#115262=CARTESIAN_POINT('Ctrl Pts',(-10.1875682578389,11.8032257602593,
12.4532219024205));
#115263=CARTESIAN_POINT('Ctrl Pts',(-10.1157303474011,11.8068007674967,
12.4606984117221));
#115264=CARTESIAN_POINT('Ctrl Pts',(-10.0354923283458,11.8110697324395,
12.4630922897331));
#115265=CARTESIAN_POINT('Ctrl Pts',(-10.0273392723034,11.8115066978225,
12.4632673411975));
#115266=CARTESIAN_POINT('Ctrl Pts',(-10.0149708413075,11.8121749900491,
12.4634294957998));
#115267=CARTESIAN_POINT('Ctrl Pts',(-10.0107561514835,11.8124036700102,
12.4634665420066));
#115268=CARTESIAN_POINT('Ctrl Pts',(-10.0031632908043,11.8128174483842,
12.4635004801965));
#115269=CARTESIAN_POINT('Ctrl Pts',(-9.99978523063362,11.8130021875297,
12.4635038829548));
#115270=CARTESIAN_POINT('Ctrl Pts',(-9.99234057179896,11.8134107649638,
12.4634856064393));
#115271=CARTESIAN_POINT('Ctrl Pts',(-9.98827411070654,11.8136348808513,
12.4634586737577));
#115272=CARTESIAN_POINT('Ctrl Pts',(-9.97650959394823,11.8142858787328,
12.4633317194362));
#115273=CARTESIAN_POINT('Ctrl Pts',(-9.96881226615034,11.8147150579741,
12.4631879032821));
#115274=CARTESIAN_POINT('Ctrl Pts',(-9.90949647449959,11.8180454556237,
12.4616113990794));
#115275=CARTESIAN_POINT('Ctrl Pts',(-9.8579897214329,11.8210714072089,12.4575084372319));
#115276=CARTESIAN_POINT('Ctrl Pts',(-9.69745368511258,11.8307165385426,
12.4361300436332));
#115277=CARTESIAN_POINT('Ctrl Pts',(-9.59007704654421,11.8374498201066,
12.4092449579377));
#115278=CARTESIAN_POINT('Ctrl Pts',(-9.44368260530488,11.8465281658592,
12.3544213684133));
#115279=CARTESIAN_POINT('Ctrl Pts',(-9.40140523225442,11.8491423945864,
12.3362751351717));
#115280=CARTESIAN_POINT('Ctrl Pts',(-9.34952205362358,11.852339245398,12.3110483235708));
#115281=CARTESIAN_POINT('Ctrl Pts',(-9.33905667484916,11.8529835608785,
12.3058036596419));
#115282=CARTESIAN_POINT('Ctrl Pts',(-9.32250811324443,11.8540017730185,
12.2972605171938));
#115283=CARTESIAN_POINT('Ctrl Pts',(-9.31638360595431,11.85437846987,12.2940435596092));
#115284=CARTESIAN_POINT('Ctrl Pts',(-9.30495923376991,11.8550809579258,
12.2879390534127));
#115285=CARTESIAN_POINT('Ctrl Pts',(-9.29965399339151,11.8554071034629,
12.2850619224599));
#115286=CARTESIAN_POINT('Ctrl Pts',(-9.2878241277172,11.8561342560457,12.2785513467937));
#115287=CARTESIAN_POINT('Ctrl Pts',(-9.2813091850471,11.8565346434405,12.2749005979892));
#115288=CARTESIAN_POINT('Ctrl Pts',(-9.26211710165048,11.8577141160207,
12.2639521491568));
#115289=CARTESIAN_POINT('Ctrl Pts',(-9.24952090630249,11.8584882066064,
12.2565139701634));
#115290=CARTESIAN_POINT('Ctrl Pts',(-9.22109322533103,11.8602365578425,
12.2391471293402));
#115291=CARTESIAN_POINT('Ctrl Pts',(-9.20533601634961,11.8612066149366,
12.2291015269812));
#115292=CARTESIAN_POINT('Ctrl Pts',(-9.15319414696045,11.8644253707161,
12.1944378029605));
#115293=CARTESIAN_POINT('Ctrl Pts',(-9.11772514137229,11.8666287442568,
12.1684833157643));
#115294=CARTESIAN_POINT('Ctrl Pts',(-9.00118954138337,11.8740177459268,
12.0748721009633));
#115295=CARTESIAN_POINT('Ctrl Pts',(-8.92630165542791,11.8790098265681,
12.000070782526));
#115296=CARTESIAN_POINT('Ctrl Pts',(-8.83784661744725,11.8861259268869,
11.8902203176989));
#115297=CARTESIAN_POINT('Ctrl Pts',(-8.81659530711786,11.8879548142065,
11.8617689111651));
#115298=CARTESIAN_POINT('Ctrl Pts',(-8.79260815497748,11.8902031535213,
11.8270922756725));
#115299=CARTESIAN_POINT('Ctrl Pts',(-8.78885288290314,11.8905608928085,
11.821583445141));
#115300=CARTESIAN_POINT('Ctrl Pts',(-8.78277387753446,11.8911498321082,
11.8125335402636));
#115301=CARTESIAN_POINT('Ctrl Pts',(-8.78042760477626,11.891379592623,11.8090076385069));
#115302=CARTESIAN_POINT('Ctrl Pts',(-8.77623701002282,11.8917944891896,
11.8026504916372));
#115303=CARTESIAN_POINT('Ctrl Pts',(-8.77438715379534,11.891979256549,11.7998229917981));
#115304=CARTESIAN_POINT('Ctrl Pts',(-8.77034207789726,11.8923868807085,
11.7935931193736));
#115305=CARTESIAN_POINT('Ctrl Pts',(-8.76815120649359,11.8926100066002,
11.7901880748501));
#115306=CARTESIAN_POINT('Ctrl Pts',(-8.76188057642953,11.8932553422944,
11.7803528273381));
#115307=CARTESIAN_POINT('Ctrl Pts',(-8.75783690187051,11.8936797898567,
11.7738999126079));
#115308=CARTESIAN_POINT('Ctrl Pts',(-8.72821205601396,11.8968499672761,
11.7257940750527));
#115309=CARTESIAN_POINT('Ctrl Pts',(-8.70468385022007,11.8997076390147,
11.6829178607607));
#115310=CARTESIAN_POINT('Ctrl Pts',(-8.63690324694497,11.9089365988993,
11.5432455677334));
#115311=CARTESIAN_POINT('Ctrl Pts',(-8.60102786700979,11.9154334416971,
11.4427514169575));
#115312=CARTESIAN_POINT('Ctrl Pts',(-8.56429942952245,11.9246877905211,
11.2886261628154));
#115313=CARTESIAN_POINT('Ctrl Pts',(-8.55494276765743,11.9276595985992,
11.2373851542438));
#115314=CARTESIAN_POINT('Ctrl Pts',(-8.54679724379622,11.9312189752489,
11.1737265765467));
#115315=CARTESIAN_POINT('Ctrl Pts',(-8.54540819747792,11.9318866101137,
11.1616844904096));
#115316=CARTESIAN_POINT('Ctrl Pts',(-8.54345191824111,11.9329331744484,
11.1426503191556));
#115317=CARTESIAN_POINT('Ctrl Pts',(-8.54278508989747,11.9333151736115,
11.1356692160593));
#115318=CARTESIAN_POINT('Ctrl Pts',(-8.54163843878561,11.9340226275517,
11.1226790183282));
#115319=CARTESIAN_POINT('Ctrl Pts',(-8.54114551634454,11.9343484811728,
11.1166712551616));
#115320=CARTESIAN_POINT('Ctrl Pts',(-8.54013430989423,11.9350688685808,
11.1033362057976));
#115321=CARTESIAN_POINT('Ctrl Pts',(-8.53963404223708,11.9354628373827,
11.0960076905857));
#115322=CARTESIAN_POINT('Ctrl Pts',(-8.53833902149591,11.9366042640014,
11.0746739752814));
#115323=CARTESIAN_POINT('Ctrl Pts',(-8.5376904099062,11.9373472107645,11.0606605250857));
#115324=CARTESIAN_POINT('Ctrl Pts',(-8.53440327311705,11.9427667660186,
10.9575661032025));
#115325=CARTESIAN_POINT('Ctrl Pts',(-8.53970464130877,11.9471841584076,
10.8684161277608));
#115326=CARTESIAN_POINT('Ctrl Pts',(-8.56729326171334,11.9561533492868,
10.6867263682943));
#115327=CARTESIAN_POINT('Ctrl Pts',(-8.59054211638132,11.9606784445313,
10.5947663909453));
#115328=CARTESIAN_POINT('Ctrl Pts',(-8.63015593426963,11.966714379885,10.4843711040327));
#115329=CARTESIAN_POINT('Ctrl Pts',(-8.63830491782483,11.9679003322964,
10.4632204211187));
#115330=CARTESIAN_POINT('Ctrl Pts',(-8.64938591504725,11.9694559988522,
10.4363378724926));
#115331=CARTESIAN_POINT('Ctrl Pts',(-8.65186950456898,11.969801313743,10.4304233460472));
#115332=CARTESIAN_POINT('Ctrl Pts',(-8.65588162559528,11.9703541846037,
10.4210419707561));
#115333=CARTESIAN_POINT('Ctrl Pts',(-8.65738490388514,11.9705602635697,
10.4175643322563));
#115334=CARTESIAN_POINT('Ctrl Pts',(-8.66027140765136,11.9709540112089,
10.410957340259));
#115335=CARTESIAN_POINT('Ctrl Pts',(-8.6616521185089,11.9711415312223,10.4078269650013));
#115336=CARTESIAN_POINT('Ctrl Pts',(-8.66493276309844,11.9715851317555,
10.4004591013694));
#115337=CARTESIAN_POINT('Ctrl Pts',(-8.66684190464219,11.9718417593491,
10.396225780811));
#115338=CARTESIAN_POINT('Ctrl Pts',(-8.67321675718063,11.9726935184268,
10.38226786777));
#115339=CARTESIAN_POINT('Ctrl Pts',(-8.67776887452713,11.9732935446977,
10.3725833936841));
#115340=CARTESIAN_POINT('Ctrl Pts',(-8.703613764076,11.9766522729277,10.319129915983));
#115341=CARTESIAN_POINT('Ctrl Pts',(-8.72697208711382,11.9795122390927,
10.2763975687509));
#115342=CARTESIAN_POINT('Ctrl Pts',(-8.81414457006448,11.9894527788356,
10.134250193169));
#115343=CARTESIAN_POINT('Ctrl Pts',(-8.88784297415349,11.9966575825876,
10.0414130238849));
#115344=CARTESIAN_POINT('Ctrl Pts',(-8.99889684461246,12.005642625901,9.93179422090867));
#115345=CARTESIAN_POINT('Ctrl Pts',(-9.02692023781159,12.0077865030222,
9.90620511124144));
#115346=CARTESIAN_POINT('Ctrl Pts',(-9.06440059964213,12.0105003703335,
9.87456251383102));
#115347=CARTESIAN_POINT('Ctrl Pts',(-9.07297449345965,12.011111382399,9.8674897382469));
#115348=CARTESIAN_POINT('Ctrl Pts',(-9.086861565038,12.0120856416605,9.85629740520999));
#115349=CARTESIAN_POINT('Ctrl Pts',(-9.09212388939959,12.0124513500671,
9.85211568673977));
#115350=CARTESIAN_POINT('Ctrl Pts',(-9.10218945284373,12.0131443567595,
9.84422958122118));
#115351=CARTESIAN_POINT('Ctrl Pts',(-9.10698726549476,12.0134719131042,
9.8405185223371));
#115352=CARTESIAN_POINT('Ctrl Pts',(-9.11799197360889,12.0142170056589,
9.83211531826694));
#115353=CARTESIAN_POINT('Ctrl Pts',(-9.12421352317552,12.0146337829848,
9.82744260753788));
#115354=CARTESIAN_POINT('Ctrl Pts',(-9.14351570151897,12.0159133755062,
9.81318499402276));
#115355=CARTESIAN_POINT('Ctrl Pts',(-9.15671883024058,12.0167698050895,
9.8037675359362));
#115356=CARTESIAN_POINT('Ctrl Pts',(-9.22133618280742,12.0208753706536,
9.7592792301931));
#115357=CARTESIAN_POINT('Ctrl Pts',(-9.2747976756298,12.0240100410187,9.72729106218812));
#115358=CARTESIAN_POINT('Ctrl Pts',(-9.40549959371762,12.0312666224709,
9.66000520675954));
#115359=CARTESIAN_POINT('Ctrl Pts',(-9.48408635047773,12.0353175094535,
9.62783045858136));
#115360=CARTESIAN_POINT('Ctrl Pts',(-9.59111449114856,12.0408670959175,
9.59451355427368));
#115361=CARTESIAN_POINT('Ctrl Pts',(-9.61743670002312,12.042235405722,9.58712183294962));
#115362=CARTESIAN_POINT('Ctrl Pts',(-9.6708217851838,12.0450440104625,9.57373161329404));
#115363=CARTESIAN_POINT('Ctrl Pts',(-9.69787854910073,12.0464844624224,
9.56775621982086));
#115364=CARTESIAN_POINT('Ctrl Pts',(-9.73175046183815,12.0483266121899,
9.56127818404375));
#115365=CARTESIAN_POINT('Ctrl Pts',(-9.73842276732701,12.0486913548658,
9.56005013065172));
#115366=CARTESIAN_POINT('Ctrl Pts',(-9.74895336939738,12.0492702831473,
9.5581875550232));
#115367=CARTESIAN_POINT('Ctrl Pts',(-9.75280616579475,12.04948278216,9.55752201235764));
#115368=CARTESIAN_POINT('Ctrl Pts',(-9.75967211349373,12.0498627679538,
9.55636428478791));
#115369=CARTESIAN_POINT('Ctrl Pts',(-9.76268418901474,12.050029916045,9.55586608079199));
#115370=CARTESIAN_POINT('Ctrl Pts',(-9.7698827128681,12.0504304439857,9.55469855796119));
#115371=CARTESIAN_POINT('Ctrl Pts',(-9.77407050209983,12.0506643052666,
9.55403800698251));
#115372=CARTESIAN_POINT('Ctrl Pts',(-9.78670444021941,12.051372272506,9.55210144690249));
#115373=CARTESIAN_POINT('Ctrl Pts',(-9.7951587990506,12.0518493152875,9.55088120183108));
#115374=CARTESIAN_POINT('Ctrl Pts',(-9.87893733775948,12.0566058053555,
9.53953695334387));
#115375=CARTESIAN_POINT('Ctrl Pts',(-9.95492454414636,12.0611478408244,
9.53522204687687));
#115376=CARTESIAN_POINT('Ctrl Pts',(-10.1527822744948,12.0730483290963,
9.53939974891064));
#115377=CARTESIAN_POINT('Ctrl Pts',(-10.2738946133895,12.0803633111809,
9.55719462233386));
#115378=CARTESIAN_POINT('Ctrl Pts',(-10.4062784178916,12.0880508868389,
9.59393874717616));
#115379=CARTESIAN_POINT('Ctrl Pts',(-10.4210825261054,12.0889070065552,
9.5983010554303));
#115380=CARTESIAN_POINT('Ctrl Pts',(-10.4432153798648,12.0901819076362,
9.60520522394749));
#115381=CARTESIAN_POINT('Ctrl Pts',(-10.4505971221414,12.0906062649102,
9.60757241588731));
#115382=CARTESIAN_POINT('Ctrl Pts',(-10.4633623027606,12.0913387099574,
9.61177812237349));
#115383=CARTESIAN_POINT('Ctrl Pts',(-10.468754425429,12.0916476678799,9.61358956472201));
#115384=CARTESIAN_POINT('Ctrl Pts',(-10.4799632069949,12.0922890517359,
9.61742793695909));
#115385=CARTESIAN_POINT('Ctrl Pts',(-10.4857779141201,12.0926212947834,
9.61946024710825));
#115386=CARTESIAN_POINT('Ctrl Pts',(-10.4995008098727,12.0934043316828,
9.62435400099146));
#115387=CARTESIAN_POINT('Ctrl Pts',(-10.5073975531057,12.0938540810313,
9.62724703579641));
#115388=CARTESIAN_POINT('Ctrl Pts',(-10.5333239737599,12.0953282281213,
9.63699967116124));
#115389=CARTESIAN_POINT('Ctrl Pts',(-10.5512433803618,12.0963431317486,
9.6441478183767));
#115390=CARTESIAN_POINT('Ctrl Pts',(-10.5937894559204,12.0987468943643,
9.66210265399243));
#115391=CARTESIAN_POINT('Ctrl Pts',(-10.6182701063352,12.1001250851949,
9.67323799873459));
#115392=CARTESIAN_POINT('Ctrl Pts',(-10.7131794117581,12.1054706786855,
9.71960653548191));
#115393=CARTESIAN_POINT('Ctrl Pts',(-10.7810256427484,12.1092894833434,
9.75982579066119));
#115394=CARTESIAN_POINT('Ctrl Pts',(-10.9134749785787,12.1171872009357,
9.85354074408562));
#115395=CARTESIAN_POINT('Ctrl Pts',(-10.9773818633263,12.1212558609013,
9.90751341006546));
#115396=CARTESIAN_POINT('Ctrl Pts',(-11.0447525946586,12.1262768103044,
9.97507731370438));
#115397=CARTESIAN_POINT('Ctrl Pts',(-11.0530701673999,12.1269109773163,
9.98362521599326));
#115398=CARTESIAN_POINT('Ctrl Pts',(-11.0643802149046,12.1277948092838,
9.99553633595286));
#115399=CARTESIAN_POINT('Ctrl Pts',(-11.0674632507447,12.1280379866086,
9.99881335330881));
#115400=CARTESIAN_POINT('Ctrl Pts',(-11.0727194557177,12.1284565571468,
10.004452150928));
#115401=CARTESIAN_POINT('Ctrl Pts',(-11.0749000758861,12.1286313963913,
10.0068069790213));
#115402=CARTESIAN_POINT('Ctrl Pts',(-11.0794301196352,12.1289971432191,
10.0117313173801));
#115403=CARTESIAN_POINT('Ctrl Pts',(-11.0817781313781,12.1291881570838,
10.014302051414));
#115404=CARTESIAN_POINT('Ctrl Pts',(-11.0874713173949,12.1296547731608,
10.0205801111985));
#115405=CARTESIAN_POINT('Ctrl Pts',(-11.0908067207928,12.1299310852558,
10.0242962124069));
#115406=CARTESIAN_POINT('Ctrl Pts',(-11.1023704176418,12.130899128477,10.0373131747386));
#115407=CARTESIAN_POINT('Ctrl Pts',(-11.110499071855,12.1315975932638,10.0467013836924));
#115408=CARTESIAN_POINT('Ctrl Pts',(-11.1628290466101,12.1362067855806,
10.1087176158682));
#115409=CARTESIAN_POINT('Ctrl Pts',(-11.2033924431876,12.1403119039653,
10.1642962803177));
#115410=CARTESIAN_POINT('Ctrl Pts',(-11.2693042751074,12.1477707613005,
10.2694092109433));
#115411=CARTESIAN_POINT('Ctrl Pts',(-11.2960274746703,12.1511101693563,
10.3179374132596));
#115412=CARTESIAN_POINT('Ctrl Pts',(-11.3519386845608,12.1587972464062,
10.4346833094707));
#115413=CARTESIAN_POINT('Ctrl Pts',(-11.3788226890236,12.1630888458333,
10.5038430529542));
#115414=CARTESIAN_POINT('Ctrl Pts',(-11.4038246835025,12.1678703798191,
10.5861750699359));
#115415=CARTESIAN_POINT('Ctrl Pts',(-11.4071542316012,12.1685294214914,
10.597642205175));
#115416=CARTESIAN_POINT('Ctrl Pts',(-11.412373780027,12.169600777187,10.616476377842));
#115417=CARTESIAN_POINT('Ctrl Pts',(-11.4143473087481,12.17001574586,10.6238195160066));
#115418=CARTESIAN_POINT('Ctrl Pts',(-11.4177873350232,12.1707574183349,
10.6370290890842));
#115419=CARTESIAN_POINT('Ctrl Pts',(-11.419274862089,12.1710847864414,10.6428898252919));
#115420=CARTESIAN_POINT('Ctrl Pts',(-11.4223641899192,12.1717792495184,
10.6553857950484));
#115421=CARTESIAN_POINT('Ctrl Pts',(-11.4239559820754,12.1721460197657,
10.6620233702162));
#115422=CARTESIAN_POINT('Ctrl Pts',(-11.4271066675951,12.1728908485569,
10.6755788353909));
#115423=CARTESIAN_POINT('Ctrl Pts',(-11.4286618355269,12.1732687816688,
10.6824974097555));
#115424=CARTESIAN_POINT('Ctrl Pts',(-11.4324315420034,12.1742116504702,
10.6998566465726));
#115425=CARTESIAN_POINT('Ctrl Pts',(-11.4345822904332,12.1747745984343,
10.7103108305581));
#115426=CARTESIAN_POINT('Ctrl Pts',(-11.454580405202,12.1802701420819,10.8132062665199));
#115427=CARTESIAN_POINT('Ctrl Pts',(-11.4635827899384,12.1849093905218,
10.9071414041028));
#115428=CARTESIAN_POINT('Ctrl Pts',(-11.463499426367,12.1894964612477,11.001295771428));
#115429=CARTESIAN_POINT('Origin',(-10.,3.5,11.));
#115430=CARTESIAN_POINT('',(-11.4634998767682,12.7606556498649,10.9993994174008));
#115431=CARTESIAN_POINT('',(-11.4634998508852,12.6893449541571,10.9993393494607));
#115432=CARTESIAN_POINT('',(-11.4635,3.5,11.));
#115433=CARTESIAN_POINT('Ctrl Pts',(-11.4634998503757,12.7618466610292,
10.9993382219031));
#115434=CARTESIAN_POINT('Ctrl Pts',(-11.4634894474406,12.7606645999763,
10.9763324830867));
#115435=CARTESIAN_POINT('Ctrl Pts',(-11.4629365817839,12.7594623465774,
10.9533312021013));
#115436=CARTESIAN_POINT('Ctrl Pts',(-11.4616132755002,12.7579758532266,
10.9255556921769));
#115437=CARTESIAN_POINT('Ctrl Pts',(-11.4613610733915,12.7577178906591,
10.9207590131217));
#115438=CARTESIAN_POINT('Ctrl Pts',(-11.4608857152345,12.757271125723,10.9124942628439));
#115439=CARTESIAN_POINT('Ctrl Pts',(-11.4606738092072,12.757082922709,10.9090255552098));
#115440=CARTESIAN_POINT('Ctrl Pts',(-11.4602450317801,12.7567217780512,
10.902394971115));
#115441=CARTESIAN_POINT('Ctrl Pts',(-11.4600302388922,12.756548950413,10.8992329621475));
#115442=CARTESIAN_POINT('Ctrl Pts',(-11.4595810867635,12.7562028765707,
10.8929240507426));
#115443=CARTESIAN_POINT('Ctrl Pts',(-11.4593468195799,12.7560296424497,
10.8897771913828));
#115444=CARTESIAN_POINT('Ctrl Pts',(-11.4587699610399,12.7556195211129,
10.8823527918867));
#115445=CARTESIAN_POINT('Ctrl Pts',(-11.4584187314394,12.755382166558,10.8780759759065));
#115446=CARTESIAN_POINT('Ctrl Pts',(-11.4571332909366,12.7545542514349,
10.8632245728841));
#115447=CARTESIAN_POINT('Ctrl Pts',(-11.4561028579416,12.7539587445218,
10.8526589028469));
#115448=CARTESIAN_POINT('Ctrl Pts',(-11.4521366632352,12.7518784527108,
10.8161113837737));
#115449=CARTESIAN_POINT('Ctrl Pts',(-11.4486197544557,12.7503678034206,
10.7901987488577));
#115450=CARTESIAN_POINT('Ctrl Pts',(-11.4369981628361,12.7461397984288,
10.7189506482705));
#115451=CARTESIAN_POINT('Ctrl Pts',(-11.4274450953092,12.7433821114147,
10.6738825386551));
#115452=CARTESIAN_POINT('Ctrl Pts',(-11.3861242123945,12.7335717682075,
10.5160512474317));
#115453=CARTESIAN_POINT('Ctrl Pts',(-11.342967712621,12.726537121834,10.4067099920741));
#115454=CARTESIAN_POINT('Ctrl Pts',(-11.2773261207098,12.7187728284586,
10.285364739421));
#115455=CARTESIAN_POINT('Ctrl Pts',(-11.2670319210252,12.7176145680666,
10.2672682976527));
#115456=CARTESIAN_POINT('Ctrl Pts',(-11.2519420209439,12.7159967905618,
10.2420109155834));
#115457=CARTESIAN_POINT('Ctrl Pts',(-11.2474641589254,12.7155260452772,
10.2346638304005));
#115458=CARTESIAN_POINT('Ctrl Pts',(-11.2396457870149,12.7147198237232,
10.2220867172594));
#115459=CARTESIAN_POINT('Ctrl Pts',(-11.2363363595623,12.7143832363241,
10.2168377177181));
#115460=CARTESIAN_POINT('Ctrl Pts',(-11.2299423810909,12.7137417304175,
10.2068379291625));
#115461=CARTESIAN_POINT('Ctrl Pts',(-11.2268634435443,12.713436615467,10.2020836989107));
#115462=CARTESIAN_POINT('Ctrl Pts',(-11.21878564542,12.7126458333635,10.1897679575433));
#115463=CARTESIAN_POINT('Ctrl Pts',(-11.2137439564345,12.7121617502312,
10.1822347370623));
#115464=CARTESIAN_POINT('Ctrl Pts',(-11.1961475355776,12.7105039412831,
10.1564636691253));
#115465=CARTESIAN_POINT('Ctrl Pts',(-11.1832488168193,12.7093430103865,
10.1384637133702));
#115466=CARTESIAN_POINT('Ctrl Pts',(-11.0981661263326,12.7020059036102,
10.0252494880466));
#115467=CARTESIAN_POINT('Ctrl Pts',(-11.0149634294888,12.696293138055,9.93888835959894));
#115468=CARTESIAN_POINT('Ctrl Pts',(-10.8841763938904,12.688043338562,9.83275525115613));
#115469=CARTESIAN_POINT('Ctrl Pts',(-10.8446469023027,12.6856209014528,
9.8038398008398));
#115470=CARTESIAN_POINT('Ctrl Pts',(-10.7899819016892,12.682262862902,9.76791554141985));
#115471=CARTESIAN_POINT('Ctrl Pts',(-10.7760666022131,12.6814073190726,
9.75910350629386));
#115472=CARTESIAN_POINT('Ctrl Pts',(-10.7552474950749,12.6801217779288,
9.74640670919831));
#115473=CARTESIAN_POINT('Ctrl Pts',(-10.7484557280079,12.6797015431931,
9.74233989661829));
#115474=CARTESIAN_POINT('Ctrl Pts',(-10.736090433911,12.6789342959174,9.73507137175173));
#115475=CARTESIAN_POINT('Ctrl Pts',(-10.7305281296132,12.6785883830516,
9.73185087222255));
#115476=CARTESIAN_POINT('Ctrl Pts',(-10.7216779502969,12.6780364812003,
9.72680428474577));
#115477=CARTESIAN_POINT('Ctrl Pts',(-10.7184038749353,12.6778319810264,
9.72495401450765));
#115478=CARTESIAN_POINT('Ctrl Pts',(-10.7122749455627,12.6774484878162,
9.7215214880068));
#115479=CARTESIAN_POINT('Ctrl Pts',(-10.7094219021865,12.677269691098,9.71993614701244));
#115480=CARTESIAN_POINT('Ctrl Pts',(-10.7027261341567,12.6768494397151,
9.71624479276612));
#115481=CARTESIAN_POINT('Ctrl Pts',(-10.6988792468815,12.6766075123453,
9.71414649007319));
#115482=CARTESIAN_POINT('Ctrl Pts',(-10.6885931111383,12.6759594623919,
9.70859566313385));
#115483=CARTESIAN_POINT('Ctrl Pts',(-10.6821374144762,12.6755515287889,
9.70517407450599));
#115484=CARTESIAN_POINT('Ctrl Pts',(-10.6289116304516,12.6721799959832,
9.67747235213827));
#115485=CARTESIAN_POINT('Ctrl Pts',(-10.5808909738258,12.6690875270071,
9.65568833507584));
#115486=CARTESIAN_POINT('Ctrl Pts',(-10.4315706989491,12.6595337911352,
9.5974471540304));
#115487=CARTESIAN_POINT('Ctrl Pts',(-10.3273171616091,12.6529748856029,
9.56951921617888));
#115488=CARTESIAN_POINT('Ctrl Pts',(-10.1739743702117,12.64396001741,9.54610089912031));
#115489=CARTESIAN_POINT('Ctrl Pts',(-10.1266819238536,12.6412582005032,
9.54121897489193));
#115490=CARTESIAN_POINT('Ctrl Pts',(-10.0677655455937,12.6379911061445,
9.53802464425919));
#115491=CARTESIAN_POINT('Ctrl Pts',(-10.0562922184129,12.6373594264461,
9.53753792985515));
#115492=CARTESIAN_POINT('Ctrl Pts',(-10.0380144679226,12.636360158785,9.53697798073755));
#115493=CARTESIAN_POINT('Ctrl Pts',(-10.0312133715262,12.635989883757,9.53681708039404));
#115494=CARTESIAN_POINT('Ctrl Pts',(-10.0183612385959,12.6352930276925,
9.53660267576345));
#115495=CARTESIAN_POINT('Ctrl Pts',(-10.0123105288893,12.6349661483493,
9.5365392673338));
#115496=CARTESIAN_POINT('Ctrl Pts',(-9.99861733198425,12.6342290348967,
9.53648069961854));
#115497=CARTESIAN_POINT('Ctrl Pts',(-9.99097489329851,12.63381949751,9.53650787333637));
#115498=CARTESIAN_POINT('Ctrl Pts',(-9.97126718221537,12.632768026784,9.53673232932138));
#115499=CARTESIAN_POINT('Ctrl Pts',(-9.95920338141168,12.6321288451747,
9.53701896861355));
#115500=CARTESIAN_POINT('Ctrl Pts',(-9.8525615147297,12.6265150488621,9.54087295853045));
#115501=CARTESIAN_POINT('Ctrl Pts',(-9.75853035651112,12.6218390501067,
9.55345757397152));
#115502=CARTESIAN_POINT('Ctrl Pts',(-9.60040233431529,12.6139231810561,
9.5904811444635));
#115503=CARTESIAN_POINT('Ctrl Pts',(-9.53559549225147,12.6106565924612,
9.6104859046516));
#115504=CARTESIAN_POINT('Ctrl Pts',(-9.43183973579149,12.6050948505191,
9.65058605550645));
#115505=CARTESIAN_POINT('Ctrl Pts',(-9.39199174492293,12.6028721921051,
9.6680655461373));
#115506=CARTESIAN_POINT('Ctrl Pts',(-9.34632746337796,12.6001577132666,
9.69057281520895));
#115507=CARTESIAN_POINT('Ctrl Pts',(-9.33969530501415,12.5997592076041,
9.69390465792816));
#115508=CARTESIAN_POINT('Ctrl Pts',(-9.32952239983745,12.599140932343,9.69911257542349));
#115509=CARTESIAN_POINT('Ctrl Pts',(-9.32596343965669,12.59892329728,9.70095303461193));
#115510=CARTESIAN_POINT('Ctrl Pts',(-9.31941764462149,12.5985204696344,
9.7043722289648));
#115511=CARTESIAN_POINT('Ctrl Pts',(-9.3164286813142,12.5983355391674,9.705946710845));
#115512=CARTESIAN_POINT('Ctrl Pts',(-9.30966652207587,12.5979149149971,
9.70953874662261));
#115513=CARTESIAN_POINT('Ctrl Pts',(-9.30589672703332,12.5976788420207,
9.71156249561004));
#115514=CARTESIAN_POINT('Ctrl Pts',(-9.29614207424592,12.5970639804193,
9.71685434595702));
#115515=CARTESIAN_POINT('Ctrl Pts',(-9.29017115375962,12.5966836876554,
9.72014776065694));
#115516=CARTESIAN_POINT('Ctrl Pts',(-9.25047931193279,12.594130476364,9.74240400788577));
#115517=CARTESIAN_POINT('Ctrl Pts',(-9.21750117099134,12.5918873798663,
9.7626544379481));
#115518=CARTESIAN_POINT('Ctrl Pts',(-9.1002739033882,12.5835638481817,9.84120032584352));
#115519=CARTESIAN_POINT('Ctrl Pts',(-9.02140065611844,12.5772965219298,
9.90699098461165));
#115520=CARTESIAN_POINT('Ctrl Pts',(-8.91959327582179,12.5686689592212,
10.0118381553829));
#115521=CARTESIAN_POINT('Ctrl Pts',(-8.8905640827925,12.5661290833656,10.0445446299181));
#115522=CARTESIAN_POINT('Ctrl Pts',(-8.85131847704376,12.5625865686471,
10.0929665998304));
#115523=CARTESIAN_POINT('Ctrl Pts',(-8.83987313394618,12.5615387070698,
10.1076522377533));
#115524=CARTESIAN_POINT('Ctrl Pts',(-8.81996814810889,12.5596892169058,
10.1342230612114));
#115525=CARTESIAN_POINT('Ctrl Pts',(-8.81140026193073,12.5588835504876,
10.1460236751454));
#115526=CARTESIAN_POINT('Ctrl Pts',(-8.79872161626993,12.5576762323239,
10.1640466250147));
#115527=CARTESIAN_POINT('Ctrl Pts',(-8.79447986189196,12.5572696445021,
10.1701753198133));
#115528=CARTESIAN_POINT('Ctrl Pts',(-8.78689292171742,12.5565374457522,
10.1813182585474));
#115529=CARTESIAN_POINT('Ctrl Pts',(-8.78353156238559,12.5562112339537,
10.1863212433915));
#115530=CARTESIAN_POINT('Ctrl Pts',(-8.77638134830163,12.5555133290493,
10.1971068339415));
#115531=CARTESIAN_POINT('Ctrl Pts',(-8.7726023567602,12.5551420064076,10.202895823314));
#115532=CARTESIAN_POINT('Ctrl Pts',(-8.7625344735466,12.5541458768174,10.2185600566457));
#115533=CARTESIAN_POINT('Ctrl Pts',(-8.75632275529827,12.553523897762,10.22848445526));
#115534=CARTESIAN_POINT('Ctrl Pts',(-8.7262263060429,12.5504716945306,10.2778774371942));
#115535=CARTESIAN_POINT('Ctrl Pts',(-8.70409682043416,12.5481047547185,
10.3183872794507));
#115536=CARTESIAN_POINT('Ctrl Pts',(-8.63567188281134,12.5402414485446,
10.4590681049536));
#115537=CARTESIAN_POINT('Ctrl Pts',(-8.59879772192441,12.5350227405036,
10.563388555284));
#115538=CARTESIAN_POINT('Ctrl Pts',(-8.56238393094561,12.5269941816567,
10.7211516090788));
#115539=CARTESIAN_POINT('Ctrl Pts',(-8.55344548046709,12.5243799337738,
10.7720188881128));
#115540=CARTESIAN_POINT('Ctrl Pts',(-8.54628397301305,12.5212211485216,
10.8308813538659));
#115541=CARTESIAN_POINT('Ctrl Pts',(-8.54541529928664,12.5208084789294,
10.83852323097));
#115542=CARTESIAN_POINT('Ctrl Pts',(-8.54417998218654,12.520172931339,10.8502107348267));
#115543=CARTESIAN_POINT('Ctrl Pts',(-8.54376986916777,12.5199523834001,
10.8542517462381));
#115544=CARTESIAN_POINT('Ctrl Pts',(-8.54304971716165,12.5195468125867,
10.8616543470988));
#115545=CARTESIAN_POINT('Ctrl Pts',(-8.54273448214689,12.5193620780995,
10.8650153482225));
#115546=CARTESIAN_POINT('Ctrl Pts',(-8.54205195033577,12.5189453153129,
10.8725736055849));
#115547=CARTESIAN_POINT('Ctrl Pts',(-8.54169115060968,12.5187129382252,
10.8767713491267));
#115548=CARTESIAN_POINT('Ctrl Pts',(-8.54068571062748,12.5180283043031,
10.8890925553855));
#115549=CARTESIAN_POINT('Ctrl Pts',(-8.54009079846664,12.5175734468549,
10.8972197803135));
#115550=CARTESIAN_POINT('Ctrl Pts',(-8.53514020494721,12.5132702662394,
10.9736078385341));
#115551=CARTESIAN_POINT('Ctrl Pts',(-8.53550765054672,12.5092067474882,
11.0420840663074));
#115552=CARTESIAN_POINT('Ctrl Pts',(-8.54686534541231,12.5001591530132,
11.1923866470026));
#115553=CARTESIAN_POINT('Ctrl Pts',(-8.55998964699262,12.4951774396486,
11.2738335673536));
#115554=CARTESIAN_POINT('Ctrl Pts',(-8.59342405360091,12.4870759654508,
11.4080548044198));
#115555=CARTESIAN_POINT('Ctrl Pts',(-8.61005727511625,12.4838747839393,
11.4615462969679));
#115556=CARTESIAN_POINT('Ctrl Pts',(-8.63393632541507,12.4801055819105,
11.5252111173232));
#115557=CARTESIAN_POINT('Ctrl Pts',(-8.63829536729621,12.4794439402727,
11.5364113963155));
#115558=CARTESIAN_POINT('Ctrl Pts',(-8.6453808793314,12.4784085342946,11.553973978279));
#115559=CARTESIAN_POINT('Ctrl Pts',(-8.64801529640762,12.4780317382863,
11.5603726387224));
#115560=CARTESIAN_POINT('Ctrl Pts',(-8.65303247927755,12.4773291037495,
11.5723173771531));
#115561=CARTESIAN_POINT('Ctrl Pts',(-8.65540435905859,12.477002910593,11.5778678446976));
#115562=CARTESIAN_POINT('Ctrl Pts',(-8.66078755461343,12.476275699633,11.5902525285417));
#115563=CARTESIAN_POINT('Ctrl Pts',(-8.66381699185834,12.4758753009355,
11.5970787158168));
#115564=CARTESIAN_POINT('Ctrl Pts',(-8.67164090223024,12.4748631210593,
11.6143504254785));
#115565=CARTESIAN_POINT('Ctrl Pts',(-8.67650645863034,12.4742537497267,
11.6247633101871));
#115566=CARTESIAN_POINT('Ctrl Pts',(-8.7079573950299,12.4704364011011,11.6900554921859));
#115567=CARTESIAN_POINT('Ctrl Pts',(-8.73782954314724,12.4673438478479,
11.7432883074414));
#115568=CARTESIAN_POINT('Ctrl Pts',(-8.82443354765386,12.4594310890618,
11.8772603134091));
#115569=CARTESIAN_POINT('Ctrl Pts',(-8.88614621896858,12.4547509232849,
11.9543953930471));
#115570=CARTESIAN_POINT('Ctrl Pts',(-8.97734030901839,12.4482619717324,
12.0473799742652));
#115571=CARTESIAN_POINT('Ctrl Pts',(-9.00027101729209,12.4466585003391,
12.0692892038057));
#115572=CARTESIAN_POINT('Ctrl Pts',(-9.03769365315214,12.4440516466825,
12.1027881828501));
#115573=CARTESIAN_POINT('Ctrl Pts',(-9.05172612389743,12.443076210292,12.1148775155358));
#115574=CARTESIAN_POINT('Ctrl Pts',(-9.07040271748093,12.4417749476347,
12.130360160247));
#115575=CARTESIAN_POINT('Ctrl Pts',(-9.07484331153129,12.4414653391721,
12.1339974863874));
#115576=CARTESIAN_POINT('Ctrl Pts',(-9.08213461224409,12.4409564086106,
12.1398985174307));
#115577=CARTESIAN_POINT('Ctrl Pts',(-9.08497261234077,12.4407581788672,
12.1421779105389));
#115578=CARTESIAN_POINT('Ctrl Pts',(-9.09051694479987,12.4403705834913,
12.1465970194147));
#115579=CARTESIAN_POINT('Ctrl Pts',(-9.09322237997149,12.4401812937438,
12.1487377854108));
#115580=CARTESIAN_POINT('Ctrl Pts',(-9.09987445609668,12.439715537668,12.1539633214591));
#115581=CARTESIAN_POINT('Ctrl Pts',(-9.10382939755445,12.4394383407508,
12.1570374202562));
#115582=CARTESIAN_POINT('Ctrl Pts',(-9.11733608042784,12.43849093561,12.1674251067066));
#115583=CARTESIAN_POINT('Ctrl Pts',(-9.12696193790596,12.4378144993517,
12.1746410080914));
#115584=CARTESIAN_POINT('Ctrl Pts',(-9.19739370495686,12.4328627054967,
12.2260953269246));
#115585=CARTESIAN_POINT('Ctrl Pts',(-9.26143560336475,12.4283532231816,
12.2657042967515));
#115586=CARTESIAN_POINT('Ctrl Pts',(-9.38564438867118,12.4199416182248,
12.3298780920897));
#115587=CARTESIAN_POINT('Ctrl Pts',(-9.44496327842079,12.4160516903926,
12.3557077969249));
#115588=CARTESIAN_POINT('Ctrl Pts',(-9.54346986221302,12.4098992913092,
12.3910479297677));
#115589=CARTESIAN_POINT('Ctrl Pts',(-9.58168270016009,12.4075825624172,
12.4030128785986));
#115590=CARTESIAN_POINT('Ctrl Pts',(-9.64555658158733,12.4038320693768,
12.420170357843));
#115591=CARTESIAN_POINT('Ctrl Pts',(-9.67095048204999,12.402371887615,12.4262680390445));
#115592=CARTESIAN_POINT('Ctrl Pts',(-9.70566461537061,12.4004165812916,
12.4336271444188));
#115593=CARTESIAN_POINT('Ctrl Pts',(-9.71485269869166,12.3999028847763,
12.4354828909204));
#115594=CARTESIAN_POINT('Ctrl Pts',(-9.73028859109409,12.3990461576815,
12.438446472925));
#115595=CARTESIAN_POINT('Ctrl Pts',(-9.73652683209026,12.3987016324888,
12.4396021641803));
#115596=CARTESIAN_POINT('Ctrl Pts',(-9.74883472305933,12.3980251995637,
12.4417996310882));
#115597=CARTESIAN_POINT('Ctrl Pts',(-9.75490381939485,12.3976932252714,
12.4428437324908));
#115598=CARTESIAN_POINT('Ctrl Pts',(-9.76826556625888,12.3969657440448,
12.4450556893994));
#115599=CARTESIAN_POINT('Ctrl Pts',(-9.77556085621405,12.3965707693593,
12.4462067164402));
#115600=CARTESIAN_POINT('Ctrl Pts',(-9.80119233926919,12.3951905920487,
12.4500521470978));
#115601=CARTESIAN_POINT('Ctrl Pts',(-9.81957111800628,12.3942144881424,
12.4524535015816));
#115602=CARTESIAN_POINT('Ctrl Pts',(-9.93764592036376,12.3880214722084,
12.4656051680104));
#115603=CARTESIAN_POINT('Ctrl Pts',(-10.0381788947011,12.3831281873992,
12.4664349054896));
#115604=CARTESIAN_POINT('Ctrl Pts',(-10.2252821373829,12.3739832539474,
12.4487111778383));
#115605=CARTESIAN_POINT('Ctrl Pts',(-10.3116207670601,12.3697379345213,
12.4326218204824));
#115606=CARTESIAN_POINT('Ctrl Pts',(-10.4095526973019,12.3644087044578,
12.4050969027435));
#115607=CARTESIAN_POINT('Ctrl Pts',(-10.4230588217514,12.3636618362922,
12.4010895483128));
#115608=CARTESIAN_POINT('Ctrl Pts',(-10.4414464326001,12.3626260908841,
12.3953437227848));
#115609=CARTESIAN_POINT('Ctrl Pts',(-10.4463800691739,12.3623463074613,
12.3937732562323));
#115610=CARTESIAN_POINT('Ctrl Pts',(-10.4546509782038,12.3618739488042,
12.3910920561473));
#115611=CARTESIAN_POINT('Ctrl Pts',(-10.4579928174043,12.3616821792871,
12.3899953955018));
#115612=CARTESIAN_POINT('Ctrl Pts',(-10.464338771086,12.361316224399,12.3878875324804));
#115613=CARTESIAN_POINT('Ctrl Pts',(-10.4673436099646,12.3611421768721,
12.3868785985005));
#115614=CARTESIAN_POINT('Ctrl Pts',(-10.4744643986938,12.3607279445525,
12.3844618836772));
#115615=CARTESIAN_POINT('Ctrl Pts',(-10.4785773726445,12.3604872696361,
12.3830455055393));
#115616=CARTESIAN_POINT('Ctrl Pts',(-10.4930201096844,12.3596373119801,
12.3779997453773));
#115617=CARTESIAN_POINT('Ctrl Pts',(-10.5033151468152,12.3590227416419,
12.3742728897));
#115618=CARTESIAN_POINT('Ctrl Pts',(-10.6099780062433,12.3525716476919,
12.3343011334252));
#115619=CARTESIAN_POINT('Ctrl Pts',(-10.7023008517762,12.346294341507,12.2881008595586));
#115620=CARTESIAN_POINT('Ctrl Pts',(-10.8442670702993,12.3361822497266,
12.197226169405));
#115621=CARTESIAN_POINT('Ctrl Pts',(-10.8970913734018,12.3322934495163,
12.1581735055416));
#115622=CARTESIAN_POINT('Ctrl Pts',(-10.9749238674062,12.3264289135999,
12.0921015598315));
#115623=CARTESIAN_POINT('Ctrl Pts',(-11.0018369888671,12.3243717478676,
12.0674667866193));
#115624=CARTESIAN_POINT('Ctrl Pts',(-11.0353211642512,12.3217726116964,
12.034434076519));
#115625=CARTESIAN_POINT('Ctrl Pts',(-11.0427586341738,12.3211925811825,
12.0269363226797));
#115626=CARTESIAN_POINT('Ctrl Pts',(-11.0547102547638,12.3202558739916,
12.0146241005199));
#115627=CARTESIAN_POINT('Ctrl Pts',(-11.0592740526431,12.3198970614614,
12.0098585397155));
#115628=CARTESIAN_POINT('Ctrl Pts',(-11.0679918317583,12.3192094107241,
12.0006312288865));
#115629=CARTESIAN_POINT('Ctrl Pts',(-11.072150463228,12.3188803779409,11.9961740784972));
#115630=CARTESIAN_POINT('Ctrl Pts',(-11.0816265808518,12.3181282324177,
11.9858896585889));
#115631=CARTESIAN_POINT('Ctrl Pts',(-11.0869250681915,12.3177059202737,
11.9800450901591));
#115632=CARTESIAN_POINT('Ctrl Pts',(-11.1036633086237,12.316365904541,11.9612790291556));
#115633=CARTESIAN_POINT('Ctrl Pts',(-11.1149221035705,12.3154556296693,
11.9481976621597));
#115634=CARTESIAN_POINT('Ctrl Pts',(-11.2031459955531,12.3082413439645,
11.8419474352726));
#115635=CARTESIAN_POINT('Ctrl Pts',(-11.2685312522559,12.302436673178,11.7397745812336));
#115636=CARTESIAN_POINT('Ctrl Pts',(-11.3439797821411,12.2938926012885,
11.5817987233216));
#115637=CARTESIAN_POINT('Ctrl Pts',(-11.3646064053514,12.2912260598091,
11.5316201918534));
#115638=CARTESIAN_POINT('Ctrl Pts',(-11.3881502599117,12.2875547587559,
11.4638726897905));
#115639=CARTESIAN_POINT('Ctrl Pts',(-11.393602080732,12.286647117436,11.4472272474252));
#115640=CARTESIAN_POINT('Ctrl Pts',(-11.4022942662534,12.285091580831,11.4189843958975));
#115641=CARTESIAN_POINT('Ctrl Pts',(-11.4056927008977,12.2844512781024,
11.4074372900909));
#115642=CARTESIAN_POINT('Ctrl Pts',(-11.4102646239921,12.2835412116344,
11.3911644503277));
#115643=CARTESIAN_POINT('Ctrl Pts',(-11.4115576362297,12.2832779154584,
11.3864724765427));
#115644=CARTESIAN_POINT('Ctrl Pts',(-11.4137290623644,12.2828253138687,
11.3784367060661));
#115645=CARTESIAN_POINT('Ctrl Pts',(-11.4146190875962,12.2826366650252,
11.3750960398911));
#115646=CARTESIAN_POINT('Ctrl Pts',(-11.4163201272103,12.2822699103311,
11.3686191001326));
#115647=CARTESIAN_POINT('Ctrl Pts',(-11.4171325735832,12.2820918967471,
11.3654832584311));
#115648=CARTESIAN_POINT('Ctrl Pts',(-11.4193088770208,12.2816072816868,
11.3569669056941));
#115649=CARTESIAN_POINT('Ctrl Pts',(-11.420652531175,12.2812995633183,11.3515813473378));
#115650=CARTESIAN_POINT('Ctrl Pts',(-11.4256318040382,12.2801265452896,
11.331129030298));
#115651=CARTESIAN_POINT('Ctrl Pts',(-11.4290585075076,12.2792505144565,
11.3160130035892));
#115652=CARTESIAN_POINT('Ctrl Pts',(-11.452936642639,12.2726092505123,11.2023358419851));
#115653=CARTESIAN_POINT('Ctrl Pts',(-11.4634095186046,12.2664666592914,
11.1019588962303));
#115654=CARTESIAN_POINT('Ctrl Pts',(-11.4634998054292,12.26040996372,11.0008714174426));
#115655=CARTESIAN_POINT('Ctrl Pts',(-11.4635,12.2603838599167,11.0004357065747));
#115656=CARTESIAN_POINT('Ctrl Pts',(-11.4635,12.2603577583743,11.0000000000809));
#115657=CARTESIAN_POINT('Ctrl Pts',(-11.4634994198187,12.1893450843268,
11.0013031462968));
#115658=CARTESIAN_POINT('Ctrl Pts',(-11.4634359485494,12.1932196543108,
11.0725846026601));
#115659=CARTESIAN_POINT('Ctrl Pts',(-11.4581608845053,12.1970942242948,
11.1436375246629));
#115660=CARTESIAN_POINT('Ctrl Pts',(-11.447796367688,12.2009687942788,11.2138175102968));
#115661=CARTESIAN_POINT('Ctrl Pts',(-11.4404497091357,12.2037151975325,
11.2635630412024));
#115662=CARTESIAN_POINT('Ctrl Pts',(-11.4305469451326,12.2064616007861,
11.3128705823204));
#115663=CARTESIAN_POINT('Ctrl Pts',(-11.4181457399084,12.2092080040398,
11.3615175104743));
#115664=CARTESIAN_POINT('Ctrl Pts',(-11.4045533990745,12.2122181992923,
11.414836975481));
#115665=CARTESIAN_POINT('Ctrl Pts',(-11.3879212767731,12.2152283945447,
11.4675007691464));
#115666=CARTESIAN_POINT('Ctrl Pts',(-11.3683304217789,12.2182385897972,
11.5191378495491));
#115667=CARTESIAN_POINT('Ctrl Pts',(-11.3487743686918,12.2212434376294,
11.5706831999645));
#115668=CARTESIAN_POINT('Ctrl Pts',(-11.3262701993104,12.2242482854616,
11.6212049668901));
#115669=CARTESIAN_POINT('Ctrl Pts',(-11.3009490650713,12.2272531332938,
11.6703460151967));
#115670=CARTESIAN_POINT('Ctrl Pts',(-11.275652968618,12.2302550099029,11.7194384723529));
#115671=CARTESIAN_POINT('Ctrl Pts',(-11.2475456658493,12.2332568865121,
11.767152448301));
#115672=CARTESIAN_POINT('Ctrl Pts',(-11.2168061261672,12.2362587631213,
11.8131513397406));
#115673=CARTESIAN_POINT('Ctrl Pts',(-11.1860848423066,12.2392588569541,
11.8591229130239));
#115674=CARTESIAN_POINT('Ctrl Pts',(-11.1527347128426,12.2422589507869,
11.9033809824768));
#115675=CARTESIAN_POINT('Ctrl Pts',(-11.1169791419518,12.2452590446198,
11.9456161200215));
#115676=CARTESIAN_POINT('Ctrl Pts',(-11.0812306859958,12.2482585414695,
11.9878428532745));
#115677=CARTESIAN_POINT('Ctrl Pts',(-11.0430780802319,12.2512580383192,
12.0280470512292));
#115678=CARTESIAN_POINT('Ctrl Pts',(-11.0027848412112,12.2542575351689,
12.0659525375161));
#115679=CARTESIAN_POINT('Ctrl Pts',(-10.9624545653709,12.2572597891021,
12.1038928658433));
#115680=CARTESIAN_POINT('Ctrl Pts',(-10.9199801106826,12.2602620430353,
12.1395298985348));
#115681=CARTESIAN_POINT('Ctrl Pts',(-10.8756605986392,12.2632642969685,
12.1726255864473));
#115682=CARTESIAN_POINT('Ctrl Pts',(-10.8313209000313,12.2662679183625,
12.2057363487189));
#115683=CARTESIAN_POINT('Ctrl Pts',(-10.7851349099702,12.2692715397564,
12.2363031668105));
#115684=CARTESIAN_POINT('Ctrl Pts',(-10.737430742612,12.2722751611503,12.2641313815623));
#115685=CARTESIAN_POINT('Ctrl Pts',(-10.6896366113356,12.2752844469876,
12.2920120767446));
#115686=CARTESIAN_POINT('Ctrl Pts',(-10.6403190549909,12.2782937328248,
12.3171436110791));
#115687=CARTESIAN_POINT('Ctrl Pts',(-10.5898297368758,12.281303018662,12.3393778897298));
#115688=CARTESIAN_POINT('Ctrl Pts',(-10.551304766603,12.2835992003446,12.3563433579919));
#115689=CARTESIAN_POINT('Ctrl Pts',(-10.5120980785672,12.2858953820271,
12.3716229555613));
#115690=CARTESIAN_POINT('Ctrl Pts',(-10.4723716545434,12.2881915637097,
12.3851704840863));
#115691=CARTESIAN_POINT('Ctrl Pts',(-10.4202917244482,12.2912017762937,
12.4029308125298));
#115692=CARTESIAN_POINT('Ctrl Pts',(-10.3670994124745,12.2942119888777,
12.4177871813881));
#115693=CARTESIAN_POINT('Ctrl Pts',(-10.3131497370528,12.2972222014618,
12.4296046628994));
#115694=CARTESIAN_POINT('Ctrl Pts',(-10.2592959026268,12.3002270664367,
12.4414011507869));
#115695=CARTESIAN_POINT('Ctrl Pts',(-10.2046878864915,12.3032319314117,
12.4501693527271));
#115696=CARTESIAN_POINT('Ctrl Pts',(-10.149696445571,12.3062367963867,12.455823898754));
#115697=CARTESIAN_POINT('Ctrl Pts',(-10.0947593827573,12.3092386900108,
12.4614728533016));
#115698=CARTESIAN_POINT('Ctrl Pts',(-10.0394401689671,12.3122405836349,
12.4640141974152));
#115699=CARTESIAN_POINT('Ctrl Pts',(-9.98411850308232,12.315242477259,12.4634138266586));
#115700=CARTESIAN_POINT('Ctrl Pts',(-9.92882969472483,12.3182425879505,
12.4628138124839));
#115701=CARTESIAN_POINT('Ctrl Pts',(-9.87353896415618,12.3212426986419,
12.4590757876622));
#115702=CARTESIAN_POINT('Ctrl Pts',(-9.81862753988087,12.3242428093334,
12.4522177111957));
#115703=CARTESIAN_POINT('Ctrl Pts',(-9.7637270456489,12.327242322857,12.4453609998198));
#115704=CARTESIAN_POINT('Ctrl Pts',(-9.70920623148442,12.3302418363806,
12.4353855355812));
#115705=CARTESIAN_POINT('Ctrl Pts',(-9.65544040457701,12.3332413499042,
12.4223610424931));
#115706=CARTESIAN_POINT('Ctrl Pts',(-9.60162516479915,12.3362436200965,
12.409324579393));
#115707=CARTESIAN_POINT('Ctrl Pts',(-9.54856681285668,12.3392458902888,
12.3932336136817));
#115708=CARTESIAN_POINT('Ctrl Pts',(-9.49662818818895,12.3422481604811,
12.3742085245966));
#115709=CARTESIAN_POINT('Ctrl Pts',(-9.44466591029834,12.3452517979288,
12.3551747713493));
#115710=CARTESIAN_POINT('Ctrl Pts',(-9.39382486179272,12.3482554353765,
12.3332044409116));
#115711=CARTESIAN_POINT('Ctrl Pts',(-9.34444739335229,12.3512590728242,
12.308465907052));
#115712=CARTESIAN_POINT('Ctrl Pts',(-9.294976814621,12.3542683741823,12.2836807241406));
#115713=CARTESIAN_POINT('Ctrl Pts',(-9.24697578822731,12.3572776755404,
12.2561171737835));
#115714=CARTESIAN_POINT('Ctrl Pts',(-9.20076054257025,12.3602869768985,
12.2259888008002));
#115715=CARTESIAN_POINT('Ctrl Pts',(-9.16549904896773,12.3625830257256,
12.2030013338701));
#115716=CARTESIAN_POINT('Ctrl Pts',(-9.13127660587293,12.3648790745528,
12.1785217172341));
#115717=CARTESIAN_POINT('Ctrl Pts',(-9.09822041264864,12.3671751233799,
12.152660325437));
#115718=CARTESIAN_POINT('Ctrl Pts',(-9.05488208539472,12.3701853585509,
12.11875474371));
#115719=CARTESIAN_POINT('Ctrl Pts',(-9.01336762957972,12.3731955937218,
12.0823303949769));
#115720=CARTESIAN_POINT('Ctrl Pts',(-8.97398407865333,12.3762058288928,
12.0436108370188));
#115721=CARTESIAN_POINT('Ctrl Pts',(-8.93467048646908,12.3792107168499,
12.0049600583228));
#115722=CARTESIAN_POINT('Ctrl Pts',(-8.89748066087892,12.3822156048071,
11.9640225286445));
#115723=CARTESIAN_POINT('Ctrl Pts',(-8.86268873646129,12.3852204927643,
11.9210620716477));
#115724=CARTESIAN_POINT('Ctrl Pts',(-8.82793121307218,12.3882224095942,
11.8781440924366));
#115725=CARTESIAN_POINT('Ctrl Pts',(-8.79556722479157,12.391224326424,11.8332075565802));
#115726=CARTESIAN_POINT('Ctrl Pts',(-8.7658328626038,12.3942262432539,11.786551795479));
#115727=CARTESIAN_POINT('Ctrl Pts',(-8.73611615880286,12.3972263773313,
11.7399237418992));
#115728=CARTESIAN_POINT('Ctrl Pts',(-8.70902626901255,12.4002265114086,
11.6915789312041));
#115729=CARTESIAN_POINT('Ctrl Pts',(-8.68475652125001,12.403226645486,11.6418464314816));
#115730=CARTESIAN_POINT('Ctrl Pts',(-8.66049160320257,12.4062261825323,
11.5921238285988));
#115731=CARTESIAN_POINT('Ctrl Pts',(-8.63904594409448,12.4092257195786,
11.5410145594304));
#115732=CARTESIAN_POINT('Ctrl Pts',(-8.62056628656747,12.412225256625,11.4888710261876));
#115733=CARTESIAN_POINT('Ctrl Pts',(-8.6020696455284,12.4152275503606,11.4366795710434));
#115734=CARTESIAN_POINT('Ctrl Pts',(-8.58654462875385,12.4182298440961,
11.3834524516073));
#115735=CARTESIAN_POINT('Ctrl Pts',(-8.57408874487946,12.4212321378317,
11.3295593156331));
#115736=CARTESIAN_POINT('Ctrl Pts',(-8.56162718835348,12.4242357988702,
11.2756416356774));
#115737=CARTESIAN_POINT('Ctrl Pts',(-8.55223764071012,12.4272394599088,
11.2210578558749));
#115738=CARTESIAN_POINT('Ctrl Pts',(-8.5459662207352,12.4302431209473,11.1661866984958));
#115739=CARTESIAN_POINT('Ctrl Pts',(-8.5396829753973,12.4332524456763,11.1112120762943));
#115740=CARTESIAN_POINT('Ctrl Pts',(-8.53652963311143,12.4362617704054,
11.0559495225351));
#115741=CARTESIAN_POINT('Ctrl Pts',(-8.53650020816352,12.4392710951345,
11.0007805732336));
#115742=CARTESIAN_POINT('Ctrl Pts',(-8.53647775939356,12.4415669577729,
10.9586912871281));
#115743=CARTESIAN_POINT('Ctrl Pts',(-8.53827247435514,12.4438628204114,
10.9166565551187));
#115744=CARTESIAN_POINT('Ctrl Pts',(-8.54186145355085,12.4461586830499,
10.8748431809322));
#115745=CARTESIAN_POINT('Ctrl Pts',(-8.54656699279778,12.4491688068656,
10.8200213325592));
#115746=CARTESIAN_POINT('Ctrl Pts',(-8.55437843174097,12.4521789306813,
10.7653500779782));
#115747=CARTESIAN_POINT('Ctrl Pts',(-8.56527639107325,12.4551890544969,
10.7112086982124));
#115748=CARTESIAN_POINT('Ctrl Pts',(-8.57615499067921,12.4581938309653,
10.6571634981315));
#115749=CARTESIAN_POINT('Ctrl Pts',(-8.59010912612933,12.4611986074337,
10.603646818399));
#115750=CARTESIAN_POINT('Ctrl Pts',(-8.60706771717639,12.4642033839021,
10.5510324004254));
#115751=CARTESIAN_POINT('Ctrl Pts',(-8.62400953955768,12.4672051892456,
10.4984700076222));
#115752=CARTESIAN_POINT('Ctrl Pts',(-8.64394977128636,12.4702069945891,
10.4468086094374));
#115753=CARTESIAN_POINT('Ctrl Pts',(-8.6667668035885,12.4732087999326,10.396409498098));
#115754=CARTESIAN_POINT('Ctrl Pts',(-8.68957028651218,12.4762088227218,
10.3460403151306));
#115755=CARTESIAN_POINT('Ctrl Pts',(-8.7152469666204,12.4792088455111,10.2969324134366));
#115756=CARTESIAN_POINT('Ctrl Pts',(-8.74362695988841,12.4822088683004,
10.2494275290948));
#115757=CARTESIAN_POINT('Ctrl Pts',(-8.772001309016,12.4852082944528,10.2019320924028));
#115758=CARTESIAN_POINT('Ctrl Pts',(-8.80307763289055,12.4882077206053,
10.1560394930444));
#115759=CARTESIAN_POINT('Ctrl Pts',(-8.83664104477877,12.4912071467577,
10.112065209992));
#115760=CARTESIAN_POINT('Ctrl Pts',(-8.87023532050129,12.494209331086,10.0680504896029));
#115761=CARTESIAN_POINT('Ctrl Pts',(-8.90632093232706,12.4972115154142,
10.0259580304943));
#115762=CARTESIAN_POINT('Ctrl Pts',(-8.94464164190699,12.5002136997425,
9.986071508437));
#115763=CARTESIAN_POINT('Ctrl Pts',(-8.98297981251082,12.5032172520312,
9.9461668118855));
#115764=CARTESIAN_POINT('Ctrl Pts',(-9.02355472345282,12.5062208043198,
9.90847041614168));
#115765=CARTESIAN_POINT('Ctrl Pts',(-9.06607444964933,12.5092243566085,
9.87322792171522));
#115766=CARTESIAN_POINT('Ctrl Pts',(-9.10867438812128,12.5122335750146,
9.83791894330773));
#115767=CARTESIAN_POINT('Ctrl Pts',(-9.15322604477021,12.5152427934207,
9.80507342790123));
#115768=CARTESIAN_POINT('Ctrl Pts',(-9.19940666010578,12.5182520118268,
9.77489488038086));
#115769=CARTESIAN_POINT('Ctrl Pts',(-9.23465336534182,12.5205487554579,
9.75186152837433));
#115770=CARTESIAN_POINT('Ctrl Pts',(-9.27084833277887,12.522845499089,9.73038089439293));
#115771=CARTESIAN_POINT('Ctrl Pts',(-9.30783917747576,12.5251422427201,
9.71052505035477));
#115772=CARTESIAN_POINT('Ctrl Pts',(-9.3563219892478,12.5281525170208,9.68450057978738));
#115773=CARTESIAN_POINT('Ctrl Pts',(-9.40637636703392,12.5311627913216,
9.6611596215563));
#115774=CARTESIAN_POINT('Ctrl Pts',(-9.45767406955702,12.5341730656223,
9.64069325199602));
#115775=CARTESIAN_POINT('Ctrl Pts',(-9.50888062854282,12.537177991398,9.62026324619524));
#115776=CARTESIAN_POINT('Ctrl Pts',(-9.56132564180244,12.5401829171737,
9.60269788736832));
#115777=CARTESIAN_POINT('Ctrl Pts',(-9.61465725107809,12.5431878429494,
9.58814192786481));
#115778=CARTESIAN_POINT('Ctrl Pts',(-9.66793611391122,12.54618979677,9.57360036460944));
#115779=CARTESIAN_POINT('Ctrl Pts',(-9.7220993287952,12.5491917505907,9.56206244293968));
#115780=CARTESIAN_POINT('Ctrl Pts',(-9.77677784667349,12.5521937044113,
9.55362379711768));
#115781=CARTESIAN_POINT('Ctrl Pts',(-9.83142387686649,12.5551938745967,
9.5451901651856));
#115782=CARTESIAN_POINT('Ctrl Pts',(-9.88658408235999,12.5581940447822,
9.53985223956952));
#115783=CARTESIAN_POINT('Ctrl Pts',(-9.94187940564944,12.5611942149676,
9.53765453927181));
#115784=CARTESIAN_POINT('Ctrl Pts',(-9.99716370792009,12.5641937871832,
9.53545727700204));
#115785=CARTESIAN_POINT('Ctrl Pts',(-10.0525825471576,12.5671933593989,
9.53639901802073));
#115786=CARTESIAN_POINT('Ctrl Pts',(-10.107754256804,12.5701929316145,9.5404722441349));
#115787=CARTESIAN_POINT('Ctrl Pts',(-10.1629766392909,12.5731952588081,
9.54454921133193));
#115788=CARTESIAN_POINT('Ctrl Pts',(-10.2179509109613,12.5761975860017,
9.55176337078766));
#115789=CARTESIAN_POINT('Ctrl Pts',(-10.2722994359728,12.5791999131953,
9.56205519328144));
#115790=CARTESIAN_POINT('Ctrl Pts',(-10.3266726958133,12.5822036067931,
9.57235169973801));
#115791=CARTESIAN_POINT('Ctrl Pts',(-10.3804191279725,12.5852073003908,
9.58572853366859));
#115792=CARTESIAN_POINT('Ctrl Pts',(-10.4331734744544,12.5882109939886,
9.6020754701955));
#115793=CARTESIAN_POINT('Ctrl Pts',(-10.4860272605871,12.5912203494182,
9.61845321998747));
#115794=CARTESIAN_POINT('Ctrl Pts',(-10.5378847294422,12.5942297048479,
9.63781207111598));
#115795=CARTESIAN_POINT('Ctrl Pts',(-10.5883990198768,12.5972390602776,
9.65999296889605));
#115796=CARTESIAN_POINT('Ctrl Pts',(-10.626932065613,12.5995346409818,9.67691288485005));
#115797=CARTESIAN_POINT('Ctrl Pts',(-10.66468390458,12.601830221686,9.69547388902272));
#115798=CARTESIAN_POINT('Ctrl Pts',(-10.7015111127347,12.6041258023902,
9.71558791320317));
#115799=CARTESIAN_POINT('Ctrl Pts',(-10.7498054253778,12.6071361715651,
9.74196495944039));
#115800=CARTESIAN_POINT('Ctrl Pts',(-10.7967113092331,12.61014654074,9.77112495197029));
#115801=CARTESIAN_POINT('Ctrl Pts',(-10.8418893385065,12.6131569099149,
9.80289741805095));
#115802=CARTESIAN_POINT('Ctrl Pts',(-10.8869871444668,12.6161619335315,
9.83461346528072));
#115803=CARTESIAN_POINT('Ctrl Pts',(-10.9303627562825,12.6191669571481,
9.86893247856823));
#115804=CARTESIAN_POINT('Ctrl Pts',(-10.9717026357077,12.6221719807647,
9.90563889060391));
#115805=CARTESIAN_POINT('Ctrl Pts',(-11.0130016540376,12.6251740341608,
9.94230902134847));
#115806=CARTESIAN_POINT('Ctrl Pts',(-11.0522685330941,12.6281760875569,
9.98136152739303));
#115807=CARTESIAN_POINT('Ctrl Pts',(-11.0892214739027,12.631178140953,10.0225396014215));
#115808=CARTESIAN_POINT('Ctrl Pts',(-11.1261524784831,12.6341784122521,
10.0636932310727));
#115809=CARTESIAN_POINT('Ctrl Pts',(-11.1607719154766,12.6371786835511,
10.106969535533));
#115810=CARTESIAN_POINT('Ctrl Pts',(-11.1928353225168,12.6401789548502,
10.1520753905233));
#115811=CARTESIAN_POINT('Ctrl Pts',(-11.2248923535146,12.6431786295234,
10.1971722758853));
#115812=CARTESIAN_POINT('Ctrl Pts',(-11.254394058255,12.6461783041966,10.2440975591149));
#115813=CARTESIAN_POINT('Ctrl Pts',(-11.281138126595,12.6491779788698,10.2925274912871));
#115814=CARTESIAN_POINT('Ctrl Pts',(-11.3079067683252,12.6521804097495,
10.3410019225834));
#115815=CARTESIAN_POINT('Ctrl Pts',(-11.3319124556534,12.6551828406292,
10.3909833017));
#115816=CARTESIAN_POINT('Ctrl Pts',(-11.3529986372382,12.658185271509,10.4421228292612));
#115817=CARTESIAN_POINT('Ctrl Pts',(-11.3740944210341,12.6611890696337,
10.4932856447059));
#115818=CARTESIAN_POINT('Ctrl Pts',(-11.3922678752924,12.6641928677583,
10.5456071602774));
#115819=CARTESIAN_POINT('Ctrl Pts',(-11.4074116677767,12.667196665883,10.5987212347931));
#115820=CARTESIAN_POINT('Ctrl Pts',(-11.4225840048725,12.6702061258821,
10.6519354242983));
#115821=CARTESIAN_POINT('Ctrl Pts',(-11.4347151563662,12.6732155858811,
10.7059446405957));
#115822=CARTESIAN_POINT('Ctrl Pts',(-11.4437487361425,12.6762250458801,
10.7603714606171));
#115823=CARTESIAN_POINT('Ctrl Pts',(-11.4506370172559,12.6785198179401,
10.8018729744899));
#115824=CARTESIAN_POINT('Ctrl Pts',(-11.4557253172557,12.6808145900002,
10.8436170499894));
#115825=CARTESIAN_POINT('Ctrl Pts',(-11.4590089977681,12.6831093620602,
10.8854356319284));
#115826=CARTESIAN_POINT('Ctrl Pts',(-11.4619832499258,12.6851878927591,
10.9233135579597));
#115827=CARTESIAN_POINT('Ctrl Pts',(-11.463482683238,12.6872664234581,10.9613088817886));
#115828=CARTESIAN_POINT('Ctrl Pts',(-11.4634998508852,12.6893449541571,
10.9993393494607));
#115829=CARTESIAN_POINT('Origin',(-10.,2.67563288526385,11.));
#115830=CARTESIAN_POINT('',(-9.81114928992193,3.88681266808998,9.83748958206689));
#115831=CARTESIAN_POINT('',(-9.81122626339384,3.78734488014006,9.83776771472429));
#115832=CARTESIAN_POINT('',(-9.81114930150157,2.67563288526385,9.83748958018577));
#115833=CARTESIAN_POINT('',(-10.6734112416282,3.60000000000002,11.9662361834193));
#115834=CARTESIAN_POINT('Ctrl Pts',(-10.6734112416282,3.60000000000002,
11.9662361834193));
#115835=CARTESIAN_POINT('Ctrl Pts',(-10.6076401063727,3.60576385847941,
12.0120748951295));
#115836=CARTESIAN_POINT('Ctrl Pts',(-10.5373609849263,3.61172496704385,
12.0510783909628));
#115837=CARTESIAN_POINT('Ctrl Pts',(-10.4144644721966,3.62142732589243,
12.1037113510594));
#115838=CARTESIAN_POINT('Ctrl Pts',(-10.3638812952038,3.62524111380476,
12.1214059755054));
#115839=CARTESIAN_POINT('Ctrl Pts',(-10.2979722282098,3.62997290147053,
12.1395294144316));
#115840=CARTESIAN_POINT('Ctrl Pts',(-10.2836078761959,3.63099050025991,
12.1431891103141));
#115841=CARTESIAN_POINT('Ctrl Pts',(-10.2618160673463,3.63251449315885,
12.1483050943822));
#115842=CARTESIAN_POINT('Ctrl Pts',(-10.2544378270285,3.63302709607077,
12.1499624513958));
#115843=CARTESIAN_POINT('Ctrl Pts',(-10.2410446760205,3.63395163506925,
12.152835710273));
#115844=CARTESIAN_POINT('Ctrl Pts',(-10.2350353052688,3.63436430889171,
12.154075872025));
#115845=CARTESIAN_POINT('Ctrl Pts',(-10.2220687292935,3.63525023891689,
12.1566463198814));
#115846=CARTESIAN_POINT('Ctrl Pts',(-10.2151086336705,3.63572299786806,
12.1579609273009));
#115847=CARTESIAN_POINT('Ctrl Pts',(-10.1961522398362,3.63700333997121,
12.1613645533158));
#115848=CARTESIAN_POINT('Ctrl Pts',(-10.1841345160798,3.63780715382542,
12.1633304880455));
#115849=CARTESIAN_POINT('Ctrl Pts',(-10.1016688057958,3.64327371775184,
12.1755107717892));
#115850=CARTESIAN_POINT('Ctrl Pts',(-10.0304479196749,3.64773776334513,
12.1795070403536));
#115851=CARTESIAN_POINT('Ctrl Pts',(-9.90282463635051,3.65568177613116,
12.1750934705548));
#115852=CARTESIAN_POINT('Ctrl Pts',(-9.84657183949155,3.65916801272263,
12.1690794671231));
#115853=CARTESIAN_POINT('Ctrl Pts',(-9.77156556559751,3.66402317316801,
12.1555525135955));
#115854=CARTESIAN_POINT('Ctrl Pts',(-9.75225159375018,3.66529260520351,
12.151566126792));
#115855=CARTESIAN_POINT('Ctrl Pts',(-9.72436350978812,3.66716537113145,
12.1450760196958));
#115856=CARTESIAN_POINT('Ctrl Pts',(-9.71570263460018,3.66775261388313,
12.1429565010709));
#115857=CARTESIAN_POINT('Ctrl Pts',(-9.7020545940468,3.66868814781368,12.1394517883324));
#115858=CARTESIAN_POINT('Ctrl Pts',(-9.69705088779674,3.66903330562306,
12.1381316602287));
#115859=CARTESIAN_POINT('Ctrl Pts',(-9.68777942932785,3.66967716405612,
12.1356200994521));
#115860=CARTESIAN_POINT('Ctrl Pts',(-9.68350936349092,3.66997540477882,
12.134437468749));
#115861=CARTESIAN_POINT('Ctrl Pts',(-9.67921189070997,3.67027737596578,
12.1332210961266));
#115862=CARTESIAN_POINT('Ctrl Pts',(-9.67917762583091,3.67027978377793,
12.1332113959896));
#115863=CARTESIAN_POINT('Ctrl Pts',(-9.67910884701939,3.67028461713749,
12.1331919218409));
#115864=CARTESIAN_POINT('Ctrl Pts',(-9.67907433308936,3.67028704268642,
12.1331821478053));
#115865=CARTESIAN_POINT('Ctrl Pts',(-9.6790050452971,3.67029191228932,12.1331625227043));
#115866=CARTESIAN_POINT('Ctrl Pts',(-9.67897027143043,3.6702943563454,12.1331526716117));
#115867=CARTESIAN_POINT('Ctrl Pts',(-9.67890045257057,3.67029926375491,
12.1331328891473));
#115868=CARTESIAN_POINT('Ctrl Pts',(-9.67886540753536,3.67030172711319,
12.1331229577364));
#115869=CARTESIAN_POINT('Ctrl Pts',(-9.67879503473358,3.67030667394865,
12.1331030112644));
#115870=CARTESIAN_POINT('Ctrl Pts',(-9.67875970701393,3.67030915742452,
12.1330929961881));
#115871=CARTESIAN_POINT('Ctrl Pts',(-9.67868875696434,3.67031414533633,
12.1330728789314));
#115872=CARTESIAN_POINT('Ctrl Pts',(-9.67865313458732,3.67031664977768,
12.1330627767077));
#115873=CARTESIAN_POINT('Ctrl Pts',(-9.67533879979775,3.67054967678575,
12.1321226887629));
#115874=CARTESIAN_POINT('Ctrl Pts',(-9.67206417250361,3.67078098341316,
12.131178487239));
#115875=CARTESIAN_POINT('Ctrl Pts',(-9.66500751402686,3.67128183960506,
12.1291105628655));
#115876=CARTESIAN_POINT('Ctrl Pts',(-9.66122698629646,3.67155165318916,
12.127982035709));
#115877=CARTESIAN_POINT('Ctrl Pts',(-9.65089094831939,3.67229326949472,
12.1248399716574));
#115878=CARTESIAN_POINT('Ctrl Pts',(-9.6443473648619,3.67276712969324,12.1227881765384));
#115879=CARTESIAN_POINT('Ctrl Pts',(-9.60966774251945,3.67530036434515,
12.1115805227044));
#115880=CARTESIAN_POINT('Ctrl Pts',(-9.58186858945627,3.67740763778038,
12.101424682371));
#115881=CARTESIAN_POINT('Ctrl Pts',(-9.48585192388128,3.68489282322666,
12.0621881909969));
#115882=CARTESIAN_POINT('Ctrl Pts',(-9.42002167801562,3.69038873977898,
12.0277244434366));
#115883=CARTESIAN_POINT('Ctrl Pts',(-9.30942826949605,3.69995604767478,
11.9557952805702));
#115884=CARTESIAN_POINT('Ctrl Pts',(-9.26336755970211,3.70406427996755,
11.920765111295));
#115885=CARTESIAN_POINT('Ctrl Pts',(-9.21119894917348,3.70885796744483,
11.8746586659127));
#115886=CARTESIAN_POINT('Ctrl Pts',(-9.20245705446857,3.70966668642815,
11.8666949562687));
#115887=CARTESIAN_POINT('Ctrl Pts',(-9.18881576452309,3.7109377915769,11.8538867754581));
#115888=CARTESIAN_POINT('Ctrl Pts',(-9.18383658816349,3.71140374365305,
11.8491288346453));
#115889=CARTESIAN_POINT('Ctrl Pts',(-9.1745441962993,3.71227723601005,11.8400920687556));
#115890=CARTESIAN_POINT('Ctrl Pts',(-9.17022182017962,3.71268517283036,
11.8358230329989));
#115891=CARTESIAN_POINT('Ctrl Pts',(-9.16054712051434,3.71360208702088,
11.8261187023165));
#115892=CARTESIAN_POINT('Ctrl Pts',(-9.15521414646362,3.71411021796876,
11.8206644341121));
#115893=CARTESIAN_POINT('Ctrl Pts',(-9.13925602307237,3.71563937748437,
11.8040229477714));
#115894=CARTESIAN_POINT('Ctrl Pts',(-9.12879707964987,3.71665339554492,
11.7926781198217));
#115895=CARTESIAN_POINT('Ctrl Pts',(-9.0578900204787,3.72362113782536,11.7126658185357));
#115896=CARTESIAN_POINT('Ctrl Pts',(-9.0053987836687,3.72923080061634,11.6373651020107));
#115897=CARTESIAN_POINT('Ctrl Pts',(-8.93275267329638,3.73875081443016,
11.5019415588118));
#115898=CARTESIAN_POINT('Ctrl Pts',(-8.90774650272783,3.74262477020322,
11.4449071565028));
#115899=CARTESIAN_POINT('Ctrl Pts',(-8.88439159573,3.74732510517342,11.3776175326174));
#115900=CARTESIAN_POINT('Ctrl Pts',(-8.88152043194352,3.74792760526034,
11.3690264979567));
#115901=CARTESIAN_POINT('Ctrl Pts',(-8.8774224206772,3.74882644413533,11.3562771769473));
#115902=CARTESIAN_POINT('Ctrl Pts',(-8.87611890386585,3.74911859101242,
11.3521436193897));
#115903=CARTESIAN_POINT('Ctrl Pts',(-8.8738385102668,3.74964113752494,11.3447706619282));
#115904=CARTESIAN_POINT('Ctrl Pts',(-8.87285273439543,3.74987102315994,
11.3415341147376));
#115905=CARTESIAN_POINT('Ctrl Pts',(-8.87072507411335,3.75037612411805,
11.3344389276494));
#115906=CARTESIAN_POINT('Ctrl Pts',(-8.86958903364209,3.75065165084314,
11.3305787356789));
#115907=CARTESIAN_POINT('Ctrl Pts',(-8.86642545266812,3.75143559383312,
11.3196220878707));
#115908=CARTESIAN_POINT('Ctrl Pts',(-8.86444484894353,3.75194653329984,
11.3125124403464));
#115909=CARTESIAN_POINT('Ctrl Pts',(-8.85114196219382,3.75552080516272,
11.2629631047359));
#115910=CARTESIAN_POINT('Ctrl Pts',(-8.84213599307941,3.7586909773219,11.219941944433));
#115911=CARTESIAN_POINT('Ctrl Pts',(-8.83269062674888,3.76329180259075,
11.157635236095));
#115912=CARTESIAN_POINT('Ctrl Pts',(-8.83028727043316,3.76469292037048,
11.138680028719));
#115913=CARTESIAN_POINT('Ctrl Pts',(-8.82326021856566,3.76976943944122,
11.069883123102));
#115914=CARTESIAN_POINT('Ctrl Pts',(-8.82135327896773,3.77344464776853,
11.0198147518067));
#115915=CARTESIAN_POINT('Ctrl Pts',(-8.82389602710666,3.78059003794093,
10.9207673506824));
#115916=CARTESIAN_POINT('Ctrl Pts',(-8.8282128638355,3.78405605637047,10.8718811716616));
#115917=CARTESIAN_POINT('Ctrl Pts',(-8.83726035092925,3.78820585674591,
10.8122253443826));
#115918=CARTESIAN_POINT('Ctrl Pts',(-8.8391159757393,3.78897817884333,10.8010751132491));
#115919=CARTESIAN_POINT('Ctrl Pts',(-8.84233083340901,3.79020181309389,
10.7833381515133));
#115920=CARTESIAN_POINT('Ctrl Pts',(-8.84358641775555,3.79065635510335,
10.7767335987616));
#115921=CARTESIAN_POINT('Ctrl Pts',(-8.84607237866616,3.7915141810694,10.7642410483639));
#115922=CARTESIAN_POINT('Ctrl Pts',(-8.84729144022765,3.7919178078913,10.7583510457577));
#115923=CARTESIAN_POINT('Ctrl Pts',(-8.85016665662888,3.79283260600555,
10.7449762663465));
#115924=CARTESIAN_POINT('Ctrl Pts',(-8.85185088265918,3.79334286975461,
10.7374977499553));
#115925=CARTESIAN_POINT('Ctrl Pts',(-8.85725501843316,3.7949052449084,10.7145492858512));
#115926=CARTESIAN_POINT('Ctrl Pts',(-8.86121557739403,3.79594969632241,
10.6991374377218));
#115927=CARTESIAN_POINT('Ctrl Pts',(-8.88754244673397,3.80233108621313,
10.6046747375139));
#115928=CARTESIAN_POINT('Ctrl Pts',(-8.91781685175525,3.80739776949927,
10.5280619652498));
#115929=CARTESIAN_POINT('Ctrl Pts',(-8.98741992908515,3.81669623702062,
10.3946547690604));
#115930=CARTESIAN_POINT('Ctrl Pts',(-9.02422218429668,3.82091459929457,
10.3369642818983));
#115931=CARTESIAN_POINT('Ctrl Pts',(-9.07217578343922,3.82608973118099,
10.2745025110137));
#115932=CARTESIAN_POINT('Ctrl Pts',(-9.07865276245423,3.82678305175988,
10.2662945873173));
#115933=CARTESIAN_POINT('Ctrl Pts',(-9.08782917457149,3.82775929311212,
10.2549789445394));
#115934=CARTESIAN_POINT('Ctrl Pts',(-9.09043714978407,3.82803608529447,
10.2517972146001));
#115935=CARTESIAN_POINT('Ctrl Pts',(-9.09523664994044,3.82854441061294,
10.2460040017464));
#115936=CARTESIAN_POINT('Ctrl Pts',(-9.09742291734095,3.82877557089012,
10.2433882801904));
#115937=CARTESIAN_POINT('Ctrl Pts',(-9.10201802268148,3.82926067464093,
10.2379388065023));
#115938=CARTESIAN_POINT('Ctrl Pts',(-9.10442889576257,3.82951475253467,
10.2351070071509));
#115939=CARTESIAN_POINT('Ctrl Pts',(-9.11084169307029,3.83018932816418,
10.2276464483381));
#115940=CARTESIAN_POINT('Ctrl Pts',(-9.11486628289574,3.83061140235356,
10.2230374511281));
#115941=CARTESIAN_POINT('Ctrl Pts',(-9.13404041202692,3.8326154227512,10.2014213848871));
#115942=CARTESIAN_POINT('Ctrl Pts',(-9.14964425372815,3.83422631343528,
10.1848259370066));
#115943=CARTESIAN_POINT('Ctrl Pts',(-9.19827334595643,3.83916155418949,
10.1360227224417));
#115944=CARTESIAN_POINT('Ctrl Pts',(-9.23271799356437,3.84254378481007,
10.1052932245412));
#115945=CARTESIAN_POINT('Ctrl Pts',(-9.33839851980891,3.85243650913369,
10.0216120200536));
#115946=CARTESIAN_POINT('Ctrl Pts',(-9.41393231624312,3.85889814558944,
9.97457820044386));
#115947=CARTESIAN_POINT('Ctrl Pts',(-9.50810387707239,3.86612829135702,
9.92977771915933));
#115948=CARTESIAN_POINT('Ctrl Pts',(-9.52229686477993,3.86719855499594,
9.92336762037548));
#115949=CARTESIAN_POINT('Ctrl Pts',(-9.54364122342731,3.86878015125677,
9.91423291359118));
#115950=CARTESIAN_POINT('Ctrl Pts',(-9.55069829669737,3.86929860288262,
9.91129366537752));
#115951=CARTESIAN_POINT('Ctrl Pts',(-9.56340361954665,3.87022419007852,
9.90614652218766));
#115952=CARTESIAN_POINT('Ctrl Pts',(-9.56904119254915,3.87063215832115,
9.90391316996486));
#115953=CARTESIAN_POINT('Ctrl Pts',(-9.58108157594356,3.87149779551212,
9.89925056941802));
#115954=CARTESIAN_POINT('Ctrl Pts',(-9.58748885398772,3.87195505375524,
9.8968334157158));
#115955=CARTESIAN_POINT('Ctrl Pts',(-9.60489169103266,3.87318812541816,
9.8904409965152));
#115956=CARTESIAN_POINT('Ctrl Pts',(-9.61592614221113,3.87396042085412,
9.88657328678001));
#115957=CARTESIAN_POINT('Ctrl Pts',(-9.6793667675919,3.87834952424524,9.86539195299809));
#115958=CARTESIAN_POINT('Ctrl Pts',(-9.73288428558844,3.88184977177665,
9.85161355363714));
#115959=CARTESIAN_POINT('Ctrl Pts',(-9.79515509970242,3.88580319363651,
9.84017267140372));
#115960=CARTESIAN_POINT('Ctrl Pts',(-9.8031463758426,3.88630842190814,9.83878966160478));
#115961=CARTESIAN_POINT('Ctrl Pts',(-9.81114928987733,3.88681266881678,
9.83748958207414));
#115962=CARTESIAN_POINT('',(-9.31533557546055,3.6,11.9582951989184));
#115963=CARTESIAN_POINT('Origin',(-10.,3.6,11.));
#115964=CARTESIAN_POINT('Ctrl Pts',(-9.31533557546055,3.59999999999999,
11.9582951989184));
#115965=CARTESIAN_POINT('Ctrl Pts',(-9.27952779879854,3.60297350162211,
11.9327119435395));
#115966=CARTESIAN_POINT('Ctrl Pts',(-9.24515221848037,3.60586801722685,
11.9050602062982));
#115967=CARTESIAN_POINT('Ctrl Pts',(-9.21243262399748,3.60872903762957,
11.8755410579236));
#115968=CARTESIAN_POINT('Ctrl Pts',(-9.20893916100851,3.60903450806848,
11.872389305772));
#115969=CARTESIAN_POINT('Ctrl Pts',(-9.20546458751275,3.60933959666946,
11.8692163130887));
#115970=CARTESIAN_POINT('Ctrl Pts',(-9.202009183194,3.60964435880173,11.8660223588113));
#115971=CARTESIAN_POINT('Ctrl Pts',(-9.16664002443302,3.61276387224969,
11.8333293754465));
#115972=CARTESIAN_POINT('Ctrl Pts',(-9.13327747291354,3.6158499463446,11.7984348992447));
#115973=CARTESIAN_POINT('Ctrl Pts',(-9.10216851218451,3.61895386478193,
11.7616324235534));
#115974=CARTESIAN_POINT('Ctrl Pts',(-9.0710664844534,3.62205709147451,11.7248381497268));
#115975=CARTESIAN_POINT('Ctrl Pts',(-9.04221668982256,3.6251786225143,11.686137155056));
#115976=CARTESIAN_POINT('Ctrl Pts',(-9.01582547133837,3.62835240830818,
11.6458410771479));
#115977=CARTESIAN_POINT('Ctrl Pts',(-8.98943097752029,3.63152658799097,
11.6055399982161));
#115978=CARTESIAN_POINT('Ctrl Pts',(-8.96549540996297,3.63475327603208,
11.5636436378072));
#115979=CARTESIAN_POINT('Ctrl Pts',(-8.94418935979433,3.63804388640053,
11.5204775031662));
#115980=CARTESIAN_POINT('Ctrl Pts',(-8.92240571076791,3.64140825946741,
11.4763437515133));
#115981=CARTESIAN_POINT('Ctrl Pts',(-8.90337077504814,3.64483962474168,
11.430882655337));
#115982=CARTESIAN_POINT('Ctrl Pts',(-8.88723137466389,3.64832333332596,
11.3844550831564));
#115983=CARTESIAN_POINT('Ctrl Pts',(-8.87141311202751,3.65173772394908,
11.3389513151826));
#115984=CARTESIAN_POINT('Ctrl Pts',(-8.85837622789009,3.65520220875543,
11.2925190888577));
#115985=CARTESIAN_POINT('Ctrl Pts',(-8.8482262988994,3.65867789490675,11.2455108681042));
#115986=CARTESIAN_POINT('Ctrl Pts',(-8.83776727856803,3.66225942460567,
11.1970711265992));
#115987=CARTESIAN_POINT('Ctrl Pts',(-8.83037424426111,3.66585260042745,
11.1480194597946));
#115988=CARTESIAN_POINT('Ctrl Pts',(-8.82612410542532,3.66939078883076,
11.0987582105073));
#115989=CARTESIAN_POINT('Ctrl Pts',(-8.82236414574358,3.67252090910609,
11.0551783844478));
#115990=CARTESIAN_POINT('Ctrl Pts',(-8.8210638569035,3.67560737985468,11.0114334068894));
#115991=CARTESIAN_POINT('Ctrl Pts',(-8.82224547606375,3.67859306807471,
10.9678187462665));
#115992=CARTESIAN_POINT('Ctrl Pts',(-8.82239952161993,3.67898230685646,
10.9621327817196));
#115993=CARTESIAN_POINT('Ctrl Pts',(-8.82259570631382,3.67936983275185,
10.9564489734659));
#115994=CARTESIAN_POINT('Ctrl Pts',(-8.82283404223744,3.67975551917013,
10.9507679222468));
#115995=CARTESIAN_POINT('Ctrl Pts',(-8.82283477330836,3.67975670222352,
10.9507504962069));
#115996=CARTESIAN_POINT('Ctrl Pts',(-8.82283550477624,3.67975788526099,
10.9507330701661));
#115997=CARTESIAN_POINT('Ctrl Pts',(-8.82283623664109,3.67975906828253,
10.9507156441244));
#115998=CARTESIAN_POINT('Ctrl Pts',(-8.82459438669725,3.68260102659963,
10.9088532754429));
#115999=CARTESIAN_POINT('Ctrl Pts',(-8.82864619469332,3.68535111233409,
10.8669822558701));
#116000=CARTESIAN_POINT('Ctrl Pts',(-8.83496693962794,3.68805751581524,
10.8253750683343));
#116001=CARTESIAN_POINT('Ctrl Pts',(-8.83593848320487,3.68847350933275,
10.8189797468615));
#116002=CARTESIAN_POINT('Ctrl Pts',(-8.83696356715889,3.68888847081849,
10.8125907347874));
#116003=CARTESIAN_POINT('Ctrl Pts',(-8.83804202823939,3.68930257527402,
10.806209101972));
#116004=CARTESIAN_POINT('Ctrl Pts',(-8.84576787862284,3.69226912559685,
10.7604925330335));
#116005=CARTESIAN_POINT('Ctrl Pts',(-8.85623641748609,3.69519241554704,
10.7151495884285));
#116006=CARTESIAN_POINT('Ctrl Pts',(-8.86936170545022,3.69812844777868,
10.6705287431991));
#116007=CARTESIAN_POINT('Ctrl Pts',(-8.88247207956862,3.70106114389061,
10.6259585992117));
#116008=CARTESIAN_POINT('Ctrl Pts',(-8.89823266840009,3.70400699377354,
10.5821089164399));
#116009=CARTESIAN_POINT('Ctrl Pts',(-8.91651908517567,3.70700480847988,
10.5393068715871));
#116010=CARTESIAN_POINT('Ctrl Pts',(-8.93479319105893,3.71000060497923,
10.4965336421863));
#116011=CARTESIAN_POINT('Ctrl Pts',(-8.95558942741747,3.71304852454467,
10.4548066158049));
#116012=CARTESIAN_POINT('Ctrl Pts',(-8.9787508638237,3.71616537582486,10.4144324703729));
#116013=CARTESIAN_POINT('Ctrl Pts',(-9.00190743045923,3.71928157177648,
10.3740668137421));
#116014=CARTESIAN_POINT('Ctrl Pts',(-9.02742805929849,3.72246674823824,
10.3350534679578));
#116015=CARTESIAN_POINT('Ctrl Pts',(-9.05512640331091,3.72571352430631,
10.2976792920264));
#116016=CARTESIAN_POINT('Ctrl Pts',(-9.08285120233328,3.72896340140791,
10.2602694195857));
#116017=CARTESIAN_POINT('Ctrl Pts',(-9.11275789086444,3.73227494106182,
10.2245018907523));
#116018=CARTESIAN_POINT('Ctrl Pts',(-9.14463101029142,3.73561632063236,
10.1906444400298));
#116019=CARTESIAN_POINT('Ctrl Pts',(-9.17652206051582,3.73895957995615,
10.1567679421887));
#116020=CARTESIAN_POINT('Ctrl Pts',(-9.2103819497421,3.74233247733741,10.1248038032949));
#116021=CARTESIAN_POINT('Ctrl Pts',(-9.24596474086576,3.74568081267078,
10.0949990455823));
#116022=CARTESIAN_POINT('Ctrl Pts',(-9.27977331508401,3.74886219445818,
10.0666804024584));
#116023=CARTESIAN_POINT('Ctrl Pts',(-9.31513781804173,3.75202094745203,
10.0403110594085));
#116024=CARTESIAN_POINT('Ctrl Pts',(-9.35181713097022,3.755096123696,10.0160830257501));
#116025=CARTESIAN_POINT('Ctrl Pts',(-9.35381316437787,3.75526347019263,
10.0147645723571));
#116026=CARTESIAN_POINT('Ctrl Pts',(-9.35581309691475,3.75543056918726,
10.0134524485644));
#116027=CARTESIAN_POINT('Ctrl Pts',(-9.35781689172642,3.75559741085792,
10.0121466813497));
#116028=CARTESIAN_POINT('Ctrl Pts',(-9.37108236899922,3.75670193232758,
10.0035022706501));
#116029=CARTESIAN_POINT('Ctrl Pts',(-9.38451652038935,3.75779506837919,
9.99513677164828));
#116030=CARTESIAN_POINT('Ctrl Pts',(-9.39810704177623,3.75887372113637,
9.9870582776767));
#116031=CARTESIAN_POINT('Ctrl Pts',(-9.39812479668914,3.75887513030863,
9.98704772378014));
#116032=CARTESIAN_POINT('Ctrl Pts',(-9.39814255190346,3.75887653945831,
9.98703717035145));
#116033=CARTESIAN_POINT('Ctrl Pts',(-9.39816030741919,3.7588779485854,9.98702661739068));
#116034=CARTESIAN_POINT('Ctrl Pts',(-9.43429528423232,3.76174572080231,
9.96554985497536));
#116035=CARTESIAN_POINT('Ctrl Pts',(-9.47168294468352,3.76451995721889,
9.94601165757724));
#116036=CARTESIAN_POINT('Ctrl Pts',(-9.51007961331314,3.76724699079868,
9.92853655434178));
#116037=CARTESIAN_POINT('Ctrl Pts',(-9.51444171242871,3.76755679868544,
9.9265512744962));
#116038=CARTESIAN_POINT('Ctrl Pts',(-9.51881677961752,3.76786599735512,
9.92459261243027));
#116039=CARTESIAN_POINT('Ctrl Pts',(-9.52320441600076,3.76817465474311,
9.92266074246035));
#116040=CARTESIAN_POINT('Ctrl Pts',(-9.56617000891803,3.77119715855265,
9.90374305388122));
#116041=CARTESIAN_POINT('Ctrl Pts',(-9.61034674190773,3.77416854800187,
9.88739513018952));
#116042=CARTESIAN_POINT('Ctrl Pts',(-9.65538534121425,3.77714573714556,
9.87373501287088));
#116043=CARTESIAN_POINT('Ctrl Pts',(-9.70037163513504,3.7801194687433,9.86009075967138));
#116044=CARTESIAN_POINT('Ctrl Pts',(-9.74621750840829,3.78309947129679,
9.8491276013752));
#116045=CARTESIAN_POINT('Ctrl Pts',(-9.79257172567752,3.78612610132558,
9.84091846578863));
#116046=CARTESIAN_POINT('Ctrl Pts',(-9.79878106658418,3.78653153105245,
9.83981881780817));
#116047=CARTESIAN_POINT('Ctrl Pts',(-9.80499952754965,3.78693776780986,
9.83876852723399));
#116048=CARTESIAN_POINT('Ctrl Pts',(-9.81122626339384,3.78734488014006,
9.83776771472429));
#116049=CARTESIAN_POINT('Origin',(-10.,2.67563288526385,11.));
#116050=CARTESIAN_POINT('',(-9.811149300339,4.38555086460676,9.83748958037463));
#116051=CARTESIAN_POINT('',(-9.8111493102158,4.28736676513878,9.83748957877014));
#116052=CARTESIAN_POINT('',(-9.81114930150157,2.67563288526385,9.83748958018577));
#116053=CARTESIAN_POINT('',(-11.1777499567556,4.02542774070688,10.9996808414991));
#116054=CARTESIAN_POINT('Ctrl Pts',(-9.81114929917643,4.38555086460676,
9.83748958056349));
#116055=CARTESIAN_POINT('Ctrl Pts',(-9.80545487101009,4.38514543956214,
9.8384146447453));
#116056=CARTESIAN_POINT('Ctrl Pts',(-9.79976679208289,4.38474175459961,
9.83938162194824));
#116057=CARTESIAN_POINT('Ctrl Pts',(-9.78692347298589,4.38383350864485,
9.84166223899126));
#116058=CARTESIAN_POINT('Ctrl Pts',(-9.77977312848684,4.38333014153298,
9.84300038606684));
#116059=CARTESIAN_POINT('Ctrl Pts',(-9.76869675801355,4.38255441403126,
9.84517967357046));
#116060=CARTESIAN_POINT('Ctrl Pts',(-9.76476200914118,4.38227963686756,
9.84597475549734));
#116061=CARTESIAN_POINT('Ctrl Pts',(-9.75750962082406,4.38177473314452,
9.84747885622845));
#116062=CARTESIAN_POINT('Ctrl Pts',(-9.75419096752231,4.38154430541003,
9.84818209299985));
#116063=CARTESIAN_POINT('Ctrl Pts',(-9.74659749587188,4.38101842603738,
9.84982549592669));
#116064=CARTESIAN_POINT('Ctrl Pts',(-9.74232483650834,4.38072350940182,
9.85077516100225));
#116065=CARTESIAN_POINT('Ctrl Pts',(-9.72899561395014,4.37980626065909,
9.85381586289115));
#116066=CARTESIAN_POINT('Ctrl Pts',(-9.71995818396933,4.37918838283575,
9.85599036371886));
#116067=CARTESIAN_POINT('Ctrl Pts',(-9.69868464022037,4.37774142853516,
9.86137621560176));
#116068=CARTESIAN_POINT('Ctrl Pts',(-9.68647245263797,4.37691668853803,
9.86467820721197));
#116069=CARTESIAN_POINT('Ctrl Pts',(-9.64185725491757,4.37391737300405,
9.87751632716325));
#116070=CARTESIAN_POINT('Ctrl Pts',(-9.60981355997273,4.37178974534407,
9.88824881754348));
#116071=CARTESIAN_POINT('Ctrl Pts',(-9.50655670984423,4.36489229626578,
9.92784863789512));
#116072=CARTESIAN_POINT('Ctrl Pts',(-9.43770457338135,4.3602144759889,9.96230129870551));
#116073=CARTESIAN_POINT('Ctrl Pts',(-9.34145779412713,4.3530147533512,10.0228717509436));
#116074=CARTESIAN_POINT('Ctrl Pts',(-9.31116277054166,4.35064182712439,
10.0439872861446));
#116075=CARTESIAN_POINT('Ctrl Pts',(-9.27332396900916,4.34750361023579,
10.0730941906534));
#116076=CARTESIAN_POINT('Ctrl Pts',(-9.26482866026045,4.34678708015665,
10.0798176692303));
#116077=CARTESIAN_POINT('Ctrl Pts',(-9.25126943767698,4.34562322085544,
10.0908565306512));
#116078=CARTESIAN_POINT('Ctrl Pts',(-9.24614709463581,4.34517876993035,
10.0950993994765));
#116079=CARTESIAN_POINT('Ctrl Pts',(-9.23640694013003,4.34432427716778,
10.1033073302091));
#116080=CARTESIAN_POINT('Ctrl Pts',(-9.2317833758583,4.34391453200491,10.1072652571192));
#116081=CARTESIAN_POINT('Ctrl Pts',(-9.22119089377006,4.34296610936018,
10.116476001195));
#116082=CARTESIAN_POINT('Ctrl Pts',(-9.2152441345657,4.34242642093464,10.1217537323093));
#116083=CARTESIAN_POINT('Ctrl Pts',(-9.19654528371765,4.34070596379446,
10.1386904612228));
#116084=CARTESIAN_POINT('Ctrl Pts',(-9.1839966013592,4.33951608066461,10.1505696018073));
#116085=CARTESIAN_POINT('Ctrl Pts',(-9.15505466941829,4.3366854442535,10.1792006289783));
#116086=CARTESIAN_POINT('Ctrl Pts',(-9.13889165452325,4.33503570117327,
10.1961738314522));
#116087=CARTESIAN_POINT('Ctrl Pts',(-9.07776075066569,4.32851922481694,
10.2643298355626));
#116088=CARTESIAN_POINT('Ctrl Pts',(-9.03676492301814,4.32352042396874,
10.3188890034304));
#116089=CARTESIAN_POINT('Ctrl Pts',(-8.99207626874832,4.31732634394048,
10.3905318506115));
#116090=CARTESIAN_POINT('Ctrl Pts',(-8.9837235148132,4.31612992847146,10.4045641994645));
#116091=CARTESIAN_POINT('Ctrl Pts',(-8.95377825338545,4.31170091294788,
10.4573380693342));
#116092=CARTESIAN_POINT('Ctrl Pts',(-8.93408497720491,4.30849945875291,
10.4971203310144));
#116093=CARTESIAN_POINT('Ctrl Pts',(-8.91402582913007,4.30493808588415,
10.5441480858898));
#116094=CARTESIAN_POINT('Ctrl Pts',(-8.91142413810173,4.30446933473366,
10.5503963238662));
#116095=CARTESIAN_POINT('Ctrl Pts',(-8.90727387630822,4.3037105996848,10.5606108732897));
#116096=CARTESIAN_POINT('Ctrl Pts',(-8.90569273757954,4.30341882011965,
10.5645636637711));
#116097=CARTESIAN_POINT('Ctrl Pts',(-8.90289280166687,4.30289728397698,
10.5716749851558));
#116098=CARTESIAN_POINT('Ctrl Pts',(-8.90166615926598,4.30266707995038,
10.5748302713845));
#116099=CARTESIAN_POINT('Ctrl Pts',(-8.898980423482,4.30215919416052,10.5818279705535));
#116100=CARTESIAN_POINT('Ctrl Pts',(-8.89752782578054,4.30188189220269,
10.5856727616492));
#116101=CARTESIAN_POINT('Ctrl Pts',(-8.89332630991856,4.30107184093554,
10.5969720480115));
#116102=CARTESIAN_POINT('Ctrl Pts',(-8.89063259554763,4.30054218547111,
10.6044470240463));
#116103=CARTESIAN_POINT('Ctrl Pts',(-8.88461317093232,4.2993329879493,10.6216960735602));
#116104=CARTESIAN_POINT('Ctrl Pts',(-8.88133987583456,4.29865608503598,
10.6314878811016));
#116105=CARTESIAN_POINT('Ctrl Pts',(-8.87066887760985,4.29637706817461,
10.6648625695285));
#116106=CARTESIAN_POINT('Ctrl Pts',(-8.86388448180307,4.29480097051105,
10.6886359566033));
#116107=CARTESIAN_POINT('Ctrl Pts',(-8.8450058056344,4.28992395321358,10.7636628412607));
#116108=CARTESIAN_POINT('Ctrl Pts',(-8.83559617110343,4.2866900431747,10.8155250020107));
#116109=CARTESIAN_POINT('Ctrl Pts',(-8.82164376118859,4.27898657352759,
10.9390815398083));
#116110=CARTESIAN_POINT('Ctrl Pts',(-8.82012126194865,4.27450245348635,
11.0108945094171));
#116111=CARTESIAN_POINT('Ctrl Pts',(-8.82599352158789,4.26900289545835,
11.094626634492));
#116112=CARTESIAN_POINT('Ctrl Pts',(-8.82704228193272,4.26819402903912,
11.106843739188));
#116113=CARTESIAN_POINT('Ctrl Pts',(-8.82899219180597,4.2669121276084,11.1260365252301));
#116114=CARTESIAN_POINT('Ctrl Pts',(-8.82976542441508,4.266443053136,11.1330245355063));
#116115=CARTESIAN_POINT('Ctrl Pts',(-8.83131765988417,4.2655682196711,11.1459896534167));
#116116=CARTESIAN_POINT('Ctrl Pts',(-8.83208007518994,4.26516298945407,
11.1519685425486));
#116117=CARTESIAN_POINT('Ctrl Pts',(-8.83387341000413,4.26426069749989,
11.1652204469248));
#116118=CARTESIAN_POINT('Ctrl Pts',(-8.83492654140633,4.26376295861869,
11.1724901499563));
#116119=CARTESIAN_POINT('Ctrl Pts',(-8.83820269195217,4.26230213088745,
11.1937045942322));
#116120=CARTESIAN_POINT('Ctrl Pts',(-8.84060851107346,4.26133339870239,
11.2076193637501));
#116121=CARTESIAN_POINT('Ctrl Pts',(-8.84665416823165,4.25911022360444,
11.2391933614422));
#116122=CARTESIAN_POINT('Ctrl Pts',(-8.85045044268305,4.2578511961013,11.2568186655625));
#116123=CARTESIAN_POINT('Ctrl Pts',(-8.8647368499826,4.25352847649837,11.3164614420512));
#116124=CARTESIAN_POINT('Ctrl Pts',(-8.87713804190924,4.25041151022462,
11.3579813186815));
#116125=CARTESIAN_POINT('Ctrl Pts',(-8.9124700471894,4.24280782000833,11.4561831086075));
#116126=CARTESIAN_POINT('Ctrl Pts',(-8.93758193569904,4.23829222730713,
11.5119493863169));
#116127=CARTESIAN_POINT('Ctrl Pts',(-8.98382977446494,4.23130202306741,
11.5964357433773));
#116128=CARTESIAN_POINT('Ctrl Pts',(-9.00213631804458,4.22877654873722,
11.6265828788589));
#116129=CARTESIAN_POINT('Ctrl Pts',(-9.02574390185242,4.22582601752877,
11.6617938132694));
#116130=CARTESIAN_POINT('Ctrl Pts',(-9.02977215507508,4.22533230680293,
11.667685503268));
#116131=CARTESIAN_POINT('Ctrl Pts',(-9.03613171866395,4.22456830015571,
11.6768078484734));
#116132=CARTESIAN_POINT('Ctrl Pts',(-9.03842620214576,4.22429569710059,
11.6800637911102));
#116133=CARTESIAN_POINT('Ctrl Pts',(-9.04270708433118,4.223792787301,11.6860735121716));
#116134=CARTESIAN_POINT('Ctrl Pts',(-9.04468887530698,4.223562198274,11.6888303463048));
#116135=CARTESIAN_POINT('Ctrl Pts',(-9.04927712089132,4.22303338986309,
11.6951550845806));
#116136=CARTESIAN_POINT('Ctrl Pts',(-9.05189175856961,4.22273572961909,
11.6987169302257));
#116137=CARTESIAN_POINT('Ctrl Pts',(-9.06020220530425,4.22180087442736,
11.7099054678455));
#116138=CARTESIAN_POINT('Ctrl Pts',(-9.06597063062168,4.22116838288076,
11.7174780968593));
#116139=CARTESIAN_POINT('Ctrl Pts',(-9.10954760207446,4.21650342491617,
11.7732683308702));
#116140=CARTESIAN_POINT('Ctrl Pts',(-9.15098082921299,4.21268562450963,
11.8185461674166));
#116141=CARTESIAN_POINT('Ctrl Pts',(-9.26208594594291,4.20326369313489,
11.922400098976));
#116142=CARTESIAN_POINT('Ctrl Pts',(-9.33535583512995,4.19769536342337,
11.9765168674888));
#116143=CARTESIAN_POINT('Ctrl Pts',(-9.42743602667551,4.19077868071714,
12.0293208992469));
#116144=CARTESIAN_POINT('Ctrl Pts',(-9.44090898253159,4.1897693726546,12.0367006395394));
#116145=CARTESIAN_POINT('Ctrl Pts',(-9.46125050617425,4.18824747642119,
12.0473307419839));
#116146=CARTESIAN_POINT('Ctrl Pts',(-9.46801279460902,4.18774186355949,
12.0507817608767));
#116147=CARTESIAN_POINT('Ctrl Pts',(-9.48021841034802,4.18682959034212,
12.0568626693673));
#116148=CARTESIAN_POINT('Ctrl Pts',(-9.48564956039587,4.18642377273221,
12.0595165056753));
#116149=CARTESIAN_POINT('Ctrl Pts',(-9.49727887281609,4.18555495197049,
12.0650884758553));
#116150=CARTESIAN_POINT('Ctrl Pts',(-9.50348252534367,4.18509155510865,
12.0679945632145));
#116151=CARTESIAN_POINT('Ctrl Pts',(-9.52039978944569,4.18382788817665,
12.0757401633843));
#116152=CARTESIAN_POINT('Ctrl Pts',(-9.53116083572198,4.18302407449006,
12.0804735451495));
#116153=CARTESIAN_POINT('Ctrl Pts',(-9.59442734495721,4.17829676033138,
12.1071790349394));
#116154=CARTESIAN_POINT('Ctrl Pts',(-9.64839152900485,4.17425298666236,
12.1254795977402));
#116155=CARTESIAN_POINT('Ctrl Pts',(-9.78379292482323,4.16410761979585,
12.1607065868919));
#116156=CARTESIAN_POINT('Ctrl Pts',(-9.86610696898521,4.15793029281035,
12.173054781595));
#116157=CARTESIAN_POINT('Ctrl Pts',(-9.97235361452773,4.15030313677893,
12.1776568101523));
#116158=CARTESIAN_POINT('Ctrl Pts',(-9.9956999893063,4.14864995150201,12.1779735010678));
#116159=CARTESIAN_POINT('Ctrl Pts',(-10.0254424184894,4.1465848903847,12.1774925564826));
#116160=CARTESIAN_POINT('Ctrl Pts',(-10.0318419636709,4.14614298796184,
12.1773368809239));
#116161=CARTESIAN_POINT('Ctrl Pts',(-10.0420187736987,4.14544444745924,
12.1770062780671));
#116162=CARTESIAN_POINT('Ctrl Pts',(-10.0457969030579,4.14518603422506,
12.1768653281657));
#116163=CARTESIAN_POINT('Ctrl Pts',(-10.0530171172669,4.14469403190513,
12.1765611422393));
#116164=CARTESIAN_POINT('Ctrl Pts',(-10.0564592244019,4.14446028826536,
12.1764009913397));
#116165=CARTESIAN_POINT('Ctrl Pts',(-10.0646877867724,4.14390336015333,
12.1759819425084));
#116166=CARTESIAN_POINT('Ctrl Pts',(-10.0694735201485,4.14358094320803,
12.17570892267));
#116167=CARTESIAN_POINT('Ctrl Pts',(-10.0858958259647,4.14247928069505,
12.1746714261922));
#116168=CARTESIAN_POINT('Ctrl Pts',(-10.0975230741869,4.14170741814325,
12.1737633183833));
#116169=CARTESIAN_POINT('Ctrl Pts',(-10.1261493788268,4.13982292967059,
12.1710992177458));
#116170=CARTESIAN_POINT('Ctrl Pts',(-10.1431277476888,4.13871903408671,
12.1691456508466));
#116171=CARTESIAN_POINT('Ctrl Pts',(-10.2159797890412,4.13401900242998,
12.1591522045225));
#116172=CARTESIAN_POINT('Ctrl Pts',(-10.2712814298878,4.13054169511843,
12.1474704403719));
#116173=CARTESIAN_POINT('Ctrl Pts',(-10.396640386337,4.12247084615861,12.1114160443687));
#116174=CARTESIAN_POINT('Ctrl Pts',(-10.4656517385879,4.11787670504938,
12.0843135719998));
#116175=CARTESIAN_POINT('Ctrl Pts',(-10.5457948020873,4.11203220953603,
12.0437691246371));
#116176=CARTESIAN_POINT('Ctrl Pts',(-10.5597822849108,4.11099267488013,
12.0363347463778));
#116177=CARTESIAN_POINT('Ctrl Pts',(-10.5804132724414,4.10942774182562,
12.0248297825597));
#116178=CARTESIAN_POINT('Ctrl Pts',(-10.5871735819314,4.10890977013106,
12.0209715127674));
#116179=CARTESIAN_POINT('Ctrl Pts',(-10.5989121811411,4.10800101296404,
12.0141168655572));
#116180=CARTESIAN_POINT('Ctrl Pts',(-10.6039075189443,4.10761129297839,
12.0111500997529));
#116181=CARTESIAN_POINT('Ctrl Pts',(-10.6143983584433,4.1067863644352,12.0048140477297));
#116182=CARTESIAN_POINT('Ctrl Pts',(-10.6198885422211,4.10635086242538,
12.0014363712938));
#116183=CARTESIAN_POINT('Ctrl Pts',(-10.6310395584621,4.10545841849413,
11.994449198718));
#116184=CARTESIAN_POINT('Ctrl Pts',(-10.6366977994507,4.10500135396665,
11.9908360319024));
#116185=CARTESIAN_POINT('Ctrl Pts',(-10.6606897373317,4.10304498470337,
11.9752252038765));
#116186=CARTESIAN_POINT('Ctrl Pts',(-10.678716563024,4.10152885166098,11.962766245634));
#116187=CARTESIAN_POINT('Ctrl Pts',(-10.7224338747785,4.09773325429489,
11.9307135440793));
#116188=CARTESIAN_POINT('Ctrl Pts',(-10.7476844619221,4.09543416873777,
11.9105526019979));
#116189=CARTESIAN_POINT('Ctrl Pts',(-10.8100300577425,4.08948330359305,
11.856430301704));
#116190=CARTESIAN_POINT('Ctrl Pts',(-10.845836857643,4.08579465355212,11.8210852615673));
#116191=CARTESIAN_POINT('Ctrl Pts',(-10.892426778849,4.0806563535634,11.7688044794737));
#116192=CARTESIAN_POINT('Ctrl Pts',(-10.9052058306496,4.07920711827698,
11.7537163328523));
#116193=CARTESIAN_POINT('Ctrl Pts',(-10.944762803722,4.07460365869485,11.7045536827577));
#116194=CARTESIAN_POINT('Ctrl Pts',(-10.9700457849697,4.07147820234942,
11.6693165612151));
#116195=CARTESIAN_POINT('Ctrl Pts',(-10.9969598285936,4.06798891737618,
11.6270660075567));
#116196=CARTESIAN_POINT('Ctrl Pts',(-11.0005394935001,4.06752115665813,
11.6213383980434));
#116197=CARTESIAN_POINT('Ctrl Pts',(-11.0062928316159,4.06676368168116,
11.6119541561829));
#116198=CARTESIAN_POINT('Ctrl Pts',(-11.008496258779,4.06647218167176,11.6083160771185));
#116199=CARTESIAN_POINT('Ctrl Pts',(-11.0124173277992,4.06595102056128,
11.6017621358257));
#116200=CARTESIAN_POINT('Ctrl Pts',(-11.0141421545963,4.06572091325328,
11.5988507367367));
#116201=CARTESIAN_POINT('Ctrl Pts',(-11.0179340359284,4.06521313529474,
11.5923869106844));
#116202=CARTESIAN_POINT('Ctrl Pts',(-11.0199950612416,4.06493584523101,
11.5888310706609));
#116203=CARTESIAN_POINT('Ctrl Pts',(-11.0259907951662,4.06412512457036,
11.5783608212627));
#116204=CARTESIAN_POINT('Ctrl Pts',(-11.0298742034711,4.06359480158102,
11.5714170848397));
#116205=CARTESIAN_POINT('Ctrl Pts',(-11.0386439438995,4.06238370640867,
11.555356460268));
#116206=CARTESIAN_POINT('Ctrl Pts',(-11.0434811955834,4.06170558964388,
11.546213374679));
#116207=CARTESIAN_POINT('Ctrl Pts',(-11.0595015775335,4.05942054711805,
11.5149428099191));
#116208=CARTESIAN_POINT('Ctrl Pts',(-11.0701068433932,4.0578398256393,11.492525321489));
#116209=CARTESIAN_POINT('Ctrl Pts',(-11.1201943011912,4.04992573185198,
11.3773791993501));
#116210=CARTESIAN_POINT('Ctrl Pts',(-11.1483650778436,4.04386800583311,
11.2801948813759));
#116211=CARTESIAN_POINT('Ctrl Pts',(-11.1681788572242,4.03561089019528,
11.1525166453065));
#116212=CARTESIAN_POINT('Ctrl Pts',(-11.171519394874,4.03376973216029,11.1242790148007));
#116213=CARTESIAN_POINT('Ctrl Pts',(-11.1746240567457,4.03125916748005,
11.0862970819995));
#116214=CARTESIAN_POINT('Ctrl Pts',(-11.1752939629511,4.030617621944,11.0766351909747));
#116215=CARTESIAN_POINT('Ctrl Pts',(-11.1762130665869,4.02954069067114,
11.0604968952244));
#116216=CARTESIAN_POINT('Ctrl Pts',(-11.1765281092073,4.02910735124556,
11.0540246031525));
#116217=CARTESIAN_POINT('Ctrl Pts',(-11.1770223572,4.02828553752146,11.0417927600797));
#116218=CARTESIAN_POINT('Ctrl Pts',(-11.1772127357043,4.02789742129255,
11.0360338314944));
#116219=CARTESIAN_POINT('Ctrl Pts',(-11.1774846441397,4.02718247833615,
11.0254592063782));
#116220=CARTESIAN_POINT('Ctrl Pts',(-11.1775789082012,4.02685605452467,
11.0206439371467));
#116221=CARTESIAN_POINT('Ctrl Pts',(-11.1777160192758,4.02616263411095,
11.0104427075363));
#116222=CARTESIAN_POINT('Ctrl Pts',(-11.1777514162835,4.02579609702368,
11.005066751442));
#116223=CARTESIAN_POINT('Ctrl Pts',(-11.1777499567556,4.02542774070688,
10.9996808414991));
#116224=CARTESIAN_POINT('Ctrl Pts',(-9.81114928987733,3.88681266881678,
9.83748958207414));
#116225=CARTESIAN_POINT('Ctrl Pts',(-9.88349677129376,3.89137113260811,
9.82573667815999));
#116226=CARTESIAN_POINT('Ctrl Pts',(-9.95679594885871,3.89583947364135,
9.82076101815262));
#116227=CARTESIAN_POINT('Ctrl Pts',(-10.0557717545651,3.90216350620044,
9.82329087899932));
#116228=CARTESIAN_POINT('Ctrl Pts',(-10.0814191107826,3.90382968482452,
9.82478701936196));
#116229=CARTESIAN_POINT('Ctrl Pts',(-10.1135968970998,3.90597745380489,
9.82772240575238));
#116230=CARTESIAN_POINT('Ctrl Pts',(-10.1201936102639,3.90642081265862,
9.82838039276763));
#116231=CARTESIAN_POINT('Ctrl Pts',(-10.1306026787047,3.90712571284111,
9.8295074736127));
#116232=CARTESIAN_POINT('Ctrl Pts',(-10.1344190160324,3.9073852855184,9.82993959938407));
#116233=CARTESIAN_POINT('Ctrl Pts',(-10.1416463850623,3.90787912410904,
9.83079378323193));
#116234=CARTESIAN_POINT('Ctrl Pts',(-10.1450577569216,3.90811318665105,
9.8312121143408));
#116235=CARTESIAN_POINT('Ctrl Pts',(-10.1531336324011,3.90866954160889,
9.83223834608793));
#116236=CARTESIAN_POINT('Ctrl Pts',(-10.1577963712204,3.90899253410569,
9.83285926596049));
#116237=CARTESIAN_POINT('Ctrl Pts',(-10.1734576679684,3.9100830910275,9.8350403857033));
#116238=CARTESIAN_POINT('Ctrl Pts',(-10.184437452998,3.91085709087615,9.83672820493649));
#116239=CARTESIAN_POINT('Ctrl Pts',(-10.2111738021389,3.91276231090104,
9.84122615332461));
#116240=CARTESIAN_POINT('Ctrl Pts',(-10.2268998435754,3.91390039852764,
9.84420260811822));
#116241=CARTESIAN_POINT('Ctrl Pts',(-10.2915134748616,3.91863642102911,
9.85780141887378));
#116242=CARTESIAN_POINT('Ctrl Pts',(-10.3397587807551,3.92231293604581,
9.87121251672868));
#116243=CARTESIAN_POINT('Ctrl Pts',(-10.4650451089811,3.93204512346644,
9.91480141214939));
#116244=CARTESIAN_POINT('Ctrl Pts',(-10.5400267401995,3.93804672012161,
9.95009587472389));
#116245=CARTESIAN_POINT('Ctrl Pts',(-10.6240429857011,3.94486345101177,
10.001046171468));
#116246=CARTESIAN_POINT('Ctrl Pts',(-10.6372197382432,3.94593633977283,
10.0093994523147));
#116247=CARTESIAN_POINT('Ctrl Pts',(-10.656745890261,3.94753269362524,10.0223287759564));
#116248=CARTESIAN_POINT('Ctrl Pts',(-10.6632215581862,3.94806321378293,
10.0267100347006));
#116249=CARTESIAN_POINT('Ctrl Pts',(-10.6745214962456,3.94899108805173,
10.0345204115596));
#116250=CARTESIAN_POINT('Ctrl Pts',(-10.6793643800589,3.94938945100427,
10.0379219751546));
#116251=CARTESIAN_POINT('Ctrl Pts',(-10.6851221326266,3.9498639694129,10.0420312837205));
#116252=CARTESIAN_POINT('Ctrl Pts',(-10.6860617836726,3.94994143856181,
10.0427040024187));
#116253=CARTESIAN_POINT('Ctrl Pts',(-10.6872928275471,3.95004296998422,
10.0435880797069));
#116254=CARTESIAN_POINT('Ctrl Pts',(-10.6875851131722,3.95006707934939,
10.0437981885497));
#116255=CARTESIAN_POINT('Ctrl Pts',(-10.6880907464622,3.95010879179155,
10.0441620135825));
#116256=CARTESIAN_POINT('Ctrl Pts',(-10.6883041389346,3.95012639722791,
10.0443156671937));
#116257=CARTESIAN_POINT('Ctrl Pts',(-10.6886801993407,3.95015742590001,
10.0445866414159));
#116258=CARTESIAN_POINT('Ctrl Pts',(-10.6888428887337,3.95017085026404,
10.0447039320891));
#116259=CARTESIAN_POINT('Ctrl Pts',(-10.6891333126216,3.95019481627762,
10.0449134255197));
#116260=CARTESIAN_POINT('Ctrl Pts',(-10.6892610585642,3.95020535852866,
10.0450056123388));
#116261=CARTESIAN_POINT('Ctrl Pts',(-10.6894912719451,3.95022435791724,
10.0451718142046));
#116262=CARTESIAN_POINT('Ctrl Pts',(-10.689593745944,3.95023281539887,10.045245820102));
#116263=CARTESIAN_POINT('Ctrl Pts',(-10.6897797545735,3.95024816788882,
10.0453801996064));
#116264=CARTESIAN_POINT('Ctrl Pts',(-10.6898632931567,3.9502550631036,10.0454405676555));
#116265=CARTESIAN_POINT('Ctrl Pts',(-10.6901667489168,3.95028011098889,
10.0456599165769));
#116266=CARTESIAN_POINT('Ctrl Pts',(-10.6903866192063,3.95029826120068,
10.0458189625864));
#116267=CARTESIAN_POINT('Ctrl Pts',(-10.6908199238057,3.95033403359993,
10.0461326272305));
#116268=CARTESIAN_POINT('Ctrl Pts',(-10.6910333612235,3.95035165595002,
10.0462872415463));
#116269=CARTESIAN_POINT('Ctrl Pts',(-10.6914553316493,3.95038649882012,
10.0465931334396));
#116270=CARTESIAN_POINT('Ctrl Pts',(-10.6916638669528,3.9504037194599,10.0467444078197));
#116271=CARTESIAN_POINT('Ctrl Pts',(-10.6920773636549,3.95043786859194,
10.0470445711401));
#116272=CARTESIAN_POINT('Ctrl Pts',(-10.6922823266804,3.95045479716884,
10.0471934578084));
#116273=CARTESIAN_POINT('Ctrl Pts',(-10.6926898585311,3.95048845947975,
10.0474896928989));
#116274=CARTESIAN_POINT('Ctrl Pts',(-10.6928924283992,3.95050519326737,
10.0476370398252));
#116275=CARTESIAN_POINT('Ctrl Pts',(-10.6932962410866,3.95053855407357,
10.0479309654342));
#116276=CARTESIAN_POINT('Ctrl Pts',(-10.6934974844736,3.95055518112166,
10.0480775433299));
#116277=CARTESIAN_POINT('Ctrl Pts',(-10.6938996286883,3.95058840975273,
10.048370644822));
#116278=CARTESIAN_POINT('Ctrl Pts',(-10.6941005296231,3.95060501134102,
10.048517168254));
#116279=CARTESIAN_POINT('Ctrl Pts',(-10.7007537293004,3.95115485020022,
10.0533727866245));
#116280=CARTESIAN_POINT('Ctrl Pts',(-10.7071581274307,3.95168559241107,
10.0581474328468));
#116281=CARTESIAN_POINT('Ctrl Pts',(-10.7209565705541,3.95283265037311,
10.0686546256902));
#116282=CARTESIAN_POINT('Ctrl Pts',(-10.7283319256506,3.95344802524244,
10.074410891923));
#116283=CARTESIAN_POINT('Ctrl Pts',(-10.7960459972145,3.9591219023593,10.1285704971005));
#116284=CARTESIAN_POINT('Ctrl Pts',(-10.8515500481824,3.96393471929509,
10.182722035206));
#116285=CARTESIAN_POINT('Ctrl Pts',(-10.9515581345386,3.97354827509237,
10.3016323791841));
#116286=CARTESIAN_POINT('Ctrl Pts',(-10.9957055578151,3.97832990072858,
10.3661647284829));
#116287=CARTESIAN_POINT('Ctrl Pts',(-11.0374477373467,3.98405328936284,
10.4424360415357));
#116288=CARTESIAN_POINT('Ctrl Pts',(-11.0416601558663,3.98464777027854,
10.4503460328993));
#116289=CARTESIAN_POINT('Ctrl Pts',(-11.0478039464498,3.98554170978516,
10.46220702612));
#116290=CARTESIAN_POINT('Ctrl Pts',(-11.0498042306579,3.98583719558249,
10.4661222342895));
#116291=CARTESIAN_POINT('Ctrl Pts',(-11.0532130063567,3.98634863627746,
10.4728875523748));
#116292=CARTESIAN_POINT('Ctrl Pts',(-11.0546319832116,3.98656395539278,
10.4757323693199));
#116293=CARTESIAN_POINT('Ctrl Pts',(-11.0576048632744,3.98702029580721,
10.4817534188943));
#116294=CARTESIAN_POINT('Ctrl Pts',(-11.0591560020607,3.98726148842192,
10.4849309484457));
#116295=CARTESIAN_POINT('Ctrl Pts',(-11.0629922828051,3.98786570642831,
10.4928802300873));
#116296=CARTESIAN_POINT('Ctrl Pts',(-11.0652596017972,3.98822978142213,
10.4976604410803));
#116297=CARTESIAN_POINT('Ctrl Pts',(-11.0738711780948,3.98963936841443,
10.5161368061777));
#116298=CARTESIAN_POINT('Ctrl Pts',(-11.0799838123693,3.99069730366133,
10.5299385045099));
#116299=CARTESIAN_POINT('Ctrl Pts',(-11.0952951204919,3.99349717016018,
10.566386109816));
#116300=CARTESIAN_POINT('Ctrl Pts',(-11.1040567912271,3.99525618840401,
10.5892070366145));
#116301=CARTESIAN_POINT('Ctrl Pts',(-11.1515590930124,4.00573336330964,
10.7254592861947));
#116302=CARTESIAN_POINT('Ctrl Pts',(-11.1735195827319,4.01465078658567,
10.8440340662471));
#116303=CARTESIAN_POINT('Ctrl Pts',(-11.1775622213838,4.02379012574538,
10.9758185091774));
#116304=CARTESIAN_POINT('Ctrl Pts',(-11.1777467220233,4.02461135750004,
10.9877441209098));
#116305=CARTESIAN_POINT('Ctrl Pts',(-11.1777499567556,4.0254277407069,10.9996808414993));
#116306=CARTESIAN_POINT('Ctrl Pts',(-9.8111909408254,3.78717977191134,9.83748281661147));
#116307=CARTESIAN_POINT('Ctrl Pts',(-9.83186521214867,3.7885115074803,9.834125025627));
#116308=CARTESIAN_POINT('Ctrl Pts',(-9.85262448211808,3.78985562457532,
9.83131948339227));
#116309=CARTESIAN_POINT('Ctrl Pts',(-9.88706949073275,3.79210489619596,
9.82759669487098));
#116310=CARTESIAN_POINT('Ctrl Pts',(-9.90071644216444,3.79300093351796,
9.82636225320016));
#116311=CARTESIAN_POINT('Ctrl Pts',(-9.92174634108278,3.79439080007871,
9.82482939198034));
#116312=CARTESIAN_POINT('Ctrl Pts',(-9.9291160318592,3.7948795703048,9.82436185323403));
#116313=CARTESIAN_POINT('Ctrl Pts',(-9.94236646803447,3.79576166591126,
9.82364627853993));
#116314=CARTESIAN_POINT('Ctrl Pts',(-9.94824564369183,3.79615421610068,
9.82337296201398));
#116315=CARTESIAN_POINT('Ctrl Pts',(-9.96023251616122,3.79695707231853,
9.82290571771047));
#116316=CARTESIAN_POINT('Ctrl Pts',(-9.96634015948064,3.79736747038934,
9.82271523625787));
#116317=CARTESIAN_POINT('Ctrl Pts',(-9.97952660612457,3.79825649510429,
9.82240668148574));
#116318=CARTESIAN_POINT('Ctrl Pts',(-9.98660551401167,3.7987356005114,9.82230489187658));
#116319=CARTESIAN_POINT('Ctrl Pts',(-10.0058511252984,3.80004337939542,
9.82220169339636));
#116320=CARTESIAN_POINT('Ctrl Pts',(-10.0180173466603,3.80087578069572,
9.82232498409029));
#116321=CARTESIAN_POINT('Ctrl Pts',(-10.0741072111654,3.80474078510826,
9.82376272344821));
#116322=CARTESIAN_POINT('Ctrl Pts',(-10.117932753502,3.80784007236256,9.82734614125115));
#116323=CARTESIAN_POINT('Ctrl Pts',(-10.2113651647645,3.81461086318063,
9.84027635675216));
#116324=CARTESIAN_POINT('Ctrl Pts',(-10.2607815333187,3.81829339099118,
9.85037980365581));
#116325=CARTESIAN_POINT('Ctrl Pts',(-10.3613839702597,3.82591219044261,
9.87777016555957));
#116326=CARTESIAN_POINT('Ctrl Pts',(-10.4123440190162,3.82983964485881,
9.89547676947773));
#116327=CARTESIAN_POINT('Ctrl Pts',(-10.4733288341233,3.83450474199927,
9.92147841532427));
#116328=CARTESIAN_POINT('Ctrl Pts',(-10.4846646379504,3.83537017676505,
9.92652470365892));
#116329=CARTESIAN_POINT('Ctrl Pts',(-10.5004474527437,3.8365706688864,9.93385163564893));
#116330=CARTESIAN_POINT('Ctrl Pts',(-10.5049624889999,3.83691357885045,
9.9359826718283));
#116331=CARTESIAN_POINT('Ctrl Pts',(-10.5126639505387,3.83749743631072,
9.93967772180947));
#116332=CARTESIAN_POINT('Ctrl Pts',(-10.5158570621624,3.83773919705357,
9.94122752583201));
#116333=CARTESIAN_POINT('Ctrl Pts',(-10.522458568816,3.8382382946786,9.94446857791479));
#116334=CARTESIAN_POINT('Ctrl Pts',(-10.5258658785043,3.83849549664795,
9.94616195839164));
#116335=CARTESIAN_POINT('Ctrl Pts',(-10.5349834121951,3.83918281232974,
9.95074846363894));
#116336=CARTESIAN_POINT('Ctrl Pts',(-10.5406784547341,3.83961114925493,
9.95367172887309));
#116337=CARTESIAN_POINT('Ctrl Pts',(-10.5665603782186,3.84155459203336,
9.96722466872166));
#116338=CARTESIAN_POINT('Ctrl Pts',(-10.5864610197276,3.84304000166565,
9.97839382371818));
#116339=CARTESIAN_POINT('Ctrl Pts',(-10.6783304987106,3.84991411205333,
10.0335252472169));
#116340=CARTESIAN_POINT('Ctrl Pts',(-10.7457712080805,3.85502528071217,
10.0845583553547));
#116341=CARTESIAN_POINT('Ctrl Pts',(-10.8340688279533,3.86259828256421,
10.1676617182122));
#116342=CARTESIAN_POINT('Ctrl Pts',(-10.8597446359299,3.8649268438506,10.1942105265188));
#116343=CARTESIAN_POINT('Ctrl Pts',(-10.8948844204761,3.86834897734536,
10.2341397514795));
#116344=CARTESIAN_POINT('Ctrl Pts',(-10.9053837716029,3.86940476758947,
10.2465809705057));
#116345=CARTESIAN_POINT('Ctrl Pts',(-10.9237564351787,3.87131702108456,
10.269290486496));
#116346=CARTESIAN_POINT('Ctrl Pts',(-10.931724872412,3.87216973914192,10.2794786016404));
#116347=CARTESIAN_POINT('Ctrl Pts',(-10.9427397837941,3.8733832540482,10.2940501381976));
#116348=CARTESIAN_POINT('Ctrl Pts',(-10.9459269194831,3.87373865916736,
10.2983264514276));
#116349=CARTESIAN_POINT('Ctrl Pts',(-10.952649409716,3.87449758863686,10.307475340365));
#116350=CARTESIAN_POINT('Ctrl Pts',(-10.9561766589285,3.87490140514236,
10.3123536543578));
#116351=CARTESIAN_POINT('Ctrl Pts',(-10.9634925728257,3.87575097777854,
10.3226369581759));
#116352=CARTESIAN_POINT('Ctrl Pts',(-10.9672734983907,3.87619700656133,
10.3280471708622));
#116353=CARTESIAN_POINT('Ctrl Pts',(-10.9769538047166,3.87735740709784,
10.3421499515712));
#116354=CARTESIAN_POINT('Ctrl Pts',(-10.9827826040734,3.87807436143261,
10.3508900219928));
#116355=CARTESIAN_POINT('Ctrl Pts',(-11.0066657026378,3.88109069429384,
10.3877610734617));
#116356=CARTESIAN_POINT('Ctrl Pts',(-11.0236336006712,3.88342865802187,
10.4165737312155));
#116357=CARTESIAN_POINT('Ctrl Pts',(-11.0771850887938,3.8915228856007,10.5170530409613));
#116358=CARTESIAN_POINT('Ctrl Pts',(-11.107642603271,3.89745749333156,10.5917225107488));
#116359=CARTESIAN_POINT('Ctrl Pts',(-11.1433600988057,3.90675989727036,
10.7136488065752));
#116360=CARTESIAN_POINT('Ctrl Pts',(-11.153801180218,3.91014559080387,10.7591410248119));
#116361=CARTESIAN_POINT('Ctrl Pts',(-11.1632088270509,3.91413436228698,
10.815216993787));
#116362=CARTESIAN_POINT('Ctrl Pts',(-11.1647687354342,3.91484568831707,
10.8253193047656));
#116363=CARTESIAN_POINT('Ctrl Pts',(-11.166832552659,3.91586385921513,10.8399451733449));
#116364=CARTESIAN_POINT('Ctrl Pts',(-11.1674420302284,3.91617607419578,
10.844453025549));
#116365=CARTESIAN_POINT('Ctrl Pts',(-11.1684620266461,3.9167194859728,10.8523411103658));
#116366=CARTESIAN_POINT('Ctrl Pts',(-11.1688840285047,3.91695130494591,
10.8557197707956));
#116367=CARTESIAN_POINT('Ctrl Pts',(-11.1697552092392,3.91744530509341,
10.8629494835501));
#116368=CARTESIAN_POINT('Ctrl Pts',(-11.1702000314669,3.91770724526915,
10.8668009720451));
#116369=CARTESIAN_POINT('Ctrl Pts',(-11.1713649764337,3.91842110390037,
10.8773441786168));
#116370=CARTESIAN_POINT('Ctrl Pts',(-11.1720467854851,3.9188709643508,10.8840401084514));
#116371=CARTESIAN_POINT('Ctrl Pts',(-11.1753451866422,3.92123264997068,
10.9194419065752));
#116372=CARTESIAN_POINT('Ctrl Pts',(-11.1769649244369,3.92309530461378,
10.9482333235354));
#116373=CARTESIAN_POINT('Ctrl Pts',(-11.1776763809832,3.92541691352806,
10.9847492214321));
#116374=CARTESIAN_POINT('Ctrl Pts',(-11.177750876702,3.92590372022819,10.992442162376));
#116375=CARTESIAN_POINT('Ctrl Pts',(-11.1777430102078,3.93021726774146,
11.0608648101056));
#116376=CARTESIAN_POINT('Ctrl Pts',(-11.1730389131068,3.93393105739488,
11.1215049712384));
#116377=CARTESIAN_POINT('Ctrl Pts',(-11.1570204480465,3.94038268400652,
11.2241987308866));
#116378=CARTESIAN_POINT('Ctrl Pts',(-11.1480193233025,3.94308672030422,
11.2664818720717));
#116379=CARTESIAN_POINT('Ctrl Pts',(-11.1320140660241,3.94700495076092,
11.3255183492424));
#116380=CARTESIAN_POINT('Ctrl Pts',(-11.1269153687118,3.94816629037035,
11.3427531794665));
#116381=CARTESIAN_POINT('Ctrl Pts',(-11.1171263907553,3.95025805637157,
11.3732580411187));
#116382=CARTESIAN_POINT('Ctrl Pts',(-11.1125887803687,3.95118365892871,
11.3865735589111));
#116383=CARTESIAN_POINT('Ctrl Pts',(-11.105334780562,3.95260161186483,11.4066736046932));
#116384=CARTESIAN_POINT('Ctrl Pts',(-11.1027918428489,3.95308826751543,
11.4135197034856));
#116385=CARTESIAN_POINT('Ctrl Pts',(-11.0980496638493,3.95397754490102,
11.4259316954146));
#116386=CARTESIAN_POINT('Ctrl Pts',(-11.0958713410895,3.95437946012569,
11.4315053591154));
#116387=CARTESIAN_POINT('Ctrl Pts',(-11.0910640770182,3.95525260093537,
11.443534468164));
#116388=CARTESIAN_POINT('Ctrl Pts',(-11.0884201273098,3.95572431708372,
11.4499836301975));
#116389=CARTESIAN_POINT('Ctrl Pts',(-11.08101985291,3.95702204152894,11.4675876270796));
#116390=CARTESIAN_POINT('Ctrl Pts',(-11.0761483594504,3.95785189837919,
11.4786928040614));
#116391=CARTESIAN_POINT('Ctrl Pts',(-11.0401596144436,3.96381649619392,
11.5574066444271));
#116392=CARTESIAN_POINT('Ctrl Pts',(-11.0028724648894,3.96916563896348,
11.6219945973047));
#116393=CARTESIAN_POINT('Ctrl Pts',(-10.9258839014303,3.97888923270412,
11.7302384326686));
#116394=CARTESIAN_POINT('Ctrl Pts',(-10.8885208976615,3.98320876028655,
11.7752677248567));
#116395=CARTESIAN_POINT('Ctrl Pts',(-10.8341149077159,3.98887156766593,
11.8317126598989));
#116396=CARTESIAN_POINT('Ctrl Pts',(-10.8198960780281,3.99030071147375,
11.8457329023861));
#116397=CARTESIAN_POINT('Ctrl Pts',(-10.7958032856493,3.99263095797866,
11.8683101630334));
#116398=CARTESIAN_POINT('Ctrl Pts',(-10.7861314861791,3.99354336405576,
11.8770762399197));
#116399=CARTESIAN_POINT('Ctrl Pts',(-10.7725682825127,3.99478913154316,
11.888964645294));
#116400=CARTESIAN_POINT('Ctrl Pts',(-10.7688002029142,3.99513171897993,
11.8922253874352));
#116401=CARTESIAN_POINT('Ctrl Pts',(-10.7623799425228,3.99570936039403,
11.8977103457199));
#116402=CARTESIAN_POINT('Ctrl Pts',(-10.7597384802511,3.99594529330754,
11.8999469342664));
#116403=CARTESIAN_POINT('Ctrl Pts',(-10.7546082460949,3.99640015180379,
11.9042521382106));
#116404=CARTESIAN_POINT('Ctrl Pts',(-10.7521207870267,3.99661918853367,
11.9063221595514));
#116405=CARTESIAN_POINT('Ctrl Pts',(-10.7453469787629,3.99721168901267,
11.9119121150621));
#116406=CARTESIAN_POINT('Ctrl Pts',(-10.7410441795162,3.99758376244596,
11.9154121210513));
#116407=CARTESIAN_POINT('Ctrl Pts',(-10.7244881757141,3.99899978997435,
11.928685956909));
#116408=CARTESIAN_POINT('Ctrl Pts',(-10.7120644240592,4.00002999623509,
11.9382457230221));
#116409=CARTESIAN_POINT('Ctrl Pts',(-10.6045503425333,4.00870883020965,
12.017608941363));
#116410=CARTESIAN_POINT('Ctrl Pts',(-10.4996539969478,4.01569141676283,
12.0730154839968));
#116411=CARTESIAN_POINT('Ctrl Pts',(-10.3665711596204,4.02464398416576,
12.1194858060677));
#116412=CARTESIAN_POINT('Ctrl Pts',(-10.3446652118292,4.02611776764204,
12.1264229571339));
#116413=CARTESIAN_POINT('Ctrl Pts',(-10.3061921711463,4.028717265921,12.1373792034351));
#116414=CARTESIAN_POINT('Ctrl Pts',(-10.2897144266052,4.02983405907228,
12.1416876111871));
#116415=CARTESIAN_POINT('Ctrl Pts',(-10.2654488487225,4.03148651947439,
12.1474731568581));
#116416=CARTESIAN_POINT('Ctrl Pts',(-10.2577298298946,4.03201331974995,
12.1492315113542));
#116417=CARTESIAN_POINT('Ctrl Pts',(-10.2440393658826,4.03294994497636,
12.1522052676661));
#116418=CARTESIAN_POINT('Ctrl Pts',(-10.2380750565669,4.03335875468874,
12.1534524073436));
#116419=CARTESIAN_POINT('Ctrl Pts',(-10.2255402103787,4.03421965523097,
12.1559720866541));
#116420=CARTESIAN_POINT('Ctrl Pts',(-10.2189679853552,4.03467203196904,
12.1572350106314));
#116421=CARTESIAN_POINT('Ctrl Pts',(-10.2015867673294,4.03587120292094,
12.1604216342817));
#116422=CARTESIAN_POINT('Ctrl Pts',(-10.1907612396291,4.03662092966357,
12.1622502869132));
#116423=CARTESIAN_POINT('Ctrl Pts',(-10.1426754265992,4.03996470536645,
12.1696830679689));
#116424=CARTESIAN_POINT('Ctrl Pts',(-10.1051879882529,4.0426084945087,12.1736480340791));
#116425=CARTESIAN_POINT('Ctrl Pts',(-9.99097281550542,4.050776290538,12.1802124228883));
#116426=CARTESIAN_POINT('Ctrl Pts',(-9.91412559701792,4.05643861130657,
12.1771177991398));
#116427=CARTESIAN_POINT('Ctrl Pts',(-9.80579576437694,4.06442957565171,
12.1620868177153));
#116428=CARTESIAN_POINT('Ctrl Pts',(-9.77365439540717,4.06679896948399,
12.1562564600043));
#116429=CARTESIAN_POINT('Ctrl Pts',(-9.7297091024715,4.07000503987318,12.1463818460743));
#116430=CARTESIAN_POINT('Ctrl Pts',(-9.71766628242738,4.07088005807052,
12.1434754936989));
#116431=CARTESIAN_POINT('Ctrl Pts',(-9.69680930490211,4.07238680119161,
12.1380923630375));
#116432=CARTESIAN_POINT('Ctrl Pts',(-9.68797417263657,4.07302232170028,
12.1357018623852));
#116433=CARTESIAN_POINT('Ctrl Pts',(-9.67497246707904,4.07395260489652,
12.1320208363953));
#116434=CARTESIAN_POINT('Ctrl Pts',(-9.67078400202692,4.07425153067137,
12.1308098422755));
#116435=CARTESIAN_POINT('Ctrl Pts',(-9.66334157587681,4.07478121149281,
12.128613187214));
#116436=CARTESIAN_POINT('Ctrl Pts',(-9.66008504401674,4.07501246863267,
12.1276366633906));
#116437=CARTESIAN_POINT('Ctrl Pts',(-9.65296184841235,4.07551717080174,
12.1254669951038));
#116438=CARTESIAN_POINT('Ctrl Pts',(-9.64909707120239,4.07579028052519,
12.1242680158706));
#116439=CARTESIAN_POINT('Ctrl Pts',(-9.63817484753469,4.0765602686588,12.1208177797033));
#116440=CARTESIAN_POINT('Ctrl Pts',(-9.63113220391451,4.07705456810155,
12.1185197772727));
#116441=CARTESIAN_POINT('Ctrl Pts',(-9.58300193994254,4.08042063832355,
12.1023109115636));
#116442=CARTESIAN_POINT('Ctrl Pts',(-9.5426835731107,4.08318052324722,12.0862040809514));
#116443=CARTESIAN_POINT('Ctrl Pts',(-9.48553598709015,4.08712810544038,
12.059626095717));
#116444=CARTESIAN_POINT('Ctrl Pts',(-9.46793974515926,4.08834867210622,
12.0509008516992));
#116445=CARTESIAN_POINT('Ctrl Pts',(-9.40619190187101,4.09267595367205,
12.0183340320949));
#116446=CARTESIAN_POINT('Ctrl Pts',(-9.36335623170701,4.09576219207596,
11.9921173430956));
#116447=CARTESIAN_POINT('Ctrl Pts',(-9.28244953479867,4.10196450703922,
11.93519691149));
#116448=CARTESIAN_POINT('Ctrl Pts',(-9.24436034925133,4.10507126687519,
11.9046987321219));
#116449=CARTESIAN_POINT('Ctrl Pts',(-9.1998798969313,4.10901668761309,11.8643097891163));
#116450=CARTESIAN_POINT('Ctrl Pts',(-9.19159740646188,4.10976590095353,
11.8565680492916));
#116451=CARTESIAN_POINT('Ctrl Pts',(-9.17855632430423,4.11096992415317,
11.8440207680903));
#116452=CARTESIAN_POINT('Ctrl Pts',(-9.17372499289209,4.11142147914149,
11.8392915933849));
#116453=CARTESIAN_POINT('Ctrl Pts',(-9.16464028349946,4.11228126111537,
11.8302445053379));
#116454=CARTESIAN_POINT('Ctrl Pts',(-9.1603789837844,4.1126891217111,11.8259348287685));
#116455=CARTESIAN_POINT('Ctrl Pts',(-9.15075050317312,4.11362130269754,
11.8160455204478));
#116456=CARTESIAN_POINT('Ctrl Pts',(-9.14540474231337,4.11414651776933,
11.8104455193861));
#116457=CARTESIAN_POINT('Ctrl Pts',(-9.12908422750585,4.11577417600533,
11.7930077868126));
#116458=CARTESIAN_POINT('Ctrl Pts',(-9.11829773088535,4.11688439372328,
11.7809972449681));
#116459=CARTESIAN_POINT('Ctrl Pts',(-9.06268070530291,4.12279777635008,
11.7164478060619));
#116460=CARTESIAN_POINT('Ctrl Pts',(-9.02229632605453,4.1277739389759,11.6602708617861));
#116461=CARTESIAN_POINT('Ctrl Pts',(-8.95614417321754,4.13726303012911,
11.5487570417756));
#116462=CARTESIAN_POINT('Ctrl Pts',(-8.92928831565067,4.1417416169295,11.4943138304972));
#116463=CARTESIAN_POINT('Ctrl Pts',(-8.90014676754216,4.14737927673124,
11.4215831948789));
#116464=CARTESIAN_POINT('Ctrl Pts',(-8.89392350837116,4.14864410014872,
11.4049745500135));
#116465=CARTESIAN_POINT('Ctrl Pts',(-8.88412702597324,4.15073657759108,
11.3769166802849));
#116466=CARTESIAN_POINT('Ctrl Pts',(-8.88034938154421,4.1515728740737,11.3655423344774));
#116467=CARTESIAN_POINT('Ctrl Pts',(-8.87529005113792,4.15273424403023,
11.3494939725525));
#116468=CARTESIAN_POINT('Ctrl Pts',(-8.87386272242192,4.15306692375363,
11.3448671338819));
#116469=CARTESIAN_POINT('Ctrl Pts',(-8.8714671421849,4.15363392655669,11.3369281190602));
#116470=CARTESIAN_POINT('Ctrl Pts',(-8.87048484797974,4.15386903624528,
11.3336202799735));
#116471=CARTESIAN_POINT('Ctrl Pts',(-8.8684647211989,4.15435803064825,11.3267063742156));
#116472=CARTESIAN_POINT('Ctrl Pts',(-8.86742956766783,4.15461176432302,
11.3230996114546));
#116473=CARTESIAN_POINT('Ctrl Pts',(-8.86470632751593,4.15528803399112,
11.3134371694362));
#116474=CARTESIAN_POINT('Ctrl Pts',(-8.86304942971062,4.15570883886035,
11.3073727167613));
#116475=CARTESIAN_POINT('Ctrl Pts',(-8.8557865665455,4.15759804924544,11.279927210067));
#116476=CARTESIAN_POINT('Ctrl Pts',(-8.85073422503047,4.15903819357584,
11.2584026929605));
#116477=CARTESIAN_POINT('Ctrl Pts',(-8.82924317984186,4.16590219087264,
11.153673125334));
#116478=CARTESIAN_POINT('Ctrl Pts',(-8.82121702098378,4.17103463526259,
11.0689943703428));
#116479=CARTESIAN_POINT('Ctrl Pts',(-8.82311674496046,4.17985462864931,
10.9275625937719));
#116480=CARTESIAN_POINT('Ctrl Pts',(-8.8279592582305,4.18344006776357,10.8710789015476));
#116481=CARTESIAN_POINT('Ctrl Pts',(-8.83868552693927,4.18792415483805,
10.8035784070306));
#116482=CARTESIAN_POINT('Ctrl Pts',(-8.84070004444882,4.18869904614588,
10.7920184036299));
#116483=CARTESIAN_POINT('Ctrl Pts',(-8.8441618316719,4.18993421222923,10.7737700630447));
#116484=CARTESIAN_POINT('Ctrl Pts',(-8.84549528090512,4.19039091276263,
10.767060724652));
#116485=CARTESIAN_POINT('Ctrl Pts',(-8.84811551936153,4.19125418005944,
10.7544523330769));
#116486=CARTESIAN_POINT('Ctrl Pts',(-8.84938937571386,4.19166032623932,
10.7485507955461));
#116487=CARTESIAN_POINT('Ctrl Pts',(-8.85236574208077,4.19257995449355,
10.7352582464699));
#116488=CARTESIAN_POINT('Ctrl Pts',(-8.8540943726802,4.1930942490326,10.7278734216752));
#116489=CARTESIAN_POINT('Ctrl Pts',(-8.85953713761521,4.19465640059544,
10.7055935227753));
#116490=CARTESIAN_POINT('Ctrl Pts',(-8.86347115095915,4.195711170969,10.6907543839071));
#116491=CARTESIAN_POINT('Ctrl Pts',(-8.89269759213039,4.20307420709794,
10.5886155976283));
#116492=CARTESIAN_POINT('Ctrl Pts',(-8.92772778630018,4.20970237084639,
10.5044376979018));
#116493=CARTESIAN_POINT('Ctrl Pts',(-9.00318625361909,4.22104808273707,
10.3695078240405));
#116494=CARTESIAN_POINT('Ctrl Pts',(-9.03876700534044,4.22571692897838,
10.3164863170655));
#116495=CARTESIAN_POINT('Ctrl Pts',(-9.0834080683673,4.23071661314367,10.2603938750841));
#116496=CARTESIAN_POINT('Ctrl Pts',(-9.0884105668474,4.23126620307071,10.2542368317976));
#116497=CARTESIAN_POINT('Ctrl Pts',(-9.09609534446169,4.23209388294506,
10.2449713362918));
#116498=CARTESIAN_POINT('Ctrl Pts',(-9.09873217570549,4.23237498809018,
10.2418257327626));
#116499=CARTESIAN_POINT('Ctrl Pts',(-9.10357236764456,4.23288564434076,
10.2361125682141));
#116500=CARTESIAN_POINT('Ctrl Pts',(-9.10577036706129,4.23311555310008,
10.2335406907896));
#116501=CARTESIAN_POINT('Ctrl Pts',(-9.11075890513035,4.23363291053683,
10.2277542771242));
#116502=CARTESIAN_POINT('Ctrl Pts',(-9.11355581204901,4.23391989205777,
10.2245453692401));
#116503=CARTESIAN_POINT('Ctrl Pts',(-9.12084420734665,4.23466001074259,
10.2162743136332));
#116504=CARTESIAN_POINT('Ctrl Pts',(-9.12536211132016,4.23511130555952,
10.2112355052733));
#116505=CARTESIAN_POINT('Ctrl Pts',(-9.15799282231843,4.23832014852505,
10.1754676793928));
#116506=CARTESIAN_POINT('Ctrl Pts',(-9.18767800847342,4.24097418281745,
10.1462064534804));
#116507=CARTESIAN_POINT('Ctrl Pts',(-9.23336477374673,4.24480256946397,
10.1057173807133));
#116508=CARTESIAN_POINT('Ctrl Pts',(-9.24819064370382,4.24600877827611,
10.0932179434441));
#116509=CARTESIAN_POINT('Ctrl Pts',(-9.30011884296329,4.2501363652677,10.0515876036319));
#116510=CARTESIAN_POINT('Ctrl Pts',(-9.33865747017137,4.25303712323874,
10.024322957885));
#116511=CARTESIAN_POINT('Ctrl Pts',(-9.42011566560855,4.25902874891225,
9.97374334336126));
#116512=CARTESIAN_POINT('Ctrl Pts',(-9.46305497035722,4.26211723545089,
9.95063933483388));
#116513=CARTESIAN_POINT('Ctrl Pts',(-9.52026460450015,4.26622949527544,
9.9242896267536));
#116514=CARTESIAN_POINT('Ctrl Pts',(-9.53333806667504,4.26716883333011,
9.91855399199684));
#116515=CARTESIAN_POINT('Ctrl Pts',(-9.55332131269216,4.26860570687354,
9.9102166964114));
#116516=CARTESIAN_POINT('Ctrl Pts',(-9.56015692971892,4.26909739586418,
9.90743990194864));
#116517=CARTESIAN_POINT('Ctrl Pts',(-9.57262613945093,4.26999486240817,
9.90251058710886));
#116518=CARTESIAN_POINT('Ctrl Pts',(-9.57825107500133,4.27039991631639,
9.90033674698008));
#116519=CARTESIAN_POINT('Ctrl Pts',(-9.59044803797316,4.27127878257451,
9.89573039547568));
#116520=CARTESIAN_POINT('Ctrl Pts',(-9.59702554792629,4.27175308049506,
9.89331316245796));
#116521=CARTESIAN_POINT('Ctrl Pts',(-9.61506887717908,4.27305532179186,
9.88686442559264));
#116522=CARTESIAN_POINT('Ctrl Pts',(-9.62657588009894,4.27388709042424,
9.88295157497811));
#116523=CARTESIAN_POINT('Ctrl Pts',(-9.69469245384951,4.27881992435266,
9.86095926410189));
#116524=CARTESIAN_POINT('Ctrl Pts',(-9.75252715560894,4.28305149012379,
9.84701279130022));
#116525=CARTESIAN_POINT('Ctrl Pts',(-9.81114931893004,4.28736676513878,
9.8374895773545));
#116526=CARTESIAN_POINT('Origin',(-10.,2.67563288526385,11.));
#116527=CARTESIAN_POINT('',(-9.81114928033716,4.88742944471338,9.83748958362395));
#116528=CARTESIAN_POINT('',(-9.81114930150159,4.7888800033368,9.83748958018577));
#116529=CARTESIAN_POINT('',(-9.81114930150157,2.67563288526385,9.83748958018577));
#116530=CARTESIAN_POINT('Ctrl Pts',(-9.81114928023156,4.88742944622416,
9.8374895836411));
#116531=CARTESIAN_POINT('Ctrl Pts',(-9.78935088328749,4.88586560561609,
9.84103075015003));
#116532=CARTESIAN_POINT('Ctrl Pts',(-9.76765219414491,4.884285230485,9.84518501267445));
#116533=CARTESIAN_POINT('Ctrl Pts',(-9.69802535573987,4.87914157996404,
9.86055799325162));
#116534=CARTESIAN_POINT('Ctrl Pts',(-9.65068647776341,4.87552991262804,
9.87416860760851));
#116535=CARTESIAN_POINT('Ctrl Pts',(-9.58516738225473,4.8704258024824,9.89753760209531));
#116536=CARTESIAN_POINT('Ctrl Pts',(-9.56617441987963,4.86893359467803,
9.90487223059995));
#116537=CARTESIAN_POINT('Ctrl Pts',(-9.5080573735057,4.86434257286067,9.92906498398443));
#116538=CARTESIAN_POINT('Ctrl Pts',(-9.46964630448459,4.86127168932063,
9.94755754742094));
#116539=CARTESIAN_POINT('Ctrl Pts',(-9.42636526504175,4.85783046383883,
9.97136769745121));
#116540=CARTESIAN_POINT('Ctrl Pts',(-9.42044071952102,4.85735986507994,
9.97469406089045));
#116541=CARTESIAN_POINT('Ctrl Pts',(-9.41084442113239,4.85659875478454,
9.98019170604868));
#116542=CARTESIAN_POINT('Ctrl Pts',(-9.40715519065467,4.85630642943153,
9.98233193722733));
#116543=CARTESIAN_POINT('Ctrl Pts',(-9.40055824947098,4.85578431568561,
9.98620706573903));
#116544=CARTESIAN_POINT('Ctrl Pts',(-9.3976463228998,4.85555407540329,9.98793450094272));
#116545=CARTESIAN_POINT('Ctrl Pts',(-9.39122158146995,4.8550465792897,9.99178338708724));
#116546=CARTESIAN_POINT('Ctrl Pts',(-9.38771237679128,4.85476969933343,
9.99391065547778));
#116547=CARTESIAN_POINT('Ctrl Pts',(-9.37746957216578,4.85396223780954,
10.0001932512222));
#116548=CARTESIAN_POINT('Ctrl Pts',(-9.3707664842563,4.85343471935769,10.0043982425234));
#116549=CARTESIAN_POINT('Ctrl Pts',(-9.31069721575149,4.84871072062784,
10.0429300201396));
#116550=CARTESIAN_POINT('Ctrl Pts',(-9.2601363207659,4.8447552483553,10.0814547848116));
#116551=CARTESIAN_POINT('Ctrl Pts',(-9.14509364953285,4.83517350826218,
10.1848046140644));
#116552=CARTESIAN_POINT('Ctrl Pts',(-9.08457940318283,4.8295833148745,10.2534000512102));
#116553=CARTESIAN_POINT('Ctrl Pts',(-9.02384554462224,4.82264392370784,
10.3408700554137));
#116554=CARTESIAN_POINT('Ctrl Pts',(-9.0153539897059,4.82163716406329,10.3536239454152));
#116555=CARTESIAN_POINT('Ctrl Pts',(-9.00303472580952,4.82011836423999,
10.3729331575823));
#116556=CARTESIAN_POINT('Ctrl Pts',(-8.99901744316373,4.81961325655743,
10.3793660505472));
#116557=CARTESIAN_POINT('Ctrl Pts',(-8.99191082418715,4.81870153798718,
10.3909944111676));
#116558=CARTESIAN_POINT('Ctrl Pts',(-8.98879879813591,4.81829576559348,
10.396175753513));
#116559=CARTESIAN_POINT('Ctrl Pts',(-8.98224236697227,4.81742665264136,
10.4072846712908));
#116560=CARTESIAN_POINT('Ctrl Pts',(-8.97880957413239,4.81696291536751,
10.4132188046981));
#116561=CARTESIAN_POINT('Ctrl Pts',(-8.9696199967512,4.81569732194231,10.4294293618923));
#116562=CARTESIAN_POINT('Ctrl Pts',(-8.96396538661737,4.81489190359518,
10.4397624909176));
#116563=CARTESIAN_POINT('Ctrl Pts',(-8.93164803050363,4.81012625115241,
10.5009816121629));
#116564=CARTESIAN_POINT('Ctrl Pts',(-8.90858624262785,4.80604335559248,
10.5536710924557));
#116565=CARTESIAN_POINT('Ctrl Pts',(-8.86310113160392,4.79613458815596,
10.682473260286));
#116566=CARTESIAN_POINT('Ctrl Pts',(-8.84433450764669,4.79025083081842,
10.7595855403343));
#116567=CARTESIAN_POINT('Ctrl Pts',(-8.8298473150328,4.78267198524842,10.8639046067092));
#116568=CARTESIAN_POINT('Ctrl Pts',(-8.82711309537822,4.78081387093843,
10.889928172748));
#116569=CARTESIAN_POINT('Ctrl Pts',(-8.824773532442,4.7785341610091,10.9226563835733));
#116570=CARTESIAN_POINT('Ctrl Pts',(-8.82435554332993,4.7780747864903,10.929293552698));
#116571=CARTESIAN_POINT('Ctrl Pts',(-8.82378517736112,4.77735515174573,
10.9397633015969));
#116572=CARTESIAN_POINT('Ctrl Pts',(-8.82359527169342,4.77709293381873,
10.9435935721269));
#116573=CARTESIAN_POINT('Ctrl Pts',(-8.82327115050244,4.77659844650349,
10.9508470485647));
#116574=CARTESIAN_POINT('Ctrl Pts',(-8.82313316132455,4.77636599007145,
10.9542698982325));
#116575=CARTESIAN_POINT('Ctrl Pts',(-8.82284229358829,4.77581845532227,
10.9623619829776));
#116576=CARTESIAN_POINT('Ctrl Pts',(-8.8227022584358,4.77550408052008,10.9670315963024));
#116577=CARTESIAN_POINT('Ctrl Pts',(-8.82232716560084,4.7744583097091,10.9826382937824));
#116578=CARTESIAN_POINT('Ctrl Pts',(-8.82221669438312,4.77373333411558,
10.9935781829952));
#116579=CARTESIAN_POINT('Ctrl Pts',(-8.82231884241623,4.77198515462371,
11.0202029591469));
#116580=CARTESIAN_POINT('Ctrl Pts',(-8.82269232899375,4.77096913520445,
11.0358854486177));
#116581=CARTESIAN_POINT('Ctrl Pts',(-8.82549279781047,4.76686750495758,
11.0997975997953));
#116582=CARTESIAN_POINT('Ctrl Pts',(-8.83057156803924,4.7638720742231,11.1478667205664));
#116583=CARTESIAN_POINT('Ctrl Pts',(-8.85275230224345,4.75560163230495,
11.2796422688943));
#116584=CARTESIAN_POINT('Ctrl Pts',(-8.87601823205132,4.75034725401852,
11.3619945436492));
#116585=CARTESIAN_POINT('Ctrl Pts',(-8.91387476661186,4.74376539921164,
11.4557139596163));
#116586=CARTESIAN_POINT('Ctrl Pts',(-8.920067223747,4.742730800921,11.4702003789319));
#116587=CARTESIAN_POINT('Ctrl Pts',(-8.92970272987694,4.74117826885783,
11.491546137922));
#116588=CARTESIAN_POINT('Ctrl Pts',(-8.93292542414599,4.74066774071938,
11.4985034574213));
#116589=CARTESIAN_POINT('Ctrl Pts',(-8.9388129675024,4.73975009953142,11.5108950689445));
#116590=CARTESIAN_POINT('Ctrl Pts',(-8.94145223039851,4.73934387104034,
11.5163412694653));
#116591=CARTESIAN_POINT('Ctrl Pts',(-8.94714711068771,4.73847792874671,
11.5278656408669));
#116592=CARTESIAN_POINT('Ctrl Pts',(-8.95021364080381,4.73801785015515,
11.5339381406458));
#116593=CARTESIAN_POINT('Ctrl Pts',(-8.95862112944483,4.73677270649401,
11.5502346434823));
#116594=CARTESIAN_POINT('Ctrl Pts',(-8.96405984860207,4.73598427211538,
11.5604070852986));
#116595=CARTESIAN_POINT('Ctrl Pts',(-8.99498602149185,4.73159128775035,
11.6162616085485));
#116596=CARTESIAN_POINT('Ctrl Pts',(-9.02334221066041,4.72788606487821,
11.6602799770764));
#116597=CARTESIAN_POINT('Ctrl Pts',(-9.10149720517369,4.71841208696263,
11.7655019380811));
#116598=CARTESIAN_POINT('Ctrl Pts',(-9.15469117032413,4.71256210582804,
11.8238643759852));
#116599=CARTESIAN_POINT('Ctrl Pts',(-9.23674938252155,4.7045849875174,11.8975163123333));
#116600=CARTESIAN_POINT('Ctrl Pts',(-9.26102516843012,4.70233613450133,
11.9176075507893));
#116601=CARTESIAN_POINT('Ctrl Pts',(-9.29158494747188,4.69966357540991,
11.9408990874632));
#116602=CARTESIAN_POINT('Ctrl Pts',(-9.29712745726284,4.69918495391991,
11.9450466516835));
#116603=CARTESIAN_POINT('Ctrl Pts',(-9.30587757506763,4.69843923848597,
11.9514749633381));
#116604=CARTESIAN_POINT('Ctrl Pts',(-9.30906048701106,4.69817000551934,
11.9537888325944));
#116605=CARTESIAN_POINT('Ctrl Pts',(-9.3147403149997,4.69769324130179,11.9578745218285));
#116606=CARTESIAN_POINT('Ctrl Pts',(-9.31723255137716,4.69748529779839,
11.9596525657217));
#116607=CARTESIAN_POINT('Ctrl Pts',(-9.32324123861699,4.69698692789213,
11.9639041050822));
#116608=CARTESIAN_POINT('Ctrl Pts',(-9.32676433278709,4.69669714003421,
11.9663680886446));
#116609=CARTESIAN_POINT('Ctrl Pts',(-9.33761411837906,4.69581184523313,
11.9738680842505));
#116610=CARTESIAN_POINT('Ctrl Pts',(-9.34498460395086,4.69522036158093,
11.9788406122913));
#116611=CARTESIAN_POINT('Ctrl Pts',(-9.39678491442307,4.69112669804982,
12.0129407560385));
#116612=CARTESIAN_POINT('Ctrl Pts',(-9.44309045240427,4.68778757293291,
12.0391201096924));
#116613=CARTESIAN_POINT('Ctrl Pts',(-9.57402772706918,4.67876200021067,
12.1018698957587));
#116614=CARTESIAN_POINT('Ctrl Pts',(-9.66141521300852,4.67315520043928,
12.1317812601404));
#116615=CARTESIAN_POINT('Ctrl Pts',(-9.77116144926607,4.66590046667336,
12.1554812977025));
#116616=CARTESIAN_POINT('Ctrl Pts',(-9.79103636417713,4.66457991090727,
12.1592403688672));
#116617=CARTESIAN_POINT('Ctrl Pts',(-9.81872901891244,4.66272586824122,
12.1637427780793));
#116618=CARTESIAN_POINT('Ctrl Pts',(-9.82647292350091,4.66220590662008,
12.1649226459023));
#116619=CARTESIAN_POINT('Ctrl Pts',(-9.83987605973425,4.66130309556185,
12.1668281506324));
#116620=CARTESIAN_POINT('Ctrl Pts',(-9.84552992403799,4.66092138466888,
12.1675900834829));
#116621=CARTESIAN_POINT('Ctrl Pts',(-9.85729087800224,4.6601254346971,12.1690881086357));
#116622=CARTESIAN_POINT('Ctrl Pts',(-9.86339863178913,4.6597109997397,12.1698174913179));
#116623=CARTESIAN_POINT('Ctrl Pts',(-9.877836390027,4.65872866243836,12.1714270255873));
#116624=CARTESIAN_POINT('Ctrl Pts',(-9.88617053079292,4.65815950906774,
12.172266211038));
#116625=CARTESIAN_POINT('Ctrl Pts',(-9.91418311736064,4.65623903703907,
12.1747853328779));
#116626=CARTESIAN_POINT('Ctrl Pts',(-9.93389378768376,4.65487534432103,
12.1760590984233));
#116627=CARTESIAN_POINT('Ctrl Pts',(-9.98162049705699,4.65154151061157,
12.1779397927006));
#116628=CARTESIAN_POINT('Ctrl Pts',(-10.0096432324052,4.64955741754914,
12.178043615419));
#116629=CARTESIAN_POINT('Ctrl Pts',(-10.1435302956369,4.63995600755402,
12.173762359381));
#116630=CARTESIAN_POINT('Ctrl Pts',(-10.2484650167861,4.63201013804697,
12.1561059782564));
#116631=CARTESIAN_POINT('Ctrl Pts',(-10.3666773423264,4.62319865589227,
12.1193578129637));
#116632=CARTESIAN_POINT('Ctrl Pts',(-10.383614430605,4.62194127412702,12.1136670235969));
#116633=CARTESIAN_POINT('Ctrl Pts',(-10.4058999067678,4.62029935988162,
12.1056103857407));
#116634=CARTESIAN_POINT('Ctrl Pts',(-10.4113686094444,4.61989746161655,
12.1035873006045));
#116635=CARTESIAN_POINT('Ctrl Pts',(-10.4202402173155,4.61924739372102,
12.1002302386096));
#116636=CARTESIAN_POINT('Ctrl Pts',(-10.4236522536035,4.61899783945435,
12.0989209194205));
#116637=CARTESIAN_POINT('Ctrl Pts',(-10.4303270736903,4.61851063261477,
12.0963238460185));
#116638=CARTESIAN_POINT('Ctrl Pts',(-10.4335902764236,4.61827291578774,
12.0950373684737));
#116639=CARTESIAN_POINT('Ctrl Pts',(-10.4416216244056,4.61768890065987,
12.0918295788202));
#116640=CARTESIAN_POINT('Ctrl Pts',(-10.4463831047845,4.61734357547912,
12.0898915608987));
#116641=CARTESIAN_POINT('Ctrl Pts',(-10.4640367009841,4.6160661161042,12.0825710942364));
#116642=CARTESIAN_POINT('Ctrl Pts',(-10.4768460109367,4.61514490297321,
12.0769903238631));
#116643=CARTESIAN_POINT('Ctrl Pts',(-10.5094744755595,4.61280552977485,
12.062078409285));
#116644=CARTESIAN_POINT('Ctrl Pts',(-10.5291386823864,4.61140256083007,
12.0524196690198));
#116645=CARTESIAN_POINT('Ctrl Pts',(-10.5908233230821,4.60698853854376,
12.0199548002418));
#116646=CARTESIAN_POINT('Ctrl Pts',(-10.6317310498277,4.60404009413044,
11.9951363422169));
#116647=CARTESIAN_POINT('Ctrl Pts',(-10.7325804761389,4.5964484446862,11.9252201048143));
#116648=CARTESIAN_POINT('Ctrl Pts',(-10.7899226762571,4.59180006704116,
11.8767706475621));
#116649=CARTESIAN_POINT('Ctrl Pts',(-10.8535185562632,4.58587867745126,
11.8117019056287));
#116650=CARTESIAN_POINT('Ctrl Pts',(-10.8645266226401,4.58482250137414,
11.7999672417249));
#116651=CARTESIAN_POINT('Ctrl Pts',(-10.8804632275538,4.5832438646828,11.782265516363));
#116652=CARTESIAN_POINT('Ctrl Pts',(-10.8855791931164,4.58272918665431,
11.776469137266));
#116653=CARTESIAN_POINT('Ctrl Pts',(-10.8946020246303,4.58180695869125,
11.7660411147553));
#116654=CARTESIAN_POINT('Ctrl Pts',(-10.898530948527,4.58140032856354,11.7614288569319));
#116655=CARTESIAN_POINT('Ctrl Pts',(-10.9067712702278,4.58053656742262,
11.7516027516027));
#116656=CARTESIAN_POINT('Ctrl Pts',(-10.9110736653269,4.58007909479101,
11.746381675673));
#116657=CARTESIAN_POINT('Ctrl Pts',(-10.922480061762,4.57884850040848,11.7322941184548));
#116658=CARTESIAN_POINT('Ctrl Pts',(-10.9295009946528,4.5780721439498,11.7233616146462));
#116659=CARTESIAN_POINT('Ctrl Pts',(-10.966214025614,4.57390872849835,11.6752356718678));
#116660=CARTESIAN_POINT('Ctrl Pts',(-10.9935552030944,4.57043330897733,
11.6343182600281));
#116661=CARTESIAN_POINT('Ctrl Pts',(-11.0433495994662,4.56328808529452,
11.548643987611));
#116662=CARTESIAN_POINT('Ctrl Pts',(-11.0656696076276,4.55962319867447,
11.5039209839741));
#116663=CARTESIAN_POINT('Ctrl Pts',(-11.0934021420118,4.55438963568818,
11.4382061677087));
#116664=CARTESIAN_POINT('Ctrl Pts',(-11.1011828247663,4.5528212810994,11.4182694194178));
#116665=CARTESIAN_POINT('Ctrl Pts',(-11.122444905285,4.54823706237586,11.3590748175927));
#116666=CARTESIAN_POINT('Ctrl Pts',(-11.1344011184732,4.54524778835645,
11.319299463151));
#116667=CARTESIAN_POINT('Ctrl Pts',(-11.1458345967664,4.54188555681425,
11.2724038241856));
#116668=CARTESIAN_POINT('Ctrl Pts',(-11.1473794057222,4.54141733013264,
11.2658218786926));
#116669=CARTESIAN_POINT('Ctrl Pts',(-11.1498040121204,4.54065927430008,
11.2550762636829));
#116670=CARTESIAN_POINT('Ctrl Pts',(-11.1507180472539,4.54036765454002,
11.2509205924777));
#116671=CARTESIAN_POINT('Ctrl Pts',(-11.1523188590524,4.53984627495291,
11.2434497287522));
#116672=CARTESIAN_POINT('Ctrl Pts',(-11.1530138804904,4.53961606914807,
11.240136452052));
#116673=CARTESIAN_POINT('Ctrl Pts',(-11.1545215403728,4.53910801973409,
11.2327917240606));
#116674=CARTESIAN_POINT('Ctrl Pts',(-11.1553273576541,4.53883055728417,
11.2287589821495));
#116675=CARTESIAN_POINT('Ctrl Pts',(-11.1576300130813,4.53801964959261,
11.216912668126));
#116676=CARTESIAN_POINT('Ctrl Pts',(-11.1590688609997,4.53748930737678,
11.2090878684105));
#116677=CARTESIAN_POINT('Ctrl Pts',(-11.1621953530721,4.53627830984126,
11.1910600862751));
#116678=CARTESIAN_POINT('Ctrl Pts',(-11.1638281512367,4.53560030423341,
11.1808481287856));
#116679=CARTESIAN_POINT('Ctrl Pts',(-11.1689154539555,4.53331630767468,
11.1461012056031));
#116680=CARTESIAN_POINT('Ctrl Pts',(-11.1717304074329,4.53173645267795,
11.1214780264382));
#116681=CARTESIAN_POINT('Ctrl Pts',(-11.1780890175756,4.52685905695322,
11.0443618685767));
#116682=CARTESIAN_POINT('Ctrl Pts',(-11.1788949953248,4.52362810332556,
10.9917081161661));
#116683=CARTESIAN_POINT('Ctrl Pts',(-11.1724719151175,4.51592269433473,
10.8675043427265));
#116684=CARTESIAN_POINT('Ctrl Pts',(-11.1622232749476,4.51143343985635,
10.7963321732177));
#116685=CARTESIAN_POINT('Ctrl Pts',(-11.1427326533986,4.50593269969573,
10.7146830681849));
#116686=CARTESIAN_POINT('Ctrl Pts',(-11.1397183487971,4.50512844291463,
10.7028708426992));
#116687=CARTESIAN_POINT('Ctrl Pts',(-11.1346814391405,4.50385221604343,
10.68433830365));
#116688=CARTESIAN_POINT('Ctrl Pts',(-11.1327811409424,4.50338414667368,
10.6775854252382));
#116689=CARTESIAN_POINT('Ctrl Pts',(-11.1291357535778,4.5025102018442,10.6650614089987));
#116690=CARTESIAN_POINT('Ctrl Pts',(-11.1274064489855,4.50210484581669,
10.6592858878423));
#116691=CARTESIAN_POINT('Ctrl Pts',(-11.1234659104343,4.50120101618447,
10.6464838475428));
#116692=CARTESIAN_POINT('Ctrl Pts',(-11.1212329599107,4.50070185444174,
10.6394643328258));
#116693=CARTESIAN_POINT('Ctrl Pts',(-11.1144968471133,4.49923276753994,
10.6189566371282));
#116694=CARTESIAN_POINT('Ctrl Pts',(-11.1098152129217,4.49825710258634,
10.605528924841));
#116695=CARTESIAN_POINT('Ctrl Pts',(-11.0800532894808,4.49231199834423,
10.5248941063271));
#116696=CARTESIAN_POINT('Ctrl Pts',(-11.0491229812589,4.48715011053184,
10.4600199533741));
#116697=CARTESIAN_POINT('Ctrl Pts',(-10.9705335679791,4.47589317269532,
10.3277604434209));
#116698=CARTESIAN_POINT('Ctrl Pts',(-10.921302147259,4.46980001440404,10.2617279248));
#116699=CARTESIAN_POINT('Ctrl Pts',(-10.8591420552707,4.46338118288953,
10.1943570294853));
#116700=CARTESIAN_POINT('Ctrl Pts',(-10.8526025098898,4.46271967824316,
10.1874394535999));
#116701=CARTESIAN_POINT('Ctrl Pts',(-10.8429380636886,4.46176291679154,
10.1774614935414));
#116702=CARTESIAN_POINT('Ctrl Pts',(-10.8398790454551,4.4614630543714,10.1743382264131));
#116703=CARTESIAN_POINT('Ctrl Pts',(-10.8344114948334,4.46093246847359,
10.1688176695815));
#116704=CARTESIAN_POINT('Ctrl Pts',(-10.8320098903734,4.46070123296669,
10.1664136802313));
#116705=CARTESIAN_POINT('Ctrl Pts',(-10.8267832916401,4.46020195052738,
10.161226983148));
#116706=CARTESIAN_POINT('Ctrl Pts',(-10.8239546257036,4.45993419493283,
10.1584481233624));
#116707=CARTESIAN_POINT('Ctrl Pts',(-10.8159123295414,4.45917965934843,
10.1506268552643));
#116708=CARTESIAN_POINT('Ctrl Pts',(-10.8106659702057,4.45869536207058,
10.1456181417232));
#116709=CARTESIAN_POINT('Ctrl Pts',(-10.7738073029846,4.45534469761582,
10.1110742739515));
#116710=CARTESIAN_POINT('Ctrl Pts',(-10.7406310742971,4.45259057852758,
10.0832485641292));
#116711=CARTESIAN_POINT('Ctrl Pts',(-10.6320453469658,4.44409095950227,
10.0019271374568));
#116712=CARTESIAN_POINT('Ctrl Pts',(-10.5518388566261,4.43850384445114,
9.95544033677818));
#116713=CARTESIAN_POINT('Ctrl Pts',(-10.4399497825646,4.43072433830512,
9.90710981141323));
#116714=CARTESIAN_POINT('Ctrl Pts',(-10.4124488876198,4.42881605951598,
9.89643737578552));
#116715=CARTESIAN_POINT('Ctrl Pts',(-10.3751064692611,4.42621405895943,
9.88353655708448));
#116716=CARTESIAN_POINT('Ctrl Pts',(-10.3655936596621,4.42555033062063,
9.88038544646553));
#116717=CARTESIAN_POINT('Ctrl Pts',(-10.349869075622,4.42445119030145,9.87539845698945));
#116718=CARTESIAN_POINT('Ctrl Pts',(-10.3436801819509,4.42401808484502,
9.87349170872139));
#116719=CARTESIAN_POINT('Ctrl Pts',(-10.3315806777661,4.42317021511648,
9.86987293631155));
#116720=CARTESIAN_POINT('Ctrl Pts',(-10.3256717452688,4.4227556247994,9.86815600111354));
#116721=CARTESIAN_POINT('Ctrl Pts',(-10.3116756534665,4.42177224390696,
9.86420788540265));
#116722=CARTESIAN_POINT('Ctrl Pts',(-10.3035776641246,4.42120219489107,
9.86201668022578));
#116723=CARTESIAN_POINT('Ctrl Pts',(-10.2762625421271,4.4192753790898,9.85493788520672));
#116724=CARTESIAN_POINT('Ctrl Pts',(-10.2569464649077,4.41790612635147,
9.85044936139298));
#116725=CARTESIAN_POINT('Ctrl Pts',(-10.1294256696776,4.40881756920577,
9.82419156072048));
#116726=CARTESIAN_POINT('Ctrl Pts',(-10.0187439281125,4.40062467277096,
9.81724218644562));
#116727=CARTESIAN_POINT('Ctrl Pts',(-9.87606656163429,4.39021398731939,
9.82833022979994));
#116728=CARTESIAN_POINT('Ctrl Pts',(-9.84350542182004,4.38785451689339,
9.83223330385834));
#116729=CARTESIAN_POINT('Ctrl Pts',(-9.81114929917643,4.38555086460676,
9.83748958056349));
#116730=CARTESIAN_POINT('Ctrl Pts',(-9.81114931893004,4.28736676513878,
9.8374895773545));
#116731=CARTESIAN_POINT('Ctrl Pts',(-9.8176029126927,4.28784182491725,9.83644118625737));
#116732=CARTESIAN_POINT('Ctrl Pts',(-9.82406605585664,4.28831781899759,
9.83544640201666));
#116733=CARTESIAN_POINT('Ctrl Pts',(-9.91549711542973,4.29505360548248,
9.82215240518902));
#116734=CARTESIAN_POINT('Ctrl Pts',(-10.0015534061697,4.30144350458995,
9.8191256241258));
#116735=CARTESIAN_POINT('Ctrl Pts',(-10.1003602461953,4.3084360922676,9.82645934817442));
#116736=CARTESIAN_POINT('Ctrl Pts',(-10.1135276330211,4.3093603270354,9.82765988147998));
#116737=CARTESIAN_POINT('Ctrl Pts',(-10.1316771713635,4.31062127344421,
9.82962334134962));
#116738=CARTESIAN_POINT('Ctrl Pts',(-10.1366782575393,4.31096735884294,
9.83019682989313));
#116739=CARTESIAN_POINT('Ctrl Pts',(-10.1451378796171,4.31155029517138,
9.83122191087831));
#116740=CARTESIAN_POINT('Ctrl Pts',(-10.1485983319158,4.31178804162246,
9.83165683008288));
#116741=CARTESIAN_POINT('Ctrl Pts',(-10.1557141877214,4.31227541003412,
9.83258329772278));
#116742=CARTESIAN_POINT('Ctrl Pts',(-10.1593692848611,4.3125249319178,9.8330766533318));
#116743=CARTESIAN_POINT('Ctrl Pts',(-10.1689490584446,4.3131769099589,9.83441555707696));
#116744=CARTESIAN_POINT('Ctrl Pts',(-10.1748698047786,4.31357785099239,
9.83528912039918));
#116745=CARTESIAN_POINT('Ctrl Pts',(-10.1997328823759,4.3152540384694,9.83915135747098));
#116746=CARTESIAN_POINT('Ctrl Pts',(-10.2186085711031,4.31650827410858,
9.84255747940336));
#116747=CARTESIAN_POINT('Ctrl Pts',(-10.2632354874528,4.31944797778381,
9.85174122760832));
#116748=CARTESIAN_POINT('Ctrl Pts',(-10.2888926705017,4.32111764828848,
9.85792630662254));
#116749=CARTESIAN_POINT('Ctrl Pts',(-10.3686225275086,4.32630117029982,
9.88000572296107));
#116750=CARTESIAN_POINT('Ctrl Pts',(-10.4217751150709,4.32975253131279,
9.89892061542318));
#116751=CARTESIAN_POINT('Ctrl Pts',(-10.5263460200968,4.33685486313371,
9.94482132151407));
#116752=CARTESIAN_POINT('Ctrl Pts',(-10.5775299905111,4.34049992035176,
9.97194353755557));
#116753=CARTESIAN_POINT('Ctrl Pts',(-10.6385455950005,4.34520488486823,
10.0102744882102));
#116754=CARTESIAN_POINT('Ctrl Pts',(-10.6504422952424,4.3461401581382,10.0180520085386));
#116755=CARTESIAN_POINT('Ctrl Pts',(-10.6682843493942,4.34757195813149,
10.0301828455577));
#116756=CARTESIAN_POINT('Ctrl Pts',(-10.6743346805138,4.34806269815868,
10.0343799819663));
#116757=CARTESIAN_POINT('Ctrl Pts',(-10.6852650846769,4.34895901403887,
10.0421152706204));
#116758=CARTESIAN_POINT('Ctrl Pts',(-10.6901581461131,4.34936387296301,
10.0456347019598));
#116759=CARTESIAN_POINT('Ctrl Pts',(-10.7006862924606,4.35024298085217,
10.0533305873043));
#116760=CARTESIAN_POINT('Ctrl Pts',(-10.7063114877112,4.35071772050998,
10.0575201137276));
#116761=CARTESIAN_POINT('Ctrl Pts',(-10.7216094924051,4.35202287284885,
10.0691276196982));
#116762=CARTESIAN_POINT('Ctrl Pts',(-10.731204858794,4.35285714296539,10.0766457434577));
#116763=CARTESIAN_POINT('Ctrl Pts',(-10.796502445049,4.35864544050587,10.1294635944975));
#116764=CARTESIAN_POINT('Ctrl Pts',(-10.8480677882746,4.36379630652066,
10.1796174884723));
#116765=CARTESIAN_POINT('Ctrl Pts',(-10.9289553239716,4.37288806274017,
10.2741173188097));
#116766=CARTESIAN_POINT('Ctrl Pts',(-10.9604536172668,4.37677112949434,
10.3163388500359));
#116767=CARTESIAN_POINT('Ctrl Pts',(-11.0024737972854,4.38239215705284,
10.3813280165174));
#116768=CARTESIAN_POINT('Ctrl Pts',(-11.0152655193393,4.38417591325399,
10.4025514105242));
#116769=CARTESIAN_POINT('Ctrl Pts',(-11.0324341194424,4.38666339097465,
10.4331827905196));
#116770=CARTESIAN_POINT('Ctrl Pts',(-11.0373704309133,4.38739068759862,
10.4422683751598));
#116771=CARTESIAN_POINT('Ctrl Pts',(-11.0458915231141,4.38866659912175,
10.4584566031053));
#116772=CARTESIAN_POINT('Ctrl Pts',(-11.0495251377214,4.38921768947345,
10.4655326738455));
#116773=CARTESIAN_POINT('Ctrl Pts',(-11.0549277393483,4.39004731762736,
10.4763212540827));
#116774=CARTESIAN_POINT('Ctrl Pts',(-11.0567493481242,4.39032888585328,
10.4800069416803));
#116775=CARTESIAN_POINT('Ctrl Pts',(-11.0600351382682,4.39084006462629,
10.4867437093701));
#116776=CARTESIAN_POINT('Ctrl Pts',(-11.0615054867223,4.39107003641809,
10.4897915949931));
#116777=CARTESIAN_POINT('Ctrl Pts',(-11.064793933245,4.39158718435804,10.4966839698019));
#116778=CARTESIAN_POINT('Ctrl Pts',(-11.066604362527,4.3918738963073,10.5005320012464));
#116779=CARTESIAN_POINT('Ctrl Pts',(-11.071236799887,4.39261297413039,10.510518212821));
#116780=CARTESIAN_POINT('Ctrl Pts',(-11.0740269543595,4.39306350502977,
10.516671118258));
#116781=CARTESIAN_POINT('Ctrl Pts',(-11.09423202715,4.39636897974889,10.5622668418));
#116782=CARTESIAN_POINT('Ctrl Pts',(-11.109524309971,4.39911267563124,10.6026201661121));
#116783=CARTESIAN_POINT('Ctrl Pts',(-11.1285947471217,4.40306160565966,
10.6627084393003));
#116784=CARTESIAN_POINT('Ctrl Pts',(-11.1341370122423,4.40429934542467,
10.6818412803923));
#116785=CARTESIAN_POINT('Ctrl Pts',(-11.1519202813151,4.40864222409862,
10.7496196157493));
#116786=CARTESIAN_POINT('Ctrl Pts',(-11.1615367472825,4.41172692598226,
10.7988957762677));
#116787=CARTESIAN_POINT('Ctrl Pts',(-11.1742623401533,4.41793383306148,
10.8970901689433));
#116788=CARTESIAN_POINT('Ctrl Pts',(-11.1775199086907,4.42104699064732,
10.9458845685595));
#116789=CARTESIAN_POINT('Ctrl Pts',(-11.1777889193395,4.42499948822347,
11.006076527421));
#116790=CARTESIAN_POINT('Ctrl Pts',(-11.1776758112269,4.42574887434394,
11.0174164216368));
#116791=CARTESIAN_POINT('Ctrl Pts',(-11.1772339670548,4.4269529486864,11.0355096328468));
#116792=CARTESIAN_POINT('Ctrl Pts',(-11.1770107960306,4.42740437628947,
11.0422649976929));
#116793=CARTESIAN_POINT('Ctrl Pts',(-11.1764774030606,4.42826376538773,
11.055069679104));
#116794=CARTESIAN_POINT('Ctrl Pts',(-11.1761786350201,4.42867135941875,
11.061119273904));
#116795=CARTESIAN_POINT('Ctrl Pts',(-11.1753921587998,4.42960271725558,
11.0748875810885));
#116796=CARTESIAN_POINT('Ctrl Pts',(-11.1748750601296,4.43012737315115,
11.0826042669487));
#116797=CARTESIAN_POINT('Ctrl Pts',(-11.1730463342591,4.43175248122253,
11.1063814520022));
#116798=CARTESIAN_POINT('Ctrl Pts',(-11.1714811221476,4.43286067986431,
11.1224199804469));
#116799=CARTESIAN_POINT('Ctrl Pts',(-11.1614619840533,4.43877660475674,
11.2070768209603));
#116800=CARTESIAN_POINT('Ctrl Pts',(-11.1473084651564,4.44375780042572,
11.2748730517339));
#116801=CARTESIAN_POINT('Ctrl Pts',(-11.109792181109,4.45323928603169,11.3988865593206));
#116802=CARTESIAN_POINT('Ctrl Pts',(-11.0878597431626,4.45770488081936,
11.4553139009629));
#116803=CARTESIAN_POINT('Ctrl Pts',(-11.0540281136573,4.46332795361206,
11.5257691978859));
#116804=CARTESIAN_POINT('Ctrl Pts',(-11.0460050614667,4.46459062953133,
11.54155516174));
#116805=CARTESIAN_POINT('Ctrl Pts',(-11.03196640375,4.4666799275982,11.567700333859));
#116806=CARTESIAN_POINT('Ctrl Pts',(-11.0261433973429,4.46751515649371,
11.5781592195697));
#116807=CARTESIAN_POINT('Ctrl Pts',(-11.0177431716448,4.4686753351643,11.5927202741614));
#116808=CARTESIAN_POINT('Ctrl Pts',(-11.0152987908928,4.46900786758517,
11.5968976914875));
#116809=CARTESIAN_POINT('Ctrl Pts',(-11.011067432765,4.46957475519306,11.6040278295014));
#116810=CARTESIAN_POINT('Ctrl Pts',(-11.0092931185738,4.46980989486945,
11.6069879525041));
#116811=CARTESIAN_POINT('Ctrl Pts',(-11.0055599974178,4.47029924075484,
11.6131543607253));
#116812=CARTESIAN_POINT('Ctrl Pts',(-11.0035988323984,4.4705532939128,11.6163591186031));
#116813=CARTESIAN_POINT('Ctrl Pts',(-10.9983089297511,4.47123069022618,
11.6249112067222));
#116814=CARTESIAN_POINT('Ctrl Pts',(-10.9949525197387,4.4716522963643,11.6302414008273));
#116815=CARTESIAN_POINT('Ctrl Pts',(-10.9795762377741,4.47354835843217,
11.65423091468));
#116816=CARTESIAN_POINT('Ctrl Pts',(-10.9670722889544,4.47499434479083,
11.6725764148484));
#116817=CARTESIAN_POINT('Ctrl Pts',(-10.9412457556231,4.47782196265575,
11.7082576133397));
#116818=CARTESIAN_POINT('Ctrl Pts',(-10.927944522357,4.47920368773306,11.7255973219149));
#116819=CARTESIAN_POINT('Ctrl Pts',(-10.9021277648146,4.48177108055849,
11.7573805126361));
#116820=CARTESIAN_POINT('Ctrl Pts',(-10.8897285386905,4.48295910905912,
11.7719086110447));
#116821=CARTESIAN_POINT('Ctrl Pts',(-10.8454961928222,4.4870688672886,11.8212528486644));
#116822=CARTESIAN_POINT('Ctrl Pts',(-10.8119299571669,4.48996980502761,
11.8544528796232));
#116823=CARTESIAN_POINT('Ctrl Pts',(-10.7363094414386,4.4962542550023,11.9207580610405));
#116824=CARTESIAN_POINT('Ctrl Pts',(-10.6938119541341,4.49964460115605,
11.9531898578906));
#116825=CARTESIAN_POINT('Ctrl Pts',(-10.6395952408456,4.5039094313344,11.9890132974028));
#116826=CARTESIAN_POINT('Ctrl Pts',(-10.6298325274351,4.50467497751764,
11.9952589343325));
#116827=CARTESIAN_POINT('Ctrl Pts',(-10.61418628108,4.50589895765639,12.0049461186358));
#116828=CARTESIAN_POINT('Ctrl Pts',(-10.6083621375354,4.5063539377153,12.0084825211948));
#116829=CARTESIAN_POINT('Ctrl Pts',(-10.5973104458913,4.50721627887771,
12.0150625008954));
#116830=CARTESIAN_POINT('Ctrl Pts',(-10.5920894779881,4.50762323948006,
12.0181167404638));
#116831=CARTESIAN_POINT('Ctrl Pts',(-10.5802163198807,4.50854789850906,
12.0249402624885));
#116832=CARTESIAN_POINT('Ctrl Pts',(-10.5735505412796,4.50906643973288,
12.0286852246221));
#116833=CARTESIAN_POINT('Ctrl Pts',(-10.5531350602009,4.51065312716357,
12.0398949166697));
#116834=CARTESIAN_POINT('Ctrl Pts',(-10.5392731379948,4.51172849594223,
12.0471505500359));
#116835=CARTESIAN_POINT('Ctrl Pts',(-10.4472749848917,4.51885592383234,
12.0929931918995));
#116836=CARTESIAN_POINT('Ctrl Pts',(-10.3652196553214,4.52519829330641,
12.1230753603032));
#116837=CARTESIAN_POINT('Ctrl Pts',(-10.2153874672716,4.53652013414761,
12.1598336646745));
#116838=CARTESIAN_POINT('Ctrl Pts',(-10.1489025225625,4.54144974552421,
12.1702289855845));
#116839=CARTESIAN_POINT('Ctrl Pts',(-10.0741109404351,4.546676416282,12.1754417917166));
#116840=CARTESIAN_POINT('Ctrl Pts',(-10.0663285411522,4.54721636035049,
12.175906616167));
#116841=CARTESIAN_POINT('Ctrl Pts',(-10.0544679034948,4.54803272961443,
12.1764968967643));
#116842=CARTESIAN_POINT('Ctrl Pts',(-10.0503928586997,4.54831204362456,
12.1766784869538));
#116843=CARTESIAN_POINT('Ctrl Pts',(-10.0429333270717,4.54882109589726,
12.1769720719134));
#116844=CARTESIAN_POINT('Ctrl Pts',(-10.0395492715957,4.54905117556684,
12.1770906440683));
#116845=CARTESIAN_POINT('Ctrl Pts',(-10.0318750593658,4.54957103068973,
12.1773264036419));
#116846=CARTESIAN_POINT('Ctrl Pts',(-10.0275847348621,4.54986031971243,
12.1774347387318));
#116847=CARTESIAN_POINT('Ctrl Pts',(-10.0164101449972,4.55061053710988,
12.177655795767));
#116848=CARTESIAN_POINT('Ctrl Pts',(-10.009525198518,4.55106953834802,12.1777316087501));
#116849=CARTESIAN_POINT('Ctrl Pts',(-9.94811945672836,4.55513767886441,
12.1778692426881));
#116850=CARTESIAN_POINT('Ctrl Pts',(-9.89364873682566,4.55856777628396,
12.1742054967705));
#116851=CARTESIAN_POINT('Ctrl Pts',(-9.7699361677852,4.56633257232132,12.1572007205283));
#116852=CARTESIAN_POINT('Ctrl Pts',(-9.70125141872055,4.57063149165816,
12.141399093971));
#116853=CARTESIAN_POINT('Ctrl Pts',(-9.59787919830339,4.57751020548022,
12.107641160083));
#116854=CARTESIAN_POINT('Ctrl Pts',(-9.56197906516847,4.57997808144023,
12.0939411662865));
#116855=CARTESIAN_POINT('Ctrl Pts',(-9.51711045968681,4.58320071565414,
12.0742555816289));
#116856=CARTESIAN_POINT('Ctrl Pts',(-9.50746436613115,4.58390188078179,
12.0698672815768));
#116857=CARTESIAN_POINT('Ctrl Pts',(-9.49191018522385,4.58504678566279,
12.0625362790872));
#116858=CARTESIAN_POINT('Ctrl Pts',(-9.48596517053034,4.58548781757339,
12.0596729662286));
#116859=CARTESIAN_POINT('Ctrl Pts',(-9.47457148731538,4.58633985404428,
12.0540669560271));
#116860=CARTESIAN_POINT('Ctrl Pts',(-9.46911943692768,4.58675059584803,
12.0513315818908));
#116861=CARTESIAN_POINT('Ctrl Pts',(-9.4566358206962,4.5876981952847,12.0449465020946));
#116862=CARTESIAN_POINT('Ctrl Pts',(-9.44961940590022,4.58823603959938,
12.0412679866012));
#116863=CARTESIAN_POINT('Ctrl Pts',(-9.42712927411358,4.58997734158236,
12.0291862013365));
#116864=CARTESIAN_POINT('Ctrl Pts',(-9.41180735817389,4.59119037708787,
12.0205069641094));
#116865=CARTESIAN_POINT('Ctrl Pts',(-9.31483805942347,4.59904510937552,
11.9626685151572));
#116866=CARTESIAN_POINT('Ctrl Pts',(-9.23923100081285,4.6060341372894,11.9041026106128));
#116867=CARTESIAN_POINT('Ctrl Pts',(-9.14387898807866,4.61586835512337,
11.8097309595252));
#116868=CARTESIAN_POINT('Ctrl Pts',(-9.11760870544614,4.6187063855589,11.7810207417496));
#116869=CARTESIAN_POINT('Ctrl Pts',(-9.07970508688606,4.62295157698888,
11.7352376234035));
#116870=CARTESIAN_POINT('Ctrl Pts',(-9.06701971101092,4.6244012196619,11.7190723152465));
#116871=CARTESIAN_POINT('Ctrl Pts',(-9.05123709173938,4.62623486180655,
11.697838762465));
#116872=CARTESIAN_POINT('Ctrl Pts',(-9.04774697102238,4.62664234330034,
11.693068659624));
#116873=CARTESIAN_POINT('Ctrl Pts',(-9.04214729130931,4.627299126527,11.6852931707056));
#116874=CARTESIAN_POINT('Ctrl Pts',(-9.04001566983577,4.62754986567732,
11.6823039118573));
#116875=CARTESIAN_POINT('Ctrl Pts',(-9.03590562890243,4.62803465793218,
11.6764828442253));
#116876=CARTESIAN_POINT('Ctrl Pts',(-9.03392564509386,4.62826880932367,
11.6736522367678));
#116877=CARTESIAN_POINT('Ctrl Pts',(-9.02908276793474,4.62884312928643,
11.666663540382));
#116878=CARTESIAN_POINT('Ctrl Pts',(-9.02623405658253,4.62918236300633,
11.6624956130718));
#116879=CARTESIAN_POINT('Ctrl Pts',(-9.01804466287896,4.63016209846142,
11.6503468237788));
#116880=CARTESIAN_POINT('Ctrl Pts',(-9.01277453485048,4.63079827246414,
11.642318589494));
#116881=CARTESIAN_POINT('Ctrl Pts',(-8.97418231570867,4.6355072288593,11.5819319555626));
#116882=CARTESIAN_POINT('Ctrl Pts',(-8.94494293651263,4.63936527579464,
11.5270704846781));
#116883=CARTESIAN_POINT('Ctrl Pts',(-8.90398648983254,4.64571778886585,
11.4330026332319));
#116884=CARTESIAN_POINT('Ctrl Pts',(-8.88973941422442,4.64821553204775,
11.3950420761122));
#116885=CARTESIAN_POINT('Ctrl Pts',(-8.86111387621251,4.65412349941017,
11.3048886236862));
#116886=CARTESIAN_POINT('Ctrl Pts',(-8.84832068443017,4.65755435814954,
11.2522941351092));
#116887=CARTESIAN_POINT('Ctrl Pts',(-8.83722201608939,4.66186476759799,
11.1875566237165));
#116888=CARTESIAN_POINT('Ctrl Pts',(-8.83542793955184,4.66263241353258,
11.1760739256517));
#116889=CARTESIAN_POINT('Ctrl Pts',(-8.83285112336307,4.663858949278,11.1578134328437));
#116890=CARTESIAN_POINT('Ctrl Pts',(-8.83195681426822,4.66431435915672,
11.151051953945));
#116891=CARTESIAN_POINT('Ctrl Pts',(-8.8303804856278,4.66517701346931,11.1382816737736));
#116892=CARTESIAN_POINT('Ctrl Pts',(-8.82968591751854,4.66558385303865,
11.1322746223257));
#116893=CARTESIAN_POINT('Ctrl Pts',(-8.82821929078819,4.66650755023159,
11.1186730893941));
#116894=CARTESIAN_POINT('Ctrl Pts',(-8.82747475292135,4.66702524419319,
11.1110759778041));
#116895=CARTESIAN_POINT('Ctrl Pts',(-8.82543504329498,4.66860682553322,
11.0879492231059));
#116896=CARTESIAN_POINT('Ctrl Pts',(-8.82437423709542,4.6696778688018,11.0724011650262));
#116897=CARTESIAN_POINT('Ctrl Pts',(-8.81937287241452,4.67686336695797,
10.9688864273935));
#116898=CARTESIAN_POINT('Ctrl Pts',(-8.82500092438609,4.68327508990191,
10.8807518817124));
#116899=CARTESIAN_POINT('Ctrl Pts',(-8.84851253836293,4.69314412886784,
10.7483459189598));
#116900=CARTESIAN_POINT('Ctrl Pts',(-8.85933421271973,4.69655186893781,
10.7031242896483));
#116901=CARTESIAN_POINT('Ctrl Pts',(-8.87724568163762,4.70097950021217,
10.643975934462));
#116902=CARTESIAN_POINT('Ctrl Pts',(-8.8819784226795,4.70206934674861,10.6293813357934));
#116903=CARTESIAN_POINT('Ctrl Pts',(-8.89051312628796,4.703902207842,10.6047156935149));
#116904=CARTESIAN_POINT('Ctrl Pts',(-8.89417036398552,4.7046514808301,10.5945969383928));
#116905=CARTESIAN_POINT('Ctrl Pts',(-8.89960267635627,4.70571328342289,
10.5801877556245));
#116906=CARTESIAN_POINT('Ctrl Pts',(-8.90126512471728,4.70603182370425,
10.5758558428181));
#116907=CARTESIAN_POINT('Ctrl Pts',(-8.90419747552359,4.70658259929692,
10.568347838692));
#116908=CARTESIAN_POINT('Ctrl Pts',(-8.90545567738848,4.70681550383555,
10.5651672872587));
#116909=CARTESIAN_POINT('Ctrl Pts',(-8.90815927000994,4.70730873398822,
10.5584190914935));
#116910=CARTESIAN_POINT('Ctrl Pts',(-8.90960830924958,4.70756884278562,
10.5548530127831));
#116911=CARTESIAN_POINT('Ctrl Pts',(-8.91363440652476,4.70828019546412,
10.5450824301981));
#116912=CARTESIAN_POINT('Ctrl Pts',(-8.91624715859867,4.70872938789392,
10.5388926567701));
#116913=CARTESIAN_POINT('Ctrl Pts',(-8.92966213313801,4.71097603291763,
10.5078557521369));
#116914=CARTESIAN_POINT('Ctrl Pts',(-8.94126738929449,4.71273057957525,
10.4833621890808));
#116915=CARTESIAN_POINT('Ctrl Pts',(-8.9894891493147,4.71942446501789,10.3900517051512));
#116916=CARTESIAN_POINT('Ctrl Pts',(-9.0320561594786,4.72415706839001,10.3245331244351));
#116917=CARTESIAN_POINT('Ctrl Pts',(-9.11679481297087,4.73260498514031,
10.2187439545342));
#116918=CARTESIAN_POINT('Ctrl Pts',(-9.15604728247543,4.73624939421226,
10.1764983601737));
#116919=CARTESIAN_POINT('Ctrl Pts',(-9.2068599499617,4.74080021401076,10.1292745729884));
#116920=CARTESIAN_POINT('Ctrl Pts',(-9.2156108547363,4.74157833374439,10.1213831547994));
#116921=CARTESIAN_POINT('Ctrl Pts',(-9.22963773862795,4.74281774122112,
10.1091105321957));
#116922=CARTESIAN_POINT('Ctrl Pts',(-9.2348362589808,4.74327542031232,10.1046416897827));
#116923=CARTESIAN_POINT('Ctrl Pts',(-9.24468955974819,4.7441399884822,10.0963199074066));
#116924=CARTESIAN_POINT('Ctrl Pts',(-9.24933557250957,4.74454645161698,
10.0924568958592));
#116925=CARTESIAN_POINT('Ctrl Pts',(-9.25987627873562,4.74546606624515,
10.083828951764));
#116926=CARTESIAN_POINT('Ctrl Pts',(-9.26578761294311,4.74598002429814,
10.0790848690289));
#116927=CARTESIAN_POINT('Ctrl Pts',(-9.28337823068622,4.74750451204133,
10.0652447163958));
#116928=CARTESIAN_POINT('Ctrl Pts',(-9.29518331334793,4.7485213098117,10.0563117018003));
#116929=CARTESIAN_POINT('Ctrl Pts',(-9.3834523900869,4.75608169018832,9.9920979262408));
#116930=CARTESIAN_POINT('Ctrl Pts',(-9.4661318174951,4.76297386497827,9.94597173662926));
#116931=CARTESIAN_POINT('Ctrl Pts',(-9.6101393026443,4.77439150988871,9.88695777810674));
#116932=CARTESIAN_POINT('Ctrl Pts',(-9.66860898375979,4.7788729784233,9.86817136444711));
#116933=CARTESIAN_POINT('Ctrl Pts',(-9.73569462249501,4.78367708283696,
9.85226493786488));
#116934=CARTESIAN_POINT('Ctrl Pts',(-9.74312480958272,4.78420455164554,
9.85057916776584));
#116935=CARTESIAN_POINT('Ctrl Pts',(-9.75452125070296,4.78500600213383,
9.84810956128453));
#116936=CARTESIAN_POINT('Ctrl Pts',(-9.75847588529832,4.78528271894022,
9.84727388230923));
#116937=CARTESIAN_POINT('Ctrl Pts',(-9.76575371767529,4.78578931728173,
9.84577505485302));
#116938=CARTESIAN_POINT('Ctrl Pts',(-9.76907549402655,4.78601951768966,
9.84510588456476));
#116939=CARTESIAN_POINT('Ctrl Pts',(-9.77665547041992,4.78654251660726,
9.84361291387361));
#116940=CARTESIAN_POINT('Ctrl Pts',(-9.7809153732916,4.78683480244171,9.84279828911069));
#116941=CARTESIAN_POINT('Ctrl Pts',(-9.79381884848504,4.78771547281951,
9.84040455437087));
#116942=CARTESIAN_POINT('Ctrl Pts',(-9.80247590263699,4.78829998253793,
9.8388985804029));
#116943=CARTESIAN_POINT('Ctrl Pts',(-9.81114930150162,4.7888800033368,9.83748958018576));
#116944=CARTESIAN_POINT('Origin',(-10.,2.67563288526385,11.));
#116945=CARTESIAN_POINT('',(-9.81114929911337,5.38686993568377,9.83748958057373));
#116946=CARTESIAN_POINT('',(-9.81114934765212,5.28707251297004,9.83748957268858));
#116947=CARTESIAN_POINT('',(-9.81114930150157,2.67563288526385,9.83748958018577));
#116948=CARTESIAN_POINT('Ctrl Pts',(-9.81114929672518,5.38686993568377,
9.8374895809617));
#116949=CARTESIAN_POINT('Ctrl Pts',(-9.77383957756958,5.38451728128952,
9.84355057326433));
#116950=CARTESIAN_POINT('Ctrl Pts',(-9.73684185792727,5.38214351580701,
9.85140438837419));
#116951=CARTESIAN_POINT('Ctrl Pts',(-9.68265892178359,5.37855494172641,
9.86566237149448));
#116952=CARTESIAN_POINT('Ctrl Pts',(-9.66514465425574,5.37737732064956,
9.87070860271603));
#116953=CARTESIAN_POINT('Ctrl Pts',(-9.63416603170385,5.37525765284383,
9.88041821359246));
#116954=CARTESIAN_POINT('Ctrl Pts',(-9.62065574617396,5.37432056159209,
9.88492342077664));
#116955=CARTESIAN_POINT('Ctrl Pts',(-9.60028242012395,5.37288646857356,
9.89213031350666));
#116956=CARTESIAN_POINT('Ctrl Pts',(-9.5933572742663,5.37239528108828,9.89465341390828));
#116957=CARTESIAN_POINT('Ctrl Pts',(-9.58081112709059,5.37149839681785,
9.8993583225349));
#116958=CARTESIAN_POINT('Ctrl Pts',(-9.57518228935085,5.37109342009036,
9.90151862839889));
#116959=CARTESIAN_POINT('Ctrl Pts',(-9.56304360255536,5.37021434086383,
9.90628461888746));
#116960=CARTESIAN_POINT('Ctrl Pts',(-9.55653997020156,5.36973974969493,
9.9089053998624));
#116961=CARTESIAN_POINT('Ctrl Pts',(-9.53880849051417,5.36843573250735,
9.91623540783355));
#116962=CARTESIAN_POINT('Ctrl Pts',(-9.52762991922011,5.3676024614754,9.92106080469345));
#116963=CARTESIAN_POINT('Ctrl Pts',(-9.4507630739026,5.36179286740916,9.95566504243812));
#116964=CARTESIAN_POINT('Ctrl Pts',(-9.38786793819306,5.35661775705928,
9.99124449867526));
#116965=CARTESIAN_POINT('Ctrl Pts',(-9.28519044294973,5.34748274547146,
10.0624831964507));
#116966=CARTESIAN_POINT('Ctrl Pts',(-9.24382927970387,5.34358089192591,
10.095513198855));
#116967=CARTESIAN_POINT('Ctrl Pts',(-9.17813003333663,5.33711477866057,
10.155645442417));
#116968=CARTESIAN_POINT('Ctrl Pts',(-9.15257050671636,5.33452115345847,
10.1813006265899));
#116969=CARTESIAN_POINT('Ctrl Pts',(-9.12353971114573,5.33151833365936,
10.213259190026));
#116970=CARTESIAN_POINT('Ctrl Pts',(-9.118894346754,5.33103599336783,10.2184652447055));
#116971=CARTESIAN_POINT('Ctrl Pts',(-9.11172086145086,5.33028866210104,
10.2266498264172));
#116972=CARTESIAN_POINT('Ctrl Pts',(-9.10916092177233,5.33002146333288,
10.2296000669919));
#116973=CARTESIAN_POINT('Ctrl Pts',(-9.10439473139028,5.32952312032252,
10.2351484573874));
#116974=CARTESIAN_POINT('Ctrl Pts',(-9.1021850863348,5.32929174278562,10.2377434417703));
#116975=CARTESIAN_POINT('Ctrl Pts',(-9.09710806630722,5.32875926311865,
10.2437585464309));
#116976=CARTESIAN_POINT('Ctrl Pts',(-9.09424883040803,5.32845874102173,
10.2471854143134));
#116977=CARTESIAN_POINT('Ctrl Pts',(-9.08503193542932,5.32748757334217,
10.25836062885));
#116978=CARTESIAN_POINT('Ctrl Pts',(-9.07875348478723,5.3268222393217,10.2661741414961));
#116979=CARTESIAN_POINT('Ctrl Pts',(-9.02563801185253,5.32115109750923,
10.3340324882525));
#116980=CARTESIAN_POINT('Ctrl Pts',(-8.98462028609136,5.31647442145438,
10.3984176284241));
#116981=CARTESIAN_POINT('Ctrl Pts',(-8.91877512769588,5.30748431055952,
10.5279535045634));
#116982=CARTESIAN_POINT('Ctrl Pts',(-8.89293734698695,5.30319302654339,
10.5922181935774));
#116983=CARTESIAN_POINT('Ctrl Pts',(-8.86727296043656,5.29746484354759,
10.6768917709104));
#116984=CARTESIAN_POINT('Ctrl Pts',(-8.8621177354506,5.29619937239654,10.695544162278));
#116985=CARTESIAN_POINT('Ctrl Pts',(-8.85540876014022,5.29436959629865,
10.7223761298572));
#116986=CARTESIAN_POINT('Ctrl Pts',(-8.85347842193886,5.29381720877396,
10.7304589367145));
#116987=CARTESIAN_POINT('Ctrl Pts',(-8.85027082141928,5.2928519470735,10.744548282752));
#116988=CARTESIAN_POINT('Ctrl Pts',(-8.84895468459916,5.29244031800254,
10.7505457088158));
#116989=CARTESIAN_POINT('Ctrl Pts',(-8.8463412736594,5.29158964127037,10.7629158425951));
#116990=CARTESIAN_POINT('Ctrl Pts',(-8.84504976925513,5.29115042726968,
10.7692895404749));
#116991=CARTESIAN_POINT('Ctrl Pts',(-8.84187814143452,5.29002149604888,
10.7856362527082));
#116992=CARTESIAN_POINT('Ctrl Pts',(-8.84007405125164,5.28932942257549,
10.7956232946519));
#116993=CARTESIAN_POINT('Ctrl Pts',(-8.83335786323388,5.28653782764351,
10.8357612510318));
#116994=CARTESIAN_POINT('Ctrl Pts',(-8.82949097789187,5.2844063735152,10.866072490169));
#116995=CARTESIAN_POINT('Ctrl Pts',(-8.81876839943437,5.27576234468517,
10.9876121294635));
#116996=CARTESIAN_POINT('Ctrl Pts',(-8.82137296420124,5.26898842046517,
11.0793454637697));
#116997=CARTESIAN_POINT('Ctrl Pts',(-8.84023647551718,5.25944943377978,
11.2087901399952));
#116998=CARTESIAN_POINT('Ctrl Pts',(-8.84786332197083,5.25660940960404,
11.2474397824672));
#116999=CARTESIAN_POINT('Ctrl Pts',(-8.85969799244893,5.25319324378736,
11.2947798968669));
#117000=CARTESIAN_POINT('Ctrl Pts',(-8.86209306935238,5.25253849845545,
11.3038942038931));
#117001=CARTESIAN_POINT('Ctrl Pts',(-8.86576683691049,5.25158640962711,
11.3172216270186));
#117002=CARTESIAN_POINT('Ctrl Pts',(-8.86696009361955,5.25128459030296,
11.3214576193168));
#117003=CARTESIAN_POINT('Ctrl Pts',(-8.86911565861918,5.25075237509649,
11.3289486107772));
#117004=CARTESIAN_POINT('Ctrl Pts',(-8.87006832596017,5.2505214481757,11.3322062539182));
#117005=CARTESIAN_POINT('Ctrl Pts',(-8.87217340130492,5.25002039625304,
11.3392907263693));
#117006=CARTESIAN_POINT('Ctrl Pts',(-8.87333121314125,5.24975058201332,
11.3431158399504));
#117007=CARTESIAN_POINT('Ctrl Pts',(-8.87662789171236,5.24899802102508,
11.3538105900437));
#117008=CARTESIAN_POINT('Ctrl Pts',(-8.87881031257755,5.24851768048171,
11.3606667692848));
#117009=CARTESIAN_POINT('Ctrl Pts',(-8.89247986271362,5.24561223097657,
11.4022867816741));
#117010=CARTESIAN_POINT('Ctrl Pts',(-8.90552126588685,5.24326647971728,
11.4365230637684));
#117011=CARTESIAN_POINT('Ctrl Pts',(-8.96477539437933,5.23391228628043,
11.5726352900586));
#117012=CARTESIAN_POINT('Ctrl Pts',(-9.02378587616673,5.22721385814172,
11.6682876468));
#117013=CARTESIAN_POINT('Ctrl Pts',(-9.10837370719953,5.21867353291113,
11.7697454049295));
#117014=CARTESIAN_POINT('Ctrl Pts',(-9.12174453154593,5.21734998302817,
11.7849666796344));
#117015=CARTESIAN_POINT('Ctrl Pts',(-9.14124519040035,5.21545113474133,
11.8060439142007));
#117016=CARTESIAN_POINT('Ctrl Pts',(-9.14705637021043,5.21488905655065,
11.8121907244224));
#117017=CARTESIAN_POINT('Ctrl Pts',(-9.15721663689287,5.21391243778539,
11.8227085000909));
#117018=CARTESIAN_POINT('Ctrl Pts',(-9.16153482086476,5.21349922796665,
11.827108949397));
#117019=CARTESIAN_POINT('Ctrl Pts',(-9.16990125761127,5.21270206108784,
11.8355019250035));
#117020=CARTESIAN_POINT('Ctrl Pts',(-9.17394427235542,5.21231833910881,
11.8394994470958));
#117021=CARTESIAN_POINT('Ctrl Pts',(-9.18357072410076,5.21140811831416,
11.8488807088324));
#117022=CARTESIAN_POINT('Ctrl Pts',(-9.18917865489282,5.21088054100748,
11.8542388200649));
#117023=CARTESIAN_POINT('Ctrl Pts',(-9.20923034713505,5.20900320872296,
11.8730219148817));
#117024=CARTESIAN_POINT('Ctrl Pts',(-9.22395720347804,5.20764074116543,
11.8861384794655));
#117025=CARTESIAN_POINT('Ctrl Pts',(-9.32431559389986,5.19845718146427,
11.9711023166934));
#117026=CARTESIAN_POINT('Ctrl Pts',(-9.41946460329918,5.19014945770986,
12.0308047578809));
#117027=CARTESIAN_POINT('Ctrl Pts',(-9.55520952467588,5.17935550942639,
12.0911517606643));
#117028=CARTESIAN_POINT('Ctrl Pts',(-9.58954065153449,5.17671391924322,
12.1045245228352));
#117029=CARTESIAN_POINT('Ctrl Pts',(-9.63127260505924,5.17364879671387,
12.1185647318539));
#117030=CARTESIAN_POINT('Ctrl Pts',(-9.63812108617193,5.17315040410591,
12.1207990940866));
#117031=CARTESIAN_POINT('Ctrl Pts',(-9.64880220310638,5.17238070331368,
12.1241757676518));
#117032=CARTESIAN_POINT('Ctrl Pts',(-9.65262074405741,5.17210703527531,
12.125361587602));
#117033=CARTESIAN_POINT('Ctrl Pts',(-9.6596916007007,5.17160314818303,12.1275179707317));
#117034=CARTESIAN_POINT('Ctrl Pts',(-9.66294208077079,5.17137263762025,
12.1284939257797));
#117035=CARTESIAN_POINT('Ctrl Pts',(-9.6704145529168,5.17084526247733,12.1307023650096));
#117036=CARTESIAN_POINT('Ctrl Pts',(-9.67463927349406,5.17054894518587,
12.1319252644798));
#117037=CARTESIAN_POINT('Ctrl Pts',(-9.68792298917391,5.16962273422924,
12.1356898892993));
#117038=CARTESIAN_POINT('Ctrl Pts',(-9.6970059153899,5.16899742081043,12.1381468199288));
#117039=CARTESIAN_POINT('Ctrl Pts',(-9.74411778931241,5.16579055321982,
12.1502865935834));
#117040=CARTESIAN_POINT('Ctrl Pts',(-9.78258770476654,5.16329412667142,
12.1581742065285));
#117041=CARTESIAN_POINT('Ctrl Pts',(-9.91148474980412,5.15512027463574,
12.1779513966106));
#117042=CARTESIAN_POINT('Ctrl Pts',(-10.0028838238839,5.14960684017788,
12.1812690027037));
#117043=CARTESIAN_POINT('Ctrl Pts',(-10.1245626232589,5.14182845144815,
12.1715521982986));
#117044=CARTESIAN_POINT('Ctrl Pts',(-10.1552619548405,5.13983099362933,
12.1678800750543));
#117045=CARTESIAN_POINT('Ctrl Pts',(-10.1958429888563,5.13712553053322,
12.1613976258602));
#117046=CARTESIAN_POINT('Ctrl Pts',(-10.2058849732749,5.13645074394458,
12.1596595572523));
#117047=CARTESIAN_POINT('Ctrl Pts',(-10.2223048843288,5.13533807897131,
12.1565976014719));
#117048=CARTESIAN_POINT('Ctrl Pts',(-10.2286967597792,5.13490262297411,
12.1553507097474));
#117049=CARTESIAN_POINT('Ctrl Pts',(-10.2410903698406,5.13405361896181,
12.152826156166));
#117050=CARTESIAN_POINT('Ctrl Pts',(-10.2470931181834,5.13364027185536,
12.1515544716907));
#117051=CARTESIAN_POINT('Ctrl Pts',(-10.2611766109388,5.13266532025565,
12.1484556912962));
#117052=CARTESIAN_POINT('Ctrl Pts',(-10.2692484687094,5.13210251703561,
12.14659014168));
#117053=CARTESIAN_POINT('Ctrl Pts',(-10.295957548229,5.13022652122012,12.1401196140459));
#117054=CARTESIAN_POINT('Ctrl Pts',(-10.3145009823067,5.12890172417182,
12.1351443353065));
#117055=CARTESIAN_POINT('Ctrl Pts',(-10.3975680186762,5.12286231762431,
12.1106655352585));
#117056=CARTESIAN_POINT('Ctrl Pts',(-10.4604578121652,5.11799110665826,
12.0861005208796));
#117057=CARTESIAN_POINT('Ctrl Pts',(-10.5911172768324,5.1073212803377,12.0216682488829));
#117058=CARTESIAN_POINT('Ctrl Pts',(-10.6577175852677,5.10152431010428,
11.9801199295008));
#117059=CARTESIAN_POINT('Ctrl Pts',(-10.7274423234572,5.09535074712509,
11.9262927586026));
#117060=CARTESIAN_POINT('Ctrl Pts',(-10.7351053454085,5.0946709144487,11.920223209443));
#117061=CARTESIAN_POINT('Ctrl Pts',(-10.74617443561,5.09368800044318,11.9112293374319));
#117062=CARTESIAN_POINT('Ctrl Pts',(-10.7496405323456,5.09338008553982,
11.9083800238188));
#117063=CARTESIAN_POINT('Ctrl Pts',(-10.7557130946631,5.09284051450154,
11.9033296286212));
#117064=CARTESIAN_POINT('Ctrl Pts',(-10.7583264006519,5.09260828128118,
11.9011369322361));
#117065=CARTESIAN_POINT('Ctrl Pts',(-10.7639005616079,5.09211289672363,
11.8964185066615));
#117066=CARTESIAN_POINT('Ctrl Pts',(-10.7668584546817,5.09184998963851,
11.893889433146));
#117067=CARTESIAN_POINT('Ctrl Pts',(-10.7750339078488,5.09112305548,11.8868287663237));
#117068=CARTESIAN_POINT('Ctrl Pts',(-10.7802243031159,5.09066123072138,
11.8822657545132));
#117069=CARTESIAN_POINT('Ctrl Pts',(-10.8113039855021,5.0878918012946,11.8544539996888));
#117070=CARTESIAN_POINT('Ctrl Pts',(-10.8361953765718,5.08565643491603,
11.8301105920734));
#117071=CARTESIAN_POINT('Ctrl Pts',(-10.9163563298724,5.07824582340873,
11.7444432170743));
#117072=CARTESIAN_POINT('Ctrl Pts',(-10.966250790811,5.07324847894144,11.6784284628813));
#117073=CARTESIAN_POINT('Ctrl Pts',(-11.0323191741656,5.06520506690983,
11.5687558494935));
#117074=CARTESIAN_POINT('Ctrl Pts',(-11.0535207903303,5.06229974692301,
11.5284499246184));
#117075=CARTESIAN_POINT('Ctrl Pts',(-11.0770875526717,5.05855865942498,
11.476560057148));
#117076=CARTESIAN_POINT('Ctrl Pts',(-11.0816854199365,5.05779954922199,
11.4660297429387));
#117077=CARTESIAN_POINT('Ctrl Pts',(-11.0887552740787,5.05658341400903,
11.4491694147342));
#117078=CARTESIAN_POINT('Ctrl Pts',(-11.0913278928781,5.05612976466467,
11.4428821930669));
#117079=CARTESIAN_POINT('Ctrl Pts',(-11.0958654931348,5.05530899895008,
11.4315131125838));
#117080=CARTESIAN_POINT('Ctrl Pts',(-11.0978498886201,5.05494254094094,
11.4264391700164));
#117081=CARTESIAN_POINT('Ctrl Pts',(-11.1024407955994,5.0540766205341,11.4144561291335));
#117082=CARTESIAN_POINT('Ctrl Pts',(-11.1050176481486,5.0535761955108,11.4075359907606));
#117083=CARTESIAN_POINT('Ctrl Pts',(-11.1123965078601,5.05209963592151,
11.3871354378024));
#117084=CARTESIAN_POINT('Ctrl Pts',(-11.1170179558219,5.05111767257959,
11.3735916126547));
#117085=CARTESIAN_POINT('Ctrl Pts',(-11.1368686147346,5.04662464344426,
11.3117516970751));
#117086=CARTESIAN_POINT('Ctrl Pts',(-11.1492181346826,5.04302380785564,
11.2625944156849));
#117087=CARTESIAN_POINT('Ctrl Pts',(-11.1724229198635,5.0337217525597,11.1362808312511));
#117088=CARTESIAN_POINT('Ctrl Pts',(-11.1788629978936,5.02794353485431,
11.058560484151));
#117089=CARTESIAN_POINT('Ctrl Pts',(-11.1771109855138,5.02019302164646,
10.95124557561));
#117090=CARTESIAN_POINT('Ctrl Pts',(-11.1755183098171,5.0180881803883,10.9217421322267));
#117091=CARTESIAN_POINT('Ctrl Pts',(-11.1721959031427,5.01556141155346,
10.8855530531357));
#117092=CARTESIAN_POINT('Ctrl Pts',(-11.1715152869319,5.01509119052823,
10.8787841720338));
#117093=CARTESIAN_POINT('Ctrl Pts',(-11.1703513971733,5.01435568545808,
10.8681366580499));
#117094=CARTESIAN_POINT('Ctrl Pts',(-11.1699074157735,5.0140883535152,10.8642540112942));
#117095=CARTESIAN_POINT('Ctrl Pts',(-11.1690806298808,5.01361320484443,
10.8573292483185));
#117096=CARTESIAN_POINT('Ctrl Pts',(-11.1687052719952,5.0134049926363,10.8542864108302));
#117097=CARTESIAN_POINT('Ctrl Pts',(-11.167770037172,5.01290372551258,10.8469411018433));
#117098=CARTESIAN_POINT('Ctrl Pts',(-11.1671982631466,5.01261133081293,
10.842640214722));
#117099=CARTESIAN_POINT('Ctrl Pts',(-11.1653543158997,5.01170983696046,
10.8293333536938));
#117100=CARTESIAN_POINT('Ctrl Pts',(-11.1640015424532,5.01110497722067,
10.8203386314895));
#117101=CARTESIAN_POINT('Ctrl Pts',(-11.1514904161216,5.00595181152115,
10.7432353949822));
#117102=CARTESIAN_POINT('Ctrl Pts',(-11.1344677578868,5.00168011800253,
10.6762039996229));
#117103=CARTESIAN_POINT('Ctrl Pts',(-11.0843042130208,4.99228203334683,
10.5328331340842));
#117104=CARTESIAN_POINT('Ctrl Pts',(-11.0487669327679,4.98717073271439,
10.4577395044924));
#117105=CARTESIAN_POINT('Ctrl Pts',(-10.9973871434363,4.98074389667977,
10.3734492959406));
#117106=CARTESIAN_POINT('Ctrl Pts',(-10.9888547086039,4.97970184073197,
10.3600677964907));
#117107=CARTESIAN_POINT('Ctrl Pts',(-10.9757905009485,4.97814028266468,
10.3404644894427));
#117108=CARTESIAN_POINT('Ctrl Pts',(-10.9714636917894,4.97762831546317,
10.3341077547538));
#117109=CARTESIAN_POINT('Ctrl Pts',(-10.9636195088911,4.97670908900929,
10.3228226530725));
#117110=CARTESIAN_POINT('Ctrl Pts',(-10.9601257621239,4.97630272654266,
10.3178781372223));
#117111=CARTESIAN_POINT('Ctrl Pts',(-10.952633409262,4.97543756494151,10.3074462126003));
#117112=CARTESIAN_POINT('Ctrl Pts',(-10.9486251765066,4.97497840917501,
10.3019660237129));
#117113=CARTESIAN_POINT('Ctrl Pts',(-10.9377167239613,4.9737384173116,10.2873191132736));
#117114=CARTESIAN_POINT('Ctrl Pts',(-10.9307297150587,4.97295425980651,
10.2782182587006));
#117115=CARTESIAN_POINT('Ctrl Pts',(-10.8918682053794,4.96864537509792,
10.2291022733612));
#117116=CARTESIAN_POINT('Ctrl Pts',(-10.8575496183533,4.96502459233316,
10.1910997863715));
#117117=CARTESIAN_POINT('Ctrl Pts',(-10.7708038815786,4.95628839840166,
10.1067856336749));
#117118=CARTESIAN_POINT('Ctrl Pts',(-10.7165060587857,4.95112187008965,
10.0626693950568));
#117119=CARTESIAN_POINT('Ctrl Pts',(-10.643428359353,4.94469951640419,10.0133738950112));
#117120=CARTESIAN_POINT('Ctrl Pts',(-10.6279929546477,4.94337093645498,
10.0034780364284));
#117121=CARTESIAN_POINT('Ctrl Pts',(-10.5915767333335,4.94030984370705,
9.98131338874795));
#117122=CARTESIAN_POINT('Ctrl Pts',(-10.5704334501427,4.93858717391493,
9.96932482500798));
#117123=CARTESIAN_POINT('Ctrl Pts',(-10.5431961669236,4.93644936836165,
9.95497606352385));
#117124=CARTESIAN_POINT('Ctrl Pts',(-10.5374345746495,4.93600165472439,
9.95200134240666));
#117125=CARTESIAN_POINT('Ctrl Pts',(-10.528259102095,4.93529611153656,9.94735959986447));
#117126=CARTESIAN_POINT('Ctrl Pts',(-10.5248613204555,4.93503644661463,
9.94566130381987));
#117127=CARTESIAN_POINT('Ctrl Pts',(-10.5183733769119,4.93454376041603,
9.94245760416173));
#117128=CARTESIAN_POINT('Ctrl Pts',(-10.5152848539088,4.93431057640804,
9.94094929464511));
#117129=CARTESIAN_POINT('Ctrl Pts',(-10.5079140699309,4.93375721855073,
9.93738958005762));
#117130=CARTESIAN_POINT('Ctrl Pts',(-10.5036259356046,4.93343779209456,
9.93535051499438));
#117131=CARTESIAN_POINT('Ctrl Pts',(-10.4890041787416,4.93235669773757,
9.92850578643829));
#117132=CARTESIAN_POINT('Ctrl Pts',(-10.4786128071935,4.93160205575712,
9.92382401955124));
#117133=CARTESIAN_POINT('Ctrl Pts',(-10.4529516563136,4.92976788168413,
9.91270778364184));
#117134=CARTESIAN_POINT('Ctrl Pts',(-10.4376105871074,4.9286964957058,9.90644314390221));
#117135=CARTESIAN_POINT('Ctrl Pts',(-10.3723904892332,4.92422629048837,
9.8814024700492));
#117136=CARTESIAN_POINT('Ctrl Pts',(-10.3213964288365,4.92093495731556,
9.86569832859299));
#117137=CARTESIAN_POINT('Ctrl Pts',(-10.1932275076868,4.91279051138116,
9.83556928329505));
#117138=CARTESIAN_POINT('Ctrl Pts',(-10.1153543503117,4.90794033421488,
9.82529695337106));
#117139=CARTESIAN_POINT('Ctrl Pts',(-10.021025004204,4.901797638359,9.82232864202871));
#117140=CARTESIAN_POINT('Ctrl Pts',(-10.0049995052522,4.90074553332221,
9.82215160432838));
#117141=CARTESIAN_POINT('Ctrl Pts',(-9.98125717062269,4.89917182107703,
9.8223738478858));
#117142=CARTESIAN_POINT('Ctrl Pts',(-9.97353941221862,4.89865792473856,
9.82252198306959));
#117143=CARTESIAN_POINT('Ctrl Pts',(-9.95976890387531,4.8977365666231,9.82292174674305));
#117144=CARTESIAN_POINT('Ctrl Pts',(-9.95371553428081,4.89733001803941,
9.8231442308925));
#117145=CARTESIAN_POINT('Ctrl Pts',(-9.9408987645737,4.89646586980267,9.82371433369115));
#117146=CARTESIAN_POINT('Ctrl Pts',(-9.9341361301628,4.89600792426916,9.82407361108874));
#117147=CARTESIAN_POINT('Ctrl Pts',(-9.91600589500242,4.89477468058692,
9.82519369663301));
#117148=CARTESIAN_POINT('Ctrl Pts',(-9.90464585239356,4.89399612332243,
9.82606114689032));
#117149=CARTESIAN_POINT('Ctrl Pts',(-9.86579458385425,4.8913126402476,9.82959545185898));
#117150=CARTESIAN_POINT('Ctrl Pts',(-9.8383940495945,4.88938401548889,9.8330636497039));
#117151=CARTESIAN_POINT('Ctrl Pts',(-9.81114928023156,4.88742944622416,
9.8374895836411));
#117152=CARTESIAN_POINT('Ctrl Pts',(-9.81114930150162,4.7888800033368,9.83748958018576));
#117153=CARTESIAN_POINT('Ctrl Pts',(-9.81144932862408,4.78890006720957,
9.8374408405524));
#117154=CARTESIAN_POINT('Ctrl Pts',(-9.81174937530434,4.78892012571072,
9.83739221695604));
#117155=CARTESIAN_POINT('Ctrl Pts',(-9.87979352543049,4.79346745574619,
9.82639246051551));
#117156=CARTESIAN_POINT('Ctrl Pts',(-9.94837521288134,4.79771647491303,
9.82138140135665));
#117157=CARTESIAN_POINT('Ctrl Pts',(-10.1002918206641,4.80711738079732,
9.82357586222741));
#117158=CARTESIAN_POINT('Ctrl Pts',(-10.1832000021336,4.81225366063202,
9.83360899739349));
#117159=CARTESIAN_POINT('Ctrl Pts',(-10.2797977998483,4.81870752550248,
9.85585863549241));
#117160=CARTESIAN_POINT('Ctrl Pts',(-10.2951689211226,4.81974830798736,
9.85972742728444));
#117161=CARTESIAN_POINT('Ctrl Pts',(-10.3178694174919,4.82130824038348,
9.86593071323048));
#117162=CARTESIAN_POINT('Ctrl Pts',(-10.3252619589583,4.82181987677813,
9.86802881346254));
#117163=CARTESIAN_POINT('Ctrl Pts',(-10.3384391827347,4.82273863779968,
9.87190842024684));
#117164=CARTESIAN_POINT('Ctrl Pts',(-10.3442317128404,4.82314486774321,
9.87366247586994));
#117165=CARTESIAN_POINT('Ctrl Pts',(-10.356492972385,4.82400988232411,9.87747876710599));
#117166=CARTESIAN_POINT('Ctrl Pts',(-10.362957881295,4.82446902443469,9.87955244177456));
#117167=CARTESIAN_POINT('Ctrl Pts',(-10.380303027397,4.82570931001288,9.88528191426843));
#117168=CARTESIAN_POINT('Ctrl Pts',(-10.3911481127463,4.82649377901595,
9.88904098138364));
#117169=CARTESIAN_POINT('Ctrl Pts',(-10.4501353397126,4.83081124885458,
9.91045760202083));
#117170=CARTESIAN_POINT('Ctrl Pts',(-10.4971333857008,4.8344407822134,9.93108393590812));
#117171=CARTESIAN_POINT('Ctrl Pts',(-10.6055015085322,4.84325937306923,
9.98733985229364));
#117172=CARTESIAN_POINT('Ctrl Pts',(-10.6652961909556,4.84850285222669,
10.0255808468813));
#117173=CARTESIAN_POINT('Ctrl Pts',(-10.7527856428889,4.85656082267927,
10.0933598301527));
#117174=CARTESIAN_POINT('Ctrl Pts',(-10.7830284947511,4.85942679321481,
10.1193470126605));
#117175=CARTESIAN_POINT('Ctrl Pts',(-10.8172064231,4.8627123686331,10.1518712285529));
#117176=CARTESIAN_POINT('Ctrl Pts',(-10.8224673008177,4.86321947546268,
10.1569719478138));
#117177=CARTESIAN_POINT('Ctrl Pts',(-10.8305440844558,4.86399967934948,
10.1649504270405));
#117178=CARTESIAN_POINT('Ctrl Pts',(-10.8333933065157,4.86427523681034,
10.1677939777956));
#117179=CARTESIAN_POINT('Ctrl Pts',(-10.83861509026,4.86478076286787,10.1730590802628));
#117180=CARTESIAN_POINT('Ctrl Pts',(-10.8409917872438,4.86501104019017,
10.1754762776879));
#117181=CARTESIAN_POINT('Ctrl Pts',(-10.8464003797232,4.86553554323703,
10.1810247528577));
#117182=CARTESIAN_POINT('Ctrl Pts',(-10.8494253608081,4.86582924395821,
10.1841626288553));
#117183=CARTESIAN_POINT('Ctrl Pts',(-10.8587831138173,4.86673918113316,
10.1939780913136));
#117184=CARTESIAN_POINT('Ctrl Pts',(-10.8650552679232,4.86735106214369,
10.2007133492027));
#117185=CARTESIAN_POINT('Ctrl Pts',(-10.8796505764579,4.86878163612467,
10.2167593836701));
#117186=CARTESIAN_POINT('Ctrl Pts',(-10.8879060028588,4.86959612322724,
10.2261305300146));
#117187=CARTESIAN_POINT('Ctrl Pts',(-10.9174926071089,4.87254258411477,
10.2608126646368));
#117188=CARTESIAN_POINT('Ctrl Pts',(-10.9379045773303,4.87462933624073,
10.2868899677504));
#117189=CARTESIAN_POINT('Ctrl Pts',(-11.0020586212681,4.88150099022316,
10.3763787963712));
#117190=CARTESIAN_POINT('Ctrl Pts',(-11.0406780308878,4.88618878943377,
10.443210898045));
#117191=CARTESIAN_POINT('Ctrl Pts',(-11.0879880207593,4.89343246841507,
10.547471116482));
#117192=CARTESIAN_POINT('Ctrl Pts',(-11.1018381841972,4.89584096618305,
10.5823248770731));
#117193=CARTESIAN_POINT('Ctrl Pts',(-11.1175547335366,4.8990236667496,10.6281313287243));
#117194=CARTESIAN_POINT('Ctrl Pts',(-11.1209626835328,4.89974751920242,
10.638534178552));
#117195=CARTESIAN_POINT('Ctrl Pts',(-11.1262142547077,4.90092026852565,
10.6553537157111));
#117196=CARTESIAN_POINT('Ctrl Pts',(-11.1281492390682,4.90136620292018,
10.6617413710231));
#117197=CARTESIAN_POINT('Ctrl Pts',(-11.1317421650146,4.9022215415435,10.6739759722585));
#117198=CARTESIAN_POINT('Ctrl Pts',(-11.1334093513402,4.90263063272673,
10.679819996474));
#117199=CARTESIAN_POINT('Ctrl Pts',(-11.1371385024988,4.90357461764932,
10.6932860716369));
#117200=CARTESIAN_POINT('Ctrl Pts',(-11.1391691742857,4.90411049264994,
10.7009164083062));
#117201=CARTESIAN_POINT('Ctrl Pts',(-11.1453255622494,4.90580682045551,
10.7250220575759));
#117202=CARTESIAN_POINT('Ctrl Pts',(-11.1491715564009,4.90697603268181,
10.7415658801416));
#117203=CARTESIAN_POINT('Ctrl Pts',(-11.157362473948,4.90974853018851,10.7806097042691));
#117204=CARTESIAN_POINT('Ctrl Pts',(-11.1614110106253,4.91136031355026,
10.8031641725468));
#117205=CARTESIAN_POINT('Ctrl Pts',(-11.1821491163321,4.92133230655422,
10.9418476099529));
#117206=CARTESIAN_POINT('Ctrl Pts',(-11.1820646756277,4.93016371082831,
11.0597933233473));
#117207=CARTESIAN_POINT('Ctrl Pts',(-11.1621508531987,4.93963510711482,
11.1917316485292));
#117208=CARTESIAN_POINT('Ctrl Pts',(-11.1594137199758,4.94076881184951,
11.2076427701734));
#117209=CARTESIAN_POINT('Ctrl Pts',(-11.1552858047043,4.9422748055171,11.2290005059576));
#117210=CARTESIAN_POINT('Ctrl Pts',(-11.154182089105,4.94266116510058,11.2344999586727));
#117211=CARTESIAN_POINT('Ctrl Pts',(-11.1523773693867,4.94326785470465,
11.2431707358121));
#117212=CARTESIAN_POINT('Ctrl Pts',(-11.1517024823791,4.94348959354747,
11.2463473177439));
#117213=CARTESIAN_POINT('Ctrl Pts',(-11.1502780647939,4.9439471109822,11.252918005051));
#117214=CARTESIAN_POINT('Ctrl Pts',(-11.1495266383952,4.94418276733786,
11.256311629842));
#117215=CARTESIAN_POINT('Ctrl Pts',(-11.147662502225,4.94475389923947,11.2645574120348));
#117216=CARTESIAN_POINT('Ctrl Pts',(-11.1465340150007,4.94508849824611,
11.2694060094633));
#117217=CARTESIAN_POINT('Ctrl Pts',(-11.1423803664345,4.94628169261917,
11.2867534269149));
#117218=CARTESIAN_POINT('Ctrl Pts',(-11.1391811643632,4.94713114765455,
11.2992101893408));
#117219=CARTESIAN_POINT('Ctrl Pts',(-11.1306122721246,4.94924815403828,
11.3304424333679));
#117220=CARTESIAN_POINT('Ctrl Pts',(-11.1249783667895,4.95050391164761,
11.3491419091925));
#117221=CARTESIAN_POINT('Ctrl Pts',(-11.0957182786318,4.9564643460093,11.4381795583914));
#117222=CARTESIAN_POINT('Ctrl Pts',(-11.0659448820378,4.9609782572752,11.5063227975903));
#117223=CARTESIAN_POINT('Ctrl Pts',(-11.0014069483683,4.96926347345763,
11.6226909354701));
#117224=CARTESIAN_POINT('Ctrl Pts',(-10.969043038991,4.97298203542559,11.6719480227077));
#117225=CARTESIAN_POINT('Ctrl Pts',(-10.9257990598139,4.97762813165029,
11.7281042364935));
#117226=CARTESIAN_POINT('Ctrl Pts',(-10.918316634404,4.97842171905366,11.7375189624746));
#117227=CARTESIAN_POINT('Ctrl Pts',(-10.9062673894164,4.97968466313244,
11.7522121779879));
#117228=CARTESIAN_POINT('Ctrl Pts',(-10.9017954313233,4.98015025380448,
11.7575676460588));
#117229=CARTESIAN_POINT('Ctrl Pts',(-10.8933705461015,4.98102179760876,
11.7674767010294));
#117230=CARTESIAN_POINT('Ctrl Pts',(-10.8894297029852,4.98142725264809,
11.772040297134));
#117231=CARTESIAN_POINT('Ctrl Pts',(-10.8805684279968,4.98233416891385,
11.7821439811619));
#117232=CARTESIAN_POINT('Ctrl Pts',(-10.8756304418856,4.9828363429974,11.7876682604741));
#117233=CARTESIAN_POINT('Ctrl Pts',(-10.8609150918387,4.98432372865178,
11.8038213924484));
#117234=CARTESIAN_POINT('Ctrl Pts',(-10.8509942814216,4.98531490113986,
11.8143170925434));
#117235=CARTESIAN_POINT('Ctrl Pts',(-10.8047467521311,4.9898853766641,11.8614763078938));
#117236=CARTESIAN_POINT('Ctrl Pts',(-10.766232001747,4.99355809055028,11.8959051280465));
#117237=CARTESIAN_POINT('Ctrl Pts',(-10.6581227140113,5.00350656235326,
11.9804619640586));
#117238=CARTESIAN_POINT('Ctrl Pts',(-10.5851050780729,5.0098866441019,12.0257108633622));
#117239=CARTESIAN_POINT('Ctrl Pts',(-10.4883149290882,5.01756422992387,
12.0719660855871));
#117240=CARTESIAN_POINT('Ctrl Pts',(-10.4685476512781,5.01909325947478,
12.0807525149932));
#117241=CARTESIAN_POINT('Ctrl Pts',(-10.4427425821387,5.02102995744698,
12.0913814602302));
#117242=CARTESIAN_POINT('Ctrl Pts',(-10.4369177896574,5.02146327774358,
12.0937263529831));
#117243=CARTESIAN_POINT('Ctrl Pts',(-10.4275820842982,5.02215136190298,
12.097398153048));
#117244=CARTESIAN_POINT('Ctrl Pts',(-10.42408319784,5.02240781473686,12.0987550170217));
#117245=CARTESIAN_POINT('Ctrl Pts',(-10.4173522155762,5.02289834180884,
12.1013283415712));
#117246=CARTESIAN_POINT('Ctrl Pts',(-10.4141211971399,5.0231325529114,12.1025473333035));
#117247=CARTESIAN_POINT('Ctrl Pts',(-10.4063383799733,5.02369379941877,
12.1054445793754));
#117248=CARTESIAN_POINT('Ctrl Pts',(-10.4017814220648,5.0240200323881,12.1071089774942));
#117249=CARTESIAN_POINT('Ctrl Pts',(-10.3858808034036,5.02515050371265,
12.1128054636253));
#117250=CARTESIAN_POINT('Ctrl Pts',(-10.3744852661921,5.02594682005417,
12.1166919034619));
#117251=CARTESIAN_POINT('Ctrl Pts',(-10.3460569593042,5.02790384169957,
12.125903207728));
#117252=CARTESIAN_POINT('Ctrl Pts',(-10.3289585779317,5.02905490768233,
12.1310171418321));
#117253=CARTESIAN_POINT('Ctrl Pts',(-10.2525568352456,5.0341105212969,12.1519886697963));
#117254=CARTESIAN_POINT('Ctrl Pts',(-10.1921802164538,5.03787731623307,
12.163585268697));
#117255=CARTESIAN_POINT('Ctrl Pts',(-10.0573999606523,5.04627537022066,
12.1786903139196));
#117256=CARTESIAN_POINT('Ctrl Pts',(-9.98302252080802,5.05091028382481,
12.1799641068196));
#117257=CARTESIAN_POINT('Ctrl Pts',(-9.89689790122508,5.05657119578408,
12.1732915131266));
#117258=CARTESIAN_POINT('Ctrl Pts',(-9.88478623426478,5.05737372187899,
12.1721641471339));
#117259=CARTESIAN_POINT('Ctrl Pts',(-9.86572757957192,5.05864773187734,
12.1700919161389));
#117260=CARTESIAN_POINT('Ctrl Pts',(-9.85876763198313,5.05911533660402,
12.1692722479207));
#117261=CARTESIAN_POINT('Ctrl Pts',(-9.84583586902019,5.05998873285216,
12.1676321401961));
#117262=CARTESIAN_POINT('Ctrl Pts',(-9.83986220692685,5.06039400826612,
12.166827870347));
#117263=CARTESIAN_POINT('Ctrl Pts',(-9.82659820482548,5.06129806405785,
12.1649382837008));
#117264=CARTESIAN_POINT('Ctrl Pts',(-9.81931140046457,5.06179753574432,
12.1638303197332));
#117265=CARTESIAN_POINT('Ctrl Pts',(-9.79797055448183,5.06326884926167,
12.1603801799919));
#117266=CARTESIAN_POINT('Ctrl Pts',(-9.78394847409247,5.06424645893532,
12.1578513576034));
#117267=CARTESIAN_POINT('Ctrl Pts',(-9.75209015237582,5.06649340875057,
12.1515069990639));
#117268=CARTESIAN_POINT('Ctrl Pts',(-9.73429010466333,5.06776747537856,
12.1475303267562));
#117269=CARTESIAN_POINT('Ctrl Pts',(-9.67377854526126,5.07216343541959,
12.1325282040226));
#117270=CARTESIAN_POINT('Ctrl Pts',(-9.63160095718511,5.0753406116986,12.1195186564465));
#117271=CARTESIAN_POINT('Ctrl Pts',(-9.53081786635906,5.0831771684397,12.0821194726807));
#117272=CARTESIAN_POINT('Ctrl Pts',(-9.47325869471765,5.08786790493696,
12.0552999620151));
#117273=CARTESIAN_POINT('Ctrl Pts',(-9.39029099118561,5.09477489144795,
12.0081546628066));
#117274=CARTESIAN_POINT('Ctrl Pts',(-9.36309832723165,5.09706291933443,
11.9912000598176));
#117275=CARTESIAN_POINT('Ctrl Pts',(-9.33088577087955,5.09977472546562,
11.969241720141));
#117276=CARTESIAN_POINT('Ctrl Pts',(-9.32517776176575,5.10025529421663,
11.9652762901257));
#117277=CARTESIAN_POINT('Ctrl Pts',(-9.31628875887191,5.10100333012165,
11.958983591966));
#117278=CARTESIAN_POINT('Ctrl Pts',(-9.31308388507036,5.10127295797896,
11.9566905681032));
#117279=CARTESIAN_POINT('Ctrl Pts',(-9.3074111418512,5.1017499945713,11.9525886298054));
#117280=CARTESIAN_POINT('Ctrl Pts',(-9.30493880180195,5.10195781946971,
11.9507861774204));
#117281=CARTESIAN_POINT('Ctrl Pts',(-9.29901806473303,5.10245535453567,
11.946434244425));
#117282=CARTESIAN_POINT('Ctrl Pts',(-9.2955765354794,5.10274443175343,11.9438755408784));
#117283=CARTESIAN_POINT('Ctrl Pts',(-9.28508481208236,5.10362558463302,
11.9359858219779));
#117284=CARTESIAN_POINT('Ctrl Pts',(-9.27808039726865,5.10421369035769,
11.9305940487124));
#117285=CARTESIAN_POINT('Ctrl Pts',(-9.26183025330577,5.10557945297592,
11.9177912995013));
#117286=CARTESIAN_POINT('Ctrl Pts',(-9.25263420333359,5.10635340479528,
11.91031853412));
#117287=CARTESIAN_POINT('Ctrl Pts',(-9.22018359223284,5.1090947154251,11.8831256909381));
#117288=CARTESIAN_POINT('Ctrl Pts',(-9.19758258635908,5.1110233009323,11.8626419706338));
#117289=CARTESIAN_POINT('Ctrl Pts',(-9.12323633130206,5.11753581749449,
11.7898071545867));
#117290=CARTESIAN_POINT('Ctrl Pts',(-9.07561409503207,5.12201543991753,
11.7334990380201));
#117291=CARTESIAN_POINT('Ctrl Pts',(-9.02700070388263,5.12736615091861,
11.663701011924));
#117292=CARTESIAN_POINT('Ctrl Pts',(-9.02058231813385,5.12809084004091,
11.6541923708683));
#117293=CARTESIAN_POINT('Ctrl Pts',(-8.99567284534512,5.13098094313283,
11.6161013286426));
#117294=CARTESIAN_POINT('Ctrl Pts',(-8.9782872071473,5.13317482428793,11.5868189808562));
#117295=CARTESIAN_POINT('Ctrl Pts',(-8.95721371552045,5.13610686600386,
11.5475425459004));
#117296=CARTESIAN_POINT('Ctrl Pts',(-8.95235725327569,5.13680407222857,
11.5381921015038));
#117297=CARTESIAN_POINT('Ctrl Pts',(-8.94467032610381,5.13794412294475,
11.5228935935638));
#117298=CARTESIAN_POINT('Ctrl Pts',(-8.94176309013027,5.13838430311074,
11.5169845939778));
#117299=CARTESIAN_POINT('Ctrl Pts',(-8.93625680252158,5.13923581030615,
11.5055519116172));
#117300=CARTESIAN_POINT('Ctrl Pts',(-8.9336508349475,5.13964688358976,11.5000317802965));
#117301=CARTESIAN_POINT('Ctrl Pts',(-8.92769111895437,5.14060621311621,
11.4871490323272));
#117302=CARTESIAN_POINT('Ctrl Pts',(-8.92437012322664,5.14115555906681,
11.4797716942523));
#117303=CARTESIAN_POINT('Ctrl Pts',(-8.91387745058903,5.14294040364245,
11.4558063794001));
#117304=CARTESIAN_POINT('Ctrl Pts',(-8.90701178677612,5.14418601258378,
11.4390880903001));
#117305=CARTESIAN_POINT('Ctrl Pts',(-8.87110137843636,5.15115965402037,
11.3455767637822));
#117306=CARTESIAN_POINT('Ctrl Pts',(-8.84976835999797,5.15713527881844,
11.2660793067991));
#117307=CARTESIAN_POINT('Ctrl Pts',(-8.82678129329819,5.16787317661145,
11.1215757976017));
#117308=CARTESIAN_POINT('Ctrl Pts',(-8.82189578655519,5.17259252077701,
11.0574005079799));
#117309=CARTESIAN_POINT('Ctrl Pts',(-8.82232554485016,5.17777320283397,
10.9835975661307));
#117310=CARTESIAN_POINT('Ctrl Pts',(-8.82249714680485,5.17843827158686,
10.9740537669406));
#117311=CARTESIAN_POINT('Ctrl Pts',(-8.8229364202516,5.17944526863039,10.9594817912362));
#117312=CARTESIAN_POINT('Ctrl Pts',(-8.82312033123578,5.17979132833694,
10.9544517446419));
#117313=CARTESIAN_POINT('Ctrl Pts',(-8.82348470875356,5.18037177385699,
10.9459745902367));
#117314=CARTESIAN_POINT('Ctrl Pts',(-8.82364809094381,5.18060707268519,
10.9425268525269));
#117315=CARTESIAN_POINT('Ctrl Pts',(-8.82401679341926,5.18109122779144,
10.9354083933392));
#117316=CARTESIAN_POINT('Ctrl Pts',(-8.82422414685637,5.1813399720985,10.9317378442333));
#117317=CARTESIAN_POINT('Ctrl Pts',(-8.82481102559976,5.18198771539791,
10.9221467220803));
#117318=CARTESIAN_POINT('Ctrl Pts',(-8.8252181100707,5.18238523434374,10.9162278495741));
#117319=CARTESIAN_POINT('Ctrl Pts',(-8.82725177669946,5.18416463307864,
10.889599984298));
#117320=CARTESIAN_POINT('Ctrl Pts',(-8.82938144580318,5.18552137481392,
10.8689317514374));
#117321=CARTESIAN_POINT('Ctrl Pts',(-8.8371554648429,5.18940799569405,10.8090678054501));
#117322=CARTESIAN_POINT('Ctrl Pts',(-8.84423087633856,5.19188537719516,
10.7700854209061));
#117323=CARTESIAN_POINT('Ctrl Pts',(-8.87590496229846,5.20051440441316,
10.6347922245004));
#117324=CARTESIAN_POINT('Ctrl Pts',(-8.91069929638746,5.20657054187645,
10.5413187964714));
#117325=CARTESIAN_POINT('Ctrl Pts',(-8.96281734149196,5.21390000260526,
10.4418650936321));
#117326=CARTESIAN_POINT('Ctrl Pts',(-8.96901073523546,5.21475052102616,
10.4305058774916));
#117327=CARTESIAN_POINT('Ctrl Pts',(-8.97923281250113,5.21612380050177,
10.4124711486786));
#117328=CARTESIAN_POINT('Ctrl Pts',(-8.98314294825022,5.21664239868115,
10.4057294104122));
#117329=CARTESIAN_POINT('Ctrl Pts',(-8.99022267288183,5.21756990677087,
10.3937972347492));
#117330=CARTESIAN_POINT('Ctrl Pts',(-8.99336612518701,5.21797786979149,
10.3885915582233));
#117331=CARTESIAN_POINT('Ctrl Pts',(-9.0000362285879,5.21883567669276,10.3777364955041));
#117332=CARTESIAN_POINT('Ctrl Pts',(-9.00357075584341,5.21928579594137,
10.372092226985));
#117333=CARTESIAN_POINT('Ctrl Pts',(-9.01300475067712,5.22047585719046,
10.3573073901725));
#117334=CARTESIAN_POINT('Ctrl Pts',(-9.01898321181328,5.22121867242826,
10.3482182417021));
#117335=CARTESIAN_POINT('Ctrl Pts',(-9.04861812060305,5.22484792513734,
10.3044953904511));
#117336=CARTESIAN_POINT('Ctrl Pts',(-9.07398462415618,5.22779756156051,
10.2710631509616));
#117337=CARTESIAN_POINT('Ctrl Pts',(-9.16772397305489,5.23819362648886,
10.160326160456));
#117338=CARTESIAN_POINT('Ctrl Pts',(-9.24441595009571,5.24591863098025,
10.0907007179582));
#117339=CARTESIAN_POINT('Ctrl Pts',(-9.34598384071172,5.25474751622672,
10.0203187121912));
#117340=CARTESIAN_POINT('Ctrl Pts',(-9.36307972343717,5.2561900881126,10.009118955144));
#117341=CARTESIAN_POINT('Ctrl Pts',(-9.38566597550263,5.25803207900457,
9.99514864482541));
#117342=CARTESIAN_POINT('Ctrl Pts',(-9.39089755161546,5.25845439114048,
9.99196887395632));
#117343=CARTESIAN_POINT('Ctrl Pts',(-9.3993460043569,5.25912914486498,9.98692366329682));
#117344=CARTESIAN_POINT('Ctrl Pts',(-9.40254725038583,5.259383166397,9.98503246386043));
#117345=CARTESIAN_POINT('Ctrl Pts',(-9.40875267389584,5.25987230637961,
9.98140601949193));
#117346=CARTESIAN_POINT('Ctrl Pts',(-9.41175562072408,5.26010753721595,
9.97966885359074));
#117347=CARTESIAN_POINT('Ctrl Pts',(-9.41905472784858,5.26067583073346,
9.97548934876312));
#117348=CARTESIAN_POINT('Ctrl Pts',(-9.42335873151174,5.26100803818526,
9.97306069635257));
#117349=CARTESIAN_POINT('Ctrl Pts',(-9.43870822479607,5.26218301792305,
9.9645262513405));
#117350=CARTESIAN_POINT('Ctrl Pts',(-9.44983687399048,5.26301701316344,
9.95857073820351));
#117351=CARTESIAN_POINT('Ctrl Pts',(-9.47797980568794,5.2650870679309,9.94408707815932));
#117352=CARTESIAN_POINT('Ctrl Pts',(-9.49510949288136,5.26631199103282,
9.93579004002828));
#117353=CARTESIAN_POINT('Ctrl Pts',(-9.57624201158654,5.27198575680174,
9.8988924522562));
#117354=CARTESIAN_POINT('Ctrl Pts',(-9.64251748923933,5.27626141068937,
9.87562630167969));
#117355=CARTESIAN_POINT('Ctrl Pts',(-9.74372672579125,5.28274817852381,
9.84995824108618));
#117356=CARTESIAN_POINT('Ctrl Pts',(-9.77731781255851,5.28489307668369,
9.84298552981361));
#117357=CARTESIAN_POINT('Ctrl Pts',(-9.81114934783795,5.28707251000898,
9.83748957265839));
#117358=CARTESIAN_POINT('Origin',(-10.,2.67563288526385,11.));
#117359=CARTESIAN_POINT('',(-9.81114930150122,5.88552497076973,9.83748958018583));
#117360=CARTESIAN_POINT('',(-9.81114942708287,5.7873151623385,9.837489559785));
#117361=CARTESIAN_POINT('',(-9.81114930150157,2.67563288526385,9.83748958018577));
#117362=CARTESIAN_POINT('Ctrl Pts',(-9.81114930150087,5.88552497076973,
9.83748958018588));
#117363=CARTESIAN_POINT('Ctrl Pts',(-9.81114406242107,5.88552459974339,
9.83749043127837));
#117364=CARTESIAN_POINT('Ctrl Pts',(-9.81113882334679,5.88552422871864,
9.8374912824063));
#117365=CARTESIAN_POINT('Ctrl Pts',(-9.8024360018317,5.88490790764762,9.83890518312361));
#117366=CARTESIAN_POINT('Ctrl Pts',(-9.79375422478925,5.88429634821271,
9.8404158508858));
#117367=CARTESIAN_POINT('Ctrl Pts',(-9.78087802284497,5.88339498956459,
9.84280555972011));
#117368=CARTESIAN_POINT('Ctrl Pts',(-9.77667035322581,5.88310134728357,
9.84361023706996));
#117369=CARTESIAN_POINT('Ctrl Pts',(-9.76946483245139,5.88260014890704,
9.84502902114163));
#117370=CARTESIAN_POINT('Ctrl Pts',(-9.76646488435682,5.88239197812917,
9.84563187154425));
#117371=CARTESIAN_POINT('Ctrl Pts',(-9.7596016137902,5.8819168798276,9.84703892117514));
#117372=CARTESIAN_POINT('Ctrl Pts',(-9.75573995403913,5.8816503887072,9.84785084973122));
#117373=CARTESIAN_POINT('Ctrl Pts',(-9.74506802685902,5.88091602711178,
9.85015073006728));
#117374=CARTESIAN_POINT('Ctrl Pts',(-9.73826664506999,5.88045038129041,
9.85167978716491));
#117375=CARTESIAN_POINT('Ctrl Pts',(-9.6999348315331,5.87783741387306,9.8606556473168));
#117376=CARTESIAN_POINT('Ctrl Pts',(-9.66870560956317,5.87575201213268,
9.86934129665199));
#117377=CARTESIAN_POINT('Ctrl Pts',(-9.5637075312571,5.86876674638351,9.90326916325355));
#117378=CARTESIAN_POINT('Ctrl Pts',(-9.49210290870555,5.86403657435735,
9.93453700007007));
#117379=CARTESIAN_POINT('Ctrl Pts',(-9.3786102531275,5.85589983708813,9.99815642822322));
#117380=CARTESIAN_POINT('Ctrl Pts',(-9.33486077963731,5.85258517254869,
10.0266529047521));
#117381=CARTESIAN_POINT('Ctrl Pts',(-9.28392688182018,5.84840546082868,
10.0648704771497));
#117382=CARTESIAN_POINT('Ctrl Pts',(-9.27480908290593,5.84764395340013,
10.0719234656966));
#117383=CARTESIAN_POINT('Ctrl Pts',(-9.26047863966877,5.84642487351907,
10.0833487707033));
#117384=CARTESIAN_POINT('Ctrl Pts',(-9.25519767027068,5.84597070568024,
10.0876345003682));
#117385=CARTESIAN_POINT('Ctrl Pts',(-9.24528793210228,5.84510892310494,
10.0958200469238));
#117386=CARTESIAN_POINT('Ctrl Pts',(-9.24065151237843,5.84470170048504,
10.0997102883073));
#117387=CARTESIAN_POINT('Ctrl Pts',(-9.23020768045122,5.84377509530863,
10.1086113755649));
#117388=CARTESIAN_POINT('Ctrl Pts',(-9.22441887064966,5.84325485693479,
10.1136435243144));
#117389=CARTESIAN_POINT('Ctrl Pts',(-9.20688101688818,5.84165799172213,
10.1291923433159));
#117390=CARTESIAN_POINT('Ctrl Pts',(-9.19529407838422,5.8405740070527,10.139888359381));
#117391=CARTESIAN_POINT('Ctrl Pts',(-9.12259871485794,5.83358134324374,
10.2097490987593));
#117392=CARTESIAN_POINT('Ctrl Pts',(-9.06784708086802,5.82739781719684,
10.2751445530646));
#117393=CARTESIAN_POINT('Ctrl Pts',(-8.99369033251992,5.81759994807685,
10.3861702362804));
#117394=CARTESIAN_POINT('Ctrl Pts',(-8.96927336903892,5.81403881829452,
10.4281178212426));
#117395=CARTESIAN_POINT('Ctrl Pts',(-8.94045560497558,5.80943498656051,
10.4855022893029));
#117396=CARTESIAN_POINT('Ctrl Pts',(-8.93368192941249,5.80831736531687,
10.4996920530868));
#117397=CARTESIAN_POINT('Ctrl Pts',(-8.92267213861576,5.80644289014544,
10.5239959750511));
#117398=CARTESIAN_POINT('Ctrl Pts',(-8.91828953693916,5.80567942425871,
10.5340411517773));
#117399=CARTESIAN_POINT('Ctrl Pts',(-8.91223818135282,5.80460122856949,
10.5484569318351));
#117400=CARTESIAN_POINT('Ctrl Pts',(-8.91045440928401,5.8042802408036,10.552778215949));
#117401=CARTESIAN_POINT('Ctrl Pts',(-8.90740801032695,5.80372662015021,
10.5602847005243));
#117402=CARTESIAN_POINT('Ctrl Pts',(-8.90613348055591,5.80349329830521,
10.563464962039));
#117403=CARTESIAN_POINT('Ctrl Pts',(-8.90346236441944,5.80300070632083,
10.570215204812));
#117404=CARTESIAN_POINT('Ctrl Pts',(-8.90206931225173,5.80274164166202,
10.5737864826511));
#117405=CARTESIAN_POINT('Ctrl Pts',(-8.89830999552497,5.80203636423725,
10.5835647459076));
#117406=CARTESIAN_POINT('Ctrl Pts',(-8.89597872324454,5.80159214434732,
10.5897851631884));
#117407=CARTESIAN_POINT('Ctrl Pts',(-8.88476098448996,5.79941854582555,
10.6205053498393));
#117408=CARTESIAN_POINT('Ctrl Pts',(-8.87663605874554,5.79772878289715,
10.6452776583816));
#117409=CARTESIAN_POINT('Ctrl Pts',(-8.84714296391513,5.79100481729385,
10.7464205376861));
#117410=CARTESIAN_POINT('Ctrl Pts',(-8.83268873918605,5.78619299971891,
10.8245914967287));
#117411=CARTESIAN_POINT('Ctrl Pts',(-8.82150063333779,5.77767052953856,
10.9608594532464));
#117412=CARTESIAN_POINT('Ctrl Pts',(-8.82099420148175,5.77403646468365,
11.0183522329159));
#117413=CARTESIAN_POINT('Ctrl Pts',(-8.82543849920718,5.76949716008584,
11.0874017388211));
#117414=CARTESIAN_POINT('Ctrl Pts',(-8.8263712559981,5.76871938450978,11.0991430180399));
#117415=CARTESIAN_POINT('Ctrl Pts',(-8.82812524258723,5.76748032267523,
11.1176928660274));
#117416=CARTESIAN_POINT('Ctrl Pts',(-8.82883013409321,5.76702264022554,
11.124511845306));
#117417=CARTESIAN_POINT('Ctrl Pts',(-8.8302684478575,5.76615793937679,11.1373305855902));
#117418=CARTESIAN_POINT('Ctrl Pts',(-8.83098860812364,5.76575134604358,
11.1433316334499));
#117419=CARTESIAN_POINT('Ctrl Pts',(-8.83271655231483,5.76483126450219,
11.1568500548333));
#117420=CARTESIAN_POINT('Ctrl Pts',(-8.83375081870324,5.76431696771949,
11.1643637107505));
#117421=CARTESIAN_POINT('Ctrl Pts',(-8.83709358290215,5.76275674420453,
11.1870254383559));
#117422=CARTESIAN_POINT('Ctrl Pts',(-8.83962512001978,5.76170394410675,
11.2021384405338));
#117423=CARTESIAN_POINT('Ctrl Pts',(-8.85926430824147,5.75432361253402,
11.3068052293917));
#117424=CARTESIAN_POINT('Ctrl Pts',(-8.88642319868119,5.74767420660396,
11.3941420762905));
#117425=CARTESIAN_POINT('Ctrl Pts',(-8.94909745041793,5.73632949069466,
11.5354682693347));
#117426=CARTESIAN_POINT('Ctrl Pts',(-8.97947433378415,5.73168246798129,
11.5913134392622));
#117427=CARTESIAN_POINT('Ctrl Pts',(-9.01853842902365,5.72670382108187,
11.6510690493442));
#117428=CARTESIAN_POINT('Ctrl Pts',(-9.02293664404694,5.72615542599091,
11.6576510695236));
#117429=CARTESIAN_POINT('Ctrl Pts',(-9.02971559722468,5.72532894656235,
11.6675777743943));
#117430=CARTESIAN_POINT('Ctrl Pts',(-9.03204790532599,5.72504786695366,
11.6709550289205));
#117431=CARTESIAN_POINT('Ctrl Pts',(-9.03633637052463,5.72453706611834,
11.6770959570043));
#117432=CARTESIAN_POINT('Ctrl Pts',(-9.03828680974816,5.72430698861169,
11.6798634172351));
#117433=CARTESIAN_POINT('Ctrl Pts',(-9.0427207451727,5.72378895972093,11.686097423051));
#117434=CARTESIAN_POINT('Ctrl Pts',(-9.04521115462734,5.72350147859463,
11.6895589226553));
#117435=CARTESIAN_POINT('Ctrl Pts',(-9.05171656195851,5.72275926243928,
11.6984981800828));
#117436=CARTESIAN_POINT('Ctrl Pts',(-9.05576030387578,5.72230638705161,
11.7039549616198));
#117437=CARTESIAN_POINT('Ctrl Pts',(-9.08540933040225,5.71904418403597,
11.743249319572));
#117438=CARTESIAN_POINT('Ctrl Pts',(-9.11278257776186,5.71634235973109,
11.7757201378216));
#117439=CARTESIAN_POINT('Ctrl Pts',(-9.15587792623229,5.71239901438189,
11.8215670137983));
#117440=CARTESIAN_POINT('Ctrl Pts',(-9.17029087370016,5.71112615640171,
11.8361203478293));
#117441=CARTESIAN_POINT('Ctrl Pts',(-9.22052008000168,5.70681409874214,
11.884260319799));
#117442=CARTESIAN_POINT('Ctrl Pts',(-9.25805239757169,5.70379426690557,
11.9159797393901));
#117443=CARTESIAN_POINT('Ctrl Pts',(-9.33747171227837,5.69759586544388,
11.9750063295858));
#117444=CARTESIAN_POINT('Ctrl Pts',(-9.37933312926429,5.69442158664187,
12.0021740393106));
#117445=CARTESIAN_POINT('Ctrl Pts',(-9.4327244065501,5.69040002346307,12.0321935128412));
#117446=CARTESIAN_POINT('Ctrl Pts',(-9.44274265852867,5.68964668518327,
12.0376363946056));
#117447=CARTESIAN_POINT('Ctrl Pts',(-9.45883660155914,5.68843764028238,
12.0460798846348));
#117448=CARTESIAN_POINT('Ctrl Pts',(-9.46486206456467,5.68798524005714,
12.0491750738924));
#117449=CARTESIAN_POINT('Ctrl Pts',(-9.4763253168761,5.68712487681217,12.0549391345705));
#117450=CARTESIAN_POINT('Ctrl Pts',(-9.48175766784359,5.68671728908274,
12.0576183783416));
#117451=CARTESIAN_POINT('Ctrl Pts',(-9.49415668642269,5.68578716624395,
12.0636151290799));
#117452=CARTESIAN_POINT('Ctrl Pts',(-9.50113571530714,5.68526375002682,
12.0669062851322));
#117453=CARTESIAN_POINT('Ctrl Pts',(-9.52269288726857,5.68364707536877,
12.0768144141167));
#117454=CARTESIAN_POINT('Ctrl Pts',(-9.537373491662,5.68254619025874,12.0832026737725));
#117455=CARTESIAN_POINT('Ctrl Pts',(-9.62519938446605,5.67595754357751,
12.1193090241073));
#117456=CARTESIAN_POINT('Ctrl Pts',(-9.70104056978686,5.67023716878254,
12.1419051472132));
#117457=CARTESIAN_POINT('Ctrl Pts',(-9.83047798117983,5.66057127619783,
12.1666841498741));
#117458=CARTESIAN_POINT('Ctrl Pts',(-9.88301121043996,5.65667956352694,
12.1731171029779));
#117459=CARTESIAN_POINT('Ctrl Pts',(-9.95227149067951,5.65169952400828,
12.1768981018724));
#117460=CARTESIAN_POINT('Ctrl Pts',(-9.96876008011703,5.65052537016828,
12.1774511781401));
#117461=CARTESIAN_POINT('Ctrl Pts',(-9.9966136112175,5.64856671112462,12.1777999057641));
#117462=CARTESIAN_POINT('Ctrl Pts',(-10.0079735508587,5.64777484537909,
12.1777777939335));
#117463=CARTESIAN_POINT('Ctrl Pts',(-10.0240731894887,5.64666406673858,
12.1775134945803));
#117464=CARTESIAN_POINT('Ctrl Pts',(-10.0288140672277,5.64633838616956,
12.1774070238633));
#117465=CARTESIAN_POINT('Ctrl Pts',(-10.0369890303224,5.64577937746597,
12.1771740233588));
#117466=CARTESIAN_POINT('Ctrl Pts',(-10.0404234054626,5.64554532178425,
12.1770610940759));
#117467=CARTESIAN_POINT('Ctrl Pts',(-10.047656018266,5.64505412198855,12.1767915772513));
#117468=CARTESIAN_POINT('Ctrl Pts',(-10.0514540396017,5.64479716141633,
12.1766316310561));
#117469=CARTESIAN_POINT('Ctrl Pts',(-10.061740876167,5.6441036859817,12.1761485171375));
#117470=CARTESIAN_POINT('Ctrl Pts',(-10.0682280147675,5.64366905365487,
12.1757900377627));
#117471=CARTESIAN_POINT('Ctrl Pts',(-10.0991106491538,5.6416113511472,12.1738270056852));
#117472=CARTESIAN_POINT('Ctrl Pts',(-10.1234570948852,5.64002304374319,
12.1715166672989));
#117473=CARTESIAN_POINT('Ctrl Pts',(-10.2285514178665,5.63324627137455,
12.1582306034192));
#117474=CARTESIAN_POINT('Ctrl Pts',(-10.3081138554265,5.62830661856359,
12.1396498766632));
#117475=CARTESIAN_POINT('Ctrl Pts',(-10.4391284790065,5.61966370903022,
12.0943156428758));
#117476=CARTESIAN_POINT('Ctrl Pts',(-10.4916931303341,5.61604662169256,
12.0717262544816));
#117477=CARTESIAN_POINT('Ctrl Pts',(-10.5528506709881,5.61152642924802,
12.0399950157005));
#117478=CARTESIAN_POINT('Ctrl Pts',(-10.5632123365653,5.61074944104743,
12.0344202940601));
#117479=CARTESIAN_POINT('Ctrl Pts',(-10.5794738502178,5.60951134623697,
12.0253546112582));
#117480=CARTESIAN_POINT('Ctrl Pts',(-10.5854299065914,5.60905383368398,
12.0219656760583));
#117481=CARTESIAN_POINT('Ctrl Pts',(-10.5965832380452,5.60818927667283,
12.0154900483042));
#117482=CARTESIAN_POINT('Ctrl Pts',(-10.6017870040175,5.607782655702,12.0124149335053));
#117483=CARTESIAN_POINT('Ctrl Pts',(-10.6134699051194,5.60686227232976,
12.0053891400716));
#117484=CARTESIAN_POINT('Ctrl Pts',(-10.6199349394416,5.60634769915679,
12.0014156547904));
#117485=CARTESIAN_POINT('Ctrl Pts',(-10.6393545172723,5.60478578231564,
11.989220036783));
#117486=CARTESIAN_POINT('Ctrl Pts',(-10.6521867798943,5.60373154325811,
11.980807241826));
#117487=CARTESIAN_POINT('Ctrl Pts',(-10.7399264649682,5.59636461716038,
11.9208021129442));
#117488=CARTESIAN_POINT('Ctrl Pts',(-10.8087887160381,5.58973181859896,
11.8609427742068));
#117489=CARTESIAN_POINT('Ctrl Pts',(-10.9001104349996,5.57978878465653,
11.7608438176995));
#117490=CARTESIAN_POINT('Ctrl Pts',(-10.9282617293026,5.57652272338885,
11.7262318700659));
#117491=CARTESIAN_POINT('Ctrl Pts',(-10.967461607773,5.5717331635018,11.6720202319838));
#117492=CARTESIAN_POINT('Ctrl Pts',(-10.9800232298039,5.57015517411939,
11.6535654361874));
#117493=CARTESIAN_POINT('Ctrl Pts',(-10.9953288582824,5.56818582382703,
11.6296447048368));
#117494=CARTESIAN_POINT('Ctrl Pts',(-10.9985644707956,5.56776666929828,
11.6245005941458));
#117495=CARTESIAN_POINT('Ctrl Pts',(-11.003710509252,5.56709569547738,11.616176947964));
#117496=CARTESIAN_POINT('Ctrl Pts',(-11.0056459330865,5.56684232732312,
11.613013112269));
#117497=CARTESIAN_POINT('Ctrl Pts',(-11.009345482797,5.56635612360757,11.6069007857162));
#117498=CARTESIAN_POINT('Ctrl Pts',(-11.0111116878844,5.56612316335686,
11.6039536590662));
#117499=CARTESIAN_POINT('Ctrl Pts',(-11.014992189835,5.5656093665597,11.5974138382281));
#117500=CARTESIAN_POINT('Ctrl Pts',(-11.0171003815897,5.56532891452956,
11.5938175263586));
#117501=CARTESIAN_POINT('Ctrl Pts',(-11.0245405850407,5.56433413180136,
11.5809695965326));
#117502=CARTESIAN_POINT('Ctrl Pts',(-11.0297660127139,5.56362614902656,
11.571656418801));
#117503=CARTESIAN_POINT('Ctrl Pts',(-11.063216956933,5.55902263083453,11.5100899144462));
#117504=CARTESIAN_POINT('Ctrl Pts',(-11.0875857488051,5.5553219452896,11.4558300495267));
#117505=CARTESIAN_POINT('Ctrl Pts',(-11.1257961811559,5.54835085356728,
11.3499988564461));
#117506=CARTESIAN_POINT('Ctrl Pts',(-11.1404329096589,5.54508402266163,
11.2988792322528));
#117507=CARTESIAN_POINT('Ctrl Pts',(-11.157832931308,5.53986631643473,11.2177390931551));
#117508=CARTESIAN_POINT('Ctrl Pts',(-11.1629825626586,5.53796778550377,
11.1883050083109));
#117509=CARTESIAN_POINT('Ctrl Pts',(-11.1697973235746,5.53470031998053,
11.1381950382607));
#117510=CARTESIAN_POINT('Ctrl Pts',(-11.1720455713564,5.53334835728354,
11.1176126781708));
#117511=CARTESIAN_POINT('Ctrl Pts',(-11.174452548057,5.53141580923354,11.0884818251458));
#117512=CARTESIAN_POINT('Ctrl Pts',(-11.1750625578011,5.53084910635873,
11.0799737452216));
#117513=CARTESIAN_POINT('Ctrl Pts',(-11.1759549176895,5.52986703646142,
11.0652936315042));
#117514=CARTESIAN_POINT('Ctrl Pts',(-11.1762812219478,5.52945304144557,
11.0591245395319));
#117515=CARTESIAN_POINT('Ctrl Pts',(-11.1768139011635,5.52865617850915,
11.0472890367062));
#117516=CARTESIAN_POINT('Ctrl Pts',(-11.1770279198747,5.52827355866869,
11.0416231289635));
#117517=CARTESIAN_POINT('Ctrl Pts',(-11.177435879426,5.52736878559432,11.028266508282));
#117518=CARTESIAN_POINT('Ctrl Pts',(-11.1775953918063,5.52684558491964,
11.0205750815706));
#117519=CARTESIAN_POINT('Ctrl Pts',(-11.1778910658077,5.52499898106644,
10.9935460788147));
#117520=CARTESIAN_POINT('Ctrl Pts',(-11.1776263072097,5.52366340042991,
10.974208137152));
#117521=CARTESIAN_POINT('Ctrl Pts',(-11.1724407701324,5.51421429580306,
10.8389321317401));
#117522=CARTESIAN_POINT('Ctrl Pts',(-11.1508821866952,5.50556835244807,
10.7242826832966));
#117523=CARTESIAN_POINT('Ctrl Pts',(-11.1018482266343,5.49470750186665,
10.5826593882331));
#117524=CARTESIAN_POINT('Ctrl Pts',(-11.0893874093102,5.49228474974297,
10.5511367259678));
#117525=CARTESIAN_POINT('Ctrl Pts',(-11.0727868559334,5.48945172931495,
10.51392331266));
#117526=CARTESIAN_POINT('Ctrl Pts',(-11.0699354526548,5.48897728695651,
10.5076786445618));
#117527=CARTESIAN_POINT('Ctrl Pts',(-11.0653864428832,5.48823947147091,
10.4979423770558));
#117528=CARTESIAN_POINT('Ctrl Pts',(-11.0637259519631,5.48797397793081,
10.49443375345));
#117529=CARTESIAN_POINT('Ctrl Pts',(-11.0605726301511,5.48747700080756,
10.48785508753));
#117530=CARTESIAN_POINT('Ctrl Pts',(-11.0590838042314,5.48724529960491,
10.4847833357211));
#117531=CARTESIAN_POINT('Ctrl Pts',(-11.0555996030202,5.48670976856614,
10.4776736407389));
#117532=CARTESIAN_POINT('Ctrl Pts',(-11.0535943950282,5.48640654164237,
10.4736406171644));
#117533=CARTESIAN_POINT('Ctrl Pts',(-11.0469480797857,5.48541729057034,
10.4604632201044));
#117534=CARTESIAN_POINT('Ctrl Pts',(-11.0422105248734,5.48473685629135,
10.4513676477389));
#117535=CARTESIAN_POINT('Ctrl Pts',(-11.0031303788792,5.47930845945104,
10.3786717647131));
#117536=CARTESIAN_POINT('Ctrl Pts',(-10.9631133308537,5.47485492961544,
10.3182852947561));
#117537=CARTESIAN_POINT('Ctrl Pts',(-10.8824209095297,5.46688975445587,
10.2179407046006));
#117538=CARTESIAN_POINT('Ctrl Pts',(-10.8439189247069,5.4633963659952,10.1765416553175));
#117539=CARTESIAN_POINT('Ctrl Pts',(-10.7871115117689,5.45845171046103,
10.1236448470087));
#117540=CARTESIAN_POINT('Ctrl Pts',(-10.7712391376717,5.45709064810652,
10.1096444533341));
#117541=CARTESIAN_POINT('Ctrl Pts',(-10.7427307503486,5.45467283327899,
10.0858328362572));
#117542=CARTESIAN_POINT('Ctrl Pts',(-10.7302557564939,5.45362335693133,
10.0758371024373));
#117543=CARTESIAN_POINT('Ctrl Pts',(-10.7114668705541,5.45205282311485,
10.0614002873347));
#117544=CARTESIAN_POINT('Ctrl Pts',(-10.7053061978194,5.45153943029495,
10.0567621237956));
#117545=CARTESIAN_POINT('Ctrl Pts',(-10.6942263617664,5.45061862925353,
10.0485897289282));
#117546=CARTESIAN_POINT('Ctrl Pts',(-10.6893246009638,5.45021212994072,
10.0450322846075));
#117547=CARTESIAN_POINT('Ctrl Pts',(-10.678880643486,5.44934772076676,10.037574908011));
#117548=CARTESIAN_POINT('Ctrl Pts',(-10.6733318073897,5.44888946223864,
10.0336846996783));
#117549=CARTESIAN_POINT('Ctrl Pts',(-10.6583479255175,5.44765447422548,
10.0233714403328));
#117550=CARTESIAN_POINT('Ctrl Pts',(-10.6488527702463,5.44687446957186,
10.0170374364967));
#117551=CARTESIAN_POINT('Ctrl Pts',(-10.602305862934,5.44306204074122,9.98695535019707));
#117552=CARTESIAN_POINT('Ctrl Pts',(-10.5640391137128,5.439960129923,9.9651614370261));
#117553=CARTESIAN_POINT('Ctrl Pts',(-10.4588046511441,5.43151692831929,
9.91280093839774));
#117554=CARTESIAN_POINT('Ctrl Pts',(-10.3900416424152,5.42607936855843,
9.88628122184891));
#117555=CARTESIAN_POINT('Ctrl Pts',(-10.2900044000344,5.41849327848107,
9.85810837965382));
#117556=CARTESIAN_POINT('Ctrl Pts',(-10.2604357582787,5.41629123771702,
9.85100370638562));
#117557=CARTESIAN_POINT('Ctrl Pts',(-10.219026518867,5.4132886761397,9.84273499111006));
#117558=CARTESIAN_POINT('Ctrl Pts',(-10.2073947470695,5.41245408513059,
9.84059396276645));
#117559=CARTESIAN_POINT('Ctrl Pts',(-10.187028629238,5.4110103215799,9.83716155093464));
#117560=CARTESIAN_POINT('Ctrl Pts',(-10.1783084910422,5.4103977231405,9.83579251832996));
#117561=CARTESIAN_POINT('Ctrl Pts',(-10.1653314596302,5.40949513956807,
9.83390440077596));
#117562=CARTESIAN_POINT('Ctrl Pts',(-10.1610860284991,5.40920129664895,
9.83331035362914));
#117563=CARTESIAN_POINT('Ctrl Pts',(-10.1538044284708,5.40869987692085,
9.83233197138127));
#117564=CARTESIAN_POINT('Ctrl Pts',(-10.1507699039277,5.40849168383517,
9.83193627566852));
#117565=CARTESIAN_POINT('Ctrl Pts',(-10.1438209931884,5.40801670140396,
9.83105768366957));
#117566=CARTESIAN_POINT('Ctrl Pts',(-10.1399056940824,5.40775034718834,
9.83058261732952));
#117567=CARTESIAN_POINT('Ctrl Pts',(-10.1290729601648,5.4070167324915,9.82932340182948));
#117568=CARTESIAN_POINT('Ctrl Pts',(-10.1221507121503,5.40655168935038,
9.82858088804931));
#117569=CARTESIAN_POINT('Ctrl Pts',(-10.0831521311226,5.40395073157816,
9.82474717346643));
#117570=CARTESIAN_POINT('Ctrl Pts',(-10.0509630330365,5.40187606457298,
9.82291178587159));
#117571=CARTESIAN_POINT('Ctrl Pts',(-9.95549252278619,5.39583034815833,
9.82139280444906));
#117572=CARTESIAN_POINT('Ctrl Pts',(-9.89226756188441,5.39196179669756,
9.82548291059762));
#117573=CARTESIAN_POINT('Ctrl Pts',(-9.82349116475283,5.38764709326431,
9.83553499775459));
#117574=CARTESIAN_POINT('Ctrl Pts',(-9.8173159697757,5.38725879013721,9.83648780022633));
#117575=CARTESIAN_POINT('Ctrl Pts',(-9.81114929672518,5.38686993568377,
9.8374895809617));
#117576=CARTESIAN_POINT('Ctrl Pts',(-9.81114934783795,5.28707251000898,
9.83748957265839));
#117577=CARTESIAN_POINT('Ctrl Pts',(-9.84003655603766,5.28893342893285,
9.83279682498117));
#117578=CARTESIAN_POINT('Ctrl Pts',(-9.8690990738413,5.29081941320123,9.82918072532109));
#117579=CARTESIAN_POINT('Ctrl Pts',(-9.91035600248275,5.29353346110809,
9.82560398103576));
#117580=CARTESIAN_POINT('Ctrl Pts',(-9.92244983736818,5.29433342294489,
9.82474342793177));
#117581=CARTESIAN_POINT('Ctrl Pts',(-9.94154279040337,5.29560425869866,
9.82368082334977));
#117582=CARTESIAN_POINT('Ctrl Pts',(-9.94853433172485,5.29607128605353,
9.8233542027683));
#117583=CARTESIAN_POINT('Ctrl Pts',(-9.96155207023144,5.29694414827467,
9.82286230308912));
#117584=CARTESIAN_POINT('Ctrl Pts',(-9.96757745713924,5.29734947218436,
9.82268093653636));
#117585=CARTESIAN_POINT('Ctrl Pts',(-9.98098357699742,5.29825433367354,
9.82238039863986));
#117586=CARTESIAN_POINT('Ctrl Pts',(-9.98836452071871,5.29875456865255,
9.82228434620873));
#117587=CARTESIAN_POINT('Ctrl Pts',(-10.0100480122875,5.300230412983,9.82220602068969));
#117588=CARTESIAN_POINT('Ctrl Pts',(-10.0243494687764,5.30121184429461,
9.82241488951198));
#117589=CARTESIAN_POINT('Ctrl Pts',(-10.1064466018248,5.30689422286634,
9.82511002214406));
#117590=CARTESIAN_POINT('Ctrl Pts',(-10.173919772126,5.31176545401268,9.8331896124798));
#117591=CARTESIAN_POINT('Ctrl Pts',(-10.3115809662342,5.32204088859045,
9.86188217036142));
#117592=CARTESIAN_POINT('Ctrl Pts',(-10.3813200809907,5.32743634491947,
9.88331267003869));
#117593=CARTESIAN_POINT('Ctrl Pts',(-10.4662599648282,5.33398713876658,
9.91830686357245));
#117594=CARTESIAN_POINT('Ctrl Pts',(-10.4837065430341,5.33533073191038,
9.92599512252269));
#117595=CARTESIAN_POINT('Ctrl Pts',(-10.50636381614,5.33706620373662,9.93664380355342));
#117596=CARTESIAN_POINT('Ctrl Pts',(-10.5117484463958,5.33747793486259,
9.93922469570708));
#117597=CARTESIAN_POINT('Ctrl Pts',(-10.5204239482764,5.3381398701793,9.9434643621364));
#117598=CARTESIAN_POINT('Ctrl Pts',(-10.5237269876681,5.33839155208412,
9.94509778493546));
#117599=CARTESIAN_POINT('Ctrl Pts',(-10.5301407993323,5.33887952871056,
9.94830710050897));
#117600=CARTESIAN_POINT('Ctrl Pts',(-10.5332523059126,5.33911591144904,
9.94988133976267));
#117601=CARTESIAN_POINT('Ctrl Pts',(-10.5408422871726,5.33969177948089,
9.9537638569598));
#117602=CARTESIAN_POINT('Ctrl Pts',(-10.5453130984274,5.3400303525816,9.95608713315175));
#117603=CARTESIAN_POINT('Ctrl Pts',(-10.5614997382277,5.34125434447246,
9.964630956192));
#117604=CARTESIAN_POINT('Ctrl Pts',(-10.573125677455,5.3421299908398,9.97102089090047));
#117605=CARTESIAN_POINT('Ctrl Pts',(-10.6598725121756,5.34865619797864,
10.0206258696862));
#117606=CARTESIAN_POINT('Ctrl Pts',(-10.7301349744772,5.35391471485805,
10.0718231339762));
#117607=CARTESIAN_POINT('Ctrl Pts',(-10.8422957840801,5.36334458069843,
10.1742374655474));
#117608=CARTESIAN_POINT('Ctrl Pts',(-10.8867028622079,5.3674436026676,10.2221167540769));
#117609=CARTESIAN_POINT('Ctrl Pts',(-10.9344091126706,5.37251143922848,
10.2829768972989));
#117610=CARTESIAN_POINT('Ctrl Pts',(-10.9417520274596,5.37331263907679,
10.2926488703571));
#117611=CARTESIAN_POINT('Ctrl Pts',(-10.9530919253782,5.37458500742185,
10.308075226238));
#117612=CARTESIAN_POINT('Ctrl Pts',(-10.9571894931464,5.37505231362611,
10.3137548678383));
#117613=CARTESIAN_POINT('Ctrl Pts',(-10.9647191132482,5.37592543355481,
10.3243903271433));
#117614=CARTESIAN_POINT('Ctrl Pts',(-10.9681642600872,5.37633073383439,
10.3293366263896));
#117615=CARTESIAN_POINT('Ctrl Pts',(-10.9757404392779,5.37723520509736,
10.3403940067513));
#117616=CARTESIAN_POINT('Ctrl Pts',(-10.9798523066338,5.37773507053128,
10.3465178471625));
#117617=CARTESIAN_POINT('Ctrl Pts',(-10.991752671097,5.37920872015507,10.3646060257387));
#117618=CARTESIAN_POINT('Ctrl Pts',(-10.9993812377255,5.38018830005791,
10.3766734613125));
#117619=CARTESIAN_POINT('Ctrl Pts',(-11.0537990668637,5.38744288416676,
10.4663234262583));
#117620=CARTESIAN_POINT('Ctrl Pts',(-11.0917078444396,5.39403838982277,
10.5489223726652));
#117621=CARTESIAN_POINT('Ctrl Pts',(-11.1388464897861,5.40520174648392,
10.693549104112));
#117622=CARTESIAN_POINT('Ctrl Pts',(-11.1533052169353,5.40971560106077,
10.7534802030505));
#117623=CARTESIAN_POINT('Ctrl Pts',(-11.164689748759,5.41478374034189,10.824769137523));
#117624=CARTESIAN_POINT('Ctrl Pts',(-11.1662239967187,5.41552393345971,
10.835289116389));
#117625=CARTESIAN_POINT('Ctrl Pts',(-11.1681602729992,5.41654374003203,
10.8499535127358));
#117626=CARTESIAN_POINT('Ctrl Pts',(-11.1686830383015,5.41682946634,10.8540810874074));
#117627=CARTESIAN_POINT('Ctrl Pts',(-11.169597240414,5.41734880062795,10.8616195678858));
#117628=CARTESIAN_POINT('Ctrl Pts',(-11.169995656157,5.41758278371806,10.8650295789037));
#117629=CARTESIAN_POINT('Ctrl Pts',(-11.1707937052025,5.41806793129367,
10.8721292277762));
#117630=CARTESIAN_POINT('Ctrl Pts',(-11.1711908184042,5.41831895740958,
10.8758190740244));
#117631=CARTESIAN_POINT('Ctrl Pts',(-11.1721935440615,5.41897946267186,
10.8855690249623));
#117632=CARTESIAN_POINT('Ctrl Pts',(-11.1727696135399,5.41938735304755,
10.8916321528842));
#117633=CARTESIAN_POINT('Ctrl Pts',(-11.1752513204197,5.42128995084117,
10.9200952317838));
#117634=CARTESIAN_POINT('Ctrl Pts',(-11.1765625327089,5.42275506185808,
10.9425439132997));
#117635=CARTESIAN_POINT('Ctrl Pts',(-11.178570873109,5.42709631502357,11.0101296033905));
#117636=CARTESIAN_POINT('Ctrl Pts',(-11.1773173543358,5.42990436419411,
11.0552844313765));
#117637=CARTESIAN_POINT('Ctrl Pts',(-11.1658069306276,5.43827995951092,
11.1900076949119));
#117638=CARTESIAN_POINT('Ctrl Pts',(-11.1478699386521,5.44380701521126,
11.2785700845506));
#117639=CARTESIAN_POINT('Ctrl Pts',(-11.1152485044215,5.45067991826223,
11.3788847325628));
#117640=CARTESIAN_POINT('Ctrl Pts',(-11.1101922042834,5.45169309687747,
11.3934540646525));
#117641=CARTESIAN_POINT('Ctrl Pts',(-11.102218422932,5.45321959649493,11.4150510869215));
#117642=CARTESIAN_POINT('Ctrl Pts',(-11.0995164126636,5.45372587649981,
11.4221569736007));
#117643=CARTESIAN_POINT('Ctrl Pts',(-11.0945430116122,5.45463876729614,
11.4348645659652));
#117644=CARTESIAN_POINT('Ctrl Pts',(-11.0922969126987,5.45504452891149,
11.4404759325852));
#117645=CARTESIAN_POINT('Ctrl Pts',(-11.0874169737869,5.45591259223395,
11.4524004627123));
#117646=CARTESIAN_POINT('Ctrl Pts',(-11.0847711348596,5.45637528250779,
11.4587084423802));
#117647=CARTESIAN_POINT('Ctrl Pts',(-11.077445555866,5.45763538786231,11.4757555697594));
#117648=CARTESIAN_POINT('Ctrl Pts',(-11.0726604020385,5.45843631435026,
11.4864482837258));
#117649=CARTESIAN_POINT('Ctrl Pts',(-11.0440676953305,5.46309958184428,
11.5478663191076));
#117650=CARTESIAN_POINT('Ctrl Pts',(-11.0168272362663,5.4670783035356,11.5969049761292));
#117651=CARTESIAN_POINT('Ctrl Pts',(-10.9394109995266,5.47734176831897,
11.7154925765967));
#117652=CARTESIAN_POINT('Ctrl Pts',(-10.8849445616635,5.48371795124326,
11.7818537567358));
#117653=CARTESIAN_POINT('Ctrl Pts',(-10.8080703047851,5.49141902045241,
11.8570880304801));
#117654=CARTESIAN_POINT('Ctrl Pts',(-10.7919444462839,5.49297240465356,
11.8720101211003));
#117655=CARTESIAN_POINT('Ctrl Pts',(-10.7706858767621,5.4949323528122,11.8906052580174));
#117656=CARTESIAN_POINT('Ctrl Pts',(-10.7659292176721,5.49536545225431,
11.8946993260946));
#117657=CARTESIAN_POINT('Ctrl Pts',(-10.7582767463356,5.49605326875225,
11.9011800684941));
#117658=CARTESIAN_POINT('Ctrl Pts',(-10.7554019404259,5.49630967257001,
11.9035911958841));
#117659=CARTESIAN_POINT('Ctrl Pts',(-10.7498589212496,5.49680016975425,
11.9081952367354));
#117660=CARTESIAN_POINT('Ctrl Pts',(-10.7471925372069,5.49703439950226,
11.9103901924176));
#117661=CARTESIAN_POINT('Ctrl Pts',(-10.7407562084799,5.4975957790995,11.9156412252569));
#117662=CARTESIAN_POINT('Ctrl Pts',(-10.736976904448,5.4979221255154,11.9186858321313));
#117663=CARTESIAN_POINT('Ctrl Pts',(-10.7237487777928,5.49905342925434,
11.9292082449067));
#117664=CARTESIAN_POINT('Ctrl Pts',(-10.7142037360135,5.49985044899447,
11.9365646303574));
#117665=CARTESIAN_POINT('Ctrl Pts',(-10.6902308992104,5.50180956290318,
11.954460862457));
#117666=CARTESIAN_POINT('Ctrl Pts',(-10.6756726646755,5.50296199112549,
11.9648216164006));
#117667=CARTESIAN_POINT('Ctrl Pts',(-10.6099529527165,5.50802826873212,
12.0093753245141));
#117668=CARTESIAN_POINT('Ctrl Pts',(-10.5563912828239,5.51180378374164,
12.0398610279887));
#117669=CARTESIAN_POINT('Ctrl Pts',(-10.4336639918296,5.52020005152387,
12.0975035431772));
#117670=CARTESIAN_POINT('Ctrl Pts',(-10.3638284418439,5.52482421478696,
12.1225886489348));
#117671=CARTESIAN_POINT('Ctrl Pts',(-10.2803235330198,5.53047305218441,
12.143967523567));
#117672=CARTESIAN_POINT('Ctrl Pts',(-10.2684958362515,5.53127547339873,
12.1468011798728));
#117673=CARTESIAN_POINT('Ctrl Pts',(-10.2497874299115,5.53254935365872,
12.1509780231997));
#117674=CARTESIAN_POINT('Ctrl Pts',(-10.2429347690995,5.53301693486544,
12.1524438660627));
#117675=CARTESIAN_POINT('Ctrl Pts',(-10.2301642890874,5.53389030945156,
12.1550566195723));
#117676=CARTESIAN_POINT('Ctrl Pts',(-10.2242499287071,5.53429558693422,
12.1562194262132));
#117677=CARTESIAN_POINT('Ctrl Pts',(-10.211083758798,5.53519967581801,12.1587031720095));
#117678=CARTESIAN_POINT('Ctrl Pts',(-10.2038280000269,5.53569917877641,
12.1600015242181));
#117679=CARTESIAN_POINT('Ctrl Pts',(-10.1825106168296,5.53717067734174,
12.1636098991202));
#117680=CARTESIAN_POINT('Ctrl Pts',(-10.1684191173383,5.53814844299294,
12.165732856474));
#117681=CARTESIAN_POINT('Ctrl Pts',(-10.1362093312238,5.5403958101997,12.1699892364676));
#117682=CARTESIAN_POINT('Ctrl Pts',(-10.118073396393,5.54167014075104,12.171958363703));
#117683=CARTESIAN_POINT('Ctrl Pts',(-10.0559368143059,5.54606738930973,
12.1772480163532));
#117684=CARTESIAN_POINT('Ctrl Pts',(-10.0118024752413,5.54924562590739,
12.1785167910004));
#117685=CARTESIAN_POINT('Ctrl Pts',(-9.90429018920359,5.55708621360699,
12.1755675827569));
#117686=CARTESIAN_POINT('Ctrl Pts',(-9.84112059918129,5.56177996137742,
12.1687073338518));
#117687=CARTESIAN_POINT('Ctrl Pts',(-9.74740744030234,5.56868543722492,
12.150788555779));
#117688=CARTESIAN_POINT('Ctrl Pts',(-9.71625822513954,5.57096933138761,
12.1435070198843));
#117689=CARTESIAN_POINT('Ctrl Pts',(-9.67874669146476,5.57367699045913,
12.1331106007244));
#117690=CARTESIAN_POINT('Ctrl Pts',(-9.67206850815527,5.57415734697159,
12.1311959442064));
#117691=CARTESIAN_POINT('Ctrl Pts',(-9.66162987120367,5.57490512522231,
12.1281029392176));
#117692=CARTESIAN_POINT('Ctrl Pts',(-9.65785785370527,5.57517470532991,
12.1269646571228));
#117693=CARTESIAN_POINT('Ctrl Pts',(-9.65116672815232,5.5756517006279,12.1249087843609));
#117694=CARTESIAN_POINT('Ctrl Pts',(-9.64824547155877,5.57585953156193,
12.1239987441045));
#117695=CARTESIAN_POINT('Ctrl Pts',(-9.64123748255917,5.57635713618037,
12.1217855930865));
#117696=CARTESIAN_POINT('Ctrl Pts',(-9.63715428391033,5.5766462763919,12.1204715295526));
#117697=CARTESIAN_POINT('Ctrl Pts',(-9.62467482199324,5.57752781745608,
12.116379990083));
#117698=CARTESIAN_POINT('Ctrl Pts',(-9.61630235863866,5.57811624329526,
12.113530153603));
#117699=CARTESIAN_POINT('Ctrl Pts',(-9.59678183201735,5.57948287406148,
12.1066393972782));
#117700=CARTESIAN_POINT('Ctrl Pts',(-9.58566094855489,5.58025736744226,
12.1025238411512));
#117701=CARTESIAN_POINT('Ctrl Pts',(-9.54614159833198,5.58300136878465,
12.0872162823073));
#117702=CARTESIAN_POINT('Ctrl Pts',(-9.51811680547734,5.58493202198807,
12.0750886196897));
#117703=CARTESIAN_POINT('Ctrl Pts',(-9.42420774075897,5.59144914596474,
12.0300386123009));
#117704=CARTESIAN_POINT('Ctrl Pts',(-9.36095543944663,5.59593139552262,
11.9920375914384));
#117705=CARTESIAN_POINT('Ctrl Pts',(-9.26639850108618,5.60331870707735,
11.9224109411773));
#117706=CARTESIAN_POINT('Ctrl Pts',(-9.23261182661492,5.60611846080799,
11.8944986564432));
#117707=CARTESIAN_POINT('Ctrl Pts',(-9.19210438609852,5.60974073079378,
11.8570468131491));
#117708=CARTESIAN_POINT('Ctrl Pts',(-9.18386131626456,5.61049269071724,
11.8492009167682));
#117709=CARTESIAN_POINT('Ctrl Pts',(-9.17089913990472,5.61169996255374,
11.8365002296261));
#117710=CARTESIAN_POINT('Ctrl Pts',(-9.16610582873728,5.61215198389991,
11.8317219356774));
#117711=CARTESIAN_POINT('Ctrl Pts',(-9.15710200405896,5.61301190517363,
11.8225902430264));
#117712=CARTESIAN_POINT('Ctrl Pts',(-9.15288335221187,5.61341943243898,
11.8182451479701));
#117713=CARTESIAN_POINT('Ctrl Pts',(-9.14336326768805,5.61434980373827,
11.8082871882457));
#117714=CARTESIAN_POINT('Ctrl Pts',(-9.13808318547892,5.61487353205715,
11.802654389986));
#117715=CARTESIAN_POINT('Ctrl Pts',(-9.12200500521743,5.61649261685196,
11.7851605743406));
#117716=CARTESIAN_POINT('Ctrl Pts',(-9.11139391342923,5.61759563504772,
11.7731309833368));
#117717=CARTESIAN_POINT('Ctrl Pts',(-9.08729801504498,5.62018361430836,
11.7446623925145));
#117718=CARTESIAN_POINT('Ctrl Pts',(-9.07400644845524,5.62167560773698,
11.728067880187));
#117719=CARTESIAN_POINT('Ctrl Pts',(-9.02679999702403,5.62721964048393,
11.6657457450799));
#117720=CARTESIAN_POINT('Ctrl Pts',(-8.99576679502239,5.63136388037159,
11.6179401684105));
#117721=CARTESIAN_POINT('Ctrl Pts',(-8.93380240767638,5.64078503571739,
11.5054078317079));
#117722=CARTESIAN_POINT('Ctrl Pts',(-8.90507110211147,5.64606296086224,
11.4397122252583));
#117723=CARTESIAN_POINT('Ctrl Pts',(-8.87922172893789,5.65180725803288,
11.3620188026973));
#117724=CARTESIAN_POINT('Ctrl Pts',(-8.87609272053191,5.65252540285743,
11.3521845987954));
#117725=CARTESIAN_POINT('Ctrl Pts',(-8.87178113502745,5.65354788576446,
11.3379905846795));
#117726=CARTESIAN_POINT('Ctrl Pts',(-8.87049384548747,5.65385773525799,
11.3336634400313));
#117727=CARTESIAN_POINT('Ctrl Pts',(-8.86827676243306,5.65439944181888,
11.3260509659468));
#117728=CARTESIAN_POINT('Ctrl Pts',(-8.86733632707572,5.65463189194131,
11.3227688400012));
#117729=CARTESIAN_POINT('Ctrl Pts',(-8.8653593561261,5.65512629786925,11.3157541400231));
#117730=CARTESIAN_POINT('Ctrl Pts',(-8.86432695123927,5.65538802059525,
11.3120205042513));
#117731=CARTESIAN_POINT('Ctrl Pts',(-8.86152494302682,5.65610847305291,
11.3016890261951));
#117732=CARTESIAN_POINT('Ctrl Pts',(-8.85979425623234,5.65656506332959,
11.2950806520859));
#117733=CARTESIAN_POINT('Ctrl Pts',(-8.8499763500194,5.6592275670099,11.2562157806712));
#117734=CARTESIAN_POINT('Ctrl Pts',(-8.84319993132417,5.66136758416781,
11.2236402782718));
#117735=CARTESIAN_POINT('Ctrl Pts',(-8.82972323400405,5.66663066304444,
11.1415598179796));
#117736=CARTESIAN_POINT('Ctrl Pts',(-8.82477498280083,5.66970516250638,
11.0918343377936));
#117737=CARTESIAN_POINT('Ctrl Pts',(-8.82043547062653,5.67724548475243,
10.970058594321));
#117738=CARTESIAN_POINT('Ctrl Pts',(-8.8244645630676,5.68171858275261,10.8980995038247));
#117739=CARTESIAN_POINT('Ctrl Pts',(-8.83740660917913,5.6874505835615,10.8109679405071));
#117740=CARTESIAN_POINT('Ctrl Pts',(-8.84011127988951,5.6885119512546,10.7950252994599));
#117741=CARTESIAN_POINT('Ctrl Pts',(-8.84459556137706,5.6900967740084,10.7715363682457));
#117742=CARTESIAN_POINT('Ctrl Pts',(-8.84612291358142,5.69061235351592,
10.7639434125485));
#117743=CARTESIAN_POINT('Ctrl Pts',(-8.84897837222354,5.6915354793211,10.7504384150271));
#117744=CARTESIAN_POINT('Ctrl Pts',(-8.85027743478322,5.6919420974047,10.7445204646237));
#117745=CARTESIAN_POINT('Ctrl Pts',(-8.85167500520383,5.69236622608789,
10.7383803797683));
#117746=CARTESIAN_POINT('Ctrl Pts',(-8.85172799934485,5.69238228933724,
10.7381478816677));
#117747=CARTESIAN_POINT('Ctrl Pts',(-8.85183602870579,5.69241499551592,
10.7376745941957));
#117748=CARTESIAN_POINT('Ctrl Pts',(-8.85189106906718,5.69243163860739,
10.737433806021));
#117749=CARTESIAN_POINT('Ctrl Pts',(-8.85199018141113,5.69246157132207,
10.7370008406896));
#117750=CARTESIAN_POINT('Ctrl Pts',(-8.85203422592418,5.69247486007415,
10.7368086572));
#117751=CARTESIAN_POINT('Ctrl Pts',(-8.85211352745354,5.69249876286179,
10.7364630321335));
#117752=CARTESIAN_POINT('Ctrl Pts',(-8.85214876699141,5.69250937634355,
10.7363095865071));
#117753=CARTESIAN_POINT('Ctrl Pts',(-8.85221221141381,5.69252846969523,
10.7360335803762));
#117754=CARTESIAN_POINT('Ctrl Pts',(-8.85224040516692,5.69253694921186,
10.7359110172968));
#117755=CARTESIAN_POINT('Ctrl Pts',(-8.85229116342918,5.692552205703,10.7356905240883));
#117756=CARTESIAN_POINT('Ctrl Pts',(-8.85231372084538,5.69255898245254,
10.7355925923131));
#117757=CARTESIAN_POINT('Ctrl Pts',(-8.85235433179264,5.69257117682672,
10.7354163852431));
#117758=CARTESIAN_POINT('Ctrl Pts',(-8.85237238080182,5.69257659430843,
10.735338108889));
#117759=CARTESIAN_POINT('Ctrl Pts',(-8.85242127803492,5.69259126518817,
10.735126146597));
#117760=CARTESIAN_POINT('Ctrl Pts',(-8.85245214160332,5.69260051907262,
10.7349924642341));
#117761=CARTESIAN_POINT('Ctrl Pts',(-8.85251250030732,5.69261860430856,
10.7347312349951));
#117762=CARTESIAN_POINT('Ctrl Pts',(-8.85254199335314,5.69262743559395,
10.7346036876289));
#117763=CARTESIAN_POINT('Ctrl Pts',(-8.85259968027501,5.69264469802397,
10.7343544007321));
#117764=CARTESIAN_POINT('Ctrl Pts',(-8.85262787225994,5.69265312910793,
10.7342326607714));
#117765=CARTESIAN_POINT('Ctrl Pts',(-8.85268302251681,5.69266961220141,
10.7339946806596));
#117766=CARTESIAN_POINT('Ctrl Pts',(-8.85270997908106,5.69267766415671,
10.7338784401099));
#117767=CARTESIAN_POINT('Ctrl Pts',(-8.85276272034361,5.69269340881282,
10.7336511692175));
#117768=CARTESIAN_POINT('Ctrl Pts',(-8.85278850349565,5.69270110146426,
10.7335401385183));
#117769=CARTESIAN_POINT('Ctrl Pts',(-8.85283895635133,5.69271614615873,
10.7333230150553));
#117770=CARTESIAN_POINT('Ctrl Pts',(-8.85286362465407,5.69272349815682,
10.7332169219713));
#117771=CARTESIAN_POINT('Ctrl Pts',(-8.85291190296945,5.69273787908416,
10.7330094177831));
#117772=CARTESIAN_POINT('Ctrl Pts',(-8.85293551171732,5.6927449079741,10.7329080063678));
#117773=CARTESIAN_POINT('Ctrl Pts',(-8.85298172302272,5.6927586591927,10.7327096247633));
#117774=CARTESIAN_POINT('Ctrl Pts',(-8.85300432442984,5.69276538148475,
10.7326126543057));
#117775=CARTESIAN_POINT('Ctrl Pts',(-8.85304857024886,5.69277853504223,
10.7324229281797));
#117776=CARTESIAN_POINT('Ctrl Pts',(-8.85307021361671,5.69278496627449,
10.7323301722665));
#117777=CARTESIAN_POINT('Ctrl Pts',(-8.85311258982465,5.69279755233854,
10.7321486621492));
#117778=CARTESIAN_POINT('Ctrl Pts',(-8.85313332171459,5.69280370713969,
10.7320599077299));
#117779=CARTESIAN_POINT('Ctrl Pts',(-8.85317391884307,5.6928157541103,10.7318862001128));
#117780=CARTESIAN_POINT('Ctrl Pts',(-8.8531937832242,5.69282164625379,10.7318012466918));
#117781=CARTESIAN_POINT('Ctrl Pts',(-8.85323268682015,5.69283318088917,
10.7316349521619));
#117782=CARTESIAN_POINT('Ctrl Pts',(-8.8532517252439,5.69283882335418,10.7315536108964));
#117783=CARTESIAN_POINT('Ctrl Pts',(-8.85328901609544,5.69284987085508,
10.7313943628751));
#117784=CARTESIAN_POINT('Ctrl Pts',(-8.85330726781337,5.69285527586961,
10.7313164559319));
#117785=CARTESIAN_POINT('Ctrl Pts',(-8.85334302230932,5.6928658600014,10.7311639088761));
#117786=CARTESIAN_POINT('Ctrl Pts',(-8.85336052443384,5.69287103909722,
10.7310892686209));
#117787=CARTESIAN_POINT('Ctrl Pts',(-8.85339481476514,5.69288118226336,
10.7309430969272));
#117788=CARTESIAN_POINT('Ctrl Pts',(-8.85341160238164,5.69288614631579,
10.7308715653344));
#117789=CARTESIAN_POINT('Ctrl Pts',(-8.85512552386732,5.69339276800916,
10.7235716620517));
#117790=CARTESIAN_POINT('Ctrl Pts',(-8.85689093365318,5.69389658491991,
10.7163596464042));
#117791=CARTESIAN_POINT('Ctrl Pts',(-8.8626508373448,5.69548619623917,10.6937570146164));
#117792=CARTESIAN_POINT('Ctrl Pts',(-8.86688873745678,5.6965796559959,10.678430866149));
#117793=CARTESIAN_POINT('Ctrl Pts',(-8.87750057083868,5.69915438054011,
10.6428726980765));
#117794=CARTESIAN_POINT('Ctrl Pts',(-8.88411323373964,5.70064277244283,
10.6227182653889));
#117795=CARTESIAN_POINT('Ctrl Pts',(-8.91038803138248,5.70616623493076,
10.5493838898778));
#117796=CARTESIAN_POINT('Ctrl Pts',(-8.933336674925,5.71029275195161,10.4974691831022));
#117797=CARTESIAN_POINT('Ctrl Pts',(-8.99364865311626,5.71971933949734,
10.3839509507372));
#117798=CARTESIAN_POINT('Ctrl Pts',(-9.03310678545581,5.72502147709497,
10.3237021884467));
#117799=CARTESIAN_POINT('Ctrl Pts',(-9.08423912071204,5.7307886061424,10.2593356009091));
#117800=CARTESIAN_POINT('Ctrl Pts',(-9.09076996775819,5.73150741546516,
10.2513328465132));
#117801=CARTESIAN_POINT('Ctrl Pts',(-9.10030663316379,5.73253066636257,
10.2399557229522));
#117802=CARTESIAN_POINT('Ctrl Pts',(-9.1032276877866,5.73284063040539,10.236511375897));
#117803=CARTESIAN_POINT('Ctrl Pts',(-9.10839187321157,5.73338246695969,
10.2304925805417));
#117804=CARTESIAN_POINT('Ctrl Pts',(-9.1106264920798,5.73361493344824,10.2279109604706));
#117805=CARTESIAN_POINT('Ctrl Pts',(-9.11541965957674,5.73410929384367,
10.2224219127305));
#117806=CARTESIAN_POINT('Ctrl Pts',(-9.11798134673244,5.73437095528417,
10.2195173564808));
#117807=CARTESIAN_POINT('Ctrl Pts',(-9.12509806049707,5.7350910618468,10.2115278941836));
#117808=CARTESIAN_POINT('Ctrl Pts',(-9.12968312862919,5.73554737088737,
10.2064697773408));
#117809=CARTESIAN_POINT('Ctrl Pts',(-9.15677638885022,5.738201483049,10.1770985948259));
#117810=CARTESIAN_POINT('Ctrl Pts',(-9.18026071028634,5.74033388788059,
10.1537017519244));
#117811=CARTESIAN_POINT('Ctrl Pts',(-9.2362193271707,5.74513504297883,10.1024700526257));
#117812=CARTESIAN_POINT('Ctrl Pts',(-9.26928434523316,5.74777729970631,
10.0753509281711));
#117813=CARTESIAN_POINT('Ctrl Pts',(-9.34543318703334,5.75361769611662,
10.0195368060908));
#117814=CARTESIAN_POINT('Ctrl Pts',(-9.3890789741614,5.75681132730609,9.99176347828966));
#117815=CARTESIAN_POINT('Ctrl Pts',(-9.46657858128663,5.76240643889298,
9.94933256948704));
#117816=CARTESIAN_POINT('Ctrl Pts',(-9.49955429327655,5.76476497861299,
9.93323191524651));
#117817=CARTESIAN_POINT('Ctrl Pts',(-9.54314932008757,5.76788657375813,
9.91441289538316));
#117818=CARTESIAN_POINT('Ctrl Pts',(-9.55313174890669,5.76860151782906,
9.91026578519691));
#117819=CARTESIAN_POINT('Ctrl Pts',(-9.56934020589601,5.769763331187,9.90379228493961));
#117820=CARTESIAN_POINT('Ctrl Pts',(-9.57553146730357,5.7702073390646,9.90138010462552));
#117821=CARTESIAN_POINT('Ctrl Pts',(-9.58743144646808,5.77106133528235,
9.89685935465352));
#117822=CARTESIAN_POINT('Ctrl Pts',(-9.59313676059736,5.77147103007217,
9.89474238441067));
#117823=CARTESIAN_POINT('Ctrl Pts',(-9.60443976780258,5.77228330594148,
9.890647752811));
#117824=CARTESIAN_POINT('Ctrl Pts',(-9.61003651976814,5.77268580439191,
9.88866801202665));
#117825=CARTESIAN_POINT('Ctrl Pts',(-9.6229648189787,5.77361634095547,9.88420456478332));
#117826=CARTESIAN_POINT('Ctrl Pts',(-9.63030629636242,5.77414533087923,
9.88175068007574));
#117827=CARTESIAN_POINT('Ctrl Pts',(-9.65663557767925,5.77604480715797,
9.87323774572988));
#117828=CARTESIAN_POINT('Ctrl Pts',(-9.67575140967261,5.77742824655517,
9.86758882331491));
#117829=CARTESIAN_POINT('Ctrl Pts',(-9.73327922432616,5.78160631487507,
9.85216478097923));
#117830=CARTESIAN_POINT('Ctrl Pts',(-9.77203822195782,5.78444156898681,
9.84384320035442));
#117831=CARTESIAN_POINT('Ctrl Pts',(-9.81114942708339,5.78731516233854,
9.83748955978492));
#117832=CARTESIAN_POINT('Origin',(-10.,2.67563288526385,11.));
#117833=CARTESIAN_POINT('',(-9.81114930150155,6.38739526456853,9.83748958018577));
#117834=CARTESIAN_POINT('',(-9.81114930150541,6.28889384320256,9.83748958018515));
#117835=CARTESIAN_POINT('',(-9.81114930150157,2.67563288526385,9.83748958018577));
#117836=CARTESIAN_POINT('',(-9.81108652115608,6.38739074626474,9.83749978064041));
#117837=CARTESIAN_POINT('Ctrl Pts',(-9.81114930150153,6.38739526456853,
9.83748958018578));
#117838=CARTESIAN_POINT('Ctrl Pts',(-9.811125092701,6.38739352228488,9.83749351292377));
#117839=CARTESIAN_POINT('Ctrl Pts',(-9.81111072975194,6.3873924885829,9.83749584659379));
#117840=CARTESIAN_POINT('Ctrl Pts',(-9.81108652115608,6.38739074626474,
9.83749978064041));
#117841=CARTESIAN_POINT('Ctrl Pts',(-9.81108652115747,6.38739074626483,
9.83749978064019));
#117842=CARTESIAN_POINT('Ctrl Pts',(-9.70629422173851,6.37984873400106,
9.85452917771854));
#117843=CARTESIAN_POINT('Ctrl Pts',(-9.60431432144809,6.37191206627698,
9.88564185940446));
#117844=CARTESIAN_POINT('Ctrl Pts',(-9.49156845948395,6.36298003618431,
9.93749594515914));
#117845=CARTESIAN_POINT('Ctrl Pts',(-9.47542747424803,6.36169889764369,
9.94537151866597));
#117846=CARTESIAN_POINT('Ctrl Pts',(-9.44872567109751,6.35958243714402,
9.95916476905495));
#117847=CARTESIAN_POINT('Ctrl Pts',(-9.43806489731962,6.35873824085316,
9.9648814886998));
#117848=CARTESIAN_POINT('Ctrl Pts',(-9.42324552134241,6.35756778761629,
9.97312466021357));
#117849=CARTESIAN_POINT('Ctrl Pts',(-9.41901203223011,6.35723377635244,
9.97551394567556));
#117850=CARTESIAN_POINT('Ctrl Pts',(-9.41179450552945,6.35666509762935,
9.97964648272454));
#117851=CARTESIAN_POINT('Ctrl Pts',(-9.40880315382429,6.35642963396348,
9.98137676529053));
#117852=CARTESIAN_POINT('Ctrl Pts',(-9.40258119724893,6.35594040726098,
9.98501236339502));
#117853=CARTESIAN_POINT('Ctrl Pts',(-9.39935202901517,6.35568679161012,
9.98691997143284));
#117854=CARTESIAN_POINT('Ctrl Pts',(-9.39075257741571,6.35501202541322,
9.99205560705719));
#117855=CARTESIAN_POINT('Ctrl Pts',(-9.38539875879872,6.3545925878495,9.99531117265904));
#117856=CARTESIAN_POINT('Ctrl Pts',(-9.36158592312661,6.35272875821254,
10.0100529393856));
#117857=CARTESIAN_POINT('Ctrl Pts',(-9.34341980893909,6.35131162651471,
10.0220069983552));
#117858=CARTESIAN_POINT('Ctrl Pts',(-9.24218941974319,6.34337931952056,
10.0927138219315));
#117859=CARTESIAN_POINT('Ctrl Pts',(-9.16667897359472,6.33728876670943,
10.1615341306614));
#117860=CARTESIAN_POINT('Ctrl Pts',(-9.0830571195697,6.3291261256659,10.2603528021599));
#117861=CARTESIAN_POINT('Ctrl Pts',(-9.06591773062386,6.32736092092334,
10.2821195240132));
#117862=CARTESIAN_POINT('Ctrl Pts',(-9.04163329601515,6.32469961721259,
10.3153040171819));
#117863=CARTESIAN_POINT('Ctrl Pts',(-9.0338903865228,6.32382455549247,10.3262734082767));
#117864=CARTESIAN_POINT('Ctrl Pts',(-9.02012551203901,6.32221755088553,
10.3464994759808));
#117865=CARTESIAN_POINT('Ctrl Pts',(-9.0140429147898,6.32148788943906,10.3557131386691));
#117866=CARTESIAN_POINT('Ctrl Pts',(-9.00455913802206,6.32031769091186,
10.3705276314881));
#117867=CARTESIAN_POINT('Ctrl Pts',(-9.00107352058646,6.31988025688667,
10.3760738359218));
#117868=CARTESIAN_POINT('Ctrl Pts',(-8.99446021896994,6.31903583900708,
10.3867941924002));
#117869=CARTESIAN_POINT('Ctrl Pts',(-8.99132574703084,6.31862911824801,
10.3919639297122));
#117870=CARTESIAN_POINT('Ctrl Pts',(-8.9843397606953,6.31770765838549,10.4036887208888));
#117871=CARTESIAN_POINT('Ctrl Pts',(-8.98051166841585,6.31719210068422,
10.4102573439408));
#117872=CARTESIAN_POINT('Ctrl Pts',(-8.96911428319043,6.31562414332695,
10.4302567463196));
#117873=CARTESIAN_POINT('Ctrl Pts',(-8.9617451120734,6.31456476942986,10.4437990606441));
#117874=CARTESIAN_POINT('Ctrl Pts',(-8.91330230911327,6.30727536796872,
10.5371414518518));
#117875=CARTESIAN_POINT('Ctrl Pts',(-8.88120873676352,6.30073476276135,
10.6212518246503));
#117876=CARTESIAN_POINT('Ctrl Pts',(-8.84773275981184,6.29082032112359,
10.7521391615196));
#117877=CARTESIAN_POINT('Ctrl Pts',(-8.8390374445294,6.28749335510108,10.7967238379003));
#117878=CARTESIAN_POINT('Ctrl Pts',(-8.82990514995668,6.28262746781723,
10.8640520316427));
#117879=CARTESIAN_POINT('Ctrl Pts',(-8.82751597898316,6.28103227993347,
10.8864870544646));
#117880=CARTESIAN_POINT('Ctrl Pts',(-8.82530126139607,6.27904486070874,
10.9150581385752));
#117881=CARTESIAN_POINT('Ctrl Pts',(-8.82487720426123,6.2786242325543,10.9211414859415));
#117882=CARTESIAN_POINT('Ctrl Pts',(-8.82427095523865,6.27795147363083,
10.9309343406105));
#117883=CARTESIAN_POINT('Ctrl Pts',(-8.82405903284976,6.27769777966777,
10.9346417966469));
#117884=CARTESIAN_POINT('Ctrl Pts',(-8.82368491539028,6.27721139947143,
10.9417790976713));
#117885=CARTESIAN_POINT('Ctrl Pts',(-8.82352017975578,6.27697858525491,
10.9452087175666));
#117886=CARTESIAN_POINT('Ctrl Pts',(-8.82318906649482,6.27646556313903,
10.9527942006495));
#117887=CARTESIAN_POINT('Ctrl Pts',(-8.82302969835505,6.27618573541428,
10.9569503652164));
#117888=CARTESIAN_POINT('Ctrl Pts',(-8.82254172955023,6.27519559324589,
10.9717190176507));
#117889=CARTESIAN_POINT('Ctrl Pts',(-8.82233460898579,6.27449154925881,
10.9823353824679));
#117890=CARTESIAN_POINT('Ctrl Pts',(-8.8219044584418,6.26976718149439,11.0542297909788));
#117891=CARTESIAN_POINT('Ctrl Pts',(-8.82632060487794,6.26595504163347,
11.1154494459901));
#117892=CARTESIAN_POINT('Ctrl Pts',(-8.84163327647415,6.25961129438993,
11.2167359195588));
#117893=CARTESIAN_POINT('Ctrl Pts',(-8.84991122505178,6.25707572594225,
11.2570674084187));
#117894=CARTESIAN_POINT('Ctrl Pts',(-8.87395575485386,6.25111862635543,
11.3493732868182));
#117895=CARTESIAN_POINT('Ctrl Pts',(-8.8912372515358,6.24767731413254,11.4008508397926));
#117896=CARTESIAN_POINT('Ctrl Pts',(-8.91645632861289,6.24335499839081,
11.4616963125574));
#117897=CARTESIAN_POINT('Ctrl Pts',(-8.92106905669942,6.24258666608632,
11.4723752498627));
#117898=CARTESIAN_POINT('Ctrl Pts',(-8.92863748940995,6.24135920285288,
11.489207521536));
#117899=CARTESIAN_POINT('Ctrl Pts',(-8.93148989452805,6.24090355951913,
11.495406680848));
#117900=CARTESIAN_POINT('Ctrl Pts',(-8.93697196258465,6.2400405667787,11.5070532914514));
#117901=CARTESIAN_POINT('Ctrl Pts',(-8.9395900445429,6.23963362339906,11.5125059733628));
#117902=CARTESIAN_POINT('Ctrl Pts',(-8.94560690027989,6.2387098301773,11.5247937903583));
#117903=CARTESIAN_POINT('Ctrl Pts',(-8.94903033056707,6.23819214482194,
11.5316164786036));
#117904=CARTESIAN_POINT('Ctrl Pts',(-8.9594032863729,6.2366463961322,11.55179731025));
#117905=CARTESIAN_POINT('Ctrl Pts',(-8.9665427019263,6.23561180301538,11.5650555448208));
#117906=CARTESIAN_POINT('Ctrl Pts',(-9.01907436029362,6.22819677966362,
11.6582819130233));
#117907=CARTESIAN_POINT('Ctrl Pts',(-9.07343307562128,6.22148788494853,
11.7328148973178));
#117908=CARTESIAN_POINT('Ctrl Pts',(-9.1773578505369,6.21026489252221,11.8450323391692));
#117909=CARTESIAN_POINT('Ctrl Pts',(-9.22224890338372,6.20579768160234,
11.8865238654787));
#117910=CARTESIAN_POINT('Ctrl Pts',(-9.27724317159866,6.20089698559862,
11.9299457598515));
#117911=CARTESIAN_POINT('Ctrl Pts',(-9.28439232458486,6.20027021996111,
11.9354582922272));
#117912=CARTESIAN_POINT('Ctrl Pts',(-9.29506001281054,6.19935095590464,
11.943490003677));
#117913=CARTESIAN_POINT('Ctrl Pts',(-9.29852998299973,6.19905439652207,
11.946072718832));
#117914=CARTESIAN_POINT('Ctrl Pts',(-9.30448243049094,6.19854996474648,
11.9504523993803));
#117915=CARTESIAN_POINT('Ctrl Pts',(-9.3069577816837,6.19834145450866,11.9522588605016));
#117916=CARTESIAN_POINT('Ctrl Pts',(-9.31261301546616,6.19786796688682,
11.9563522030986));
#117917=CARTESIAN_POINT('Ctrl Pts',(-9.31579727962397,6.19760340783684,
11.9586329023276));
#117918=CARTESIAN_POINT('Ctrl Pts',(-9.32457472648706,6.1968795678452,11.9648536512827));
#117919=CARTESIAN_POINT('Ctrl Pts',(-9.33019106076757,6.19642240951869,
11.9687609916347));
#117920=CARTESIAN_POINT('Ctrl Pts',(-9.360758868145,6.19396462558051,11.9896343959691));
#117921=CARTESIAN_POINT('Ctrl Pts',(-9.38632353872697,6.19201756019995,
12.0056873314156));
#117922=CARTESIAN_POINT('Ctrl Pts',(-9.46857154385732,6.18599384250776,
12.0530278343754));
#117923=CARTESIAN_POINT('Ctrl Pts',(-9.52723302750387,6.18203637754222,
12.0806369383949));
#117924=CARTESIAN_POINT('Ctrl Pts',(-9.64690685357045,6.17410845601267,
12.1253408998996));
#117925=CARTESIAN_POINT('Ctrl Pts',(-9.70761252432059,6.17015287263634,
12.142617627114));
#117926=CARTESIAN_POINT('Ctrl Pts',(-9.78341873219423,6.16510613487855,
12.1577529330576));
#117927=CARTESIAN_POINT('Ctrl Pts',(-9.79748253232348,6.16416580695201,
12.1602956287908));
#117928=CARTESIAN_POINT('Ctrl Pts',(-9.81887412787079,6.16272776976035,
12.1637624127615));
#117929=CARTESIAN_POINT('Ctrl Pts',(-9.82617041122119,6.16223592465893,
12.1648745875945));
#117930=CARTESIAN_POINT('Ctrl Pts',(-9.83944562195321,6.16133835370048,
12.1667706334527));
#117931=CARTESIAN_POINT('Ctrl Pts',(-9.84542107699788,6.16093335351449,
12.167577309497));
#117932=CARTESIAN_POINT('Ctrl Pts',(-9.85835005048697,6.16005481325003,
12.1692217092685));
#117933=CARTESIAN_POINT('Ctrl Pts',(-9.86530534269043,6.15958078922281,
12.1700433578527));
#117934=CARTESIAN_POINT('Ctrl Pts',(-9.88433464202471,6.1582798489739,12.1721194215927));
#117935=CARTESIAN_POINT('Ctrl Pts',(-9.89642108615721,6.1574491176511,12.1732492501675));
#117936=CARTESIAN_POINT('Ctrl Pts',(-9.9729680335276,6.15215804231381,12.1792127781107));
#117937=CARTESIAN_POINT('Ctrl Pts',(-10.0377067570292,6.14754052359055,
12.1789186618631));
#117938=CARTESIAN_POINT('Ctrl Pts',(-10.1710445990236,6.13778864143651,
12.167317529738));
#117939=CARTESIAN_POINT('Ctrl Pts',(-10.2393399837693,6.13265920832274,
12.1552501402892));
#117940=CARTESIAN_POINT('Ctrl Pts',(-10.3244485035658,6.12630571835054,
12.1323365883588));
#117941=CARTESIAN_POINT('Ctrl Pts',(-10.3425966403301,6.12495397033817,
12.1269785282937));
#117942=CARTESIAN_POINT('Ctrl Pts',(-10.3725727336541,6.12273439176715,
12.1173372651871));
#117943=CARTESIAN_POINT('Ctrl Pts',(-10.3844749519752,6.12185662009324,
12.1132978258146));
#117944=CARTESIAN_POINT('Ctrl Pts',(-10.4009575402082,6.12064811768897,
12.1074079928679));
#117945=CARTESIAN_POINT('Ctrl Pts',(-10.4055938967586,6.12030896742988,
12.1057183207342));
#117946=CARTESIAN_POINT('Ctrl Pts',(-10.4134709318236,6.11973426652526,
12.1027914044581));
#117947=CARTESIAN_POINT('Ctrl Pts',(-10.4167169836809,6.11949787715479,
12.1015689038777));
#117948=CARTESIAN_POINT('Ctrl Pts',(-10.4234353573576,6.11900959176672,
12.099004739103));
#117949=CARTESIAN_POINT('Ctrl Pts',(-10.4269067770909,6.11875782237371,
12.0976609326531));
#117950=CARTESIAN_POINT('Ctrl Pts',(-10.4360856578786,6.11809337082034,
12.0940576039124));
#117951=CARTESIAN_POINT('Ctrl Pts',(-10.4417820176929,6.11768231092122,
12.0917698450513));
#117952=CARTESIAN_POINT('Ctrl Pts',(-10.4664961426038,6.11590345518523,
12.0816191105415));
#117953=CARTESIAN_POINT('Ctrl Pts',(-10.4853251086725,6.11455999829749,
12.0733024795324));
#117954=CARTESIAN_POINT('Ctrl Pts',(-10.596999059492,6.10660738205377,12.0204365229945));
#117955=CARTESIAN_POINT('Ctrl Pts',(-10.6838971370887,6.10044786928515,
11.9643585897023));
#117956=CARTESIAN_POINT('Ctrl Pts',(-10.7835859986464,6.09220195164302,
11.8796935140586));
#117957=CARTESIAN_POINT('Ctrl Pts',(-10.8041275965974,6.09043068872284,
11.8609566443414));
#117958=CARTESIAN_POINT('Ctrl Pts',(-10.8380157696309,6.08736140424382,
11.8277742309498));
#117959=CARTESIAN_POINT('Ctrl Pts',(-10.8516989095593,6.08607765539683,
11.8136888246224));
#117960=CARTESIAN_POINT('Ctrl Pts',(-10.8706946591815,6.08422611440667,
11.7931303294171));
#117961=CARTESIAN_POINT('Ctrl Pts',(-10.8763007186664,6.08367064232529,
11.7869319878202));
#117962=CARTESIAN_POINT('Ctrl Pts',(-10.8859154404189,6.08270177586815,
11.7760713194669));
#117963=CARTESIAN_POINT('Ctrl Pts',(-10.8899544872706,6.08228965374864,
11.7714362375604));
#117964=CARTESIAN_POINT('Ctrl Pts',(-10.8981801593538,6.081439623963,11.7618461403508));
#117965=CARTESIAN_POINT('Ctrl Pts',(-10.9023625000221,6.08100156215505,
11.7568877432476));
#117966=CARTESIAN_POINT('Ctrl Pts',(-10.9129333354446,6.07987908813245,
11.7441432794363));
#117967=CARTESIAN_POINT('Ctrl Pts',(-10.9192631972995,6.07919237201247,
11.7363094855211));
#117968=CARTESIAN_POINT('Ctrl Pts',(-10.9439864918241,6.07645070848699,
11.7048963358474));
#117969=CARTESIAN_POINT('Ctrl Pts',(-10.9615780516534,6.07436525955523,
11.6807031041947));
#117970=CARTESIAN_POINT('Ctrl Pts',(-11.0294744998208,6.06573414008526,
11.5794354614752));
#117971=CARTESIAN_POINT('Ctrl Pts',(-11.0715807899662,6.05892008917143,
11.4972660251621));
#117972=CARTESIAN_POINT('Ctrl Pts',(-11.1175036907816,6.04932392050498,
11.3739613752723));
#117973=CARTESIAN_POINT('Ctrl Pts',(-11.1294405004094,6.04646795035366,
11.3361939740255));
#117974=CARTESIAN_POINT('Ctrl Pts',(-11.1418431774274,6.04303491028879,
11.2887533171767));
#117975=CARTESIAN_POINT('Ctrl Pts',(-11.1441228329361,6.04237842695314,
11.2795841147672));
#117976=CARTESIAN_POINT('Ctrl Pts',(-11.1473033681052,6.04142430431516,
11.266100452843));
#117977=CARTESIAN_POINT('Ctrl Pts',(-11.1482907015608,6.04112216282071,
11.2618070582505));
#117978=CARTESIAN_POINT('Ctrl Pts',(-11.1499961159496,6.04058959787017,
11.2541958261614));
#117979=CARTESIAN_POINT('Ctrl Pts',(-11.150723971087,6.04035864070637,11.2508803063934));
#117980=CARTESIAN_POINT('Ctrl Pts',(-11.1522768610569,6.03985777636539,
11.2436576349092));
#117981=CARTESIAN_POINT('Ctrl Pts',(-11.1530963675353,6.03958817792172,
11.2397494023623));
#117982=CARTESIAN_POINT('Ctrl Pts',(-11.1553337788786,6.03883680301431,
11.2288022654326));
#117983=CARTESIAN_POINT('Ctrl Pts',(-11.1567072447311,6.03835742072707,
11.22175430904));
#117984=CARTESIAN_POINT('Ctrl Pts',(-11.1646265435953,6.03547599864402,
11.1790392091209));
#117985=CARTESIAN_POINT('Ctrl Pts',(-11.1695873791818,6.03315178173758,
11.1430941929195));
#117986=CARTESIAN_POINT('Ctrl Pts',(-11.1830507830697,6.02380828805878,
10.995479029044));
#117987=CARTESIAN_POINT('Ctrl Pts',(-11.1772710642939,6.01710399785173,
10.883107957809));
#117988=CARTESIAN_POINT('Ctrl Pts',(-11.15177936822,6.00854620343227,10.7531864146719));
#117989=CARTESIAN_POINT('Ctrl Pts',(-11.1473238032225,6.00721130635091,
10.7332404282512));
#117990=CARTESIAN_POINT('Ctrl Pts',(-11.1402866442378,6.0052989923684,10.7051891003853));
#117991=CARTESIAN_POINT('Ctrl Pts',(-11.138132560821,6.00473505819836,10.6969795958973));
#117992=CARTESIAN_POINT('Ctrl Pts',(-11.1342595724544,6.00375625404548,
10.6828433246477));
#117993=CARTESIAN_POINT('Ctrl Pts',(-11.1325824488133,6.0033427313431,10.6769053875374));
#117994=CARTESIAN_POINT('Ctrl Pts',(-11.1292722071328,6.00254569599005,
10.6655278810401));
#117995=CARTESIAN_POINT('Ctrl Pts',(-11.1276462458137,6.00216242366987,
10.6600863955035));
#117996=CARTESIAN_POINT('Ctrl Pts',(-11.1237142616486,6.00125442002403,
10.6472662744635));
#117997=CARTESIAN_POINT('Ctrl Pts',(-11.1213748436088,6.00072862286135,
10.6398982391766));
#117998=CARTESIAN_POINT('Ctrl Pts',(-11.1128600091068,5.99886394203865,
10.6139684874737));
#117999=CARTESIAN_POINT('Ctrl Pts',(-11.1062951536931,5.99751256811168,
10.5955390223871));
#118000=CARTESIAN_POINT('Ctrl Pts',(-11.0577356971366,5.9880659199627,10.469260400461));
#118001=CARTESIAN_POINT('Ctrl Pts',(-11.0005034541431,5.97944263925819,
10.3679620832917));
#118002=CARTESIAN_POINT('Ctrl Pts',(-10.9086570334226,5.968605568674,10.2499441843482));
#118003=CARTESIAN_POINT('Ctrl Pts',(-10.8867187140578,5.96618430723135,
10.2241316361699));
#118004=CARTESIAN_POINT('Ctrl Pts',(-10.8590302048183,5.96335277436182,
10.1942647598513));
#118005=CARTESIAN_POINT('Ctrl Pts',(-10.8543199605625,5.96287840483543,
10.1892721907946));
#118006=CARTESIAN_POINT('Ctrl Pts',(-10.8468780511222,5.962140677148,10.1815211094861));
#118007=CARTESIAN_POINT('Ctrl Pts',(-10.8441760278416,5.96187519937299,
10.1787345357308));
#118008=CARTESIAN_POINT('Ctrl Pts',(-10.8390717898062,5.96137823466725,
10.1735223856035));
#118009=CARTESIAN_POINT('Ctrl Pts',(-10.8366728139832,5.96114653026263,
10.1710939026464));
#118010=CARTESIAN_POINT('Ctrl Pts',(-10.8310838448612,5.9606109700974,10.1654851746107));
#118011=CARTESIAN_POINT('Ctrl Pts',(-10.8278861247826,5.96030771746657,
10.1623127570297));
#118012=CARTESIAN_POINT('Ctrl Pts',(-10.8173475005805,5.95931829342201,
10.151976811946));
#118013=CARTESIAN_POINT('Ctrl Pts',(-10.8099309719718,5.95863771457508,
10.144890590444));
#118014=CARTESIAN_POINT('Ctrl Pts',(-10.7495441853622,5.95321181468442,
10.0886838601736));
#118015=CARTESIAN_POINT('Ctrl Pts',(-10.692242036395,5.94876058173987,10.0444282099289));
#118016=CARTESIAN_POINT('Ctrl Pts',(-10.5835458903057,5.94079626491515,
9.97542178330105));
#118017=CARTESIAN_POINT('Ctrl Pts',(-10.5337394266677,5.937301350591,9.94861617554074));
#118018=CARTESIAN_POINT('Ctrl Pts',(-10.4628930425399,5.93235473993236,
9.9168226588763));
#118019=CARTESIAN_POINT('Ctrl Pts',(-10.4433519336298,5.93099333191455,
9.90867873434603));
#118020=CARTESIAN_POINT('Ctrl Pts',(-10.4086849019479,5.92857495945463,
9.8953157353362));
#118021=CARTESIAN_POINT('Ctrl Pts',(-10.3936520492041,5.92752527597006,
9.88986996340276));
#118022=CARTESIAN_POINT('Ctrl Pts',(-10.3712106766067,5.92595449166869,
9.8822535298701));
#118023=CARTESIAN_POINT('Ctrl Pts',(-10.3638837659836,5.92544105913767,
9.87984682384738));
#118024=CARTESIAN_POINT('Ctrl Pts',(-10.3507613863413,5.92452021417186,
9.87567878436805));
#118025=CARTESIAN_POINT('Ctrl Pts',(-10.3449749183962,5.92411371098358,
9.87388985911269));
#118026=CARTESIAN_POINT('Ctrl Pts',(-10.3326857641733,5.92324932245628,
9.87019419222461));
#118027=CARTESIAN_POINT('Ctrl Pts',(-10.3261799266074,5.92279108867051,
9.86829878804781));
#118028=CARTESIAN_POINT('Ctrl Pts',(-10.3086745537846,5.92155623859653,
9.86336227544526));
#118029=CARTESIAN_POINT('Ctrl Pts',(-10.2976468070993,5.92077634841056,
9.86042478994145));
#118030=CARTESIAN_POINT('Ctrl Pts',(-10.2436175470539,5.91694453892045,
9.84687062917507));
#118031=CARTESIAN_POINT('Ctrl Pts',(-10.2000881977963,5.91382215544051,
9.83852649164516));
#118032=CARTESIAN_POINT('Ctrl Pts',(-10.0834333548866,5.90536608682455,
9.82291747677267));
#118033=CARTESIAN_POINT('Ctrl Pts',(-10.009922120106,5.89993789865148,9.82000658530401));
#118034=CARTESIAN_POINT('Ctrl Pts',(-9.90637557113827,5.89236928612994,
9.82558639901517));
#118035=CARTESIAN_POINT('Ctrl Pts',(-9.87619670925931,5.89017484800594,
9.82838324284337));
#118036=CARTESIAN_POINT('Ctrl Pts',(-9.83446346949928,5.88718191571037,
9.83388171966526));
#118037=CARTESIAN_POINT('Ctrl Pts',(-9.82279274497268,5.88634954765775,
9.835598093972));
#118038=CARTESIAN_POINT('Ctrl Pts',(-9.81114930150087,5.88552497076973,
9.83748958018588));
#118039=CARTESIAN_POINT('Ctrl Pts',(-9.81114942708287,5.78731516233851,
9.837489559785));
#118040=CARTESIAN_POINT('Ctrl Pts',(-9.90947160064604,5.79453912650356,
9.82151705909552));
#118041=CARTESIAN_POINT('Ctrl Pts',(-10.0094102735156,5.80199718996431,
9.8180824094726));
#118042=CARTESIAN_POINT('Ctrl Pts',(-10.1158737937996,5.80950143692189,
9.82794125172127));
#118043=CARTESIAN_POINT('Ctrl Pts',(-10.1231428226069,5.81001136187773,
9.82868266597279));
#118044=CARTESIAN_POINT('Ctrl Pts',(-10.1364257823334,5.8109381422852,9.83016250190705));
#118045=CARTESIAN_POINT('Ctrl Pts',(-10.1424417717871,5.81135600042542,
9.83087977025029));
#118046=CARTESIAN_POINT('Ctrl Pts',(-10.1521266188609,5.81202535872896,
9.83211033300425));
#118047=CARTESIAN_POINT('Ctrl Pts',(-10.1557989617142,5.81227839549757,
9.83259455760698));
#118048=CARTESIAN_POINT('Ctrl Pts',(-10.1628740332343,5.81276432143749,
9.83356143649753));
#118049=CARTESIAN_POINT('Ctrl Pts',(-10.1662770028275,5.81299733261119,
9.83404166807149));
#118050=CARTESIAN_POINT('Ctrl Pts',(-10.1738091880881,5.81351159877274,
9.83513826644664));
#118051=CARTESIAN_POINT('Ctrl Pts',(-10.1779373689123,5.81379246602502,
9.83576171415851));
#118052=CARTESIAN_POINT('Ctrl Pts',(-10.1922349074714,5.81476206868853,
9.83799878668286));
#118053=CARTESIAN_POINT('Ctrl Pts',(-10.2023867043277,5.81544498728578,
9.8397238609111));
#118054=CARTESIAN_POINT('Ctrl Pts',(-10.2801247790684,5.82064096924409,
9.85398512492233));
#118055=CARTESIAN_POINT('Ctrl Pts',(-10.3465284807465,5.82488919782711,
9.87228525326674));
#118056=CARTESIAN_POINT('Ctrl Pts',(-10.4660855137594,5.83278156314981,
9.91680147391089));
#118057=CARTESIAN_POINT('Ctrl Pts',(-10.5195891101423,5.83641337635526,
9.94142487387269));
#118058=CARTESIAN_POINT('Ctrl Pts',(-10.5899678887931,5.84153504657397,
9.98044032716379));
#118059=CARTESIAN_POINT('Ctrl Pts',(-10.6086139186056,5.8429268475616,9.99145994123044));
#118060=CARTESIAN_POINT('Ctrl Pts',(-10.6405808342553,5.84538366108026,
10.0115614719147));
#118061=CARTESIAN_POINT('Ctrl Pts',(-10.6540389683504,5.84644077711937,
10.0204146201527));
#118062=CARTESIAN_POINT('Ctrl Pts',(-10.673259961579,5.84798634290642,10.0336314297363));
#118063=CARTESIAN_POINT('Ctrl Pts',(-10.6791712632499,5.84846670142559,
10.0377767510773));
#118064=CARTESIAN_POINT('Ctrl Pts',(-10.6851680254147,5.84895929271713,
10.0420647920094));
#118065=CARTESIAN_POINT('Ctrl Pts',(-10.6852920634587,5.84896948388425,
10.0421535229907));
#118066=CARTESIAN_POINT('Ctrl Pts',(-10.6855475884722,5.84899048302827,
10.042336388605));
#118067=CARTESIAN_POINT('Ctrl Pts',(-10.6856790732958,5.84900129111814,
10.0424305262309));
#118068=CARTESIAN_POINT('Ctrl Pts',(-10.6859504176161,5.84902360110197,
10.0426248819419));
#118069=CARTESIAN_POINT('Ctrl Pts',(-10.6860902745437,5.84903510313059,
10.0427251035983));
#118070=CARTESIAN_POINT('Ctrl Pts',(-10.6863794437516,5.84905889094312,
10.0429324185521));
#118071=CARTESIAN_POINT('Ctrl Pts',(-10.686528752931,5.84907117688871,10.0430395161439));
#118072=CARTESIAN_POINT('Ctrl Pts',(-10.6916040110387,5.8494889109615,10.0466817339086));
#118073=CARTESIAN_POINT('Ctrl Pts',(-10.6965025329501,5.84989578610632,
10.050254747946));
#118074=CARTESIAN_POINT('Ctrl Pts',(-10.7067823119526,5.85075758464687,
10.0578751869046));
#118075=CARTESIAN_POINT('Ctrl Pts',(-10.7121568676708,5.85121283065427,
10.0619312431805));
#118076=CARTESIAN_POINT('Ctrl Pts',(-10.7263929426214,5.85243140557028,
10.0728677446094));
#118077=CARTESIAN_POINT('Ctrl Pts',(-10.7351912427192,5.85319786122763,
10.0798289574122));
#118078=CARTESIAN_POINT('Ctrl Pts',(-10.7758653243394,5.85680532844437,
10.1129660344793));
#118079=CARTESIAN_POINT('Ctrl Pts',(-10.8064478968707,5.85970689640087,
10.1406762262686));
#118080=CARTESIAN_POINT('Ctrl Pts',(-10.895556579142,5.86876608198137,10.2303690942567));
#118081=CARTESIAN_POINT('Ctrl Pts',(-10.9488640058241,5.87509134210871,
10.2971428844925));
#118082=CARTESIAN_POINT('Ctrl Pts',(-11.0077711710052,5.8830780034626,10.3899947905962));
#118083=CARTESIAN_POINT('Ctrl Pts',(-11.0203829632282,5.88486226307866,
10.4113338370063));
#118084=CARTESIAN_POINT('Ctrl Pts',(-11.0372908443385,5.88735038048038,
10.4421203471628));
#118085=CARTESIAN_POINT('Ctrl Pts',(-11.0421494712075,5.88807782057147,
10.4512500580464));
#118086=CARTESIAN_POINT('Ctrl Pts',(-11.0505319410105,5.88935396544953,
10.4675143279457));
#118087=CARTESIAN_POINT('Ctrl Pts',(-11.0541048699363,5.88990514641565,
10.4746227243214));
#118088=CARTESIAN_POINT('Ctrl Pts',(-11.0594148296537,5.89073489823167,
10.4854592464811));
#118089=CARTESIAN_POINT('Ctrl Pts',(-11.0612047314854,5.89101650016448,
10.4891609965118));
#118090=CARTESIAN_POINT('Ctrl Pts',(-11.0644325507665,5.89152773883546,
10.4959267297449));
#118091=CARTESIAN_POINT('Ctrl Pts',(-11.0658766643162,5.8917577368547,10.4989875709834));
#118092=CARTESIAN_POINT('Ctrl Pts',(-11.0691057930816,5.89227494629921,
10.5059089615551));
#118093=CARTESIAN_POINT('Ctrl Pts',(-11.0708831070205,5.89256169346219,
10.5097729877074));
#118094=CARTESIAN_POINT('Ctrl Pts',(-11.075429587041,5.89330086127631,10.5198001290989));
#118095=CARTESIAN_POINT('Ctrl Pts',(-11.078166765539,5.8937514467997,10.52597769716));
#118096=CARTESIAN_POINT('Ctrl Pts',(-11.0982704139765,5.89710591934993,
10.5724250061464));
#118097=CARTESIAN_POINT('Ctrl Pts',(-11.1134307745713,5.89989462363576,
10.613617925865));
#118098=CARTESIAN_POINT('Ctrl Pts',(-11.1318844536946,5.90384498513094,
10.6739591580923));
#118099=CARTESIAN_POINT('Ctrl Pts',(-11.1370584093556,5.90504028836632,
10.6924886177964));
#118100=CARTESIAN_POINT('Ctrl Pts',(-11.1538881992863,5.90929301887068,
10.7590109600925));
#118101=CARTESIAN_POINT('Ctrl Pts',(-11.162976854303,5.91233058417215,10.8075983550166));
#118102=CARTESIAN_POINT('Ctrl Pts',(-11.1750155459169,5.91852626408267,
10.9057454031004));
#118103=CARTESIAN_POINT('Ctrl Pts',(-11.1779379923034,5.92167863521211,
10.9552042523465));
#118104=CARTESIAN_POINT('Ctrl Pts',(-11.1776952635886,5.92567537975267,
11.0160747781951));
#118105=CARTESIAN_POINT('Ctrl Pts',(-11.1774850013983,5.92642725270317,
11.0274515773558));
#118106=CARTESIAN_POINT('Ctrl Pts',(-11.1768868485671,5.92763441770235,
11.0455874118374));
#118107=CARTESIAN_POINT('Ctrl Pts',(-11.1766054568,5.92808642022136,11.052349424586));
#118108=CARTESIAN_POINT('Ctrl Pts',(-11.175961858709,5.92894632661825,11.0651570948562));
#118109=CARTESIAN_POINT('Ctrl Pts',(-11.1756112669987,5.92935385801442,
11.0712031369153));
#118110=CARTESIAN_POINT('Ctrl Pts',(-11.1747076567851,5.93028426795964,
11.0849505660536));
#118111=CARTESIAN_POINT('Ctrl Pts',(-11.1741255074466,5.93080803107064,
11.0926496920355));
#118112=CARTESIAN_POINT('Ctrl Pts',(-11.1721009181036,5.93242733381381,
11.1163265290887));
#118113=CARTESIAN_POINT('Ctrl Pts',(-11.1704077434366,5.9335305381578,11.1322803605795));
#118114=CARTESIAN_POINT('Ctrl Pts',(-11.1586219860055,5.94002985697228,
11.2252014999871));
#118115=CARTESIAN_POINT('Ctrl Pts',(-11.1412671196536,5.94564998499509,
11.3010416623207));
#118116=CARTESIAN_POINT('Ctrl Pts',(-11.0994558299612,5.95528925424692,
11.4256665548531));
#118117=CARTESIAN_POINT('Ctrl Pts',(-11.078844579872,5.95925571722541,11.4754892218222));
#118118=CARTESIAN_POINT('Ctrl Pts',(-11.0474862437933,5.96432013598574,
11.5386513020983));
#118119=CARTESIAN_POINT('Ctrl Pts',(-11.0397610445403,5.96550642379532,
11.5534163754663));
#118120=CARTESIAN_POINT('Ctrl Pts',(-11.0262058764351,5.96748303446041,
11.5780376347333));
#118121=CARTESIAN_POINT('Ctrl Pts',(-11.0205409367788,5.96828088418374,
11.5879814866216));
#118122=CARTESIAN_POINT('Ctrl Pts',(-11.012317977323,5.96939845561366,11.6019385233083));
#118123=CARTESIAN_POINT('Ctrl Pts',(-11.0098794059447,5.96972505526765,
11.6060208416054));
#118124=CARTESIAN_POINT('Ctrl Pts',(-11.0056354870955,5.97028507328242,
11.6130286662371));
#118125=CARTESIAN_POINT('Ctrl Pts',(-11.0038419520618,5.97051922711342,
11.6159612123169));
#118126=CARTESIAN_POINT('Ctrl Pts',(-11.0000420840315,5.97101001093681,
11.6221135619159));
#118127=CARTESIAN_POINT('Ctrl Pts',(-10.9980330091693,5.97126646210512,
11.6253315659574));
#118128=CARTESIAN_POINT('Ctrl Pts',(-10.9925583583521,5.97195729212957,
11.6340069077107));
#118129=CARTESIAN_POINT('Ctrl Pts',(-10.9890632810347,5.97238981207894,
11.6394456071847));
#118130=CARTESIAN_POINT('Ctrl Pts',(-10.9723353491798,5.97442157832678,
11.6650106716581));
#118131=CARTESIAN_POINT('Ctrl Pts',(-10.958530907186,5.97598710954884,11.6847582879155));
#118132=CARTESIAN_POINT('Ctrl Pts',(-10.9028407971031,5.98194992737554,
11.7594364605432));
#118133=CARTESIAN_POINT('Ctrl Pts',(-10.8567588458612,5.98617139903251,
11.81106783501));
#118134=CARTESIAN_POINT('Ctrl Pts',(-10.7584952246908,5.9945312462484,11.9033841529435));
#118135=CARTESIAN_POINT('Ctrl Pts',(-10.7068970201755,5.99865029955416,
11.9443055507134));
#118136=CARTESIAN_POINT('Ctrl Pts',(-10.6403315529191,6.00387006293588,
11.9885708346382));
#118137=CARTESIAN_POINT('Ctrl Pts',(-10.6283637779072,6.00480471257315,
11.9962207221405));
#118138=CARTESIAN_POINT('Ctrl Pts',(-10.6099876276135,6.00623574767356,
12.0075040195473));
#118139=CARTESIAN_POINT('Ctrl Pts',(-10.6036784065798,6.00672635565561,
12.0112970051144));
#118140=CARTESIAN_POINT('Ctrl Pts',(-10.5921397370371,6.00762252715203,
12.0180873836492));
#118141=CARTESIAN_POINT('Ctrl Pts',(-10.5869220096243,6.00802737479339,
12.0211042753982));
#118142=CARTESIAN_POINT('Ctrl Pts',(-10.5755814230532,6.00890656972139,
12.027545766937));
#118143=CARTESIAN_POINT('Ctrl Pts',(-10.5694506895897,6.00938140858583,
12.0309559574311));
#118144=CARTESIAN_POINT('Ctrl Pts',(-10.5525790327372,6.01068712373316,
12.0401443292468));
#118145=CARTESIAN_POINT('Ctrl Pts',(-10.5417784976248,6.01152186302523,
12.0458106201535));
#118146=CARTESIAN_POINT('Ctrl Pts',(-10.4665999776609,6.01732642989461,
12.0837744660025));
#118147=CARTESIAN_POINT('Ctrl Pts',(-10.3994766430831,6.0224944250484,12.1102691906438));
#118148=CARTESIAN_POINT('Ctrl Pts',(-10.2796567893891,6.03161908203103,
12.1452851907529));
#118149=CARTESIAN_POINT('Ctrl Pts',(-10.2280080506737,6.03551786450257,
12.1566756184141));
#118150=CARTESIAN_POINT('Ctrl Pts',(-10.1515834263136,6.04112962872133,
12.1682105073654));
#118151=CARTESIAN_POINT('Ctrl Pts',(-10.1272885316629,6.04289016423973,
12.1711067860192));
#118152=CARTESIAN_POINT('Ctrl Pts',(-10.0927069711798,6.04534868355793,
12.1741403584893));
#118153=CARTESIAN_POINT('Ctrl Pts',(-10.0824826348186,6.04606969412131,
12.1749028874096));
#118154=CARTESIAN_POINT('Ctrl Pts',(-10.0643622881309,6.04733569457318,
12.1760165805728));
#118155=CARTESIAN_POINT('Ctrl Pts',(-10.0564703610344,6.04788310826346,
12.1764219517979));
#118156=CARTESIAN_POINT('Ctrl Pts',(-10.0444775131329,6.04870837079211,
12.1769170016562));
#118157=CARTESIAN_POINT('Ctrl Pts',(-10.0403794025583,6.04898920282887,
12.1770647319035));
#118158=CARTESIAN_POINT('Ctrl Pts',(-10.0328972549855,6.04949969635539,
12.1772953285025));
#118159=CARTESIAN_POINT('Ctrl Pts',(-10.0295135976092,6.04972971248978,
12.1773850126808));
#118160=CARTESIAN_POINT('Ctrl Pts',(-10.0218649315126,6.0502477731439,12.1775547471037));
#118161=CARTESIAN_POINT('Ctrl Pts',(-10.017599837303,6.05053534615001,12.1776262160832));
#118162=CARTESIAN_POINT('Ctrl Pts',(-10.0065365869644,6.05127810145475,
12.1777514811081));
#118163=CARTESIAN_POINT('Ctrl Pts',(-9.99973807400412,6.05173141895143,
12.1777695933052));
#118164=CARTESIAN_POINT('Ctrl Pts',(-9.94703997528089,6.0552237622368,12.1774536716179));
#118165=CARTESIAN_POINT('Ctrl Pts',(-9.90118981057364,6.05813647379192,
12.1744954204296));
#118166=CARTESIAN_POINT('Ctrl Pts',(-9.83850812105004,6.06208433004872,
12.1667531323157));
#118167=CARTESIAN_POINT('Ctrl Pts',(-9.82144006302314,6.06315570866509,
12.1642632295234));
#118168=CARTESIAN_POINT('Ctrl Pts',(-9.75464996471581,6.06735324763434,
12.1530164804466));
#118169=CARTESIAN_POINT('Ctrl Pts',(-9.7054590877052,6.07045818225584,12.1414416932365));
#118170=CARTESIAN_POINT('Ctrl Pts',(-9.61086941177181,6.07665833042173,
12.1126607684765));
#118171=CARTESIAN_POINT('Ctrl Pts',(-9.565492693937,6.07974261654607,12.0957368116173));
#118172=CARTESIAN_POINT('Ctrl Pts',(-9.51095249436908,6.08366260936188,
12.0714735567464));
#118173=CARTESIAN_POINT('Ctrl Pts',(-9.5006833065229,6.08441023225558,12.0667267085232));
#118174=CARTESIAN_POINT('Ctrl Pts',(-9.48439540958915,6.08561217650794,
12.0589110354723));
#118175=CARTESIAN_POINT('Ctrl Pts',(-9.47833179796513,6.08606325884864,
12.0559370049776));
#118176=CARTESIAN_POINT('Ctrl Pts',(-9.46687748099454,6.08692244306843,
12.0501962451072));
#118177=CARTESIAN_POINT('Ctrl Pts',(-9.46148187561897,6.08733018131324,
12.0474397361521));
#118178=CARTESIAN_POINT('Ctrl Pts',(-9.44923739567313,6.08826250434251,
12.0410646546737));
#118179=CARTESIAN_POINT('Ctrl Pts',(-9.44240252874945,6.08878798738599,
12.0374199326366));
#118180=CARTESIAN_POINT('Ctrl Pts',(-9.42140825397861,6.0904180874743,12.025957239138));
#118181=CARTESIAN_POINT('Ctrl Pts',(-9.40737407563235,6.09153051819662,
12.0179150916901));
#118182=CARTESIAN_POINT('Ctrl Pts',(-9.33379521931331,6.09748777759601,
11.9737140386729));
#118183=CARTESIAN_POINT('Ctrl Pts',(-9.27739000599291,6.10250883656341,
11.9326198247534));
#118184=CARTESIAN_POINT('Ctrl Pts',(-9.17981419023098,6.11199402890588,
11.8473395231834));
#118185=CARTESIAN_POINT('Ctrl Pts',(-9.13775194974572,6.11642177259655,
11.8044984387828));
#118186=CARTESIAN_POINT('Ctrl Pts',(-9.08777731861914,6.12200282642176,
11.7451547875916));
#118187=CARTESIAN_POINT('Ctrl Pts',(-9.07672468994285,6.12326003064341,
11.7314155091281));
#118188=CARTESIAN_POINT('Ctrl Pts',(-9.05871548420487,6.12534130879301,
11.7079695644674));
#118189=CARTESIAN_POINT('Ctrl Pts',(-9.05159069704285,6.12617390861915,
11.6983962093682));
#118190=CARTESIAN_POINT('Ctrl Pts',(-9.04178532445334,6.12733112196246,
11.6847941798981));
#118191=CARTESIAN_POINT('Ctrl Pts',(-9.03898245074212,6.12766326646496,
11.6808551280019));
#118192=CARTESIAN_POINT('Ctrl Pts',(-9.03422079000655,6.12822971748844,
11.6740752814595));
#118193=CARTESIAN_POINT('Ctrl Pts',(-9.03225010613175,6.12846480515564,
11.6712429602783));
#118194=CARTESIAN_POINT('Ctrl Pts',(-9.02815820107811,6.12895425969481,
11.6653064816562));
#118195=CARTESIAN_POINT('Ctrl Pts',(-9.0260393646799,6.12920847189046,11.6622007841338));
#118196=CARTESIAN_POINT('Ctrl Pts',(-9.02040426770968,6.1298867784185,11.6538555491758));
#118197=CARTESIAN_POINT('Ctrl Pts',(-9.01691512223378,6.13030912745391,
11.6485977223077));
#118198=CARTESIAN_POINT('Ctrl Pts',(-9.0012750329835,6.13221435726023,11.6246133343469));
#118199=CARTESIAN_POINT('Ctrl Pts',(-8.98961489105718,6.13366842656563,
11.6055703606862));
#118200=CARTESIAN_POINT('Ctrl Pts',(-8.96763850352448,6.13650225493909,
11.5672752412326));
#118201=CARTESIAN_POINT('Ctrl Pts',(-8.95730253432802,6.13788238655509,
11.5480452025423));
#118202=CARTESIAN_POINT('Ctrl Pts',(-8.9166486186316,6.1435617755003,11.4670898730716));
#118203=CARTESIAN_POINT('Ctrl Pts',(-8.89123096516069,6.14775342711004,
11.4030568239904));
#118204=CARTESIAN_POINT('Ctrl Pts',(-8.85693437350742,6.15525136477062,
11.2882717732334));
#118205=CARTESIAN_POINT('Ctrl Pts',(-8.84551926511867,6.15849743397149,
11.2384804320415));
#118206=CARTESIAN_POINT('Ctrl Pts',(-8.83553832368823,6.16259975366978,
11.1767922684761));
#118207=CARTESIAN_POINT('Ctrl Pts',(-8.83387259266239,6.163357218145,11.1654489545542));
#118208=CARTESIAN_POINT('Ctrl Pts',(-8.83148489797139,6.16457125180627,
11.1473552697741));
#118209=CARTESIAN_POINT('Ctrl Pts',(-8.83065521510991,6.16502446451204,
11.1406196643484));
#118210=CARTESIAN_POINT('Ctrl Pts',(-8.82919577056458,6.165885335354,11.1278638150882));
#118211=CARTESIAN_POINT('Ctrl Pts',(-8.82855411552353,6.16629260945253,
11.121845132331));
#118212=CARTESIAN_POINT('Ctrl Pts',(-8.82720271741023,6.16722057532817,
11.1081698722249));
#118213=CARTESIAN_POINT('Ctrl Pts',(-8.82652151366565,6.16774213412433,
11.100510818159));
#118214=CARTESIAN_POINT('Ctrl Pts',(-8.82466391719549,6.16934766410132,
11.077020519941));
#118215=CARTESIAN_POINT('Ctrl Pts',(-8.82373260712074,6.17043911208709,
11.0611722644537));
#118216=CARTESIAN_POINT('Ctrl Pts',(-8.81994039894409,6.17727679848077,
10.9626752375845));
#118217=CARTESIAN_POINT('Ctrl Pts',(-8.8254716351637,6.18328105719493,10.8799488573848));
#118218=CARTESIAN_POINT('Ctrl Pts',(-8.85145132348145,6.19442286019621,
10.7303393820249));
#118219=CARTESIAN_POINT('Ctrl Pts',(-8.86927084106631,6.19951365297629,
10.6633483482401));
#118220=CARTESIAN_POINT('Ctrl Pts',(-8.89597270092113,6.20499005121681,
10.589754333469));
#118221=CARTESIAN_POINT('Ctrl Pts',(-8.89917383850949,6.20562162857878,
10.5812404522781));
#118222=CARTESIAN_POINT('Ctrl Pts',(-8.90404699459608,6.20654649929942,
10.5687217955917));
#118223=CARTESIAN_POINT('Ctrl Pts',(-8.90564293713968,6.20684392410625,
10.5646880427521));
#118224=CARTESIAN_POINT('Ctrl Pts',(-8.9085251933115,6.20737135213772,10.5575191630085));
#118225=CARTESIAN_POINT('Ctrl Pts',(-8.90980278748786,6.20760185033157,
10.554380674198));
#118226=CARTESIAN_POINT('Ctrl Pts',(-8.91263372108549,6.2081054476046,10.5475113609995));
#118227=CARTESIAN_POINT('Ctrl Pts',(-8.91419272808288,6.20837820795604,
10.5437829875848));
#118228=CARTESIAN_POINT('Ctrl Pts',(-8.91866012672926,6.20914723092183,
10.5332518066875));
#118229=CARTESIAN_POINT('Ctrl Pts',(-8.92161353228926,6.20964091670073,
10.526468131364));
#118230=CARTESIAN_POINT('Ctrl Pts',(-8.94237360183216,6.21301507758722,
10.479986094138));
#118231=CARTESIAN_POINT('Ctrl Pts',(-8.96230639805596,6.21578275798562,
10.4412684457535));
#118232=CARTESIAN_POINT('Ctrl Pts',(-8.99424397426174,6.21973319052331,
10.3868665181161));
#118233=CARTESIAN_POINT('Ctrl Pts',(-9.00456824894697,6.22094906703784,
10.3702432929228));
#118234=CARTESIAN_POINT('Ctrl Pts',(-9.042848454305,6.2252736976786,10.3119031812852));
#118235=CARTESIAN_POINT('Ctrl Pts',(-9.07305070880461,6.2283619059775,10.271727265241));
#118236=CARTESIAN_POINT('Ctrl Pts',(-9.13746595293808,6.23456760567458,
10.1965639886571));
#118237=CARTESIAN_POINT('Ctrl Pts',(-9.17147437984068,6.23767572605648,
10.161537809113));
#118238=CARTESIAN_POINT('Ctrl Pts',(-9.21593957255163,6.24162259097188,
10.12109567214));
#118239=CARTESIAN_POINT('Ctrl Pts',(-9.22443529865826,6.2423717198824,10.1135898517853));
#118240=CARTESIAN_POINT('Ctrl Pts',(-9.23816697858046,6.24357551410664,
10.1018067078392));
#118241=CARTESIAN_POINT('Ctrl Pts',(-9.24333384539688,6.24402692254065,
10.0974496856814));
#118242=CARTESIAN_POINT('Ctrl Pts',(-9.25320244835176,6.24488636155847,
10.0892721710971));
#118243=CARTESIAN_POINT('Ctrl Pts',(-9.25789673572267,6.24529402536646,
10.0854430010735));
#118244=CARTESIAN_POINT('Ctrl Pts',(-9.26865323526619,6.24622566489964,
10.0768061774196));
#118245=CARTESIAN_POINT('Ctrl Pts',(-9.27473364840652,6.24675053399349,
10.0720217466764));
#118246=CARTESIAN_POINT('Ctrl Pts',(-9.2936322345923,6.24837677466826,10.0574504126231));
#118247=CARTESIAN_POINT('Ctrl Pts',(-9.30660416466416,6.24948590651322,
10.0478669653783));
#118248=CARTESIAN_POINT('Ctrl Pts',(-9.37658707831844,6.25543525747671,
9.99835345659297));
#118249=CARTESIAN_POINT('Ctrl Pts',(-9.43684831745196,6.26045148134564,
9.96327594894306));
#118250=CARTESIAN_POINT('Ctrl Pts',(-9.55421430847007,6.26993962622691,
9.9082230851759));
#118251=CARTESIAN_POINT('Ctrl Pts',(-9.61045754356547,6.27437536955614,
9.88691474052568));
#118252=CARTESIAN_POINT('Ctrl Pts',(-9.68501252270141,6.27996531685678,
9.86501571460661));
#118253=CARTESIAN_POINT('Ctrl Pts',(-9.7020536997882,6.28122368640625,9.8604235398414));
#118254=CARTESIAN_POINT('Ctrl Pts',(-9.73078847295159,6.28330667744125,
9.85336894024559));
#118255=CARTESIAN_POINT('Ctrl Pts',(-9.7424276179688,6.28413984170077,9.85069841692303));
#118256=CARTESIAN_POINT('Ctrl Pts',(-9.75883493815722,6.28529769725672,
9.8471956547395));
#118257=CARTESIAN_POINT('Ctrl Pts',(-9.76357024640248,6.28562993036857,
9.84621517639846));
#118258=CARTESIAN_POINT('Ctrl Pts',(-9.77169471585385,6.28619648463342,
9.84458506750503));
#118259=CARTESIAN_POINT('Ctrl Pts',(-9.77508090643458,6.28643158766354,
9.84392112222993));
#118260=CARTESIAN_POINT('Ctrl Pts',(-9.78216200544157,6.28692102306534,
9.84256499064077));
#118261=CARTESIAN_POINT('Ctrl Pts',(-9.78585736253136,6.28717520113481,
9.84187560056085));
#118262=CARTESIAN_POINT('Ctrl Pts',(-9.79576210200434,6.28785331693078,
9.84007684340012));
#118263=CARTESIAN_POINT('Ctrl Pts',(-9.80197730639773,6.2882755110681,9.83899962731526));
#118264=CARTESIAN_POINT('Ctrl Pts',(-9.80918359072738,6.28876150219062,
9.83781019098842));
#118265=CARTESIAN_POINT('Ctrl Pts',(-9.81016634717706,6.28882770338877,
9.83764926186054));
#118266=CARTESIAN_POINT('Ctrl Pts',(-9.81114930150925,6.28889384320256,
9.83748958018452));
#118267=CARTESIAN_POINT('Origin',(-10.,2.67563288526385,11.));
#118268=CARTESIAN_POINT('',(-9.81114930150157,6.88692359881868,9.83748958018577));
#118269=CARTESIAN_POINT('',(-9.81114930155385,6.78711399980274,9.83748958017728));
#118270=CARTESIAN_POINT('',(-9.81114930150157,2.67563288526385,9.83748958018577));
#118271=CARTESIAN_POINT('Ctrl Pts',(-9.81114930150157,6.88692359881869,
9.83748958018577));
#118272=CARTESIAN_POINT('Ctrl Pts',(-9.76179042850999,6.88380575833335,
9.84550796650101));
#118273=CARTESIAN_POINT('Ctrl Pts',(-9.7129624323272,6.8806441789585,9.85666654922391));
#118274=CARTESIAN_POINT('Ctrl Pts',(-9.64974224407113,6.87635091260822,
9.87542603022264));
#118275=CARTESIAN_POINT('Ctrl Pts',(-9.63461569572728,6.87530842991322,
9.88024941152047));
#118276=CARTESIAN_POINT('Ctrl Pts',(-9.61231325242055,6.87374635546162,
9.88786098144651));
#118277=CARTESIAN_POINT('Ctrl Pts',(-9.60505933493838,6.87323430605266,
9.89041625947696));
#118278=CARTESIAN_POINT('Ctrl Pts',(-9.59214058766744,6.87231498885222,
9.89510977083978));
#118279=CARTESIAN_POINT('Ctrl Pts',(-9.5864661895756,6.87190861854475,9.89722100853172));
#118280=CARTESIAN_POINT('Ctrl Pts',(-9.57446415273821,6.87104350070152,
9.90179219024364));
#118281=CARTESIAN_POINT('Ctrl Pts',(-9.56814102279633,6.87058439699561,
9.90426327468967));
#118282=CARTESIAN_POINT('Ctrl Pts',(-9.5511931304261,6.86934469582523,9.91105600927023));
#118283=CARTESIAN_POINT('Ctrl Pts',(-9.54060978228383,6.86856077964798,
9.91547833914255));
#118284=CARTESIAN_POINT('Ctrl Pts',(-9.4832417468298,6.86425654377663,9.94044037423251));
#118285=CARTESIAN_POINT('Ctrl Pts',(-9.43777328038918,6.86064042014211,
9.96385063048835));
#118286=CARTESIAN_POINT('Ctrl Pts',(-9.3345596547659,6.85194779297395,10.0257898499238));
#118287=CARTESIAN_POINT('Ctrl Pts',(-9.27841011587521,6.84682189398038,
10.0666172370726));
#118288=CARTESIAN_POINT('Ctrl Pts',(-9.19493393992593,6.83875158519271,
10.1393714025256));
#118289=CARTESIAN_POINT('Ctrl Pts',(-9.1651440962155,6.83576621817576,10.1682372235315));
#118290=CARTESIAN_POINT('Ctrl Pts',(-9.13233734381287,6.83240784216452,
10.2035690569654));
#118291=CARTESIAN_POINT('Ctrl Pts',(-9.12778158932141,6.83193979573026,
10.208560942762));
#118292=CARTESIAN_POINT('Ctrl Pts',(-9.12042836942682,6.83118197293282,
10.2167587174884));
#118293=CARTESIAN_POINT('Ctrl Pts',(-9.11760493578553,6.83089040770405,
10.2199409560735));
#118294=CARTESIAN_POINT('Ctrl Pts',(-9.11256570719197,6.83036908374168,
10.2256829465782));
#118295=CARTESIAN_POINT('Ctrl Pts',(-9.11034365390934,6.83013887950344,
10.2282370117834));
#118296=CARTESIAN_POINT('Ctrl Pts',(-9.10544625595514,6.8296307827573,10.2339154230651));
#118297=CARTESIAN_POINT('Ctrl Pts',(-9.10277624372192,6.82935327183675,
10.2370442264093));
#118298=CARTESIAN_POINT('Ctrl Pts',(-9.0949880147737,6.8285420897468,10.2462681421888));
#118299=CARTESIAN_POINT('Ctrl Pts',(-9.08991500411405,6.82801152468811,
10.2524013672887));
#118300=CARTESIAN_POINT('Ctrl Pts',(-9.07839110009297,6.82679993981414,
10.2666248246997));
#118301=CARTESIAN_POINT('Ctrl Pts',(-9.07198378166519,6.82612157327325,
10.2747496799778));
#118302=CARTESIAN_POINT('Ctrl Pts',(-9.050587773727,6.82383593427871,10.3026289894329));
#118303=CARTESIAN_POINT('Ctrl Pts',(-9.03611539849764,6.82225483822977,
10.3227729074299));
#118304=CARTESIAN_POINT('Ctrl Pts',(-8.99297176984956,6.8173772938791,10.3870120642228));
#118305=CARTESIAN_POINT('Ctrl Pts',(-8.96660976898363,6.81414729723689,
10.4325802684868));
#118306=CARTESIAN_POINT('Ctrl Pts',(-8.91168687598181,6.80644384007156,
10.5441297845966));
#118307=CARTESIAN_POINT('Ctrl Pts',(-8.88594577952553,6.80195556185637,
10.6112528618167));
#118308=CARTESIAN_POINT('Ctrl Pts',(-8.86316351407304,6.79645588799566,
10.6920284422795));
#118309=CARTESIAN_POINT('Ctrl Pts',(-8.86003677285234,6.79565161104774,
10.7038117172662));
#118310=CARTESIAN_POINT('Ctrl Pts',(-8.85539980489722,6.79437535476795,
10.7224487972974));
#118311=CARTESIAN_POINT('Ctrl Pts',(-8.85376690724421,6.79390727631051,
10.7292714085222));
#118312=CARTESIAN_POINT('Ctrl Pts',(-8.85084421183912,6.79303331594007,
10.7419837497076));
#118313=CARTESIAN_POINT('Ctrl Pts',(-8.84953849442978,6.79262795348139,
10.7478696115752));
#118314=CARTESIAN_POINT('Ctrl Pts',(-8.84673797962109,6.79172411118871,
10.7609685467832));
#118315=CARTESIAN_POINT('Ctrl Pts',(-8.84526555833112,6.79122494322128,
10.7681860913628));
#118316=CARTESIAN_POINT('Ctrl Pts',(-8.84114938812104,6.78975584280423,
10.7893758587363));
#118317=CARTESIAN_POINT('Ctrl Pts',(-8.83869094749129,6.78878017059658,
10.8033822911032));
#118318=CARTESIAN_POINT('Ctrl Pts',(-8.82536651925484,6.78283486572284,
10.8882981462983));
#118319=CARTESIAN_POINT('Ctrl Pts',(-8.82074613153098,6.7776727719978,10.9600225828784));
#118320=CARTESIAN_POINT('Ctrl Pts',(-8.82488830363903,6.76641594566124,
11.1138122572782));
#118321=CARTESIAN_POINT('Ctrl Pts',(-8.8356817974282,6.76032312666523,11.1954628546032));
#118322=CARTESIAN_POINT('Ctrl Pts',(-8.85711033871251,6.75390455613337,
11.2845854857307));
#118323=CARTESIAN_POINT('Ctrl Pts',(-8.85944790637781,6.75324301673536,
11.2938139082215));
#118324=CARTESIAN_POINT('Ctrl Pts',(-8.86302198055884,6.75228621149174,
11.3072379506916));
#118325=CARTESIAN_POINT('Ctrl Pts',(-8.86417029767902,6.75198633959229,
11.3114563595402));
#118326=CARTESIAN_POINT('Ctrl Pts',(-8.86625288273057,6.75145573934282,
11.318942132196));
#118327=CARTESIAN_POINT('Ctrl Pts',(-8.86717783475078,6.75122449892443,
11.3222119684327));
#118328=CARTESIAN_POINT('Ctrl Pts',(-8.86921277893933,6.75072520772989,
11.3292886974684));
#118329=CARTESIAN_POINT('Ctrl Pts',(-8.87032785275883,6.75045744828318,
11.3330940205084));
#118330=CARTESIAN_POINT('Ctrl Pts',(-8.8735368645652,6.74970290661337,11.3438436759775));
#118331=CARTESIAN_POINT('Ctrl Pts',(-8.8756758054223,6.74921860705328,11.3507745443964));
#118332=CARTESIAN_POINT('Ctrl Pts',(-8.89101712500389,6.745868036217,11.3989029284176));
#118333=CARTESIAN_POINT('Ctrl Pts',(-8.90641820536623,6.74311400244167,
11.439370363674));
#118334=CARTESIAN_POINT('Ctrl Pts',(-8.96157880909751,6.73461477932193,
11.5633038306765));
#118335=CARTESIAN_POINT('Ctrl Pts',(-9.00894260295148,6.72902795338409,
11.6429893197167));
#118336=CARTESIAN_POINT('Ctrl Pts',(-9.0830695657527,6.72124872695082,11.7397319874945));
#118337=CARTESIAN_POINT('Ctrl Pts',(-9.10187856883824,6.71934038468655,
11.7624581984725));
#118338=CARTESIAN_POINT('Ctrl Pts',(-9.12819410550953,6.71673831021565,
11.7919280066178));
#118339=CARTESIAN_POINT('Ctrl Pts',(-9.13496373456065,6.71607457323208,
11.7993170426254));
#118340=CARTESIAN_POINT('Ctrl Pts',(-9.14626195848161,6.71497542121608,
11.8113373883223));
#118341=CARTESIAN_POINT('Ctrl Pts',(-9.15073602384149,6.71454231276816,
11.8160194220677));
#118342=CARTESIAN_POINT('Ctrl Pts',(-9.15953609391194,6.71369443898523,
11.8250777834417));
#118343=CARTESIAN_POINT('Ctrl Pts',(-9.16385823894177,6.7132798476198,11.829457581262));
#118344=CARTESIAN_POINT('Ctrl Pts',(-9.17415364035798,6.71229646702617,
11.8397280693911));
#118345=CARTESIAN_POINT('Ctrl Pts',(-9.18015584080465,6.71172641938154,
11.8455891369838));
#118346=CARTESIAN_POINT('Ctrl Pts',(-9.20055381911394,6.70979962182896,
11.8650861421125));
#118347=CARTESIAN_POINT('Ctrl Pts',(-9.21523053033918,6.70843038631718,
11.8784218955218));
#118348=CARTESIAN_POINT('Ctrl Pts',(-9.31376777079229,6.6993419895866,11.9635151153038));
#118349=CARTESIAN_POINT('Ctrl Pts',(-9.40701564978442,6.69114924935245,
12.023541157303));
#118350=CARTESIAN_POINT('Ctrl Pts',(-9.54223638866296,6.68031865963084,
12.085833253133));
#118351=CARTESIAN_POINT('Ctrl Pts',(-9.57802714927119,6.67754861317366,
12.100236758403));
#118352=CARTESIAN_POINT('Ctrl Pts',(-9.6213369515905,6.67435719096461,12.115240903243));
#118353=CARTESIAN_POINT('Ctrl Pts',(-9.6282324977917,6.67385381597231,12.117558458173));
#118354=CARTESIAN_POINT('Ctrl Pts',(-9.6389659699121,6.67307808184156,12.1210555762556));
#118355=CARTESIAN_POINT('Ctrl Pts',(-9.64278905718063,6.67280330578054,
12.1222796084176));
#118356=CARTESIAN_POINT('Ctrl Pts',(-9.64985425857583,6.6722984191618,12.1245019026164));
#118357=CARTESIAN_POINT('Ctrl Pts',(-9.65309443876776,6.67206800729686,
12.1255057091432));
#118358=CARTESIAN_POINT('Ctrl Pts',(-9.66052484702463,6.67154218082568,
12.1277725101334));
#118359=CARTESIAN_POINT('Ctrl Pts',(-9.6647178196377,6.67124730103432,12.1290261623021));
#118360=CARTESIAN_POINT('Ctrl Pts',(-9.67783608168133,6.67033019621591,
12.1328688508746));
#118361=CARTESIAN_POINT('Ctrl Pts',(-9.68678534660256,6.66971242431087,
12.1353757165151));
#118362=CARTESIAN_POINT('Ctrl Pts',(-9.70798118605942,6.66826574547116,
12.1410433886532));
#118363=CARTESIAN_POINT('Ctrl Pts',(-9.72025104788914,6.66744117351677,
12.1441134357934));
#118364=CARTESIAN_POINT('Ctrl Pts',(-9.76545139601389,6.66444268131249,
12.1546523643158));
#118365=CARTESIAN_POINT('Ctrl Pts',(-9.79865124764172,6.66231568911361,
12.1609022946999));
#118366=CARTESIAN_POINT('Ctrl Pts',(-9.90806180388688,6.65542136814449,
12.1766631168506));
#118367=CARTESIAN_POINT('Ctrl Pts',(-9.98493354166135,6.6507460253511,12.1801532290513));
#118368=CARTESIAN_POINT('Ctrl Pts',(-10.0985151286715,6.64354566969613,
12.1742045969359));
#118369=CARTESIAN_POINT('Ctrl Pts',(-10.1353173729581,6.64116920144629,
12.1705342620274));
#118370=CARTESIAN_POINT('Ctrl Pts',(-10.1826064781939,6.63802694301749,
12.1635580858076));
#118371=CARTESIAN_POINT('Ctrl Pts',(-10.1933067058868,6.63731008068205,
12.161828321907));
#118372=CARTESIAN_POINT('Ctrl Pts',(-10.210532889724,6.63614583254991,12.1587990404762));
#118373=CARTESIAN_POINT('Ctrl Pts',(-10.2170745332368,6.63570132919074,
12.1575914468501));
#118374=CARTESIAN_POINT('Ctrl Pts',(-10.2295802899452,6.63484683790583,
12.1551731412115));
#118375=CARTESIAN_POINT('Ctrl Pts',(-10.2355459527948,6.63443714747739,
12.1539714890093));
#118376=CARTESIAN_POINT('Ctrl Pts',(-10.249280783566,6.63348900242105,12.1510939665381));
#118377=CARTESIAN_POINT('Ctrl Pts',(-10.2570427610736,6.63294953842154,
12.1493855934702));
#118378=CARTESIAN_POINT('Ctrl Pts',(-10.2816068545799,6.63123042579049,
12.1437178941811));
#118379=CARTESIAN_POINT('Ctrl Pts',(-10.2983388429721,6.63004168180246,
12.1394678241189));
#118380=CARTESIAN_POINT('Ctrl Pts',(-10.3375236542188,6.62721423210916,
12.1285923373315));
#118381=CARTESIAN_POINT('Ctrl Pts',(-10.3598836497916,6.6255665631354,12.121662388081));
#118382=CARTESIAN_POINT('Ctrl Pts',(-10.4577772599144,6.61820097037958,
12.0880941366478));
#118383=CARTESIAN_POINT('Ctrl Pts',(-10.530679998881,6.61228990679209,12.0544595481455));
#118384=CARTESIAN_POINT('Ctrl Pts',(-10.6414629784819,6.60287674189544,
11.9889319383886));
#118385=CARTESIAN_POINT('Ctrl Pts',(-10.6817603144619,6.5993536170655,11.9615950761432));
#118386=CARTESIAN_POINT('Ctrl Pts',(-10.7256744122961,6.59548644304517,
11.9276522110296));
#118387=CARTESIAN_POINT('Ctrl Pts',(-10.7310572330969,6.59501194937347,
11.9234161059442));
#118388=CARTESIAN_POINT('Ctrl Pts',(-10.7397443081093,6.59424582523743,
11.916456083266));
#118389=CARTESIAN_POINT('Ctrl Pts',(-10.7430711137178,6.59395234260584,
11.9137607538859));
#118390=CARTESIAN_POINT('Ctrl Pts',(-10.7490027680495,6.59342902100396,
11.9089011958108));
#118391=CARTESIAN_POINT('Ctrl Pts',(-10.7516130483494,6.5931987204336,11.9067438208934));
#118392=CARTESIAN_POINT('Ctrl Pts',(-10.7573548594867,6.59269211430589,
11.9019564298167));
#118393=CARTESIAN_POINT('Ctrl Pts',(-10.7604820230539,6.59241617607557,
11.8993213432081));
#118394=CARTESIAN_POINT('Ctrl Pts',(-10.7695668428105,6.59161424881051,
11.8915847987638));
#118395=CARTESIAN_POINT('Ctrl Pts',(-10.7754874800048,6.59109125950153,
11.8864399333479));
#118396=CARTESIAN_POINT('Ctrl Pts',(-10.7889537788866,6.58989968459779,
11.8744999102825));
#118397=CARTESIAN_POINT('Ctrl Pts',(-10.7964639393049,6.58923362999945,
11.8676654694838));
#118398=CARTESIAN_POINT('Ctrl Pts',(-10.8839716782026,6.58144145673279,
11.7859374081227));
#118399=CARTESIAN_POINT('Ctrl Pts',(-10.9532364529416,6.57491599384366,
11.700321474848));
#118400=CARTESIAN_POINT('Ctrl Pts',(-11.031285485609,6.56536422591013,11.5703579361543));
#118401=CARTESIAN_POINT('Ctrl Pts',(-11.0509594657076,6.56267631391967,
11.5332368592667));
#118402=CARTESIAN_POINT('Ctrl Pts',(-11.0733468547502,6.55917913160202,
11.4849212523699));
#118403=CARTESIAN_POINT('Ctrl Pts',(-11.0779380929265,6.55843424845893,
11.4746277963509));
#118404=CARTESIAN_POINT('Ctrl Pts',(-11.0850399464836,6.55723558973298,
11.4580708263394));
#118405=CARTESIAN_POINT('Ctrl Pts',(-11.0876457619713,6.55678502015619,
11.4518487143755));
#118406=CARTESIAN_POINT('Ctrl Pts',(-11.0924917646039,6.55592608960512,
11.4399926849028));
#118407=CARTESIAN_POINT('Ctrl Pts',(-11.0947421871476,6.55551808629213,
11.4343631658178));
#118408=CARTESIAN_POINT('Ctrl Pts',(-11.0997758331871,6.5545841375757,11.421483671792));
#118409=CARTESIAN_POINT('Ctrl Pts',(-11.1025309899034,6.55405728367611,
11.4142231043229));
#118410=CARTESIAN_POINT('Ctrl Pts',(-11.1108366607301,6.5524190081942,11.3916653922981));
#118411=CARTESIAN_POINT('Ctrl Pts',(-11.1161418866876,6.55129966122063,
11.3762806257664));
#118412=CARTESIAN_POINT('Ctrl Pts',(-11.1277621006485,6.54866656244746,
11.3401718808432));
#118413=CARTESIAN_POINT('Ctrl Pts',(-11.1338272455177,6.54714543593486,
11.3193742940431));
#118414=CARTESIAN_POINT('Ctrl Pts',(-11.1542244518601,6.54143304830739,
11.2415019630706));
#118415=CARTESIAN_POINT('Ctrl Pts',(-11.1648456206274,6.53714329020795,
11.1835500173462));
#118416=CARTESIAN_POINT('Ctrl Pts',(-11.1783873291903,6.52778684236313,
11.0567355453575));
#118417=CARTESIAN_POINT('Ctrl Pts',(-11.1796910592591,6.52272683389703,
10.9879042701646));
#118418=CARTESIAN_POINT('Ctrl Pts',(-11.1742798673433,6.51718196869544,
10.9090718243968));
#118419=CARTESIAN_POINT('Ctrl Pts',(-11.1734397746921,6.5164649841199,10.8988058644734));
#118420=CARTESIAN_POINT('Ctrl Pts',(-11.1720699095102,6.51546684018339,
10.8843945108316));
#118421=CARTESIAN_POINT('Ctrl Pts',(-11.1716526217668,6.51518002206189,
10.8802392504279));
#118422=CARTESIAN_POINT('Ctrl Pts',(-11.1708515595871,6.51465928753007,
10.8726677388568));
#118423=CARTESIAN_POINT('Ctrl Pts',(-11.1704749132637,6.51442498922441,
10.8692507822105));
#118424=CARTESIAN_POINT('Ctrl Pts',(-11.1696612221101,6.51393991739212,
10.8621543752526));
#118425=CARTESIAN_POINT('Ctrl Pts',(-11.1692217684653,6.51368927710423,
10.8584752746962));
#118426=CARTESIAN_POINT('Ctrl Pts',(-11.1680177751548,6.5130311350681,10.848784033788));
#118427=CARTESIAN_POINT('Ctrl Pts',(-11.1672241679208,6.51262520103223,
10.8427755196371));
#118428=CARTESIAN_POINT('Ctrl Pts',(-11.1633164929477,6.51074740421205,
10.8148520936329));
#118429=CARTESIAN_POINT('Ctrl Pts',(-11.159631178728,6.50930420512535,10.7930200736271));
#118430=CARTESIAN_POINT('Ctrl Pts',(-11.1467961777879,6.50505804700152,
10.7281800828165));
#118431=CARTESIAN_POINT('Ctrl Pts',(-11.1358516230769,6.5023197365674,10.6855652547127));
#118432=CARTESIAN_POINT('Ctrl Pts',(-11.0947249586194,6.49389633131512,
10.5560074590836));
#118433=CARTESIAN_POINT('Ctrl Pts',(-11.0567345797142,6.48826107279846,
10.4719260396827));
#118434=CARTESIAN_POINT('Ctrl Pts',(-11.0016044054063,6.48128782741805,
10.3802340526167));
#118435=CARTESIAN_POINT('Ctrl Pts',(-10.9936095226019,6.4802996421887,10.367496009589));
#118436=CARTESIAN_POINT('Ctrl Pts',(-10.9811943762407,6.47879683705197,
10.3485317606691));
#118437=CARTESIAN_POINT('Ctrl Pts',(-10.9769536876819,6.47828878401259,
10.3421894205994));
#118438=CARTESIAN_POINT('Ctrl Pts',(-10.9692412522094,6.47737385615558,
10.3308938506353));
#118439=CARTESIAN_POINT('Ctrl Pts',(-10.9657923733862,6.47696784485768,
10.3259252761871));
#118440=CARTESIAN_POINT('Ctrl Pts',(-10.9621551520774,6.47654282839967,
10.3207705882591));
#118441=CARTESIAN_POINT('Ctrl Pts',(-10.9620048021144,6.47652526529023,
10.3205576616433));
#118442=CARTESIAN_POINT('Ctrl Pts',(-10.9617341699507,6.47649366145813,
10.3201746604881));
#118443=CARTESIAN_POINT('Ctrl Pts',(-10.9616139132548,6.4764796217014,10.3200045678625));
#118444=CARTESIAN_POINT('Ctrl Pts',(-10.961397585805,6.47645437224409,10.3196987636674));
#118445=CARTESIAN_POINT('Ctrl Pts',(-10.9613015314006,6.4764431631628,10.319563040485));
#118446=CARTESIAN_POINT('Ctrl Pts',(-10.9611288225856,6.47642301295004,
10.319319115533));
#118447=CARTESIAN_POINT('Ctrl Pts',(-10.9610521786254,6.47641407221492,
10.3192109063426));
#118448=CARTESIAN_POINT('Ctrl Pts',(-10.960914419698,6.47639800482786,10.3190164820757));
#118449=CARTESIAN_POINT('Ctrl Pts',(-10.9608533113843,6.47639087842781,
10.3189302622565));
#118450=CARTESIAN_POINT('Ctrl Pts',(-10.9567595664819,6.47591353043197,
10.313155904505));
#118451=CARTESIAN_POINT('Ctrl Pts',(-10.9526765848592,6.47544140561772,
10.3075037901762));
#118452=CARTESIAN_POINT('Ctrl Pts',(-10.9441014310368,6.4744578185113,10.2958524897032));
#118453=CARTESIAN_POINT('Ctrl Pts',(-10.9396017112942,6.47394608042074,
10.2898592759349));
#118454=CARTESIAN_POINT('Ctrl Pts',(-10.9279345186782,6.47263011900641,
10.2746246752531));
#118455=CARTESIAN_POINT('Ctrl Pts',(-10.9206861767294,6.47182280728793,
10.2654465439755));
#118456=CARTESIAN_POINT('Ctrl Pts',(-10.899010914347,6.46943762440835,10.2388253882844));
#118457=CARTESIAN_POINT('Ctrl Pts',(-10.8842170660407,6.46784588929161,
10.2216893432562));
#118458=CARTESIAN_POINT('Ctrl Pts',(-10.8259012126992,6.46170513764661,
10.1579505000429));
#118459=CARTESIAN_POINT('Ctrl Pts',(-10.7791183195288,6.45704047028252,
10.1144870315301));
#118460=CARTESIAN_POINT('Ctrl Pts',(-10.6806149535299,6.44783599438381,
10.0368476926493));
#118461=CARTESIAN_POINT('Ctrl Pts',(-10.629246720199,6.44331249685648,10.0025286438084));
#118462=CARTESIAN_POINT('Ctrl Pts',(-10.5670520870114,6.43830829164045,
9.96770206869916));
#118463=CARTESIAN_POINT('Ctrl Pts',(-10.5586247063069,6.43763978817619,
9.96311739323915));
#118464=CARTESIAN_POINT('Ctrl Pts',(-10.5456798268929,6.43662847756751,
9.95627874596362));
#118465=CARTESIAN_POINT('Ctrl Pts',(-10.5412025203919,6.43628149125897,
9.9539501140723));
#118466=CARTESIAN_POINT('Ctrl Pts',(-10.5336351595802,6.4356999025399,9.95007594852423));
#118467=CARTESIAN_POINT('Ctrl Pts',(-10.530553054412,6.43546437968896,9.94851511896717));
#118468=CARTESIAN_POINT('Ctrl Pts',(-10.5241794531227,6.43498017951108,
9.94532258068705));
#118469=CARTESIAN_POINT('Ctrl Pts',(-10.5208871266898,6.43473161128179,
9.94369267726372));
#118470=CARTESIAN_POINT('Ctrl Pts',(-10.5122719052983,6.43408506184391,
9.93947768899875));
#118471=CARTESIAN_POINT('Ctrl Pts',(-10.5069369788951,6.43368854995923,
9.93691722798775));
#118472=CARTESIAN_POINT('Ctrl Pts',(-10.4829410806476,6.43192131550433,
9.92562227941228));
#118473=CARTESIAN_POINT('Ctrl Pts',(-10.4640708914842,6.43057530843563,
9.91733758482847));
#118474=CARTESIAN_POINT('Ctrl Pts',(-10.4088184902817,6.42673207738054,
9.89479010534935));
#118475=CARTESIAN_POINT('Ctrl Pts',(-10.3719303602719,6.42428596659195,
9.8818364482973));
#118476=CARTESIAN_POINT('Ctrl Pts',(-10.2760182156491,6.4180720185036,9.85342920792167));
#118477=CARTESIAN_POINT('Ctrl Pts',(-10.2163181946885,6.41433691856388,
9.84068256519486));
#118478=CARTESIAN_POINT('Ctrl Pts',(-10.1134751395846,6.40781166946424,
9.82694822893905));
#118479=CARTESIAN_POINT('Ctrl Pts',(-10.0707767319115,6.40507765948761,
9.82359993246088));
#118480=CARTESIAN_POINT('Ctrl Pts',(-10.0159877731083,6.40148502921441,
9.82229728578206));
#118481=CARTESIAN_POINT('Ctrl Pts',(-10.0039783204683,6.40069248273311,
9.82219549683343));
#118482=CARTESIAN_POINT('Ctrl Pts',(-9.98499530024241,6.39943074911249,
9.82232493155173));
#118483=CARTESIAN_POINT('Ctrl Pts',(-9.97802152927992,6.39896531426812,
9.82243443869749));
#118484=CARTESIAN_POINT('Ctrl Pts',(-9.96503141139489,6.39809459135314,
9.82275385038394));
#118485=CARTESIAN_POINT('Ctrl Pts',(-9.95901487699916,6.39768980472283,
9.82294795511619));
#118486=CARTESIAN_POINT('Ctrl Pts',(-9.94721752970901,6.39689303775286,
9.82341912057908));
#118487=CARTESIAN_POINT('Ctrl Pts',(-9.94143674205579,6.39650117696969,
9.82369268567168));
#118488=CARTESIAN_POINT('Ctrl Pts',(-9.92841544259355,6.3956151669874,9.82440511673336));
#118489=CARTESIAN_POINT('Ctrl Pts',(-9.92117655154485,6.39512028112661,
9.82486828895023));
#118490=CARTESIAN_POINT('Ctrl Pts',(-9.90045467898295,6.39369676742912,
9.82638648165186));
#118491=CARTESIAN_POINT('Ctrl Pts',(-9.88698534657606,6.39276312490249,
9.82760688191719));
#118492=CARTESIAN_POINT('Ctrl Pts',(-9.85267089459624,6.3903625670311,9.8313127805553));
#118493=CARTESIAN_POINT('Ctrl Pts',(-9.8318664609301,6.38888625823141,9.83412406193983));
#118494=CARTESIAN_POINT('Ctrl Pts',(-9.81114930150153,6.38739526456853,
9.83748958018578));
#118495=CARTESIAN_POINT('Ctrl Pts',(-9.81114930150925,6.28889384320256,
9.83748958018452));
#118496=CARTESIAN_POINT('Ctrl Pts',(-9.83217396752733,6.29030852489224,
9.83407410726026));
#118497=CARTESIAN_POINT('Ctrl Pts',(-9.85328916382042,6.29169514151888,
9.83122934520844));
#118498=CARTESIAN_POINT('Ctrl Pts',(-9.89617828576813,6.29446374418358,
9.82663189519018));
#118499=CARTESIAN_POINT('Ctrl Pts',(-9.91794655001183,6.29584420572935,
9.82490894845336));
#118500=CARTESIAN_POINT('Ctrl Pts',(-9.96063918496295,6.29852432224818,
9.82272210337179));
#118501=CARTESIAN_POINT('Ctrl Pts',(-9.98155255812689,6.29982444267296,
9.82220874040484));
#118502=CARTESIAN_POINT('Ctrl Pts',(-10.0524501001525,6.30421865218534,
9.82235736437935));
#118503=CARTESIAN_POINT('Ctrl Pts',(-10.102372720044,6.3072926477863,9.82564363432128));
#118504=CARTESIAN_POINT('Ctrl Pts',(-10.2006291928598,6.3135028030339,9.83842596070636));
#118505=CARTESIAN_POINT('Ctrl Pts',(-10.2488742064699,6.31663088569745,
9.8477990283414));
#118506=CARTESIAN_POINT('Ctrl Pts',(-10.3073797526552,6.32060025391447,
9.86301200751928));
#118507=CARTESIAN_POINT('Ctrl Pts',(-10.3183274550742,6.32135062903676,
9.86602838480624));
#118508=CARTESIAN_POINT('Ctrl Pts',(-10.3357227821993,6.32255595410178,
9.87109300102004));
#118509=CARTESIAN_POINT('Ctrl Pts',(-10.3421995154701,6.32300763235351,
9.87303935861515));
#118510=CARTESIAN_POINT('Ctrl Pts',(-10.3544446705997,6.32386728313721,
9.87683450587686));
#118511=CARTESIAN_POINT('Ctrl Pts',(-10.3602163124535,6.32427488629912,
9.87867223453655));
#118512=CARTESIAN_POINT('Ctrl Pts',(-10.3733205341226,6.325205964905,9.88295631662731));
#118513=CARTESIAN_POINT('Ctrl Pts',(-10.3806436572598,6.32573032970159,
9.88543048084908));
#118514=CARTESIAN_POINT('Ctrl Pts',(-10.4031323625625,6.32735340456808,
9.8932759154381));
#118515=CARTESIAN_POINT('Ctrl Pts',(-10.4182121084477,6.32845983122719,
9.89888579649363));
#118516=CARTESIAN_POINT('Ctrl Pts',(-10.5027427225827,6.33476789642603,
9.93231927577882));
#118517=CARTESIAN_POINT('Ctrl Pts',(-10.5695219883126,6.34017597535457,
9.96639777855707));
#118518=CARTESIAN_POINT('Ctrl Pts',(-10.6729950598149,6.34916657788513,
10.0322886833606));
#118519=CARTESIAN_POINT('Ctrl Pts',(-10.7117765736319,6.35269340505642,
10.0604459187035));
#118520=CARTESIAN_POINT('Ctrl Pts',(-10.7739054899705,6.35851980659507,
10.1116146854433));
#118521=CARTESIAN_POINT('Ctrl Pts',(-10.798204808411,6.3608489191406,10.133381467443));
#118522=CARTESIAN_POINT('Ctrl Pts',(-10.8264410490351,6.36358818697766,
10.1608716172262));
#118523=CARTESIAN_POINT('Ctrl Pts',(-10.8312695829954,6.36405782680935,
10.1656546661223));
#118524=CARTESIAN_POINT('Ctrl Pts',(-10.8387795772585,6.36478980571842,
10.1732238332109));
#118525=CARTESIAN_POINT('Ctrl Pts',(-10.8414890907739,6.36505421310971,
10.1759817232688));
#118526=CARTESIAN_POINT('Ctrl Pts',(-10.8465670431253,6.36555026022516,
10.1812015062211));
#118527=CARTESIAN_POINT('Ctrl Pts',(-10.8489383433094,6.36578210809694,
10.1836603516253));
#118528=CARTESIAN_POINT('Ctrl Pts',(-10.854427909427,6.36631937956946,10.1894023739248));
#118529=CARTESIAN_POINT('Ctrl Pts',(-10.8575379832642,6.36662418651468,
10.1926932598141));
#118530=CARTESIAN_POINT('Ctrl Pts',(-10.8677259934319,6.3676243999898,10.2035988819598));
#118531=CARTESIAN_POINT('Ctrl Pts',(-10.8747223244253,6.36831404309873,
10.2112896515093));
#118532=CARTESIAN_POINT('Ctrl Pts',(-10.9275832057929,6.37355557130202,
10.2709661276993));
#118533=CARTESIAN_POINT('Ctrl Pts',(-10.9688851040908,6.37783792873874,
10.3268245004164));
#118534=CARTESIAN_POINT('Ctrl Pts',(-11.0354983911175,6.38574235523404,
10.4358614179606));
#118535=CARTESIAN_POINT('Ctrl Pts',(-11.0622057174546,6.38935136529559,
10.4879183076003));
#118536=CARTESIAN_POINT('Ctrl Pts',(-11.0933340670707,6.39444393097727,
10.5616152592759));
#118537=CARTESIAN_POINT('Ctrl Pts',(-11.101180893692,6.39583073523075,10.5817164608792));
#118538=CARTESIAN_POINT('Ctrl Pts',(-11.1139528173571,6.39828998263429,
10.6172894549519));
#118539=CARTESIAN_POINT('Ctrl Pts',(-11.1191184439728,6.39935478400995,
10.6326689401085));
#118540=CARTESIAN_POINT('Ctrl Pts',(-11.1262813850154,6.40094375495417,
10.6555505188657));
#118541=CARTESIAN_POINT('Ctrl Pts',(-11.1285249876063,6.40145998777256,
10.6629739611946));
#118542=CARTESIAN_POINT('Ctrl Pts',(-11.1323908979861,6.40238383991421,
10.6762367528507));
#118543=CARTESIAN_POINT('Ctrl Pts',(-11.1340417690815,6.40279052546244,
10.6820675391139));
#118544=CARTESIAN_POINT('Ctrl Pts',(-11.13743582127,6.40365318382968,10.6944180016443));
#118545=CARTESIAN_POINT('Ctrl Pts',(-11.1391681039494,6.40410948881517,
10.7009404191445));
#118546=CARTESIAN_POINT('Ctrl Pts',(-11.1436481533967,6.40533395956629,
10.7184126958472));
#118547=CARTESIAN_POINT('Ctrl Pts',(-11.1462946371025,6.40610530556393,
10.7293875497957));
#118548=CARTESIAN_POINT('Ctrl Pts',(-11.158108550393,6.40979124284393,10.7816662056745));
#118549=CARTESIAN_POINT('Ctrl Pts',(-11.1652026957464,6.41276975924071,
10.8234016250495));
#118550=CARTESIAN_POINT('Ctrl Pts',(-11.1825361006483,6.42364956251278,
10.974102466896));
#118551=CARTESIAN_POINT('Ctrl Pts',(-11.1798333680014,6.43187006434389,
11.0839791656808));
#118552=CARTESIAN_POINT('Ctrl Pts',(-11.1603686901995,6.44032657929434,
11.2018444576054));
#118553=CARTESIAN_POINT('Ctrl Pts',(-11.1585984920666,6.44103526499194,
11.2117692887905));
#118554=CARTESIAN_POINT('Ctrl Pts',(-11.1552331384942,6.44228179030265,
11.2293300709823));
#118555=CARTESIAN_POINT('Ctrl Pts',(-11.153689167492,6.44282195479856,11.2369751013588));
#118556=CARTESIAN_POINT('Ctrl Pts',(-11.1512220756028,6.4436385708266,11.2485949247318));
#118557=CARTESIAN_POINT('Ctrl Pts',(-11.1503540915028,6.44391791434338,
11.252581015481));
#118558=CARTESIAN_POINT('Ctrl Pts',(-11.1487278000906,6.44442698106938,
11.2598672129701));
#118559=CARTESIAN_POINT('Ctrl Pts',(-11.1479759674725,6.44465704604658,
11.2631685881364));
#118560=CARTESIAN_POINT('Ctrl Pts',(-11.1462391511918,6.44517681391507,
11.2706460401156));
#118561=CARTESIAN_POINT('Ctrl Pts',(-11.1452455770436,6.44546603089243,
11.2748200146712));
#118562=CARTESIAN_POINT('Ctrl Pts',(-11.1425990859452,6.44621594308083,
11.2856741963277));
#118563=CARTESIAN_POINT('Ctrl Pts',(-11.1409103644785,6.44667471364137,
11.2923456231267));
#118564=CARTESIAN_POINT('Ctrl Pts',(-11.1259577532096,6.45057671105032,
11.349313340769));
#118565=CARTESIAN_POINT('Ctrl Pts',(-11.109431945306,6.45385723645849,11.3987014531337));
#118566=CARTESIAN_POINT('Ctrl Pts',(-11.0854280758571,6.45779638413193,
11.4572387343791));
#118567=CARTESIAN_POINT('Ctrl Pts',(-11.081015482048,6.45849391788365,11.4675755556586));
#118568=CARTESIAN_POINT('Ctrl Pts',(-11.0557855815724,6.46234744014686,
11.5244113753327));
#118569=CARTESIAN_POINT('Ctrl Pts',(-11.0321166870885,6.4654808309648,11.5695835854562));
#118570=CARTESIAN_POINT('Ctrl Pts',(-10.9807448891762,6.47167249639648,
11.6538455159632));
#118571=CARTESIAN_POINT('Ctrl Pts',(-10.9534389330596,6.47471717707662,
11.6930569124288));
#118572=CARTESIAN_POINT('Ctrl Pts',(-10.9168388029762,6.47859250628929,
11.7393434710986));
#118573=CARTESIAN_POINT('Ctrl Pts',(-10.9097198733394,6.47933758263407,
11.7480854874865));
#118574=CARTESIAN_POINT('Ctrl Pts',(-10.8981428532842,6.48053639877852,
11.7618923644829));
#118575=CARTESIAN_POINT('Ctrl Pts',(-10.893764719189,6.48098692967035,11.76702358732));
#118576=CARTESIAN_POINT('Ctrl Pts',(-10.8853695264092,6.48184568587702,
11.7766933732516));
#118577=CARTESIAN_POINT('Ctrl Pts',(-10.8813610250861,6.48225355288609,
11.7812391026142));
#118578=CARTESIAN_POINT('Ctrl Pts',(-10.8721397774403,6.48318704586131,
11.7915349045038));
#118579=CARTESIAN_POINT('Ctrl Pts',(-10.8669049655136,6.48371357844924,
11.7972647441227));
#118580=CARTESIAN_POINT('Ctrl Pts',(-10.8505321523428,6.48535028959538,
11.8148339331578));
#118581=CARTESIAN_POINT('Ctrl Pts',(-10.8392058027676,6.4864683737595,11.8264943168244));
#118582=CARTESIAN_POINT('Ctrl Pts',(-10.777077899462,6.4925299012312,11.8878604587627));
#118583=CARTESIAN_POINT('Ctrl Pts',(-10.7221048432263,6.49765733572671,
11.9331172455703));
#118584=CARTESIAN_POINT('Ctrl Pts',(-10.6148703370555,6.50716076011914,
12.0062201081526));
#118585=CARTESIAN_POINT('Ctrl Pts',(-10.5639346196445,6.51149630259752,
12.0356266774468));
#118586=CARTESIAN_POINT('Ctrl Pts',(-10.4952995125897,6.51697469563982,
12.0686803852398));
#118587=CARTESIAN_POINT('Ctrl Pts',(-10.4794155378241,6.51821831385074,
12.0758997074673));
#118588=CARTESIAN_POINT('Ctrl Pts',(-10.4524915447586,6.52027960564922,
12.0874220152448));
#118589=CARTESIAN_POINT('Ctrl Pts',(-10.4415367161865,6.52110560947637,
12.09191601888));
#118590=CARTESIAN_POINT('Ctrl Pts',(-10.4260295246585,6.52225531395607,
12.0980059808534));
#118591=CARTESIAN_POINT('Ctrl Pts',(-10.4215327062809,6.52258641956077,
12.099740182698));
#118592=CARTESIAN_POINT('Ctrl Pts',(-10.4138007681067,6.52315166112207,
12.102667617511));
#118593=CARTESIAN_POINT('Ctrl Pts',(-10.410570853343,6.52338656965778,12.1038743252981));
#118594=CARTESIAN_POINT('Ctrl Pts',(-10.4038022880098,6.5238762533397,12.1063692670518));
#118595=CARTESIAN_POINT('Ctrl Pts',(-10.4002627091289,6.52413086939655,
12.1076547330098));
#118596=CARTESIAN_POINT('Ctrl Pts',(-10.3907495202915,6.52481143338115,
12.111058073576));
#118597=CARTESIAN_POINT('Ctrl Pts',(-10.3847647776579,6.52523561574829,
12.1131447797846));
#118598=CARTESIAN_POINT('Ctrl Pts',(-10.3573243603021,6.52716372399278,
12.1224647051404));
#118599=CARTESIAN_POINT('Ctrl Pts',(-10.3356781923197,6.52863797809679,
12.1291271066355));
#118600=CARTESIAN_POINT('Ctrl Pts',(-10.2928662884244,6.53148740729562,
12.1409638269983));
#118601=CARTESIAN_POINT('Ctrl Pts',(-10.2717229373381,6.53286364770264,
12.1461831666583));
#118602=CARTESIAN_POINT('Ctrl Pts',(-10.1835314371377,6.53852065877968,
12.165375865962));
#118603=CARTESIAN_POINT('Ctrl Pts',(-10.1154737109269,6.54269578734149,
12.1740744920734));
#118604=CARTESIAN_POINT('Ctrl Pts',(-9.99608463157067,6.55017420278105,
12.1788472333208));
#118605=CARTESIAN_POINT('Ctrl Pts',(-9.94505199112209,6.55341817142289,
12.1775720315404));
#118606=CARTESIAN_POINT('Ctrl Pts',(-9.88285008625814,6.55751812484059,
12.1719651685598));
#118607=CARTESIAN_POINT('Ctrl Pts',(-9.87144953293953,6.55827546716636,
12.1707694994951));
#118608=CARTESIAN_POINT('Ctrl Pts',(-9.85333053289396,6.55948935077882,
12.1686013781829));
#118609=CARTESIAN_POINT('Ctrl Pts',(-9.8465997156234,6.55994253705385,12.1677368980973));
#118610=CARTESIAN_POINT('Ctrl Pts',(-9.83388019347696,6.56080338665888,
12.1659913848843));
#118611=CARTESIAN_POINT('Ctrl Pts',(-9.82789005624522,6.56121066620264,
12.1651222530967));
#118612=CARTESIAN_POINT('Ctrl Pts',(-9.81430545551029,6.56213868460753,
12.1630441668263));
#118613=CARTESIAN_POINT('Ctrl Pts',(-9.80671566338288,6.56266029086538,
12.1618069367191));
#118614=CARTESIAN_POINT('Ctrl Pts',(-9.78349302348635,6.56426611662105,
12.1577875070688));
#118615=CARTESIAN_POINT('Ctrl Pts',(-9.76790442400641,6.56535781693441,
12.1547635184029));
#118616=CARTESIAN_POINT('Ctrl Pts',(-9.6716195683883,6.57218973020986,12.134057158988));
#118617=CARTESIAN_POINT('Ctrl Pts',(-9.59292224727309,6.5781873523608,12.1082429432195));
#118618=CARTESIAN_POINT('Ctrl Pts',(-9.45440275226747,6.58932858620843,
12.0460476673394));
#118619=CARTESIAN_POINT('Ctrl Pts',(-9.39383852667254,6.59442557723975,
12.0121572030866));
#118620=CARTESIAN_POINT('Ctrl Pts',(-9.32908415561941,6.59990767598515,
11.9680132882963));
#118621=CARTESIAN_POINT('Ctrl Pts',(-9.32162788354656,6.60053930203682,
11.962802721637));
#118622=CARTESIAN_POINT('Ctrl Pts',(-9.31070566703958,6.60146422996624,
11.9549802109705));
#118623=CARTESIAN_POINT('Ctrl Pts',(-9.30719279671884,6.60176166400383,
11.9524348068935));
#118624=CARTESIAN_POINT('Ctrl Pts',(-9.3009610903509,6.60228910188104,11.9478666296448));
#118625=CARTESIAN_POINT('Ctrl Pts',(-9.29823683661112,6.60251960076676,
11.9458514726241));
#118626=CARTESIAN_POINT('Ctrl Pts',(-9.29228283922467,6.60302319188202,
11.9414073573419));
#118627=CARTESIAN_POINT('Ctrl Pts',(-9.2890568732937,6.60329594544645,11.9389735160922));
#118628=CARTESIAN_POINT('Ctrl Pts',(-9.27996082033554,6.60406493081268,
11.9320372151194));
#118629=CARTESIAN_POINT('Ctrl Pts',(-9.27412041406071,6.60455858617302,
11.9274958890501));
#118630=CARTESIAN_POINT('Ctrl Pts',(-9.23431913559704,6.60792510773057,
11.8959413440579));
#118631=CARTESIAN_POINT('Ctrl Pts',(-9.20182695212705,6.61068579222854,
11.8671209595094));
#118632=CARTESIAN_POINT('Ctrl Pts',(-9.15702365623844,6.61463605337505,
11.8227228665574));
#118633=CARTESIAN_POINT('Ctrl Pts',(-9.14339955577342,6.61585857508875,
11.8085281331262));
#118634=CARTESIAN_POINT('Ctrl Pts',(-9.09690669654099,6.62013275218794,
11.7575930127024));
#118635=CARTESIAN_POINT('Ctrl Pts',(-9.06599522280667,6.62316471111318,
11.7191381151035));
#118636=CARTESIAN_POINT('Ctrl Pts',(-9.00898528464385,6.62936134108222,
11.6383154973168));
#118637=CARTESIAN_POINT('Ctrl Pts',(-8.98298004644003,6.63252073355408,
11.5960086909625));
#118638=CARTESIAN_POINT('Ctrl Pts',(-8.95438357439872,6.63652539132615,
11.5421355674871));
#118639=CARTESIAN_POINT('Ctrl Pts',(-8.94919189064131,6.63727769351883,
11.5320028059577));
#118640=CARTESIAN_POINT('Ctrl Pts',(-8.94114895842337,6.63848538580078,
11.5157279879783));
#118641=CARTESIAN_POINT('Ctrl Pts',(-8.93820228517077,6.63893748124079,
11.5096336874575));
#118642=CARTESIAN_POINT('Ctrl Pts',(-8.93271931447399,6.63979746110695,
11.498039832924));
#118643=CARTESIAN_POINT('Ctrl Pts',(-8.93017257208598,6.64020497216094,
11.4925454385248));
#118644=CARTESIAN_POINT('Ctrl Pts',(-8.92447650368585,6.64113519158471,
11.4800040085575));
#118645=CARTESIAN_POINT('Ctrl Pts',(-8.92135388123496,6.64165878315078,
11.4729452240182));
#118646=CARTESIAN_POINT('Ctrl Pts',(-8.91196054369535,6.64327701144146,
11.4511342872184));
#118647=CARTESIAN_POINT('Ctrl Pts',(-8.90592165865342,6.64437929813376,
11.4362849330254));
#118648=CARTESIAN_POINT('Ctrl Pts',(-8.87222635461074,6.65091498288681,
11.3483263388159));
#118649=CARTESIAN_POINT('Ctrl Pts',(-8.85160518327261,6.65657587018532,
11.2727453069239));
#118650=CARTESIAN_POINT('Ctrl Pts',(-8.82642492560129,6.66768942697238,
11.1233083210996));
#118651=CARTESIAN_POINT('Ctrl Pts',(-8.82102086386312,6.67310554175141,
11.0499353294086));
#118652=CARTESIAN_POINT('Ctrl Pts',(-8.82266590935937,6.67888099350935,
10.9673966547548));
#118653=CARTESIAN_POINT('Ctrl Pts',(-8.82295426711707,6.67951549620996,
10.9582639893612));
#118654=CARTESIAN_POINT('Ctrl Pts',(-8.82353657371618,6.68044380326055,
10.9447935235844));
#118655=CARTESIAN_POINT('Ctrl Pts',(-8.82374829339999,6.68074178191599,
10.9404527695534));
#118656=CARTESIAN_POINT('Ctrl Pts',(-8.8241678784361,6.68126980138062,10.9327291285926));
#118657=CARTESIAN_POINT('Ctrl Pts',(-8.82436632319345,6.68150034176889,
10.9293458623558));
#118658=CARTESIAN_POINT('Ctrl Pts',(-8.82483302657028,6.68200357262701,
10.9219363853628));
#118659=CARTESIAN_POINT('Ctrl Pts',(-8.8251073727273,6.68227592811037,10.9179106647281));
#118660=CARTESIAN_POINT('Ctrl Pts',(-8.8259413280288,6.68304270931541,10.9065354415489));
#118661=CARTESIAN_POINT('Ctrl Pts',(-8.82654925886707,6.68353458164326,
10.8991895151856));
#118662=CARTESIAN_POINT('Ctrl Pts',(-8.83096961497361,6.68672542202354,
10.8512555654499));
#118663=CARTESIAN_POINT('Ctrl Pts',(-8.836818688758,6.68932573401529,10.8108784900547));
#118664=CARTESIAN_POINT('Ctrl Pts',(-8.85791915835156,6.69613316472432,
10.7044866323357));
#118665=CARTESIAN_POINT('Ctrl Pts',(-8.87678663683874,6.7002607983372,10.6393491803509));
#118666=CARTESIAN_POINT('Ctrl Pts',(-8.92029880942133,6.70781748696491,
10.5265303502385));
#118667=CARTESIAN_POINT('Ctrl Pts',(-8.94279447390394,6.71119708577969,
10.4782303320154));
#118668=CARTESIAN_POINT('Ctrl Pts',(-8.97406530778238,6.71544978720752,
10.4214784669267));
#118669=CARTESIAN_POINT('Ctrl Pts',(-8.97980285440935,6.71621472292437,
10.4114195674998));
#118670=CARTESIAN_POINT('Ctrl Pts',(-8.98914929746522,6.71743793412615,
10.3955810104814));
#118671=CARTESIAN_POINT('Ctrl Pts',(-8.99266173119407,6.71789276279152,
10.3897450806246));
#118672=CARTESIAN_POINT('Ctrl Pts',(-8.99938844587789,6.71875494623751,
10.3787849278232));
#118673=CARTESIAN_POINT('Ctrl Pts',(-9.00259197809741,6.71916190168266,
10.373654341718));
#118674=CARTESIAN_POINT('Ctrl Pts',(-9.00993541856415,6.7200867254438,10.3620927325341));
#118675=CARTESIAN_POINT('Ctrl Pts',(-9.01409870278219,6.72060543814387,
10.3556769562781));
#118676=CARTESIAN_POINT('Ctrl Pts',(-9.02697588364101,6.72219329228768,
10.3362497807862));
#118677=CARTESIAN_POINT('Ctrl Pts',(-9.03588675289696,6.72326967283151,
10.3233716748229));
#118678=CARTESIAN_POINT('Ctrl Pts',(-9.09593158010532,6.73038361239888,
10.2401891799696));
#118679=CARTESIAN_POINT('Ctrl Pts',(-9.15445050236053,6.73670990898075,
10.1755650998434));
#118680=CARTESIAN_POINT('Ctrl Pts',(-9.27001121821062,6.74803414866175,
10.0733097001899));
#118681=CARTESIAN_POINT('Ctrl Pts',(-9.32423839146912,6.75298227860817,
10.0330528743344));
#118682=CARTESIAN_POINT('Ctrl Pts',(-9.38823085442226,6.75822377886304,
9.9935736680313));
#118683=CARTESIAN_POINT('Ctrl Pts',(-9.3948848540847,6.75876196901004,9.98955894908117));
#118684=CARTESIAN_POINT('Ctrl Pts',(-9.40508687247327,6.75957622831783,
9.9835404448594));
#118685=CARTESIAN_POINT('Ctrl Pts',(-9.40860620521168,6.75985516483237,
9.98148881337406));
#118686=CARTESIAN_POINT('Ctrl Pts',(-9.41507045712849,6.76036384472535,
9.97776521324488));
#118687=CARTESIAN_POINT('Ctrl Pts',(-9.41801196564356,6.76059392634019,
9.97608767082733));
#118688=CARTESIAN_POINT('Ctrl Pts',(-9.42470299523363,6.76111417561724,
9.97230992657975));
#118689=CARTESIAN_POINT('Ctrl Pts',(-9.42845680975917,6.76140385333729,
9.97021754052496));
#118690=CARTESIAN_POINT('Ctrl Pts',(-9.43827161982545,6.76215577507538,
9.96481694025215));
#118691=CARTESIAN_POINT('Ctrl Pts',(-9.44435050565404,6.7626160774822,9.96154134157663));
#118692=CARTESIAN_POINT('Ctrl Pts',(-9.50163282923052,6.76690645690041,
9.93132186900783));
#118693=CARTESIAN_POINT('Ctrl Pts',(-9.55473499849234,6.77053462237589,
9.90812834394334));
#118694=CARTESIAN_POINT('Ctrl Pts',(-9.67495745459185,6.77844663222738,
9.86585658195173));
#118695=CARTESIAN_POINT('Ctrl Pts',(-9.74249234371883,6.78270439926348,
9.84864295499058));
#118696=CARTESIAN_POINT('Ctrl Pts',(-9.81114930160613,6.78711399980274,
9.83748958016879));
#118697=CARTESIAN_POINT('Origin',(-10.,2.67563288526385,11.));
#118698=CARTESIAN_POINT('',(-9.8111493015013,7.38550319809767,9.83748958018582));
#118699=CARTESIAN_POINT('',(-9.81114930363318,7.28726551493505,9.83748957983949));
#118700=CARTESIAN_POINT('',(-9.81114930150157,2.67563288526385,9.83748958018577));
#118701=CARTESIAN_POINT('Ctrl Pts',(-9.81114930150104,7.38550319809767,
9.83748958018586));
#118702=CARTESIAN_POINT('Ctrl Pts',(-9.80456303233157,7.38503940439618,
9.83855952460266));
#118703=CARTESIAN_POINT('Ctrl Pts',(-9.79798577865897,7.38457827590337,
9.83968545392653));
#118704=CARTESIAN_POINT('Ctrl Pts',(-9.78758650275148,7.38385277612494,
9.84155676596716));
#118705=CARTESIAN_POINT('Ctrl Pts',(-9.78375811782733,7.3835864637623,9.842265285228));
#118706=CARTESIAN_POINT('Ctrl Pts',(-9.77691868855482,7.38311216271557,
9.84356616820762));
#118707=CARTESIAN_POINT('Ctrl Pts',(-9.7739064420784,7.38290378759597,9.84415131518379));
#118708=CARTESIAN_POINT('Ctrl Pts',(-9.76661894261053,7.38240088247456,
9.84559653462716));
#118709=CARTESIAN_POINT('Ctrl Pts',(-9.76234613458593,7.38210702485039,
9.84646858708479));
#118710=CARTESIAN_POINT('Ctrl Pts',(-9.74906321936703,7.38119636107075,
9.84925648196381));
#118711=CARTESIAN_POINT('Ctrl Pts',(-9.74007041987291,7.38058391921619,
9.85125436304195));
#118712=CARTESIAN_POINT('Ctrl Pts',(-9.71893001031958,7.37915186468899,
9.85621198660835));
#118713=CARTESIAN_POINT('Ctrl Pts',(-9.70680406467292,7.37833646891464,
9.85926009580439));
#118714=CARTESIAN_POINT('Ctrl Pts',(-9.66270603997496,7.37538554060596,
9.87109471779888));
#118715=CARTESIAN_POINT('Ctrl Pts',(-9.63105843528758,7.37329537089962,
9.88103762883233));
#118716=CARTESIAN_POINT('Ctrl Pts',(-9.52737139324232,7.36641563649889,
9.91849214696055));
#118717=CARTESIAN_POINT('Ctrl Pts',(-9.45762028258616,7.36172300327169,
9.95173416871535));
#118718=CARTESIAN_POINT('Ctrl Pts',(-9.35964020421842,7.35448228980732,
10.0108442617877));
#118719=CARTESIAN_POINT('Ctrl Pts',(-9.32860172672824,7.35208260102111,
10.03164382885));
#118720=CARTESIAN_POINT('Ctrl Pts',(-9.28982078161402,7.3489098308116,10.0603936305447));
#118721=CARTESIAN_POINT('Ctrl Pts',(-9.28112722742756,7.34818668779305,
10.0670280950305));
#118722=CARTESIAN_POINT('Ctrl Pts',(-9.2672795991387,7.34701472896229,10.0779043393385));
#118723=CARTESIAN_POINT('Ctrl Pts',(-9.26206686668539,7.34656886689955,
10.0820706558163));
#118724=CARTESIAN_POINT('Ctrl Pts',(-9.25217315152062,7.34571342628298,
10.0901170238515));
#118725=CARTESIAN_POINT('Ctrl Pts',(-9.24748624403664,7.34530415896303,
10.0939894756124));
#118726=CARTESIAN_POINT('Ctrl Pts',(-9.23677521076191,7.3443594157383,10.1029796753242));
#118727=CARTESIAN_POINT('Ctrl Pts',(-9.23077226108025,7.34382295455406,
10.1081220811151));
#118728=CARTESIAN_POINT('Ctrl Pts',(-9.21200569764494,7.34212332684976,
10.1245287961239));
#118729=CARTESIAN_POINT('Ctrl Pts',(-9.19943478365673,7.34095135453911,
10.1360091832843));
#118730=CARTESIAN_POINT('Ctrl Pts',(-9.17048907591853,7.33817120173341,
10.163618055932));
#118731=CARTESIAN_POINT('Ctrl Pts',(-9.15432929260231,7.33655446075115,
10.1799609376487));
#118732=CARTESIAN_POINT('Ctrl Pts',(-9.05778883399869,7.32648686664703,
10.2834851768497));
#118733=CARTESIAN_POINT('Ctrl Pts',(-8.99049244071223,7.3175536507483,10.3819031745628));
#118734=CARTESIAN_POINT('Ctrl Pts',(-8.93248258652605,7.30808615503733,
10.5022763849072));
#118735=CARTESIAN_POINT('Ctrl Pts',(-8.92620020751459,7.30702911785883,
10.5159790467937));
#118736=CARTESIAN_POINT('Ctrl Pts',(-8.91800188295383,7.30560824256921,
10.5348065309434));
#118737=CARTESIAN_POINT('Ctrl Pts',(-8.91585631079926,7.30523221700577,
10.5398289958871));
#118738=CARTESIAN_POINT('Ctrl Pts',(-8.91250166047466,7.30463776016894,
10.5478354422089));
#118739=CARTESIAN_POINT('Ctrl Pts',(-8.91126977899309,7.30441801459158,
10.5508096925675));
#118740=CARTESIAN_POINT('Ctrl Pts',(-8.90872415355256,7.30396091668772,
10.5570278365203));
#118741=CARTESIAN_POINT('Ctrl Pts',(-8.90741265167142,7.30372370933032,
10.560272587438));
#118742=CARTESIAN_POINT('Ctrl Pts',(-8.90422529158039,7.30314286077923,
10.5682606481716));
#118743=CARTESIAN_POINT('Ctrl Pts',(-8.90236571758186,7.30280016871734,
10.5730104638729));
#118744=CARTESIAN_POINT('Ctrl Pts',(-8.89562932086222,7.30154394081403,
10.5905517553367));
#118745=CARTESIAN_POINT('Ctrl Pts',(-8.89094454521518,7.3006408612127,10.6034164655634));
#118746=CARTESIAN_POINT('Ctrl Pts',(-8.87955002463621,7.29835842348968,
10.6364891133431));
#118747=CARTESIAN_POINT('Ctrl Pts',(-8.87316178153946,7.29699334100039,
10.6568031911077));
#118748=CARTESIAN_POINT('Ctrl Pts',(-8.85191482947508,7.29207805213374,
10.7313751830044));
#118749=CARTESIAN_POINT('Ctrl Pts',(-8.84039641839956,7.28862351479121,
10.7865074311745));
#118750=CARTESIAN_POINT('Ctrl Pts',(-8.8229928731511,7.28057667350593,10.9152737878085));
#118751=CARTESIAN_POINT('Ctrl Pts',(-8.8199990222924,7.27597410674167,10.9890482038267));
#118752=CARTESIAN_POINT('Ctrl Pts',(-8.82456219839563,7.27034923467111,
11.0747594884836));
#118753=CARTESIAN_POINT('Ctrl Pts',(-8.82539693728081,7.26954673764853,
11.0868943824763));
#118754=CARTESIAN_POINT('Ctrl Pts',(-8.82700870101769,7.2682726846099,11.1059981266348));
#118755=CARTESIAN_POINT('Ctrl Pts',(-8.82766028607641,7.26780500676094,
11.1129769088182));
#118756=CARTESIAN_POINT('Ctrl Pts',(-8.82898817684258,7.26693141816832,
11.1259473117257));
#118757=CARTESIAN_POINT('Ctrl Pts',(-8.82964828058892,7.26652602330956,
11.131940387539));
#118758=CARTESIAN_POINT('Ctrl Pts',(-8.83121791404866,7.26562162790229,
11.1452510600789));
#118759=CARTESIAN_POINT('Ctrl Pts',(-8.83215020284632,7.2651219350284,11.1525656642507));
#118760=CARTESIAN_POINT('Ctrl Pts',(-8.83508644983624,7.26364972211495,
11.1739964360923));
#118761=CARTESIAN_POINT('Ctrl Pts',(-8.83727806427532,7.26267142525286,
11.1880851095267));
#118762=CARTESIAN_POINT('Ctrl Pts',(-8.84285733128236,7.26042271956303,
11.2201114531015));
#118763=CARTESIAN_POINT('Ctrl Pts',(-8.84640727737929,7.25914757484266,
11.2380167548423));
#118764=CARTESIAN_POINT('Ctrl Pts',(-8.85996441087032,7.254746660682,11.2989383483794));
#118765=CARTESIAN_POINT('Ctrl Pts',(-8.87197311069318,7.251565476542,11.3414673073801));
#118766=CARTESIAN_POINT('Ctrl Pts',(-8.90701833127548,7.24371355225981,
11.4433113409571));
#118767=CARTESIAN_POINT('Ctrl Pts',(-8.93252652934635,7.23901130237155,
11.5016315926436));
#118768=CARTESIAN_POINT('Ctrl Pts',(-8.97767572207397,7.23211037901414,
11.5856278747216));
#118769=CARTESIAN_POINT('Ctrl Pts',(-8.99386674205704,7.22983842498088,
11.6130278925004));
#118770=CARTESIAN_POINT('Ctrl Pts',(-9.0149183041041,7.22714266082391,11.6455674011038));
#118771=CARTESIAN_POINT('Ctrl Pts',(-9.01873921358551,7.22666283487739,
11.6513604929667));
#118772=CARTESIAN_POINT('Ctrl Pts',(-9.02480889384697,7.22591565596024,
11.6603884339836));
#118773=CARTESIAN_POINT('Ctrl Pts',(-9.02702299585082,7.22564615077735,
11.6636462369345));
#118774=CARTESIAN_POINT('Ctrl Pts',(-9.03098669086085,7.22516915062024,
11.669415893681));
#118775=CARTESIAN_POINT('Ctrl Pts',(-9.03272973832329,7.22496124100921,
11.6719320450926));
#118776=CARTESIAN_POINT('Ctrl Pts',(-9.0369414309462,7.22446326623873,11.6779614228233));
#118777=CARTESIAN_POINT('Ctrl Pts',(-9.03941950144486,7.22417383663789,
11.6814679783453));
#118778=CARTESIAN_POINT('Ctrl Pts',(-9.04707097245005,7.22329075848971,
11.6921704074906));
#118779=CARTESIAN_POINT('Ctrl Pts',(-9.05230660341444,7.22270110406661,
11.6993217014769));
#118780=CARTESIAN_POINT('Ctrl Pts',(-9.06475353300969,7.22133119295638,
11.7159262892428));
#118781=CARTESIAN_POINT('Ctrl Pts',(-9.07202834453338,7.2205546716017,11.7253309835701));
#118782=CARTESIAN_POINT('Ctrl Pts',(-9.09856091545684,7.21780078394325,
11.7585788647495));
#118783=CARTESIAN_POINT('Ctrl Pts',(-9.11860633332818,7.21586256867839,
11.781779882111));
#118784=CARTESIAN_POINT('Ctrl Pts',(-9.14360759288296,7.21357181614479,
11.8085311845212));
#118785=CARTESIAN_POINT('Ctrl Pts',(-9.14771288550749,7.21319951785788,
11.8128574948114));
#118786=CARTESIAN_POINT('Ctrl Pts',(-9.20752073031973,7.20782790407061,
11.8749340009141));
#118787=CARTESIAN_POINT('Ctrl Pts',(-9.26894694508746,7.20294297894025,
11.9268732757477));
#118788=CARTESIAN_POINT('Ctrl Pts',(-9.36234963743888,7.19574876061458,
11.9907476060144));
#118789=CARTESIAN_POINT('Ctrl Pts',(-9.39028839289087,7.19362506594439,
12.008181657977));
#118790=CARTESIAN_POINT('Ctrl Pts',(-9.42797894050415,7.1907738700824,12.0295608128537));
#118791=CARTESIAN_POINT('Ctrl Pts',(-9.43710661876336,7.19008445945855,
12.034579426547));
#118792=CARTESIAN_POINT('Ctrl Pts',(-9.45208992144726,7.1889538847721,12.0425606226484));
#118793=CARTESIAN_POINT('Ctrl Pts',(-9.45790598603467,7.18851529953383,
12.0455965680688));
#118794=CARTESIAN_POINT('Ctrl Pts',(-9.46919212312733,7.18766458165058,
12.0513683768899));
#118795=CARTESIAN_POINT('Ctrl Pts',(-9.47465874941698,7.18725268447713,
12.0541105416839));
#118796=CARTESIAN_POINT('Ctrl Pts',(-9.48746611844015,7.18628792476728,
12.0604105929349));
#118797=CARTESIAN_POINT('Ctrl Pts',(-9.49482288549503,7.18573393550218,
12.0639349992082));
#118798=CARTESIAN_POINT('Ctrl Pts',(-9.5189362651053,7.18391836178151,12.0751805132597));
#118799=CARTESIAN_POINT('Ctrl Pts',(-9.53583707012708,7.1826461769156,12.0825840203608));
#118800=CARTESIAN_POINT('Ctrl Pts',(-9.61267134258743,7.17686084697968,
12.1141118292701));
#118801=CARTESIAN_POINT('Ctrl Pts',(-9.67434632165505,7.17220365495304,
12.1336737027781));
#118802=CARTESIAN_POINT('Ctrl Pts',(-9.81445776863071,7.16168892727099,
12.1657329625074));
#118803=CARTESIAN_POINT('Ctrl Pts',(-9.89319733916668,7.15581990273731,
12.1755653729065));
#118804=CARTESIAN_POINT('Ctrl Pts',(-9.98409275487158,7.14941813920328,
12.1777013300578));
#118805=CARTESIAN_POINT('Ctrl Pts',(-9.99585793830614,7.14859699984235,
12.1778014827138));
#118806=CARTESIAN_POINT('Ctrl Pts',(-10.0120868775894,7.14747636700087,
12.1776964359569));
#118807=CARTESIAN_POINT('Ctrl Pts',(-10.0165504590798,7.14716940792077,
12.1776421662736));
#118808=CARTESIAN_POINT('Ctrl Pts',(-10.024210147981,7.146644933501,12.1775054784091));
#118809=CARTESIAN_POINT('Ctrl Pts',(-10.0274063858961,7.14642676207325,
12.1774354222551));
#118810=CARTESIAN_POINT('Ctrl Pts',(-10.034121785823,7.14596986377546,12.1772608721305));
#118811=CARTESIAN_POINT('Ctrl Pts',(-10.0376408307015,7.14573130037873,
12.1771536117722));
#118812=CARTESIAN_POINT('Ctrl Pts',(-10.0463622095752,7.14514208546159,
12.1768486353545));
#118813=CARTESIAN_POINT('Ctrl Pts',(-10.0515638940641,7.1447924467446,12.1766321992691));
#118814=CARTESIAN_POINT('Ctrl Pts',(-10.07118936976,7.14347945777119,12.1756852084053));
#118815=CARTESIAN_POINT('Ctrl Pts',(-10.0856014246771,7.14252783127494,
12.1747238304073));
#118816=CARTESIAN_POINT('Ctrl Pts',(-10.122859843571,7.14009182309856,12.1715490658749));
#118817=CARTESIAN_POINT('Ctrl Pts',(-10.1456663752112,7.13862425958408,
12.1689325013321));
#118818=CARTESIAN_POINT('Ctrl Pts',(-10.2868212261419,7.12960887434274,
12.1485420864135));
#118819=CARTESIAN_POINT('Ctrl Pts',(-10.4019560768608,7.12247392096375,
12.1134849655821));
#118820=CARTESIAN_POINT('Ctrl Pts',(-10.5252488923081,7.11358759114768,
12.0542774485041));
#118821=CARTESIAN_POINT('Ctrl Pts',(-10.5404964116846,7.11246664629602,
12.0465423632592));
#118822=CARTESIAN_POINT('Ctrl Pts',(-10.5624759697614,7.11081553764283,
12.0347836469239));
#118823=CARTESIAN_POINT('Ctrl Pts',(-10.5693451953029,7.11029439410972,
12.0310201046277));
#118824=CARTESIAN_POINT('Ctrl Pts',(-10.5814859859092,7.10936388936937,
12.0242100247835));
#118825=CARTESIAN_POINT('Ctrl Pts',(-10.586772476655,7.10895549571897,12.0211905722957));
#118826=CARTESIAN_POINT('Ctrl Pts',(-10.5977782287226,7.10809838208765,
12.0147908090029));
#118827=CARTESIAN_POINT('Ctrl Pts',(-10.6034927584972,7.10764939851695,
12.011402829784));
#118828=CARTESIAN_POINT('Ctrl Pts',(-10.6184198350379,7.10646601734254,
12.0023814508891));
#118829=CARTESIAN_POINT('Ctrl Pts',(-10.6275839220843,7.1057288060035,11.9966694902225));
#118830=CARTESIAN_POINT('Ctrl Pts',(-10.671044510002,7.10217991700831,11.9687435166859));
#118831=CARTESIAN_POINT('Ctrl Pts',(-10.704244323729,7.09930842887193,11.9448830536208));
#118832=CARTESIAN_POINT('Ctrl Pts',(-10.7734519043827,7.09296199601663,
11.8894676366601));
#118833=CARTESIAN_POINT('Ctrl Pts',(-10.8089128465887,7.08947263928147,
11.8573446726783));
#118834=CARTESIAN_POINT('Ctrl Pts',(-10.8912209819115,7.0808342880044,11.7731204377217));
#118835=CARTESIAN_POINT('Ctrl Pts',(-10.9355688926824,7.07567801491109,
11.7188202930857));
#118836=CARTESIAN_POINT('Ctrl Pts',(-10.9806512093493,7.07004136477047,
11.6523232630607));
#118837=CARTESIAN_POINT('Ctrl Pts',(-10.9863527140921,7.06932017985713,
11.6436697721853));
#118838=CARTESIAN_POINT('Ctrl Pts',(-10.9943777343327,7.06829413233643,
11.6311326631173));
#118839=CARTESIAN_POINT('Ctrl Pts',(-10.9967940562876,7.0679837081334,11.6273094356312));
#118840=CARTESIAN_POINT('Ctrl Pts',(-11.0009967172374,7.06744129561164,
11.6205741728159));
#118841=CARTESIAN_POINT('Ctrl Pts',(-11.002792498063,7.06720870999565,11.6176681462682));
#118842=CARTESIAN_POINT('Ctrl Pts',(-11.0065961829106,7.06671435078057,
11.6114525091213));
#118843=CARTESIAN_POINT('Ctrl Pts',(-11.0086004360471,7.06645280784112,
11.6081407796282));
#118844=CARTESIAN_POINT('Ctrl Pts',(-11.0140882208431,7.06573358005744,
11.5989712762055));
#118845=CARTESIAN_POINT('Ctrl Pts',(-11.0175373582328,7.06527802195826,
11.5930929433202));
#118846=CARTESIAN_POINT('Ctrl Pts',(-11.0373555230779,7.06263765302235,
11.5586351976354));
#118847=CARTESIAN_POINT('Ctrl Pts',(-11.0525726042463,7.0605174557016,11.5294063825332));
#118848=CARTESIAN_POINT('Ctrl Pts',(-11.0872863988974,7.0553373624199,11.4552957319249));
#118849=CARTESIAN_POINT('Ctrl Pts',(-11.1052505502069,7.05232368682522,
11.4097653219609));
#118850=CARTESIAN_POINT('Ctrl Pts',(-11.1429689238423,7.04475723960945,
11.2934339700671));
#118851=CARTESIAN_POINT('Ctrl Pts',(-11.1590272413713,7.04019787473598,
11.2216654336696));
#118852=CARTESIAN_POINT('Ctrl Pts',(-11.1703393322768,7.0343739957142,11.1328926504938));
#118853=CARTESIAN_POINT('Ctrl Pts',(-11.1720475706517,7.03331642164604,
11.1168719846597));
#118854=CARTESIAN_POINT('Ctrl Pts',(-11.1740887832349,7.03173609823456,
11.0931151166481));
#118855=CARTESIAN_POINT('Ctrl Pts',(-11.1746750049606,7.03122115634786,
11.0854021300784));
#118856=CARTESIAN_POINT('Ctrl Pts',(-11.1755848617806,7.03029863934739,
11.0716380451647));
#118857=CARTESIAN_POINT('Ctrl Pts',(-11.1759378565216,7.0298919863224,11.0655891151254));
#118858=CARTESIAN_POINT('Ctrl Pts',(-11.176586035025,7.02902837012298,11.0527835387011));
#118859=CARTESIAN_POINT('Ctrl Pts',(-11.1768697262391,7.02857106680536,
11.0460265569456));
#118860=CARTESIAN_POINT('Ctrl Pts',(-11.1774736315989,7.02734140247045,
11.0279237540038));
#118861=CARTESIAN_POINT('Ctrl Pts',(-11.177688044813,7.02656581518332,11.0165753621496));
#118862=CARTESIAN_POINT('Ctrl Pts',(-11.1779557546508,7.02241613743726,
10.9562436739114));
#118863=CARTESIAN_POINT('Ctrl Pts',(-11.1751171594198,7.01895439290733,
10.9073021529061));
#118864=CARTESIAN_POINT('Ctrl Pts',(-11.1632335996219,7.01181410622739,
10.8089775920459));
#118865=CARTESIAN_POINT('Ctrl Pts',(-11.1540626107498,7.00813955662012,
10.7597066180039));
#118866=CARTESIAN_POINT('Ctrl Pts',(-11.1366917331144,7.00294220305098,
10.69103667551));
#118867=CARTESIAN_POINT('Ctrl Pts',(-11.1310664800047,7.00141975738431,
10.6710393980602));
#118868=CARTESIAN_POINT('Ctrl Pts',(-11.1184534335279,6.99831450571608,
10.6303609249584));
#118869=CARTESIAN_POINT('Ctrl Pts',(-11.1114134211862,6.99673308923194,
10.6097034187031));
#118870=CARTESIAN_POINT('Ctrl Pts',(-11.0959661819627,6.99355986266214,
10.5681919888782));
#118871=CARTESIAN_POINT('Ctrl Pts',(-11.0875273308079,6.99196975493211,
10.5473583178036));
#118872=CARTESIAN_POINT('Ctrl Pts',(-11.0759557983401,6.98997094654322,
10.5209862460038));
#118873=CARTESIAN_POINT('Ctrl Pts',(-11.0733680939396,6.98953444935822,
10.5152155160713));
#118874=CARTESIAN_POINT('Ctrl Pts',(-11.0691665340739,6.98884247505051,
10.5060443871361));
#118875=CARTESIAN_POINT('Ctrl Pts',(-11.0675826901648,6.98858527729134,
10.5026304937711));
#118876=CARTESIAN_POINT('Ctrl Pts',(-11.0645154094007,6.98809419807456,
10.4961012894803));
#118877=CARTESIAN_POINT('Ctrl Pts',(-11.0630346210165,6.9878601730517,10.4929848501944));
#118878=CARTESIAN_POINT('Ctrl Pts',(-11.0594484023269,6.98730057367608,
10.4855221410046));
#118879=CARTESIAN_POINT('Ctrl Pts',(-11.0573298661109,6.98697578870033,
10.4811821698823));
#118880=CARTESIAN_POINT('Ctrl Pts',(-11.0499006373031,6.98585623485933,
10.466197391157));
#118881=CARTESIAN_POINT('Ctrl Pts',(-11.0444552053208,6.9850691838067,10.4556196879729));
#118882=CARTESIAN_POINT('Ctrl Pts',(-11.0305792035198,6.98313974098937,
10.4296406687201));
#118883=CARTESIAN_POINT('Ctrl Pts',(-11.0219625723902,6.9820066399515,10.4143415430918));
#118884=CARTESIAN_POINT('Ctrl Pts',(-10.9826823537663,6.97708982109436,
10.3481069020108));
#118885=CARTESIAN_POINT('Ctrl Pts',(-10.9485278832279,6.97343637096266,
10.2993395377957));
#118886=CARTESIAN_POINT('Ctrl Pts',(-10.8662458419095,6.96540299895493,
10.1989631295888));
#118887=CARTESIAN_POINT('Ctrl Pts',(-10.8168798587582,6.96102376182901,
10.1486789178639));
#118888=CARTESIAN_POINT('Ctrl Pts',(-10.7510362871584,6.95539728067929,
10.0926411767633));
#118889=CARTESIAN_POINT('Ctrl Pts',(-10.7385324511397,6.95433785198476,
10.0824351158772));
#118890=CARTESIAN_POINT('Ctrl Pts',(-10.7197273612972,6.95275528724952,
10.0677191918045));
#118891=CARTESIAN_POINT('Ctrl Pts',(-10.7135846428599,6.95223999155,10.0630091074995));
#118892=CARTESIAN_POINT('Ctrl Pts',(-10.7025510765595,6.9513170818885,10.054720269492));
#118893=CARTESIAN_POINT('Ctrl Pts',(-10.697678150988,6.9509103930267,10.0511180371731));
#118894=CARTESIAN_POINT('Ctrl Pts',(-10.6873110399871,6.95004695438959,
10.0435773464579));
#118895=CARTESIAN_POINT('Ctrl Pts',(-10.6818103286631,6.9495898663991,10.0396482777969));
#118896=CARTESIAN_POINT('Ctrl Pts',(-10.666995426664,6.94836140172638,10.0292576730323));
#118897=CARTESIAN_POINT('Ctrl Pts',(-10.6576214572477,6.94758680975163,
10.02288303261));
#118898=CARTESIAN_POINT('Ctrl Pts',(-10.6074614629191,6.94345489273674,
9.98982115964472));
#118899=CARTESIAN_POINT('Ctrl Pts',(-10.5651453533168,6.94001082366544,
9.9655531346084));
#118900=CARTESIAN_POINT('Ctrl Pts',(-10.4764056170453,6.93287706764159,
9.92173436529136));
#118901=CARTESIAN_POINT('Ctrl Pts',(-10.4299837702706,6.92919017672033,
9.90239693431866));
#118902=CARTESIAN_POINT('Ctrl Pts',(-10.3637871919489,6.92405463255425,
9.87966780144392));
#118903=CARTESIAN_POINT('Ctrl Pts',(-10.3449433495534,6.92260637095113,
9.87372318469324));
#118904=CARTESIAN_POINT('Ctrl Pts',(-10.2843245442658,6.91800419409123,
9.85626410235194));
#118905=CARTESIAN_POINT('Ctrl Pts',(-10.2420555734649,6.91487905098748,
9.84657805375115));
#118906=CARTESIAN_POINT('Ctrl Pts',(-10.1920496350892,6.91134493418146,
9.83799019486647));
#118907=CARTESIAN_POINT('Ctrl Pts',(-10.1847427200789,6.91083257861849,
9.83680612797481));
#118908=CARTESIAN_POINT('Ctrl Pts',(-10.173428493072,6.91004598123102,9.83508199325979));
#118909=CARTESIAN_POINT('Ctrl Pts',(-10.169428902887,6.90976921817809,9.8344935638392));
#118910=CARTESIAN_POINT('Ctrl Pts',(-10.1620703570259,6.90926250738813,
9.83344963640334));
#118911=CARTESIAN_POINT('Ctrl Pts',(-10.1587124458408,6.90903224088061,
9.83298804140135));
#118912=CARTESIAN_POINT('Ctrl Pts',(-10.1510515128679,6.90850905039826,
9.83196860976443));
#118913=CARTESIAN_POINT('Ctrl Pts',(-10.1467473601533,6.90821663976902,
9.83142004899233));
#118914=CARTESIAN_POINT('Ctrl Pts',(-10.1334104713215,6.90731504648324,
9.82979512273177));
#118915=CARTESIAN_POINT('Ctrl Pts',(-10.1243679709793,6.9067101045831,9.82879957784292));
#118916=CARTESIAN_POINT('Ctrl Pts',(-10.0464839631293,6.90154717067071,
9.82113707127153));
#118917=CARTESIAN_POINT('Ctrl Pts',(-9.97718042366107,6.89726697558048,
9.82044052843688));
#118918=CARTESIAN_POINT('Ctrl Pts',(-9.87568512331888,6.89096809829667,
9.82837501737253));
#118919=CARTESIAN_POINT('Ctrl Pts',(-9.84330458172222,6.88895474394848,
9.83226593055083));
#118920=CARTESIAN_POINT('Ctrl Pts',(-9.81114930150157,6.88692359881869,
9.83748958018577));
#118921=CARTESIAN_POINT('Ctrl Pts',(-9.81114930160613,6.78711399980274,
9.83748958016879));
#118922=CARTESIAN_POINT('Ctrl Pts',(-9.81165865453416,6.78714671379146,
9.83740683539975));
#118923=CARTESIAN_POINT('Ctrl Pts',(-9.81216806925791,6.78717943559225,
9.83732442420086));
#118924=CARTESIAN_POINT('Ctrl Pts',(-9.84739949050416,6.78944276472268,
9.83164857568015));
#118925=CARTESIAN_POINT('Ctrl Pts',(-9.88235162672327,6.79170711495437,
9.82761334767695));
#118926=CARTESIAN_POINT('Ctrl Pts',(-9.92806455013969,6.7947207236186,9.82440057201284));
#118927=CARTESIAN_POINT('Ctrl Pts',(-9.93870889477625,6.79542604679494,
9.8237975887402));
#118928=CARTESIAN_POINT('Ctrl Pts',(-9.95596605151993,6.79657605360612,
9.82305488706229));
#118929=CARTESIAN_POINT('Ctrl Pts',(-9.96257458412418,6.79701798340986,
9.82282621388235));
#118930=CARTESIAN_POINT('Ctrl Pts',(-9.97527772703814,6.79787059677669,
9.8224937267279));
#118931=CARTESIAN_POINT('Ctrl Pts',(-9.9813719199314,6.79828100820676,9.8223815530432));
#118932=CARTESIAN_POINT('Ctrl Pts',(-9.99549397218604,6.79923537918694,
9.82223126038202));
#118933=CARTESIAN_POINT('Ctrl Pts',(-10.0035218188105,6.79978039344215,
9.82222790847409));
#118934=CARTESIAN_POINT('Ctrl Pts',(-10.0292649535235,6.80153642938082,
9.8224803553207));
#118935=CARTESIAN_POINT('Ctrl Pts',(-10.0469739426987,6.80275711069989,
9.82305380715873));
#118936=CARTESIAN_POINT('Ctrl Pts',(-10.0888515527345,6.80567532620799,
9.82535650285618));
#118937=CARTESIAN_POINT('Ctrl Pts',(-10.1129922950995,6.8073826282093,9.8274324986164));
#118938=CARTESIAN_POINT('Ctrl Pts',(-10.2093826906933,6.81429913051286,
9.83872582109171));
#118939=CARTESIAN_POINT('Ctrl Pts',(-10.2807668703331,6.81965942393501,
9.85389060782328));
#118940=CARTESIAN_POINT('Ctrl Pts',(-10.4021546231384,6.82897493337465,
9.89170477922401));
#118941=CARTESIAN_POINT('Ctrl Pts',(-10.4528506143468,6.83292643968186,
9.91143473943408));
#118942=CARTESIAN_POINT('Ctrl Pts',(-10.5082358099888,6.83719281706454,
9.93753173143941));
#118943=CARTESIAN_POINT('Ctrl Pts',(-10.5144380150171,6.83766978855705,
9.94052088527869));
#118944=CARTESIAN_POINT('Ctrl Pts',(-10.5244632017613,6.83843905807482,
9.94546131949502));
#118945=CARTESIAN_POINT('Ctrl Pts',(-10.5283022522786,6.83873323317957,
9.94737936065352));
#118946=CARTESIAN_POINT('Ctrl Pts',(-10.5351514477798,6.839257220031,9.95084822112669));
#118947=CARTESIAN_POINT('Ctrl Pts',(-10.5381654689918,6.83948749962473,
9.95239107675725));
#118948=CARTESIAN_POINT('Ctrl Pts',(-10.5447954655564,6.83999337636174,
9.95582108891341));
#118949=CARTESIAN_POINT('Ctrl Pts',(-10.5484083202271,6.84026861206831,
9.95771404441627));
#118950=CARTESIAN_POINT('Ctrl Pts',(-10.5588972801966,6.8410666461757,9.96327937332951));
#118951=CARTESIAN_POINT('Ctrl Pts',(-10.5657470082468,6.84158648818206,
9.96700137549403));
#118952=CARTESIAN_POINT('Ctrl Pts',(-10.6306056379888,6.84650113723427,
10.00308290321));
#118953=CARTESIAN_POINT('Ctrl Pts',(-10.685824861638,6.85063068201233,10.0402323136601));
#118954=CARTESIAN_POINT('Ctrl Pts',(-10.8062065005216,6.86019183421428,
10.1369439770718));
#118955=CARTESIAN_POINT('Ctrl Pts',(-10.8683930005054,6.86559822922517,
10.1995462634242));
#118956=CARTESIAN_POINT('Ctrl Pts',(-10.9327103267732,6.87234319087347,
10.2807020684408));
#118957=CARTESIAN_POINT('Ctrl Pts',(-10.9421487187703,6.87336717271529,
10.2931097519017));
#118958=CARTESIAN_POINT('Ctrl Pts',(-10.955838415462,6.87490676472398,10.3118675470388));
#118959=CARTESIAN_POINT('Ctrl Pts',(-10.9602789402022,6.87541515073502,
10.3180779357509));
#118960=CARTESIAN_POINT('Ctrl Pts',(-10.9681279744353,6.87633034143428,
10.3292840712264));
#118961=CARTESIAN_POINT('Ctrl Pts',(-10.9715590064366,6.87673627906025,
10.3342637709421));
#118962=CARTESIAN_POINT('Ctrl Pts',(-10.9787774987635,6.87760310387184,
10.3449151345576));
#118963=CARTESIAN_POINT('Ctrl Pts',(-10.9825543348174,6.87806436718427,
10.3505936951545));
#118964=CARTESIAN_POINT('Ctrl Pts',(-10.9926319598948,6.87931649393747,
10.3660348128915));
#118965=CARTESIAN_POINT('Ctrl Pts',(-10.998837804494,6.88011079344423,10.3758581172305));
#118966=CARTESIAN_POINT('Ctrl Pts',(-11.0330680192284,6.88462772834538,
10.4318598079068));
#118967=CARTESIAN_POINT('Ctrl Pts',(-11.0580307929856,6.88845808245707,
10.4798248960721));
#118968=CARTESIAN_POINT('Ctrl Pts',(-11.0924813458439,6.89469673414182,
10.5588463247718));
#118969=CARTESIAN_POINT('Ctrl Pts',(-11.1041340284224,6.897051251909,10.5888796428063));
#118970=CARTESIAN_POINT('Ctrl Pts',(-11.1374642360981,6.90461488750198,
10.686470679371));
#118971=CARTESIAN_POINT('Ctrl Pts',(-11.1542795214332,6.90984485056745,
10.7555290402598));
#118972=CARTESIAN_POINT('Ctrl Pts',(-11.1663055234763,6.91554508812385,
10.8358875516916));
#118973=CARTESIAN_POINT('Ctrl Pts',(-11.1676982350094,6.91626297000211,
10.8461093901593));
#118974=CARTESIAN_POINT('Ctrl Pts',(-11.1695070714827,6.9172851489878,10.8608287152093));
#118975=CARTESIAN_POINT('Ctrl Pts',(-11.1700318741482,6.91759495313364,
10.8653120201424));
#118976=CARTESIAN_POINT('Ctrl Pts',(-11.170908326613,6.91813660824291,10.8731914477863));
#118977=CARTESIAN_POINT('Ctrl Pts',(-11.171271003691,6.91836905189644,10.8765862432607));
#118978=CARTESIAN_POINT('Ctrl Pts',(-11.1720137042958,6.91886347589555,
10.8838365484634));
#118979=CARTESIAN_POINT('Ctrl Pts',(-11.1723894717543,6.91912522291862,
10.8876923950372));
#118980=CARTESIAN_POINT('Ctrl Pts',(-11.1733753756158,6.91984581252435,
10.8983536770298));
#118981=CARTESIAN_POINT('Ctrl Pts',(-11.1739453390482,6.92030251431377,
10.9051628053703));
#118982=CARTESIAN_POINT('Ctrl Pts',(-11.1769438259324,6.92296725598487,
10.9451702951498));
#118983=CARTESIAN_POINT('Ctrl Pts',(-11.1780235384313,6.92510926990228,
10.9784579210194));
#118984=CARTESIAN_POINT('Ctrl Pts',(-11.1771923471998,6.93038075948637,
11.0617692510761));
#118985=CARTESIAN_POINT('Ctrl Pts',(-11.1735071117453,6.93346143365807,
11.1117086315468));
#118986=CARTESIAN_POINT('Ctrl Pts',(-11.1568325932704,6.94099722565733,
11.2323393781032));
#118987=CARTESIAN_POINT('Ctrl Pts',(-11.1405351230815,6.94545963074922,
11.3023593628651));
#118988=CARTESIAN_POINT('Ctrl Pts',(-11.1128757074553,6.951181412913,11.3858302844127));
#118989=CARTESIAN_POINT('Ctrl Pts',(-11.1074652090303,6.95224444402214,
11.4010961458548));
#118990=CARTESIAN_POINT('Ctrl Pts',(-11.0990028766858,6.95383127645805,
11.4234947463477));
#118991=CARTESIAN_POINT('Ctrl Pts',(-11.0961924491044,6.9543471726105,11.4307171146851));
#118992=CARTESIAN_POINT('Ctrl Pts',(-11.0910579929475,6.95527065034166,
11.4435360582521));
#118993=CARTESIAN_POINT('Ctrl Pts',(-11.088761643206,6.95567730101118,11.4491434747255));
#118994=CARTESIAN_POINT('Ctrl Pts',(-11.0838154108504,6.95654012453228,
11.4609607354383));
#118995=CARTESIAN_POINT('Ctrl Pts',(-11.0811552044576,6.95699663136441,
11.4671659929967));
#118996=CARTESIAN_POINT('Ctrl Pts',(-11.0738992235544,6.95822222624694,
11.483697497566));
#118997=CARTESIAN_POINT('Ctrl Pts',(-11.0692080011012,6.9589945047686,11.4939808158791));
#118998=CARTESIAN_POINT('Ctrl Pts',(-11.0437272525085,6.96308793890694,
11.5477714133036));
#118999=CARTESIAN_POINT('Ctrl Pts',(-11.0204310276766,6.96649389541748,
11.5900334905316));
#119000=CARTESIAN_POINT('Ctrl Pts',(-10.9675111489711,6.97361345098019,
11.6734822037529));
#119001=CARTESIAN_POINT('Ctrl Pts',(-10.9376837656646,6.97732685370013,
11.7144261177717));
#119002=CARTESIAN_POINT('Ctrl Pts',(-10.8947538876449,6.98225167017783,
11.7660178318959));
#119003=CARTESIAN_POINT('Ctrl Pts',(-10.8839238386263,6.98346267692399,
11.7784898826693));
#119004=CARTESIAN_POINT('Ctrl Pts',(-10.841498648658,6.98808016313202,11.8253202569992));
#119005=CARTESIAN_POINT('Ctrl Pts',(-10.8081300733243,6.99145557320917,
11.8580211408581));
#119006=CARTESIAN_POINT('Ctrl Pts',(-10.7677639444479,6.99518262035704,
11.8931293356577));
#119007=CARTESIAN_POINT('Ctrl Pts',(-10.7625841326585,6.99565457358155,
11.8975560877365));
#119008=CARTESIAN_POINT('Ctrl Pts',(-10.7540959288575,6.9964173855241,11.9046837162791));
#119009=CARTESIAN_POINT('Ctrl Pts',(-10.7508108360015,6.99671007169759,
11.9074119166069));
#119010=CARTESIAN_POINT('Ctrl Pts',(-10.7448950863615,6.99723249945962,
11.9122707006347));
#119011=CARTESIAN_POINT('Ctrl Pts',(-10.742270018797,6.99746269642173,11.9144078635862));
#119012=CARTESIAN_POINT('Ctrl Pts',(-10.7364475617438,6.99796969578397,
11.9191065414099));
#119013=CARTESIAN_POINT('Ctrl Pts',(-10.7332459971836,6.99824612588312,
11.9216627119199));
#119014=CARTESIAN_POINT('Ctrl Pts',(-10.7238453606961,6.99905116914096,
11.9290883133652));
#119015=CARTESIAN_POINT('Ctrl Pts',(-10.7176105171636,6.99957674605434,
11.9339123910437));
#119016=CARTESIAN_POINT('Ctrl Pts',(-10.7031820669488,7.00077519334837,
11.9448462798436));
#119017=CARTESIAN_POINT('Ctrl Pts',(-10.6949563267502,7.00144549053447,
11.9509128410331));
#119018=CARTESIAN_POINT('Ctrl Pts',(-10.5975028865921,7.00924980231475,
12.0208455488302));
#119019=CARTESIAN_POINT('Ctrl Pts',(-10.4998413897803,7.01578315034754,
12.0720542325587));
#119020=CARTESIAN_POINT('Ctrl Pts',(-10.3571838960684,7.02533078838272,
12.1230570996598));
#119021=CARTESIAN_POINT('Ctrl Pts',(-10.3171614733879,7.02800366797263,
12.1350090800011));
#119022=CARTESIAN_POINT('Ctrl Pts',(-10.265653932376,7.03148385768885,12.1474535624513));
#119023=CARTESIAN_POINT('Ctrl Pts',(-10.2546787816675,7.03222758301654,
12.1499392999861));
#119024=CARTESIAN_POINT('Ctrl Pts',(-10.2370751754345,7.03342473963628,
12.1536619350291));
#119025=CARTESIAN_POINT('Ctrl Pts',(-10.2304686180908,7.03387497794746,
12.1549998753391));
#119026=CARTESIAN_POINT('Ctrl Pts',(-10.2178999354993,7.03473350855163,
12.1574331184898));
#119027=CARTESIAN_POINT('Ctrl Pts',(-10.2119401089706,7.03514144537417,
12.1585392498846));
#119028=CARTESIAN_POINT('Ctrl Pts',(-10.1983226619466,7.03607556639405,
12.1609580286707));
#119029=CARTESIAN_POINT('Ctrl Pts',(-10.1906601264017,7.03660266169847,
12.1622409964259));
#119030=CARTESIAN_POINT('Ctrl Pts',(-10.1668853912186,7.0382429243873,12.1659802562812));
#119031=CARTESIAN_POINT('Ctrl Pts',(-10.1507350783665,7.039364046988,12.1681778896968));
#119032=CARTESIAN_POINT('Ctrl Pts',(-10.1129805475338,7.04200217535782,
12.1725193537282));
#119033=CARTESIAN_POINT('Ctrl Pts',(-10.0913528787889,7.043526596353,12.1744023110127));
#119034=CARTESIAN_POINT('Ctrl Pts',(-10.0107225406934,7.04925876677697,
12.1791815265163));
#119035=CARTESIAN_POINT('Ctrl Pts',(-9.95158498874825,7.05356577982892,
12.1782354034993));
#119036=CARTESIAN_POINT('Ctrl Pts',(-9.82468377092682,7.06291484233857,
12.1666337641989));
#119037=CARTESIAN_POINT('Ctrl Pts',(-9.75725871623206,7.06794945412695,
12.1544905639196));
#119038=CARTESIAN_POINT('Ctrl Pts',(-9.6821665797117,7.0734099639287,12.134092518972));
#119039=CARTESIAN_POINT('Ctrl Pts',(-9.6730992039668,7.07406666543416,12.131512177507));
#119040=CARTESIAN_POINT('Ctrl Pts',(-9.65926876106935,7.07506326109653,
12.1273962525905));
#119041=CARTESIAN_POINT('Ctrl Pts',(-9.65448310569204,7.07540717021679,
12.1259387929861));
#119042=CARTESIAN_POINT('Ctrl Pts',(-9.64641688889671,7.07598507713754,
12.1234259743158));
#119043=CARTESIAN_POINT('Ctrl Pts',(-9.64313144245742,7.07621997000779,
12.1223866401824));
#119044=CARTESIAN_POINT('Ctrl Pts',(-9.63634064170335,7.0767043928802,12.1202055720394));
#119045=CARTESIAN_POINT('Ctrl Pts',(-9.6328360213339,7.07695380308728,12.119061779446));
#119046=CARTESIAN_POINT('Ctrl Pts',(-9.62366193906326,7.07760527364036,
12.1160199238925));
#119047=CARTESIAN_POINT('Ctrl Pts',(-9.61800137057801,7.07800582248132,
12.1140950845841));
#119048=CARTESIAN_POINT('Ctrl Pts',(-9.59228377130419,7.07982020323933,
12.105130925934));
#119049=CARTESIAN_POINT('Ctrl Pts',(-9.5724035481661,7.08120767074359,12.0975920443112));
#119050=CARTESIAN_POINT('Ctrl Pts',(-9.51471206571097,7.08521963830381,
12.0739088568943));
#119051=CARTESIAN_POINT('Ctrl Pts',(-9.47752756285411,7.08778755163321,
12.0563179766644));
#119052=CARTESIAN_POINT('Ctrl Pts',(-9.35620794602017,7.09633855736261,
11.9909479118797));
#119053=CARTESIAN_POINT('Ctrl Pts',(-9.27706171316799,7.10224403132633,
11.9347749660114));
#119054=CARTESIAN_POINT('Ctrl Pts',(-9.19589184900835,7.10941600538715,
11.8606280550987));
#119055=CARTESIAN_POINT('Ctrl Pts',(-9.18626241497194,7.11028651857718,
11.8515290292971));
#119056=CARTESIAN_POINT('Ctrl Pts',(-9.17115188074181,7.11168582274353,
11.8367604113687));
#119057=CARTESIAN_POINT('Ctrl Pts',(-9.16557051385687,7.11221019044671,
11.8311946934718));
#119058=CARTESIAN_POINT('Ctrl Pts',(-9.15577393229354,7.11314429250534,
11.8212274615917));
#119059=CARTESIAN_POINT('Ctrl Pts',(-9.15153618464364,7.11355303155063,
11.8168484245695));
#119060=CARTESIAN_POINT('Ctrl Pts',(-9.14276818517147,7.11440866878137,
11.807646247941));
#119061=CARTESIAN_POINT('Ctrl Pts',(-9.13824422735141,7.11485581406018,
11.8028174334143));
#119062=CARTESIAN_POINT('Ctrl Pts',(-9.12652418455816,7.11602934011728,
11.7900944003536));
#119063=CARTESIAN_POINT('Ctrl Pts',(-9.11939452241287,7.11675845096712,
11.7821401034664));
#119064=CARTESIAN_POINT('Ctrl Pts',(-9.08646289567101,7.12019962205745,
11.7443784032387));
#119065=CARTESIAN_POINT('Ctrl Pts',(-9.06206257805021,7.12296713144085,
11.713387709906));
#119066=CARTESIAN_POINT('Ctrl Pts',(-8.98923021723505,7.13196782840287,
11.6106732760269));
#119067=CARTESIAN_POINT('Ctrl Pts',(-8.94712514452389,7.13838714501175,
11.5348170503302));
#119068=CARTESIAN_POINT('Ctrl Pts',(-8.9061460852412,7.14609857239075,11.4369918889146));
#119069=CARTESIAN_POINT('Ctrl Pts',(-8.89903335609785,7.14751277359536,
11.4187491081265));
#119070=CARTESIAN_POINT('Ctrl Pts',(-8.88545716169023,7.15036611530907,
11.3811875131619));
#119071=CARTESIAN_POINT('Ctrl Pts',(-8.87903314728264,7.15180354467346,
11.3618606002703));
#119072=CARTESIAN_POINT('Ctrl Pts',(-8.87133565921433,7.15364002468118,
11.3365252632519));
#119073=CARTESIAN_POINT('Ctrl Pts',(-8.86960375412886,7.15406180561386,
11.3306611230906));
#119074=CARTESIAN_POINT('Ctrl Pts',(-8.86689269643877,7.15473591586353,
11.32121132087));
#119075=CARTESIAN_POINT('Ctrl Pts',(-8.8658847386127,7.15498981993244,11.3176341431503));
#119076=CARTESIAN_POINT('Ctrl Pts',(-8.86396841716875,7.15547889723786,
11.3107078150592));
#119077=CARTESIAN_POINT('Ctrl Pts',(-8.86305790372677,7.15571418165724,
11.3073593557755));
#119078=CARTESIAN_POINT('Ctrl Pts',(-8.8608854037027,7.15628283562606,11.2992281166866));
#119079=CARTESIAN_POINT('Ctrl Pts',(-8.85963870467275,7.15661534724143,
11.2944412464405));
#119080=CARTESIAN_POINT('Ctrl Pts',(-8.85531094597071,7.15779263077702,
11.2773843429932));
#119081=CARTESIAN_POINT('Ctrl Pts',(-8.85239733680639,7.15862858013191,
11.2650721850143));
#119082=CARTESIAN_POINT('Ctrl Pts',(-8.84558592345296,7.16070455095235,
11.2340677265738));
#119083=CARTESIAN_POINT('Ctrl Pts',(-8.8419430949966,7.1619333543182,11.2153226590861));
#119084=CARTESIAN_POINT('Ctrl Pts',(-8.82697921390544,7.16764214086865,
11.1268899725776));
#119085=CARTESIAN_POINT('Ctrl Pts',(-8.82148249036645,7.17194682567929,
11.0563614794458));
#119086=CARTESIAN_POINT('Ctrl Pts',(-8.82309786245486,7.18024999671284,
10.9227535747313));
#119087=CARTESIAN_POINT('Ctrl Pts',(-8.82891472518208,7.18421814271105,
10.8599164502919));
#119088=CARTESIAN_POINT('Ctrl Pts',(-8.84180773714321,7.18914122931831,
10.7859146325037));
#119089=CARTESIAN_POINT('Ctrl Pts',(-8.84407134684014,7.18994067473012,
10.7740115192775));
#119090=CARTESIAN_POINT('Ctrl Pts',(-8.8479312869556,7.19121087118127,10.7552926112887));
#119091=CARTESIAN_POINT('Ctrl Pts',(-8.84940547147821,7.19167778221233,
10.7484522847466));
#119092=CARTESIAN_POINT('Ctrl Pts',(-8.85226296937522,7.19255053712155,
10.7357442323773));
#119093=CARTESIAN_POINT('Ctrl Pts',(-8.85363055702685,7.1929558710821,10.7298731777575));
#119094=CARTESIAN_POINT('Ctrl Pts',(-8.8567734085209,7.19386089624394,10.7168347772511));
#119095=CARTESIAN_POINT('Ctrl Pts',(-8.85857111351893,7.19436128608009,
10.709673157194));
#119096=CARTESIAN_POINT('Ctrl Pts',(-8.86405124036055,7.19583805048366,
10.6886796608658));
#119097=CARTESIAN_POINT('Ctrl Pts',(-8.86791850177335,7.19682025803088,
10.6748978803393));
#119098=CARTESIAN_POINT('Ctrl Pts',(-8.88661407039467,7.20131612265656,
10.6126566140892));
#119099=CARTESIAN_POINT('Ctrl Pts',(-8.90430756781351,7.20491968977872,
10.5651207077329));
#119100=CARTESIAN_POINT('Ctrl Pts',(-8.95706673317573,7.21427434940384,
10.4472384470748));
#119101=CARTESIAN_POINT('Ctrl Pts',(-8.99620787556259,7.22010496877039,
10.3789880507339));
#119102=CARTESIAN_POINT('Ctrl Pts',(-9.04473955631525,7.22612793207715,
10.3110897557392));
#119103=CARTESIAN_POINT('Ctrl Pts',(-9.04765975988754,7.22648635661377,
10.3070585102653));
#119104=CARTESIAN_POINT('Ctrl Pts',(-9.06511561785741,7.22860498064223,
10.283280050629));
#119105=CARTESIAN_POINT('Ctrl Pts',(-9.08024074262172,7.23034380847114,
10.2639705161614));
#119106=CARTESIAN_POINT('Ctrl Pts',(-9.1001261074507,7.23249841912012,10.2401550730176));
#119107=CARTESIAN_POINT('Ctrl Pts',(-9.10433465808834,7.23294738707613,
10.2351987606793));
#119108=CARTESIAN_POINT('Ctrl Pts',(-9.11106879769303,7.23365440166092,
10.2273999525602));
#119109=CARTESIAN_POINT('Ctrl Pts',(-9.11356740155779,7.2339142969905,10.2245344848482));
#119110=CARTESIAN_POINT('Ctrl Pts',(-9.11834973341286,7.23440704975766,
10.2191032927936));
#119111=CARTESIAN_POINT('Ctrl Pts',(-9.12063080009237,7.23464007276924,
10.2165354695666));
#119112=CARTESIAN_POINT('Ctrl Pts',(-9.12608465351509,7.23519253616889,
10.210449830751));
#119113=CARTESIAN_POINT('Ctrl Pts',(-9.1292674823748,7.23551123513328,10.2069411199333));
#119114=CARTESIAN_POINT('Ctrl Pts',(-9.14013726532212,7.23658750646814,
10.1951027340893));
#119115=CARTESIAN_POINT('Ctrl Pts',(-9.1479235383552,7.23733813586079,10.1868645513261));
#119116=CARTESIAN_POINT('Ctrl Pts',(-9.16729775348845,7.23916068762187,
10.1669498273378));
#119117=CARTESIAN_POINT('Ctrl Pts',(-9.17901395931552,7.24022459647593,
10.1554009245735));
#119118=CARTESIAN_POINT('Ctrl Pts',(-9.22919113742058,7.24464375396235,
10.1079713967805));
#119119=CARTESIAN_POINT('Ctrl Pts',(-9.26979357389781,7.24789398535228,
10.0744403190192));
#119120=CARTESIAN_POINT('Ctrl Pts',(-9.37690190980518,7.25605424897156,
9.99743609743425));
#119121=CARTESIAN_POINT('Ctrl Pts',(-9.44580343115982,7.26095979364624,
9.95776688848817));
#119122=CARTESIAN_POINT('Ctrl Pts',(-9.53276104529315,7.26716279202987,
9.91877905885108));
#119123=CARTESIAN_POINT('Ctrl Pts',(-9.54748918981858,7.26821306132519,
9.91253280909261));
#119124=CARTESIAN_POINT('Ctrl Pts',(-9.56949960935692,7.26978446932996,
9.90372268182108));
#119125=CARTESIAN_POINT('Ctrl Pts',(-9.5766876224835,7.2702979287095,9.90092713116257));
#119126=CARTESIAN_POINT('Ctrl Pts',(-9.58956720381623,7.27121870368291,
9.89606311383766));
#119127=CARTESIAN_POINT('Ctrl Pts',(-9.59524829642875,7.27162510909946,
9.89396754797411));
#119128=CARTESIAN_POINT('Ctrl Pts',(-9.60731743551697,7.27248916316173,
9.88962108376982));
#119129=CARTESIAN_POINT('Ctrl Pts',(-9.61370922310152,7.27294715910361,
9.88738130231654));
#119130=CARTESIAN_POINT('Ctrl Pts',(-9.63091205410315,7.27418105115824,
9.88151926860928));
#119131=CARTESIAN_POINT('Ctrl Pts',(-9.64175673907339,7.27496021373416,
9.8779987484569));
#119132=CARTESIAN_POINT('Ctrl Pts',(-9.70033578511025,7.27917732241226,
9.85991801359534));
#119133=CARTESIAN_POINT('Ctrl Pts',(-9.74890176212053,7.28270643786671,
9.84824740365316));
#119134=CARTESIAN_POINT('Ctrl Pts',(-9.80241649052628,7.28662544021495,
9.83893350277088));
#119135=CARTESIAN_POINT('Ctrl Pts',(-9.8067810654517,7.28694525765071,9.83819920342532));
#119136=CARTESIAN_POINT('Ctrl Pts',(-9.81114930576479,7.28726551493505,
9.83748957949321));
#119137=CARTESIAN_POINT('Origin',(-10.,2.67563288526385,11.));
#119138=CARTESIAN_POINT('',(-9.81114930150157,7.88735883108162,9.83748958018577));
#119139=CARTESIAN_POINT('',(-9.81114930150278,7.78890339972193,9.83748958018558));
#119140=CARTESIAN_POINT('',(-9.81114930150157,2.67563288526385,9.83748958018577));
#119141=CARTESIAN_POINT('Ctrl Pts',(-9.81114930150157,7.88735883108162,
9.83748958018577));
#119142=CARTESIAN_POINT('Ctrl Pts',(-9.74943107542683,7.88290340352557,
9.84751575277368));
#119143=CARTESIAN_POINT('Ctrl Pts',(-9.68857434077757,7.87832101353714,
9.86244662222568));
#119144=CARTESIAN_POINT('Ctrl Pts',(-9.58638890922645,7.87042032301345,
9.89634623793599));
#119145=CARTESIAN_POINT('Ctrl Pts',(-9.54446494224,7.86711755370434,9.91297928531574));
#119146=CARTESIAN_POINT('Ctrl Pts',(-9.48322646397056,7.86228195855108,
9.9414421632336));
#119147=CARTESIAN_POINT('Ctrl Pts',(-9.46313093829663,7.86069357339216,
9.95149089166864));
#119148=CARTESIAN_POINT('Ctrl Pts',(-9.437967233662,7.85871329830822,9.964987287547));
#119149=CARTESIAN_POINT('Ctrl Pts',(-9.43262306370001,7.85829325086483,
9.9679071933588));
#119150=CARTESIAN_POINT('Ctrl Pts',(-9.42405840609558,7.85762119538577,
9.97267331444895));
#119151=CARTESIAN_POINT('Ctrl Pts',(-9.42082366478352,7.85736762980968,
9.97449348508955));
#119152=CARTESIAN_POINT('Ctrl Pts',(-9.41461239925589,7.85688131954688,
9.97802729256199));
#119153=CARTESIAN_POINT('Ctrl Pts',(-9.41163470634162,7.85664844817307,
9.97973869062973));
#119154=CARTESIAN_POINT('Ctrl Pts',(-9.40506443222326,7.85613512220821,
9.98355321742165));
#119155=CARTESIAN_POINT('Ctrl Pts',(-9.40147539334602,7.85585504949519,
9.98566243875509));
#119156=CARTESIAN_POINT('Ctrl Pts',(-9.38875205165487,7.85486308814584,
9.99323078962856));
#119157=CARTESIAN_POINT('Ctrl Pts',(-9.37968031223164,7.85415750027515,
9.99879482537806));
#119158=CARTESIAN_POINT('Ctrl Pts',(-9.32070828520934,7.84957328519771,
10.0360738736426));
#119159=CARTESIAN_POINT('Ctrl Pts',(-9.27317506302755,7.84588793213582,
10.0713891657175));
#119160=CARTESIAN_POINT('Ctrl Pts',(-9.18872929210029,7.83896291861324,
10.1446028521408));
#119161=CARTESIAN_POINT('Ctrl Pts',(-9.15132399448373,7.83572638062435,
10.1817009887514));
#119162=CARTESIAN_POINT('Ctrl Pts',(-9.09645807225226,7.83051274360634,
10.2439391986843));
#119163=CARTESIAN_POINT('Ctrl Pts',(-9.07727925166329,7.8285852224052,10.2674686551036));
#119164=CARTESIAN_POINT('Ctrl Pts',(-9.04643749691965,7.8252728600388,10.3084422316967));
#119165=CARTESIAN_POINT('Ctrl Pts',(-9.03429280986289,7.82390564156193,
10.3255052773521));
#119166=CARTESIAN_POINT('Ctrl Pts',(-9.01782979429182,7.82195502303108,
10.3499921909187));
#119167=CARTESIAN_POINT('Ctrl Pts',(-9.01312743757314,7.82138586783488,
10.3571539811538));
#119168=CARTESIAN_POINT('Ctrl Pts',(-9.00516599340077,7.82040089994723,
10.369572677558));
#119169=CARTESIAN_POINT('Ctrl Pts',(-9.0018693660908,7.8199864812399,10.3748051945668));
#119170=CARTESIAN_POINT('Ctrl Pts',(-8.99563382252948,7.81918974802054,
10.3848774899367));
#119171=CARTESIAN_POINT('Ctrl Pts',(-8.99268829063581,7.818807688374,10.3897129863052));
#119172=CARTESIAN_POINT('Ctrl Pts',(-8.98508569131969,7.81780639150752,
10.4023986938285));
#119173=CARTESIAN_POINT('Ctrl Pts',(-8.9804848905286,7.81718516033154,10.4102820093168));
#119174=CARTESIAN_POINT('Ctrl Pts',(-8.96464819231441,7.81499153345654,
10.4381569681104));
#119175=CARTESIAN_POINT('Ctrl Pts',(-8.95390560423597,7.81340206563585,
10.4584214305627));
#119176=CARTESIAN_POINT('Ctrl Pts',(-8.90422762609893,7.80552306297277,
10.5591321735631));
#119177=CARTESIAN_POINT('Ctrl Pts',(-8.87394936832593,7.79895307775005,
10.6435078764449));
#119178=CARTESIAN_POINT('Ctrl Pts',(-8.84175855188041,7.78864714183354,
10.7804409286624));
#119179=CARTESIAN_POINT('Ctrl Pts',(-8.83329018446766,7.78491312219991,
10.8311250036772));
#119180=CARTESIAN_POINT('Ctrl Pts',(-8.82721547832075,7.78066133481692,
10.8915570254728));
#119181=CARTESIAN_POINT('Ctrl Pts',(-8.8263873231804,7.78000825302077,10.900920679869));
#119182=CARTESIAN_POINT('Ctrl Pts',(-8.82533647356514,7.77905811142901,
10.9146771442689));
#119183=CARTESIAN_POINT('Ctrl Pts',(-8.82502615729278,7.77875660097518,
10.919062613318));
#119184=CARTESIAN_POINT('Ctrl Pts',(-8.82451981918072,7.77822472069115,
10.92683631955));
#119185=CARTESIAN_POINT('Ctrl Pts',(-8.82431387674356,7.77799382238227,
10.9302237845562));
#119186=CARTESIAN_POINT('Ctrl Pts',(-8.82389712328976,7.77749258889408,
10.9376054299811));
#119187=CARTESIAN_POINT('Ctrl Pts',(-8.82369201316351,7.77722256643187,
10.9415998265102));
#119188=CARTESIAN_POINT('Ctrl Pts',(-8.82317424591607,7.77646886041132,
10.9527964512655));
#119189=CARTESIAN_POINT('Ctrl Pts',(-8.82290735365027,7.77598759469651,
10.9600007653021));
#119190=CARTESIAN_POINT('Ctrl Pts',(-8.8216777369192,7.77305877580818,11.0041453287305));
#119191=CARTESIAN_POINT('Ctrl Pts',(-8.82238773403703,7.7706920874923,11.0411154471114));
#119192=CARTESIAN_POINT('Ctrl Pts',(-8.83060896623812,7.76287220682805,
11.1649867825008));
#119193=CARTESIAN_POINT('Ctrl Pts',(-8.8460237164487,7.75760089972407,11.2510691351177));
#119194=CARTESIAN_POINT('Ctrl Pts',(-8.88203763804603,7.74959274599,11.3725849238408));
#119195=CARTESIAN_POINT('Ctrl Pts',(-8.8951783224685,7.74705369044557,11.4099120973305));
#119196=CARTESIAN_POINT('Ctrl Pts',(-8.91422478788929,7.74375009079304,
11.4564007166879));
#119197=CARTESIAN_POINT('Ctrl Pts',(-8.9184135666646,7.74304263426259,11.4662404962497));
#119198=CARTESIAN_POINT('Ctrl Pts',(-8.92541163253317,7.7418899297302,11.4820775227592));
#119199=CARTESIAN_POINT('Ctrl Pts',(-8.928138588902,7.74144745865819,11.4881106532559));
#119200=CARTESIAN_POINT('Ctrl Pts',(-8.93347331432446,7.74059433295124,
11.4996529186084));
#119201=CARTESIAN_POINT('Ctrl Pts',(-8.93607327252425,7.74018395494179,
11.5051654446809));
#119202=CARTESIAN_POINT('Ctrl Pts',(-8.94213257515066,7.73923961335664,
11.517758312413));
#119203=CARTESIAN_POINT('Ctrl Pts',(-8.9456203965101,7.73870468675656,11.5248245470166));
#119204=CARTESIAN_POINT('Ctrl Pts',(-8.9551563016396,7.73726460527448,11.5436652637392));
#119205=CARTESIAN_POINT('Ctrl Pts',(-8.96133226654104,7.73635507936613,
11.5553733769103));
#119206=CARTESIAN_POINT('Ctrl Pts',(-9.01431338981796,7.7287362910599,11.6518366190005));
#119207=CARTESIAN_POINT('Ctrl Pts',(-9.07120114146556,7.7216555510736,11.7306124133267));
#119208=CARTESIAN_POINT('Ctrl Pts',(-9.16499544169033,7.7115472236744,11.8315927996381));
#119209=CARTESIAN_POINT('Ctrl Pts',(-9.19447849853451,7.70854760479785,
11.8601829577406));
#119210=CARTESIAN_POINT('Ctrl Pts',(-9.24139251425142,7.70409517830533,
11.9011441203719));
#119211=CARTESIAN_POINT('Ctrl Pts',(-9.25776551050205,7.7025954618132,11.9146770696243));
#119212=CARTESIAN_POINT('Ctrl Pts',(-9.27920568813946,7.70070865662662,
11.9314431581423));
#119213=CARTESIAN_POINT('Ctrl Pts',(-9.28394275085752,7.70029644460818,
11.9350897371872));
#119214=CARTESIAN_POINT('Ctrl Pts',(-9.29164609525518,7.69963388158351,
11.9409268843436));
#119215=CARTESIAN_POINT('Ctrl Pts',(-9.29459518455639,7.69938204858146,
11.9431398111324));
#119216=CARTESIAN_POINT('Ctrl Pts',(-9.30032161709896,7.69889663068955,
11.9473949050965));
#119217=CARTESIAN_POINT('Ctrl Pts',(-9.30309759307152,7.69866293684108,
11.949438771741));
#119218=CARTESIAN_POINT('Ctrl Pts',(-9.30992657165068,7.69809190192296,
11.9544206535867));
#119219=CARTESIAN_POINT('Ctrl Pts',(-9.3139894702766,7.69775547003068,11.9573451184726));
#119220=CARTESIAN_POINT('Ctrl Pts',(-9.3257648657861,7.69678949781629,11.9657075625778));
#119221=CARTESIAN_POINT('Ctrl Pts',(-9.33352443209061,7.69616411302244,
11.9710790099035));
#119222=CARTESIAN_POINT('Ctrl Pts',(-9.39782834585944,7.6910649793618,12.0144585409606));
#119223=CARTESIAN_POINT('Ctrl Pts',(-9.45751629780706,7.68685210721725,
12.0475928413633));
#119224=CARTESIAN_POINT('Ctrl Pts',(-9.56441427852582,7.67960915107862,
12.0953327314901));
#119225=CARTESIAN_POINT('Ctrl Pts',(-9.6102852064595,7.67658857719186,12.1124795713582));
#119226=CARTESIAN_POINT('Ctrl Pts',(-9.69665170568933,7.67089390940305,
12.1387647625826));
#119227=CARTESIAN_POINT('Ctrl Pts',(-9.73681873110736,7.66824293908909,
12.1487125088813));
#119228=CARTESIAN_POINT('Ctrl Pts',(-9.78806389039291,7.66481243150475,
12.1585748042698));
#119229=CARTESIAN_POINT('Ctrl Pts',(-9.79873254523177,7.66409572875389,
12.160475717325));
#119230=CARTESIAN_POINT('Ctrl Pts',(-9.81598960685156,7.66293167652171,
12.1633054121734));
#119231=CARTESIAN_POINT('Ctrl Pts',(-9.82256246987904,7.6624872076712,12.1643260825989));
#119232=CARTESIAN_POINT('Ctrl Pts',(-9.83516477952391,7.66163274012948,
12.1661738496661));
#119233=CARTESIAN_POINT('Ctrl Pts',(-9.84119269819625,7.66122303858443,
12.1670099982711));
#119234=CARTESIAN_POINT('Ctrl Pts',(-9.85497638860506,7.66028380211372,
12.1688132013588));
#119235=CARTESIAN_POINT('Ctrl Pts',(-9.8627357799825,7.65975333923783,12.169749834939));
#119236=CARTESIAN_POINT('Ctrl Pts',(-9.88343570574244,7.65833334927146,
12.1720397218351));
#119237=CARTESIAN_POINT('Ctrl Pts',(-9.8963900001829,7.65743964055994,12.1732558496495));
#119238=CARTESIAN_POINT('Ctrl Pts',(-10.0078349386093,7.64970516456164,
12.1818580708166));
#119239=CARTESIAN_POINT('Ctrl Pts',(-10.1068561737339,7.64247538467015,
12.1770403367912));
#119240=CARTESIAN_POINT('Ctrl Pts',(-10.2589763085333,7.63114982641165,
12.1502747891218));
#119241=CARTESIAN_POINT('Ctrl Pts',(-10.3131140758385,7.62708576562497,
12.1367329256127));
#119242=CARTESIAN_POINT('Ctrl Pts',(-10.3745458551827,7.62256682567292,
12.1166420805908));
#119243=CARTESIAN_POINT('Ctrl Pts',(-10.3829662981124,7.62194957785701,
12.1137822768003));
#119244=CARTESIAN_POINT('Ctrl Pts',(-10.395409021027,7.62104151562285,12.1093986001857));
#119245=CARTESIAN_POINT('Ctrl Pts',(-10.3994564181847,7.62074677725093,
12.1079477060947));
#119246=CARTESIAN_POINT('Ctrl Pts',(-10.4063721096402,7.62024436770512,
12.10542577497));
#119247=CARTESIAN_POINT('Ctrl Pts',(-10.409244272511,7.62003607314136,12.1043656829349));
#119248=CARTESIAN_POINT('Ctrl Pts',(-10.415798383721,7.61956159847327,12.1019175327269));
#119249=CARTESIAN_POINT('Ctrl Pts',(-10.4194775382595,7.61929584787206,
12.1005222127986));
#119250=CARTESIAN_POINT('Ctrl Pts',(-10.4296087147944,7.61856552379729,
12.0966217748843));
#119251=CARTESIAN_POINT('Ctrl Pts',(-10.4360458780282,7.61810313556992,
12.0940781338228));
#119252=CARTESIAN_POINT('Ctrl Pts',(-10.4716310289381,7.61555418649345,
12.0796527181057));
#119253=CARTESIAN_POINT('Ctrl Pts',(-10.5003187709561,7.61352600618621,
12.0666617707111));
#119254=CARTESIAN_POINT('Ctrl Pts',(-10.5854581331762,7.60748854771771,
12.0239152435637));
#119255=CARTESIAN_POINT('Ctrl Pts',(-10.640045758301,7.60358769934821,11.9907098284495));
#119256=CARTESIAN_POINT('Ctrl Pts',(-10.7274889412229,7.5968819043087,11.9272607647575));
#119257=CARTESIAN_POINT('Ctrl Pts',(-10.7618046919119,7.59411406732138,
11.8992807387113));
#119258=CARTESIAN_POINT('Ctrl Pts',(-10.8079538534198,7.59011040833927,
11.8571111823773));
#119259=CARTESIAN_POINT('Ctrl Pts',(-10.8211549083992,7.58892970881053,
11.8444723627325));
#119260=CARTESIAN_POINT('Ctrl Pts',(-10.8441318053855,7.58680500021843,
11.8214257211127));
#119261=CARTESIAN_POINT('Ctrl Pts',(-10.8540226368043,7.58586598161522,
11.8111374898562));
#119262=CARTESIAN_POINT('Ctrl Pts',(-10.8687385074957,7.58442953984668,
11.7952627743305));
#119263=CARTESIAN_POINT('Ctrl Pts',(-10.8737022306786,7.58393796064214,
11.7898062310485));
#119264=CARTESIAN_POINT('Ctrl Pts',(-10.8826294993968,7.58304066751989,
11.7798054781242));
#119265=CARTESIAN_POINT('Ctrl Pts',(-10.8866100564021,7.5826356770038,11.7752767392976));
#119266=CARTESIAN_POINT('Ctrl Pts',(-10.8951409347728,7.58175691971124,
11.7654194057265));
#119267=CARTESIAN_POINT('Ctrl Pts',(-10.8996788060038,7.58128266708211,
11.7600803918878));
#119268=CARTESIAN_POINT('Ctrl Pts',(-10.9119566425842,7.57998048683745,
11.7453709494854));
#119269=CARTESIAN_POINT('Ctrl Pts',(-10.9195994484237,7.57914873207881,
11.7359209234565));
#119270=CARTESIAN_POINT('Ctrl Pts',(-10.9733837839764,7.5731387209641,11.6672724210527));
#119271=CARTESIAN_POINT('Ctrl Pts',(-11.0139110053601,7.5677438053203,11.6039115574382));
#119272=CARTESIAN_POINT('Ctrl Pts',(-11.0758337722912,7.55780913789568,
11.4830802310864));
#119273=CARTESIAN_POINT('Ctrl Pts',(-11.0993140143457,7.55332132571333,
11.4269589001096));
#119274=CARTESIAN_POINT('Ctrl Pts',(-11.1239259723911,7.54767345631272,
11.3524209442968));
#119275=CARTESIAN_POINT('Ctrl Pts',(-11.1291098421337,7.54640747729846,
11.3354417180618));
#119276=CARTESIAN_POINT('Ctrl Pts',(-11.1371498602182,7.54431326053139,
11.3068046335979));
#119277=CARTESIAN_POINT('Ctrl Pts',(-11.140215154176,7.54347637054082,11.295208939023));
#119278=CARTESIAN_POINT('Ctrl Pts',(-11.1442694027425,7.54231422139191,
11.2788656809099));
#119279=CARTESIAN_POINT('Ctrl Pts',(-11.1454068763686,7.54198134934764,
11.2741562030578));
#119280=CARTESIAN_POINT('Ctrl Pts',(-11.1473052105571,7.54141400011797,
11.2660784444642));
#119281=CARTESIAN_POINT('Ctrl Pts',(-11.1480803708964,7.54117873613198,
11.2627136235878));
#119282=CARTESIAN_POINT('Ctrl Pts',(-11.1496680518051,7.54068927382666,
11.25568055882));
#119283=CARTESIAN_POINT('Ctrl Pts',(-11.1504778310229,7.54043522764607,
11.2520117830932));
#119284=CARTESIAN_POINT('Ctrl Pts',(-11.1525974917259,7.53975805564364,
11.242185293465));
#119285=CARTESIAN_POINT('Ctrl Pts',(-11.1538756030746,7.53933666424317,
11.2360207433045));
#119286=CARTESIAN_POINT('Ctrl Pts',(-11.1594267770394,7.53744388315675,
11.2081230090223));
#119287=CARTESIAN_POINT('Ctrl Pts',(-11.1631359799511,7.53600083947334,
11.1862806485443));
#119288=CARTESIAN_POINT('Ctrl Pts',(-11.1760582182084,7.53005563252371,
11.0945817249614));
#119289=CARTESIAN_POINT('Ctrl Pts',(-11.1796105011957,7.52574958290094,
11.0240710767667));
#119290=CARTESIAN_POINT('Ctrl Pts',(-11.1742170486215,7.5172522330217,10.887097955277));
#119291=CARTESIAN_POINT('Ctrl Pts',(-11.1659541321944,7.51308161537175,
10.8208857684327));
#119292=CARTESIAN_POINT('Ctrl Pts',(-11.1491939774275,7.50780509134025,
10.7418331687425));
#119293=CARTESIAN_POINT('Ctrl Pts',(-11.1459962051112,7.50687017450675,
10.7279897424527));
#119294=CARTESIAN_POINT('Ctrl Pts',(-11.1407620494892,7.50543873167473,
10.7070644571896));
#119295=CARTESIAN_POINT('Ctrl Pts',(-11.1389082708635,7.50494798655903,
10.6999379526993));
#119296=CARTESIAN_POINT('Ctrl Pts',(-11.1354154310126,7.50405156333176,
10.6870092518229));
#119297=CARTESIAN_POINT('Ctrl Pts',(-11.1337983997197,7.50364660150011,
10.6812013238562));
#119298=CARTESIAN_POINT('Ctrl Pts',(-11.1302028513811,7.50276715547185,
10.6686605657566));
#119299=CARTESIAN_POINT('Ctrl Pts',(-11.1282086168535,7.50229217940577,
10.6619325228126));
#119300=CARTESIAN_POINT('Ctrl Pts',(-11.1225829528006,7.50098607288355,
10.6435572738364));
#119301=CARTESIAN_POINT('Ctrl Pts',(-11.1188305686585,7.50015107704404,
10.631948315857));
#119302=CARTESIAN_POINT('Ctrl Pts',(-11.0920525475674,7.49442494220537,
10.553300296523));
#119303=CARTESIAN_POINT('Ctrl Pts',(-11.0631997518326,7.48934234273294,
10.4884118279321));
#119304=CARTESIAN_POINT('Ctrl Pts',(-10.9975180451698,7.47948671327182,
10.3705934060303));
#119305=CARTESIAN_POINT('Ctrl Pts',(-10.9618309628822,7.4747501169921,10.3173021175708));
#119306=CARTESIAN_POINT('Ctrl Pts',(-10.9106490697403,7.46882714053968,
10.2529086745656));
#119307=CARTESIAN_POINT('Ctrl Pts',(-10.8989794028841,7.467526384343,10.2389065214375));
#119308=CARTESIAN_POINT('Ctrl Pts',(-10.8789444381728,7.4653811941965,10.2159711389096));
#119309=CARTESIAN_POINT('Ctrl Pts',(-10.8707566983525,7.46452759484298,
10.2068875351151));
#119310=CARTESIAN_POINT('Ctrl Pts',(-10.8591039732379,7.46334646728263,
10.1943578598798));
#119311=CARTESIAN_POINT('Ctrl Pts',(-10.8557570967964,7.46301100098719,
10.190803677613));
#119312=CARTESIAN_POINT('Ctrl Pts',(-10.8500010354418,7.46244062120765,
10.1847667398202));
#119313=CARTESIAN_POINT('Ctrl Pts',(-10.8476028572891,7.46220489949364,
10.1822736237919));
#119314=CARTESIAN_POINT('Ctrl Pts',(-10.8425874696134,7.46171595909973,
10.1771054605648));
#119315=CARTESIAN_POINT('Ctrl Pts',(-10.8399684556945,7.46146288181669,
10.174432279336));
#119316=CARTESIAN_POINT('Ctrl Pts',(-10.8329566067514,7.46079112356029,
10.1673433189644));
#119317=CARTESIAN_POINT('Ctrl Pts',(-10.828541336462,7.46037412891333,10.1629497534888));
#119318=CARTESIAN_POINT('Ctrl Pts',(-10.8087647728235,7.45853165994443,
10.1435802198638));
#119319=CARTESIAN_POINT('Ctrl Pts',(-10.793029800355,7.45713271717309,10.1289895692622));
#119320=CARTESIAN_POINT('Ctrl Pts',(-10.7591678867197,7.45423697302327,
10.0992691462175));
#119321=CARTESIAN_POINT('Ctrl Pts',(-10.7409671201972,7.45274500648803,
10.0842381354397));
#119322=CARTESIAN_POINT('Ctrl Pts',(-10.7063595370843,7.44999966819764,
10.0573654423217));
#119323=CARTESIAN_POINT('Ctrl Pts',(-10.6900760472545,7.44874325700108,
10.0453802908853));
#119324=CARTESIAN_POINT('Ctrl Pts',(-10.6323821660265,7.44438448625274,
10.005163813606));
#119325=CARTESIAN_POINT('Ctrl Pts',(-10.5894865184984,7.4413024621769,9.9791612565795));
#119326=CARTESIAN_POINT('Ctrl Pts',(-10.5017013264157,7.43509494270162,
9.93333047826263));
#119327=CARTESIAN_POINT('Ctrl Pts',(-10.4569733486797,7.43197825696323,
9.91341701457162));
#119328=CARTESIAN_POINT('Ctrl Pts',(-10.400507908756,7.42802160753003,9.89238218702632));
#119329=CARTESIAN_POINT('Ctrl Pts',(-10.3898188964615,7.4272718114063,9.88857523065238));
#119330=CARTESIAN_POINT('Ctrl Pts',(-10.3726745602887,7.42606711769201,
9.88274691273329));
#119331=CARTESIAN_POINT('Ctrl Pts',(-10.3662537638086,7.42561548428398,
9.8806256362703));
#119332=CARTESIAN_POINT('Ctrl Pts',(-10.3540454888068,7.42475572592515,
9.87670859946695));
#119333=CARTESIAN_POINT('Ctrl Pts',(-10.3482617044017,7.42434796890641,
9.87490197691403));
#119334=CARTESIAN_POINT('Ctrl Pts',(-10.3350620114337,7.42341626688575,
9.87089045431234));
#119335=CARTESIAN_POINT('Ctrl Pts',(-10.3276378651401,7.42289142945741,
9.86871385491808));
#119336=CARTESIAN_POINT('Ctrl Pts',(-10.3046820964827,7.42126584643753,
9.86222863843633));
#119337=CARTESIAN_POINT('Ctrl Pts',(-10.2890836136496,7.42015735168672,
9.85816574280178));
#119338=CARTESIAN_POINT('Ctrl Pts',(-10.2022383123386,7.4139612426353,9.83743892184782));
#119339=CARTESIAN_POINT('Ctrl Pts',(-10.12965318867,7.40867713324825,9.82712518626822));
#119340=CARTESIAN_POINT('Ctrl Pts',(-10.0075903270549,7.3997241386216,9.82125311418582));
#119341=CARTESIAN_POINT('Ctrl Pts',(-9.95848786180473,7.39610887968032,
9.82195977036591));
#119342=CARTESIAN_POINT('Ctrl Pts',(-9.87668310329429,7.39016761705955,
9.82825937951728));
#119343=CARTESIAN_POINT('Ctrl Pts',(-9.84391195329899,7.38781048722023,
9.83217291710457));
#119344=CARTESIAN_POINT('Ctrl Pts',(-9.81128001650616,7.38551240301472,
9.83746835110486));
#119345=CARTESIAN_POINT('Ctrl Pts',(-9.81121465855839,7.38550780042879,
9.83747896288237));
#119346=CARTESIAN_POINT('Ctrl Pts',(-9.81114930150104,7.38550319809767,
9.83748958018586));
#119347=CARTESIAN_POINT('Ctrl Pts',(-9.81114930576479,7.28726551493505,
9.83748957949321));
#119348=CARTESIAN_POINT('Ctrl Pts',(-9.85519968856744,7.29049506618666,
9.83033356159706));
#119349=CARTESIAN_POINT('Ctrl Pts',(-9.89962266941641,7.29377134196203,
9.82568685856417));
#119350=CARTESIAN_POINT('Ctrl Pts',(-9.96506182480563,7.2985783188177,9.82258314744129));
#119351=CARTESIAN_POINT('Ctrl Pts',(-9.98594335352587,7.30010900212892,
9.82214875308509));
#119352=CARTESIAN_POINT('Ctrl Pts',(-10.028665519363,7.30322380343086,9.82239635504111));
#119353=CARTESIAN_POINT('Ctrl Pts',(-10.0504986223138,7.30480659445796,
9.82313041004437));
#119354=CARTESIAN_POINT('Ctrl Pts',(-10.0946051848168,7.30797197528952,
9.82584313524102));
#119355=CARTESIAN_POINT('Ctrl Pts',(-10.1168690011022,7.3095531131394,9.82784972143138));
#119356=CARTESIAN_POINT('Ctrl Pts',(-10.1453318261569,7.31154242376404,
9.83123416982243));
#119357=CARTESIAN_POINT('Ctrl Pts',(-10.1515938824679,7.31197808281688,
9.8320298785049));
#119358=CARTESIAN_POINT('Ctrl Pts',(-10.1615755111745,7.31266899761399,
9.83337985853362));
#119359=CARTESIAN_POINT('Ctrl Pts',(-10.1652992437233,7.31292596585307,
9.8339016502409));
#119360=CARTESIAN_POINT('Ctrl Pts',(-10.1724350044001,7.31341680734857,
9.8349364240891));
#119361=CARTESIAN_POINT('Ctrl Pts',(-10.1758473378235,7.31365082256536,
9.83544657454675));
#119362=CARTESIAN_POINT('Ctrl Pts',(-10.1840342696806,7.31421066878331,
9.83670734142605));
#119363=CARTESIAN_POINT('Ctrl Pts',(-10.1888066473296,7.31453570782569,
9.83747237715991));
#119364=CARTESIAN_POINT('Ctrl Pts',(-10.2053371266664,7.3156574503389,9.84022677520798));
#119365=CARTESIAN_POINT('Ctrl Pts',(-10.2170700803555,7.31644639406028,
9.84236539635367));
#119366=CARTESIAN_POINT('Ctrl Pts',(-10.2460487947011,7.31838152658141,
9.84810358560095));
#119367=CARTESIAN_POINT('Ctrl Pts',(-10.2632505217913,7.31951835213249,
9.85191263910326));
#119368=CARTESIAN_POINT('Ctrl Pts',(-10.3384900116516,7.32446393754164,
9.87035336972859));
#119369=CARTESIAN_POINT('Ctrl Pts',(-10.3954524098334,7.32814088329592,
9.88901151713232));
#119370=CARTESIAN_POINT('Ctrl Pts',(-10.5210572863991,7.33655651133908,
9.94104516928128));
#119371=CARTESIAN_POINT('Ctrl Pts',(-10.5883639569782,7.34130070312863,
9.97691069748441));
#119372=CARTESIAN_POINT('Ctrl Pts',(-10.6618940832352,7.34708549657348,
10.0257618417384));
#119373=CARTESIAN_POINT('Ctrl Pts',(-10.6719454745204,7.34789001319641,
10.032667054387));
#119374=CARTESIAN_POINT('Ctrl Pts',(-10.6876071293454,7.3491664871892,10.0437883563707));
#119375=CARTESIAN_POINT('Ctrl Pts',(-10.693290213132,7.34963453998412,10.0479007674953));
#119376=CARTESIAN_POINT('Ctrl Pts',(-10.7037872067802,7.35050835244923,
10.0556404515272));
#119377=CARTESIAN_POINT('Ctrl Pts',(-10.708610687845,7.35091359202307,10.0592544020934));
#119378=CARTESIAN_POINT('Ctrl Pts',(-10.7192639034136,7.35181703090415,
10.067364647811));
#119379=CARTESIAN_POINT('Ctrl Pts',(-10.7250796041024,7.35231591684206,
10.0718788730091));
#119380=CARTESIAN_POINT('Ctrl Pts',(-10.741992189509,7.35378375748748,10.0852626293453));
#119381=CARTESIAN_POINT('Ctrl Pts',(-10.7529710420379,7.35475843871651,
10.0942784943133));
#119382=CARTESIAN_POINT('Ctrl Pts',(-10.8146467945483,7.36036252513828,
10.1468233154076));
#119383=CARTESIAN_POINT('Ctrl Pts',(-10.8617215715397,7.36515688342821,
10.1943989033175));
#119384=CARTESIAN_POINT('Ctrl Pts',(-10.9498400999013,7.37520603627754,
10.3000644923196));
#119385=CARTESIAN_POINT('Ctrl Pts',(-10.9901836338833,7.380451043011,10.3584060445358));
#119386=CARTESIAN_POINT('Ctrl Pts',(-11.0357146264638,7.38706841774755,
10.4388763534742));
#119387=CARTESIAN_POINT('Ctrl Pts',(-11.0458630622127,7.38860036763467,
10.4580266320085));
#119388=CARTESIAN_POINT('Ctrl Pts',(-11.058260351626,7.3905393158012,10.4830673010665));
#119389=CARTESIAN_POINT('Ctrl Pts',(-11.060997830851,7.39097208422777,10.4887094814884));
#119390=CARTESIAN_POINT('Ctrl Pts',(-11.0653005269334,7.39165949999992,
10.4977610933084));
#119391=CARTESIAN_POINT('Ctrl Pts',(-11.066894701596,7.39191583079058,10.5011565087334));
#119392=CARTESIAN_POINT('Ctrl Pts',(-11.0699256539667,7.39240628402739,
10.5076930958745));
#119393=CARTESIAN_POINT('Ctrl Pts',(-11.0713648617547,7.39264054213048,
10.5108330283381));
#119394=CARTESIAN_POINT('Ctrl Pts',(-11.0747939922603,7.39320212287608,
10.518402125014));
#119395=CARTESIAN_POINT('Ctrl Pts',(-11.0767704049314,7.39352864057986,
10.522837411238));
#119396=CARTESIAN_POINT('Ctrl Pts',(-11.0835623263213,7.39466120180154,
10.5383363386874));
#119397=CARTESIAN_POINT('Ctrl Pts',(-11.0882353917611,7.39545928418995,
10.5494620870147));
#119398=CARTESIAN_POINT('Ctrl Pts',(-11.0994135677282,7.39742156018471,
10.5772645980097));
#119399=CARTESIAN_POINT('Ctrl Pts',(-11.1057112188219,7.39857604753192,
10.5940219427354));
#119400=CARTESIAN_POINT('Ctrl Pts',(-11.1320268859238,7.40365849175708,
10.6692068329938));
#119401=CARTESIAN_POINT('Ctrl Pts',(-11.1478140766051,7.40744723045613,
10.7290149295057));
#119402=CARTESIAN_POINT('Ctrl Pts',(-11.1720056913125,7.41584079796938,
10.8623768700391));
#119403=CARTESIAN_POINT('Ctrl Pts',(-11.1783222942617,7.42044864649759,
10.9360314579091));
#119404=CARTESIAN_POINT('Ctrl Pts',(-11.1776082779531,7.42607917376526,
11.0219468535385));
#119405=CARTESIAN_POINT('Ctrl Pts',(-11.1773189276972,7.42688144202832,
11.0341034497015));
#119406=CARTESIAN_POINT('Ctrl Pts',(-11.1765662293497,7.42815513295858,
11.0532547703275));
#119407=CARTESIAN_POINT('Ctrl Pts',(-11.1762285663683,7.42862267973525,
11.0602537857825));
#119408=CARTESIAN_POINT('Ctrl Pts',(-11.1754842984373,7.42949602241598,
11.073267038325));
#119409=CARTESIAN_POINT('Ctrl Pts',(-11.175093935262,7.4299013027302,11.0792820015953));
#119410=CARTESIAN_POINT('Ctrl Pts',(-11.174123562899,7.43080543937125,11.0926458996963));
#119411=CARTESIAN_POINT('Ctrl Pts',(-11.1735206968037,7.43130498761684,
11.0999928676837));
#119412=CARTESIAN_POINT('Ctrl Pts',(-11.1715499594041,7.43277675482695,
11.1215273945051));
#119413=CARTESIAN_POINT('Ctrl Pts',(-11.1699935045902,7.43375474703828,
11.1356959223877));
#119414=CARTESIAN_POINT('Ctrl Pts',(-11.1658590934259,7.43600272058274,
11.1679302361913));
#119415=CARTESIAN_POINT('Ctrl Pts',(-11.1631176715643,7.43727743456243,
11.185970991878));
#119416=CARTESIAN_POINT('Ctrl Pts',(-11.1523146586199,7.44167655516551,
11.2474157666236));
#119417=CARTESIAN_POINT('Ctrl Pts',(-11.1422334713113,7.44485633235953,
11.2904232018084));
#119418=CARTESIAN_POINT('Ctrl Pts',(-11.111823474531,7.45270276548694,11.3936692006648));
#119419=CARTESIAN_POINT('Ctrl Pts',(-11.0889872088971,7.45740087683083,
11.453027290922));
#119420=CARTESIAN_POINT('Ctrl Pts',(-11.0476609282709,7.4643041727149,11.5389978534609));
#119421=CARTESIAN_POINT('Ctrl Pts',(-11.0326810784807,7.46658208705166,
11.567170426086));
#119422=CARTESIAN_POINT('Ctrl Pts',(-11.0130689804116,7.46928374529891,
11.6006950156024));
#119423=CARTESIAN_POINT('Ctrl Pts',(-11.0095103536734,7.46976379370117,
11.6066565028673));
#119424=CARTESIAN_POINT('Ctrl Pts',(-11.00385034371,7.47051119774183,11.6159505379086));
#119425=CARTESIAN_POINT('Ctrl Pts',(-11.0017846720567,7.47078070836658,
11.6193044886726));
#119426=CARTESIAN_POINT('Ctrl Pts',(-10.9980844729809,7.47125764344715,
11.6252454001082));
#119427=CARTESIAN_POINT('Ctrl Pts',(-10.9964566847459,7.47146548303709,
11.627836365093));
#119428=CARTESIAN_POINT('Ctrl Pts',(-10.9925220474162,7.47196318837868,
11.6340453122912));
#119429=CARTESIAN_POINT('Ctrl Pts',(-10.9902055036909,7.47225241989804,
11.6376570665748));
#119430=CARTESIAN_POINT('Ctrl Pts',(-10.9830502392681,7.47313452422121,
11.6486799090549));
#119431=CARTESIAN_POINT('Ctrl Pts',(-10.9781475431363,7.47372341463591,
11.6560493828098));
#119432=CARTESIAN_POINT('Ctrl Pts',(-10.9664767740408,7.4750913056241,11.6731705472613));
#119433=CARTESIAN_POINT('Ctrl Pts',(-10.9596433381991,7.47586658524173,
11.6828767291657));
#119434=CARTESIAN_POINT('Ctrl Pts',(-10.9346886645188,7.47861449561872,
11.7172076523373));
#119435=CARTESIAN_POINT('Ctrl Pts',(-10.9157558950832,7.48054815310547,
11.741229463679));
#119436=CARTESIAN_POINT('Ctrl Pts',(-10.8940555415662,7.48263984738474,
11.7666602244407));
#119437=CARTESIAN_POINT('Ctrl Pts',(-10.8921947088025,7.48281826351546,
11.7688249559254));
#119438=CARTESIAN_POINT('Ctrl Pts',(-10.8404223914961,7.48775662627848,
11.828611289114));
#119439=CARTESIAN_POINT('Ctrl Pts',(-10.7850427814799,7.49239714324551,
11.8812572533082));
#119440=CARTESIAN_POINT('Ctrl Pts',(-10.6942862226725,7.49967331736426,
11.9521433423309));
#119441=CARTESIAN_POINT('Ctrl Pts',(-10.6624424479499,7.50217150830225,
11.9745664828692));
#119442=CARTESIAN_POINT('Ctrl Pts',(-10.6202249413218,7.50545382701069,
12.0012681013186));
#119443=CARTESIAN_POINT('Ctrl Pts',(-10.6108183454274,7.50618328233104,
12.0070341225404));
#119444=CARTESIAN_POINT('Ctrl Pts',(-10.5955775155201,7.50736291227459,
12.016084288828));
#119445=CARTESIAN_POINT('Ctrl Pts',(-10.5897937219677,7.50781006015288,
12.0194524125259));
#119446=CARTESIAN_POINT('Ctrl Pts',(-10.578708259231,7.50866627415854,12.0257819884076));
#119447=CARTESIAN_POINT('Ctrl Pts',(-10.5734117632605,7.50907501513885,
12.0287521005717));
#119448=CARTESIAN_POINT('Ctrl Pts',(-10.5612085408018,7.51001609675676,
12.0354717746911));
#119449=CARTESIAN_POINT('Ctrl Pts',(-10.5542868419995,7.51054939804968,
12.0391933958879));
#119450=CARTESIAN_POINT('Ctrl Pts',(-10.5324697879892,7.51222915989967,
12.0506438916526));
#119451=CARTESIAN_POINT('Ctrl Pts',(-10.5174467435795,7.51338413810669,
12.0581235653549));
#119452=CARTESIAN_POINT('Ctrl Pts',(-10.4818708143132,7.51611668590152,
12.074897296537));
#119453=CARTESIAN_POINT('Ctrl Pts',(-10.4612011343202,7.51770242286672,
12.0839266946263));
#119454=CARTESIAN_POINT('Ctrl Pts',(-10.3815467789936,7.52380608128021,
12.1160322389629));
#119455=CARTESIAN_POINT('Ctrl Pts',(-10.3209992249661,7.52843811462932,
12.1349289940568));
#119456=CARTESIAN_POINT('Ctrl Pts',(-10.1984958244323,7.53765444871598,
12.162571007012));
#119457=CARTESIAN_POINT('Ctrl Pts',(-10.1367611806452,7.54222271828028,
12.1714391992568));
#119458=CARTESIAN_POINT('Ctrl Pts',(-10.065038971152,7.54726795199432,12.1759919068787));
#119459=CARTESIAN_POINT('Ctrl Pts',(-10.0554606768047,7.54793624946695,
12.1764825372595));
#119460=CARTESIAN_POINT('Ctrl Pts',(-10.040835873149,7.54894725611489,12.1770526523838));
#119461=CARTESIAN_POINT('Ctrl Pts',(-10.0357933267798,7.54929414203913,
12.1772167833914));
#119462=CARTESIAN_POINT('Ctrl Pts',(-10.0272972263487,7.54987556429548,
12.1774386829497));
#119463=CARTESIAN_POINT('Ctrl Pts',(-10.0238442272722,7.55011102054624,
12.1775136706962));
#119464=CARTESIAN_POINT('Ctrl Pts',(-10.0167188985909,7.55059508007801,
12.1776370528487));
#119465=CARTESIAN_POINT('Ctrl Pts',(-10.0130466006967,7.55084357435315,
12.1776834621215));
#119466=CARTESIAN_POINT('Ctrl Pts',(-10.0034589443997,7.55148991746841,
12.1777597757095));
#119467=CARTESIAN_POINT('Ctrl Pts',(-9.99754338211674,7.55188629801649,
12.1777622944516));
#119468=CARTESIAN_POINT('Ctrl Pts',(-9.97103455058822,7.55365275776168,
12.1775738502062));
#119469=CARTESIAN_POINT('Ctrl Pts',(-9.95044706365898,7.55499814457705,
12.1768873352899));
#119470=CARTESIAN_POINT('Ctrl Pts',(-9.89091325727442,7.55883910554718,
12.173336899003));
#119471=CARTESIAN_POINT('Ctrl Pts',(-9.85207646255803,7.56128363162729,
12.1690759062038));
#119472=CARTESIAN_POINT('Ctrl Pts',(-9.71882008265134,7.56966748959021,
12.1477071532082));
#119473=CARTESIAN_POINT('Ctrl Pts',(-9.62633860911317,7.57551203807908,
12.1210126936489));
#119474=CARTESIAN_POINT('Ctrl Pts',(-9.52243717642316,7.58285116080175,
12.0767169669674));
#119475=CARTESIAN_POINT('Ctrl Pts',(-9.50690307542164,7.5839689833877,12.0696920363489));
#119476=CARTESIAN_POINT('Ctrl Pts',(-9.48447152168634,7.58561625695119,
12.0589554493254));
#119477=CARTESIAN_POINT('Ctrl Pts',(-9.47744948836911,7.58613674611029,
12.055508035726));
#119478=CARTESIAN_POINT('Ctrl Pts',(-9.46502701671613,7.58706640900151,
12.0492549735298));
#119479=CARTESIAN_POINT('Ctrl Pts',(-9.45961295183891,7.58747461999549,
12.0464769123747));
#119480=CARTESIAN_POINT('Ctrl Pts',(-9.44833207440883,7.58833168439508,
12.0405775905508));
#119481=CARTESIAN_POINT('Ctrl Pts',(-9.4424696800644,7.58878080374154,12.0374483897113));
#119482=CARTESIAN_POINT('Ctrl Pts',(-9.42713881994972,7.58996530641948,
12.0290976841812));
#119483=CARTESIAN_POINT('Ctrl Pts',(-9.41771541816138,7.59070351455073,
12.0237952077635));
#119484=CARTESIAN_POINT('Ctrl Pts',(-9.37285404803744,7.59426786783325,
11.9977323394992));
#119485=CARTESIAN_POINT('Ctrl Pts',(-9.33844906745561,7.59715447376726,
11.9752597279124));
#119486=CARTESIAN_POINT('Ctrl Pts',(-9.2663042472857,7.60355106637837,11.9225598214281));
#119487=CARTESIAN_POINT('Ctrl Pts',(-9.2291083232013,7.60707620518142,11.8917126486717));
#119488=CARTESIAN_POINT('Ctrl Pts',(-9.14346779251222,7.61569333340251,
11.8113167829369));
#119489=CARTESIAN_POINT('Ctrl Pts',(-9.09728945122025,7.62079035646171,
11.7596036505155));
#119490=CARTESIAN_POINT('Ctrl Pts',(-9.04969565487249,7.62637619838662,
11.6957908910849));
#119491=CARTESIAN_POINT('Ctrl Pts',(-9.04358583168573,7.62710037947976,
11.6873683653177));
#119492=CARTESIAN_POINT('Ctrl Pts',(-9.03497745913946,7.62812983576394,
11.6751644780727));
#119493=CARTESIAN_POINT('Ctrl Pts',(-9.03238806292291,7.6284407231772,11.6714482241731));
#119494=CARTESIAN_POINT('Ctrl Pts',(-9.02788334532991,7.62898360895538,
11.664902957135));
#119495=CARTESIAN_POINT('Ctrl Pts',(-9.02595879918785,7.62921620872815,
11.6620804128033));
#119496=CARTESIAN_POINT('Ctrl Pts',(-9.02188287935203,7.62971020831165,
11.6560464170241));
#119497=CARTESIAN_POINT('Ctrl Pts',(-9.01973501082036,7.62997138056356,
11.6528327159842));
#119498=CARTESIAN_POINT('Ctrl Pts',(-9.01385645676312,7.63068872759903,
11.6439426312588));
#119499=CARTESIAN_POINT('Ctrl Pts',(-9.01015892465356,7.63114279313097,
11.6382443506753));
#119500=CARTESIAN_POINT('Ctrl Pts',(-8.98903637209678,7.63375546439494,
11.605067187394));
#119501=CARTESIAN_POINT('Ctrl Pts',(-8.97270506931862,7.63585102708472,
11.5769049397346));
#119502=CARTESIAN_POINT('Ctrl Pts',(-8.93537468170182,7.64093077034107,
11.5059056353345));
#119503=CARTESIAN_POINT('Ctrl Pts',(-8.91577075809617,7.64387146857802,
11.4624013351057));
#119504=CARTESIAN_POINT('Ctrl Pts',(-8.87221479830077,7.65146665784319,
11.3476136721635));
#119505=CARTESIAN_POINT('Ctrl Pts',(-8.85235207913066,7.65612610292347,
11.2750221382633));
#119506=CARTESIAN_POINT('Ctrl Pts',(-8.83678949046423,7.66205958569363,
11.1851893731293));
#119507=CARTESIAN_POINT('Ctrl Pts',(-8.83436889751725,7.66311553004509,
11.1692864021845));
#119508=CARTESIAN_POINT('Ctrl Pts',(-8.83126851799267,7.66469379887375,
11.1456760963642));
#119509=CARTESIAN_POINT('Ctrl Pts',(-8.83033769030074,7.6652083439785,11.138003183303));
#119510=CARTESIAN_POINT('Ctrl Pts',(-8.82881223362302,7.66613032160656,
11.124301917761));
#119511=CARTESIAN_POINT('Ctrl Pts',(-8.82818845768339,7.6665368347176,11.1182770384605));
#119512=CARTESIAN_POINT('Ctrl Pts',(-8.82696661147169,7.6674003327857,11.105515274149));
#119513=CARTESIAN_POINT('Ctrl Pts',(-8.82638004490823,7.66785765906529,
11.098777534894));
#119514=CARTESIAN_POINT('Ctrl Pts',(-8.82496405541385,7.6690878189272,11.0807129117521));
#119515=CARTESIAN_POINT('Ctrl Pts',(-8.82424040485695,7.66986388469948,
11.0693786996952));
#119516=CARTESIAN_POINT('Ctrl Pts',(-8.82125961410012,7.67402449811763,
11.0089618284884));
#119517=CARTESIAN_POINT('Ctrl Pts',(-8.82191202652291,7.67749727327642,
10.9597907772295));
#119518=CARTESIAN_POINT('Ctrl Pts',(-8.82941569685543,7.68464166316884,
10.8609901001067));
#119519=CARTESIAN_POINT('Ctrl Pts',(-8.83636553731358,7.68830854309182,
10.8114644394558));
#119520=CARTESIAN_POINT('Ctrl Pts',(-8.85814964154146,7.69623600287555,
10.705642174287));
#119521=CARTESIAN_POINT('Ctrl Pts',(-8.87405463299841,7.70048627949963,
10.6496899507921));
#119522=CARTESIAN_POINT('Ctrl Pts',(-8.89759233310584,7.70529304353014,
10.585391678394));
#119523=CARTESIAN_POINT('Ctrl Pts',(-8.90128796778085,7.70601565032005,
10.5756951415607));
#119524=CARTESIAN_POINT('Ctrl Pts',(-8.90667533106688,7.70702415877659,
10.5621024705801));
#119525=CARTESIAN_POINT('Ctrl Pts',(-8.90826058794254,7.70731576572947,
10.5581650358792));
#119526=CARTESIAN_POINT('Ctrl Pts',(-8.91112371990633,7.70783327095792,
10.551163134539));
#119527=CARTESIAN_POINT('Ctrl Pts',(-8.912393327851,7.70805964474647,10.5480953498713));
#119528=CARTESIAN_POINT('Ctrl Pts',(-8.91504615305489,7.70852623311223,
10.5417612041035));
#119529=CARTESIAN_POINT('Ctrl Pts',(-8.91643118149428,7.70876633724323,
10.5384956549827));
#119530=CARTESIAN_POINT('Ctrl Pts',(-8.91930226314544,7.70925705610649,
10.5318105458603));
#119531=CARTESIAN_POINT('Ctrl Pts',(-8.92078984500464,7.70950757811946,
10.5283916819095));
#119532=CARTESIAN_POINT('Ctrl Pts',(-8.92448126239604,7.71012032178206,
10.5200167441402));
#119533=CARTESIAN_POINT('Ctrl Pts',(-8.92670317118583,7.71048152960302,
10.5150686638693));
#119534=CARTESIAN_POINT('Ctrl Pts',(-8.95226235995247,7.71455366154662,
10.4591859432606));
#119535=CARTESIAN_POINT('Ctrl Pts',(-8.97917475356925,7.71807387587225,
10.4099563264487));
#119536=CARTESIAN_POINT('Ctrl Pts',(-9.06038939496961,7.72740206881303,
10.2837060232455));
#119537=CARTESIAN_POINT('Ctrl Pts',(-9.12057561909425,7.73313321001146,
10.2109774769063));
#119538=CARTESIAN_POINT('Ctrl Pts',(-9.20205894599789,7.74041699659072,
10.1335583518798));
#119539=CARTESIAN_POINT('Ctrl Pts',(-9.21563977005296,7.74161636475479,
10.1212451842009));
#119540=CARTESIAN_POINT('Ctrl Pts',(-9.23519198608419,7.74332642162918,
10.1043324453351));
#119541=CARTESIAN_POINT('Ctrl Pts',(-9.24092906785537,7.7438262339833,10.0994651687764));
#119542=CARTESIAN_POINT('Ctrl Pts',(-9.25103840866681,7.74470380011763,
10.091053758916));
#119543=CARTESIAN_POINT('Ctrl Pts',(-9.25539021628676,7.74508056689302,
10.0874853411548));
#119544=CARTESIAN_POINT('Ctrl Pts',(-9.26460000058779,7.74587593122935,
10.0800432034653));
#119545=CARTESIAN_POINT('Ctrl Pts',(-9.26946337762514,7.74629478924844,
10.0761764738583));
#119546=CARTESIAN_POINT('Ctrl Pts',(-9.28123504540855,7.74730602109766,
10.0669682447641));
#119547=CARTESIAN_POINT('Ctrl Pts',(-9.28817250584574,7.74789985363187,
10.0616648105928));
#119548=CARTESIAN_POINT('Ctrl Pts',(-9.31281159390732,7.75000195286584,
10.0432596235438));
#119549=CARTESIAN_POINT('Ctrl Pts',(-9.33082013478496,7.75152601215833,
10.030578394585));
#119550=CARTESIAN_POINT('Ctrl Pts',(-9.37629158006102,7.75534672433294,
10.0004292816455));
#119551=CARTESIAN_POINT('Ctrl Pts',(-9.4041418877605,7.75766335513131,9.98358147941796));
#119552=CARTESIAN_POINT('Ctrl Pts',(-9.51802792521591,7.76703341137145,
9.9209774561804));
#119553=CARTESIAN_POINT('Ctrl Pts',(-9.60889009110396,7.77432048683787,
9.88482364980576));
#119554=CARTESIAN_POINT('Ctrl Pts',(-9.72109540292787,7.78258184088193,
9.85560029742336));
#119555=CARTESIAN_POINT('Ctrl Pts',(-9.73913697270404,7.78388717627685,
9.85135339313152));
#119556=CARTESIAN_POINT('Ctrl Pts',(-9.76293297006085,7.78557253689137,
9.84634158046878));
#119557=CARTESIAN_POINT('Ctrl Pts',(-9.76860237037194,7.78597138913534,
9.84519106945274));
#119558=CARTESIAN_POINT('Ctrl Pts',(-9.77790713634475,7.7866213515191,9.8433740972194));
#119559=CARTESIAN_POINT('Ctrl Pts',(-9.7815374884962,7.78687378639935,9.84268290814946));
#119560=CARTESIAN_POINT('Ctrl Pts',(-9.78833478544891,7.78734419957058,
9.84142188314543));
#119561=CARTESIAN_POINT('Ctrl Pts',(-9.79150087649421,7.7875624007946,9.84084792556047));
#119562=CARTESIAN_POINT('Ctrl Pts',(-9.79724441442967,7.78795664395391,
9.83983101487458));
#119563=CARTESIAN_POINT('Ctrl Pts',(-9.7998210595927,7.78813292929592,9.83938365784728));
#119564=CARTESIAN_POINT('Ctrl Pts',(-9.80531730704864,7.78850777249613,
9.83844824758667));
#119565=CARTESIAN_POINT('Ctrl Pts',(-9.80822746519122,7.78870553243243,
9.83796423470817));
#119566=CARTESIAN_POINT('Ctrl Pts',(-9.81114930150281,7.78890339972193,
9.83748958018557));
#119567=CARTESIAN_POINT('Origin',(-10.,2.67563288526385,11.));
#119568=CARTESIAN_POINT('',(-9.81114929946799,8.38697610116908,9.83748958051613));
#119569=CARTESIAN_POINT('',(-9.81114931542107,8.28715739324099,9.83748957792454));
#119570=CARTESIAN_POINT('',(-9.81114930150157,2.67563288526385,9.83748958018577));
#119571=CARTESIAN_POINT('Ctrl Pts',(-9.8111492994685,8.3869761011691,9.83748958051605));
#119572=CARTESIAN_POINT('Ctrl Pts',(-9.77556036952072,8.38472373587762,
9.84327102921462));
#119573=CARTESIAN_POINT('Ctrl Pts',(-9.74026784148269,8.38244840423991,
9.85068108673375));
#119574=CARTESIAN_POINT('Ctrl Pts',(-9.68692738278437,8.37890183676023,
9.8644634933903));
#119575=CARTESIAN_POINT('Ctrl Pts',(-9.66861095479658,8.37766427285661,
9.86967311841689));
#119576=CARTESIAN_POINT('Ctrl Pts',(-9.64275823187661,8.37588497099228,
9.87770863089574));
#119577=CARTESIAN_POINT('Ctrl Pts',(-9.63511160246356,8.37535460048461,
9.88017141926841));
#119578=CARTESIAN_POINT('Ctrl Pts',(-9.6217623689767,8.37442117849832,9.88462211737458));
#119579=CARTESIAN_POINT('Ctrl Pts',(-9.6160486859111,8.37401922603431,9.88657604089253));
#119580=CARTESIAN_POINT('Ctrl Pts',(-9.60455850842549,8.37320584571282,
9.89060432757954));
#119581=CARTESIAN_POINT('Ctrl Pts',(-9.59878270410538,8.37279438344432,
9.89268007771308));
#119582=CARTESIAN_POINT('Ctrl Pts',(-9.58691541141096,8.37194347296274,
9.89705006792086));
#119583=CARTESIAN_POINT('Ctrl Pts',(-9.58082620253724,8.37150385416781,
9.89934984913751));
#119584=CARTESIAN_POINT('Ctrl Pts',(-9.56526729835222,8.37037265699688,
9.9053739982479));
#119585=CARTESIAN_POINT('Ctrl Pts',(-9.55582640437731,8.36967870390447,
9.90917076896322));
#119586=CARTESIAN_POINT('Ctrl Pts',(-9.5180330990935,8.36686937528555,9.92494177682027));
#119587=CARTESIAN_POINT('Ctrl Pts',(-9.4901080344637,8.36472155024413,9.93790200046723));
#119588=CARTESIAN_POINT('Ctrl Pts',(-9.42177525925837,8.35927994148038,
9.97293197492884));
#119589=CARTESIAN_POINT('Ctrl Pts',(-9.38209521749148,8.35594890082038,
9.99630406285483));
#119590=CARTESIAN_POINT('Ctrl Pts',(-9.29923127863222,8.34865344932402,
10.0518914572739));
#119591=CARTESIAN_POINT('Ctrl Pts',(-9.25667919725604,8.34468453681421,
10.0848711012418));
#119592=CARTESIAN_POINT('Ctrl Pts',(-9.19056427301779,8.33826278624568,
10.1437767738638));
#119593=CARTESIAN_POINT('Ctrl Pts',(-9.16563388113863,8.33577371902835,
10.16805163265));
#119594=CARTESIAN_POINT('Ctrl Pts',(-9.13707791139942,8.33287440325377,
10.1984338343264));
#119595=CARTESIAN_POINT('Ctrl Pts',(-9.13238786957444,8.3323965710423,10.2035126831959));
#119596=CARTESIAN_POINT('Ctrl Pts',(-9.12512747193593,8.33165467008442,
10.2115152059889));
#119597=CARTESIAN_POINT('Ctrl Pts',(-9.12252652107469,8.33138844359755,
10.2144107271394));
#119598=CARTESIAN_POINT('Ctrl Pts',(-9.11767294706688,8.33089088485827,
10.2198681708174));
#119599=CARTESIAN_POINT('Ctrl Pts',(-9.11541710650467,8.33065932822984,
10.2224269782662));
#119600=CARTESIAN_POINT('Ctrl Pts',(-9.11022037385239,8.33012513256885,
10.2283735336706));
#119601=CARTESIAN_POINT('Ctrl Pts',(-9.10728768184697,8.32982308646122,
10.2317683257603));
#119602=CARTESIAN_POINT('Ctrl Pts',(-9.09778120315093,8.32884175804199,
10.2429006760444));
#119603=CARTESIAN_POINT('Ctrl Pts',(-9.09128784721195,8.32816794276472,
10.2507067436001));
#119604=CARTESIAN_POINT('Ctrl Pts',(-9.03833882936707,8.32263438755876,
10.3160609457134));
#119605=CARTESIAN_POINT('Ctrl Pts',(-8.99729122596342,8.31808389526572,
10.3777918201091));
#119606=CARTESIAN_POINT('Ctrl Pts',(-8.93610866554592,8.31008150545563,
10.4917701897934));
#119607=CARTESIAN_POINT('Ctrl Pts',(-8.9133907729591,8.30665195128781,10.5423515549895));
#119608=CARTESIAN_POINT('Ctrl Pts',(-8.88710858139322,8.30178917390322,
10.613987410639));
#119609=CARTESIAN_POINT('Ctrl Pts',(-8.88042563402193,8.30044269590367,
10.6338221867075));
#119610=CARTESIAN_POINT('Ctrl Pts',(-8.86964874752022,8.29805556156961,
10.6688673625453));
#119611=CARTESIAN_POINT('Ctrl Pts',(-8.86532479772586,8.29702210101917,
10.6840017008985));
#119612=CARTESIAN_POINT('Ctrl Pts',(-8.85941664178613,8.29548879372607,
10.7063686473337));
#119613=CARTESIAN_POINT('Ctrl Pts',(-8.85759515350955,8.29499648629831,
10.7135372086045));
#119614=CARTESIAN_POINT('Ctrl Pts',(-8.8558231761747,8.29449691210722,10.7207967332053));
#119615=CARTESIAN_POINT('Ctrl Pts',(-8.85580501912333,8.29449179080672,
10.7208711514294));
#119616=CARTESIAN_POINT('Ctrl Pts',(-8.85576792481073,8.29448132348796,
10.721023250071));
#119617=CARTESIAN_POINT('Ctrl Pts',(-8.85574898819711,8.29447597744853,
10.721100930656));
#119618=CARTESIAN_POINT('Ctrl Pts',(-8.85571029619013,8.29446504914115,
10.7212597208443));
#119619=CARTESIAN_POINT('Ctrl Pts',(-8.85569054151254,8.29445946685143,
10.7213408306099));
#119620=CARTESIAN_POINT('Ctrl Pts',(-8.85565017259324,8.29444805383541,
10.7215066560655));
#119621=CARTESIAN_POINT('Ctrl Pts',(-8.85562955913633,8.29444222308487,
10.7215913719383));
#119622=CARTESIAN_POINT('Ctrl Pts',(-8.85558742951142,8.29443030019162,
10.7217645973198));
#119623=CARTESIAN_POINT('Ctrl Pts',(-8.85556591420485,8.29442420802198,
10.7218531070332));
#119624=CARTESIAN_POINT('Ctrl Pts',(-8.85552193521963,8.29441174853525,
10.7220341193636));
#119625=CARTESIAN_POINT('Ctrl Pts',(-8.85549947248842,8.29440538118856,
10.7221266222053));
#119626=CARTESIAN_POINT('Ctrl Pts',(-8.85545355033533,8.29439235674162,
10.7223158323515));
#119627=CARTESIAN_POINT('Ctrl Pts',(-8.8554300919517,8.29438569960754,10.7224125399213));
#119628=CARTESIAN_POINT('Ctrl Pts',(-8.85538212732569,8.29437208006286,
10.722610384326));
#119629=CARTESIAN_POINT('Ctrl Pts',(-8.85535762223406,8.29436511761703,
10.722711521423));
#119630=CARTESIAN_POINT('Ctrl Pts',(-8.85530751003482,8.29435087095634,
10.722918463683));
#119631=CARTESIAN_POINT('Ctrl Pts',(-8.85528190419233,8.2943435867017,10.7230242691482));
#119632=CARTESIAN_POINT('Ctrl Pts',(-8.85522953315601,8.29432867889302,
10.7232408019257));
#119633=CARTESIAN_POINT('Ctrl Pts',(-8.85520276935465,8.29432105529422,
10.7233515295838));
#119634=CARTESIAN_POINT('Ctrl Pts',(-8.85514802169724,8.29430545015865,
10.7235781765189));
#119635=CARTESIAN_POINT('Ctrl Pts',(-8.85512003938032,8.29429746857302,
10.723694096169));
#119636=CARTESIAN_POINT('Ctrl Pts',(-8.8550627904312,8.29428112764478,10.7239314138862));
#119637=CARTESIAN_POINT('Ctrl Pts',(-8.8550335255047,8.2942727682497,10.724052812343));
#119638=CARTESIAN_POINT('Ctrl Pts',(-8.85497364334648,8.29425565063358,
10.7243013924929));
#119639=CARTESIAN_POINT('Ctrl Pts',(-8.85494302799789,8.29424689235375,
10.7244285746273));
#119640=CARTESIAN_POINT('Ctrl Pts',(-8.85488037307807,8.29422895456967,
10.7246890461119));
#119641=CARTESIAN_POINT('Ctrl Pts',(-8.854848335588,8.29421977499969,10.7248223359591));
#119642=CARTESIAN_POINT('Ctrl Pts',(-8.85479779340273,8.29420528166352,
10.7250327750455));
#119643=CARTESIAN_POINT('Ctrl Pts',(-8.85477927322158,8.2941999683856,10.7251099206018));
#119644=CARTESIAN_POINT('Ctrl Pts',(-8.85473760971123,8.29418800989958,
10.7252835466628));
#119645=CARTESIAN_POINT('Ctrl Pts',(-8.85471447078386,8.29418136455375,
10.7253800281986));
#119646=CARTESIAN_POINT('Ctrl Pts',(-8.85466241491039,8.29416640570187,
10.7255972046706));
#119647=CARTESIAN_POINT('Ctrl Pts',(-8.85463350485297,8.29415809197843,
10.7257179012439));
#119648=CARTESIAN_POINT('Ctrl Pts',(-8.85456846424777,8.29413937440689,
10.7259896288093));
#119649=CARTESIAN_POINT('Ctrl Pts',(-8.85453234449702,8.29412897021821,
10.7261406623607));
#119650=CARTESIAN_POINT('Ctrl Pts',(-8.85445108493201,8.29410554213005,
10.7264807438894));
#119651=CARTESIAN_POINT('Ctrl Pts',(-8.85440596204729,8.2940925176959,10.7266697958807));
#119652=CARTESIAN_POINT('Ctrl Pts',(-8.85430445601056,8.2940631848596,10.7270955438495));
#119653=CARTESIAN_POINT('Ctrl Pts',(-8.85424809941994,8.2940468756198,10.7273322460922));
#119654=CARTESIAN_POINT('Ctrl Pts',(-8.85415859059837,8.29402093487177,
10.7277087081224));
#119655=CARTESIAN_POINT('Ctrl Pts',(-8.85412539055327,8.29401130487389,
10.7278484566327));
#119656=CARTESIAN_POINT('Ctrl Pts',(-8.85396192671454,8.29396385005024,
10.7285370829823));
#119657=CARTESIAN_POINT('Ctrl Pts',(-8.85383203190104,8.29392601357968,
10.7290860475398));
#119658=CARTESIAN_POINT('Ctrl Pts',(-8.85230338138177,8.29347923570598,
10.7355672447981));
#119659=CARTESIAN_POINT('Ctrl Pts',(-8.85095032377587,8.29306885722141,
10.7415100590245));
#119660=CARTESIAN_POINT('Ctrl Pts',(-8.84795378748113,8.29212451211253,
10.7551598816575));
#119661=CARTESIAN_POINT('Ctrl Pts',(-8.84634142619944,8.29158958243961,
10.7628733477612));
#119662=CARTESIAN_POINT('Ctrl Pts',(-8.84222839638118,8.29014948708989,
10.7835856035655));
#119663=CARTESIAN_POINT('Ctrl Pts',(-8.83986932894413,8.28923995025461,
10.7966110167332));
#119664=CARTESIAN_POINT('Ctrl Pts',(-8.82209528764146,8.28162592791745,
10.905151717001));
#119665=CARTESIAN_POINT('Ctrl Pts',(-8.81828779635137,8.27455055149884,
11.0021763687677));
#119666=CARTESIAN_POINT('Ctrl Pts',(-8.8298185325078,8.2644435196521,11.139494176537));
#119667=CARTESIAN_POINT('Ctrl Pts',(-8.83539712749543,8.2614401490568,11.1802327814251));
#119668=CARTESIAN_POINT('Ctrl Pts',(-8.84707469331223,8.25698293784529,
11.2414745303275));
#119669=CARTESIAN_POINT('Ctrl Pts',(-8.85161993797699,8.25548208385647,
11.2622405022161));
#119670=CARTESIAN_POINT('Ctrl Pts',(-8.85816116729086,8.25359407535006,
11.2886778389005));
#119671=CARTESIAN_POINT('Ctrl Pts',(-8.85964150301728,8.25318175958601,
11.2944712493583));
#119672=CARTESIAN_POINT('Ctrl Pts',(-8.86210596052712,8.25251907086765,
11.3038187179651));
#119673=CARTESIAN_POINT('Ctrl Pts',(-8.86306274081926,8.25226721492617,
11.307379778266));
#119674=CARTESIAN_POINT('Ctrl Pts',(-8.86494629057716,8.25178178587113,
11.3142610717138));
#119675=CARTESIAN_POINT('Ctrl Pts',(-8.86587093115574,8.25154810356121,
11.3175818005444));
#119676=CARTESIAN_POINT('Ctrl Pts',(-8.86817379814349,8.25097714500599,
11.3257139228676));
#119677=CARTESIAN_POINT('Ctrl Pts',(-8.86956816086632,8.25064077735985,
11.3305207558966));
#119678=CARTESIAN_POINT('Ctrl Pts',(-8.87367881022585,8.24967511525845,
11.3443611763634));
#119679=CARTESIAN_POINT('Ctrl Pts',(-8.87647310695524,8.24904997251947,
11.3533714425046));
#119680=CARTESIAN_POINT('Ctrl Pts',(-8.90036742997673,8.24394443481163,
11.4272689157817));
#119681=CARTESIAN_POINT('Ctrl Pts',(-8.92696433820455,8.23972572386603,
11.4902524749306));
#119682=CARTESIAN_POINT('Ctrl Pts',(-8.98652447135822,8.2318437015954,11.6028778939458));
#119683=CARTESIAN_POINT('Ctrl Pts',(-9.01807750091479,8.22819215501801,
11.6530099510619));
#119684=CARTESIAN_POINT('Ctrl Pts',(-9.06618489197308,8.22304524692729,
11.7180225855625));
#119685=CARTESIAN_POINT('Ctrl Pts',(-9.0795883688967,8.22164907248295,11.7351254544231));
#119686=CARTESIAN_POINT('Ctrl Pts',(-9.10386867223547,8.21917469201588,
11.7644015508209));
#119687=CARTESIAN_POINT('Ctrl Pts',(-9.11453998748962,8.21810426192985,
11.7767378011318));
#119688=CARTESIAN_POINT('Ctrl Pts',(-9.13066974467157,8.21650840800628,
11.794619648124));
#119689=CARTESIAN_POINT('Ctrl Pts',(-9.13593276951992,8.21599102097178,
11.8003394869624));
#119690=CARTESIAN_POINT('Ctrl Pts',(-9.14540153482438,8.21506578495448,
11.810427844803));
#119691=CARTESIAN_POINT('Ctrl Pts',(-9.14958516104849,8.21465887888075,
11.8148168061963));
#119692=CARTESIAN_POINT('Ctrl Pts',(-9.15849164908155,8.21379646346055,
11.8240171176682));
#119693=CARTESIAN_POINT('Ctrl Pts',(-9.16322229207724,8.2133406271567,11.8288205952672));
#119694=CARTESIAN_POINT('Ctrl Pts',(-9.17595825122229,8.21211913328534,
11.84153246103));
#119695=CARTESIAN_POINT('Ctrl Pts',(-9.18403593992989,8.21135032390752,
11.8493670138083));
#119696=CARTESIAN_POINT('Ctrl Pts',(-9.22257998300997,8.20770814724297,
11.88569358494));
#119697=CARTESIAN_POINT('Ctrl Pts',(-9.25443044085048,8.20477275739549,
11.9126665983159));
#119698=CARTESIAN_POINT('Ctrl Pts',(-9.37506482398508,8.19391375305726,
12.0042923467936));
#119699=CARTESIAN_POINT('Ctrl Pts',(-9.47133148950188,8.18566358757108,
12.0581368006178));
#119700=CARTESIAN_POINT('Ctrl Pts',(-9.58318148769671,8.17716659114382,
12.1015724456768));
#119701=CARTESIAN_POINT('Ctrl Pts',(-9.59275712701194,8.17644782570462,
12.1051483083695));
#119702=CARTESIAN_POINT('Ctrl Pts',(-9.60979913204881,8.17518534133158,
12.1112607684766));
#119703=CARTESIAN_POINT('Ctrl Pts',(-9.61724659686887,8.1746392171673,12.1138478593024));
#119704=CARTESIAN_POINT('Ctrl Pts',(-9.62860371626302,8.17381544488009,
12.1176657161515));
#119705=CARTESIAN_POINT('Ctrl Pts',(-9.63249456933567,8.17353483024211,
12.1189511215168));
#119706=CARTESIAN_POINT('Ctrl Pts',(-9.63961275152208,8.17302447771851,
12.1212615925268));
#119707=CARTESIAN_POINT('Ctrl Pts',(-9.6428378243459,8.17279438756758,12.1222930582728));
#119708=CARTESIAN_POINT('Ctrl Pts',(-9.65014179218854,8.17227583701901,
12.1245943914682));
#119709=CARTESIAN_POINT('Ctrl Pts',(-9.65422318333184,8.17198785130665,
12.1258559878503));
#119710=CARTESIAN_POINT('Ctrl Pts',(-9.66483521445962,8.17124344131276,
12.1290731155613));
#119711=CARTESIAN_POINT('Ctrl Pts',(-9.67137623671441,8.17078889490343,
12.1309942357473));
#119712=CARTESIAN_POINT('Ctrl Pts',(-9.72293768046522,8.16723676432551,
12.1456529070027));
#119713=CARTESIAN_POINT('Ctrl Pts',(-9.76866986137388,8.16427046876545,
12.1557558409163));
#119714=CARTESIAN_POINT('Ctrl Pts',(-9.83105704888142,8.16032424278019,
12.1656849631472));
#119715=CARTESIAN_POINT('Ctrl Pts',(-9.84727920570528,8.15930722514059,
12.1679210288769));
#119716=CARTESIAN_POINT('Ctrl Pts',(-9.91376978636862,8.1551586412886,12.1756770283791));
#119717=CARTESIAN_POINT('Ctrl Pts',(-9.96432054234315,8.15204853487959,
12.1782949303744));
#119718=CARTESIAN_POINT('Ctrl Pts',(-10.0631460941493,8.1458502025093,12.1770460461663));
#119719=CARTESIAN_POINT('Ctrl Pts',(-10.1113214028668,8.14277339313188,
12.1734698690164));
#119720=CARTESIAN_POINT('Ctrl Pts',(-10.1703416913516,8.13886170294202,
12.1654212255078));
#119721=CARTESIAN_POINT('Ctrl Pts',(-10.1815226915575,8.13811442629396,
12.1637321094811));
#119722=CARTESIAN_POINT('Ctrl Pts',(-10.1993400586989,8.13691282746779,
12.1607774189109));
#119723=CARTESIAN_POINT('Ctrl Pts',(-10.2059930411572,8.13646173958394,
12.1596152547496));
#119724=CARTESIAN_POINT('Ctrl Pts',(-10.2185969903339,8.13560240739732,
12.1573016696628));
#119725=CARTESIAN_POINT('Ctrl Pts',(-10.2245498017528,8.13519452576914,
12.1561614000505));
#119726=CARTESIAN_POINT('Ctrl Pts',(-10.2380950000418,8.13426167991051,
12.1534582429777));
#119727=CARTESIAN_POINT('Ctrl Pts',(-10.2456812241632,8.1337358150676,12.1518662589303));
#119728=CARTESIAN_POINT('Ctrl Pts',(-10.2690688831002,8.13210377290235,
12.1467167623073));
#119729=CARTESIAN_POINT('Ctrl Pts',(-10.2848124915868,8.13098975698842,
12.1429082186581));
#119730=CARTESIAN_POINT('Ctrl Pts',(-10.3698947637703,8.12488238159755,
12.1204588314285));
#119731=CARTESIAN_POINT('Ctrl Pts',(-10.4374857565018,8.11970071870876,
12.0958344744591));
#119732=CARTESIAN_POINT('Ctrl Pts',(-10.5476141593115,8.11078291768397,
12.0438929028704));
#119733=CARTESIAN_POINT('Ctrl Pts',(-10.5914213181272,8.10709812416089,
12.0197130373406));
#119734=CARTESIAN_POINT('Ctrl Pts',(-10.6616120180867,8.10106717299453,
11.974921507908));
#119735=CARTESIAN_POINT('Ctrl Pts',(-10.6888954577046,8.09868862901539,
11.9558378013248));
#119736=CARTESIAN_POINT('Ctrl Pts',(-10.7207648882595,8.09589977148649,
11.9314718101271));
#119737=CARTESIAN_POINT('Ctrl Pts',(-10.7261573447767,8.09542751929018,
11.927274109092));
#119738=CARTESIAN_POINT('Ctrl Pts',(-10.734549923372,8.09469234436067,11.9206228799053));
#119739=CARTESIAN_POINT('Ctrl Pts',(-10.7375748882609,8.09442732519014,
11.9182011556447));
#119740=CARTESIAN_POINT('Ctrl Pts',(-10.7432433923885,8.0939307199376,11.9136169797366));
#119741=CARTESIAN_POINT('Ctrl Pts',(-10.7458894692348,8.09369892062497,
11.9114579672218));
#119742=CARTESIAN_POINT('Ctrl Pts',(-10.7520125790718,8.09316250546291,
11.9064174175853));
#119743=CARTESIAN_POINT('Ctrl Pts',(-10.7554824776741,8.09285849911824,
11.9035273551934));
#119744=CARTESIAN_POINT('Ctrl Pts',(-10.7668289374351,8.09186399428393,
11.8939658762343));
#119745=CARTESIAN_POINT('Ctrl Pts',(-10.7746346836783,8.09117916789845,
11.8872106468071));
#119746=CARTESIAN_POINT('Ctrl Pts',(-10.8358071347924,8.08579753893997,
11.8328480184471));
#119747=CARTESIAN_POINT('Ctrl Pts',(-10.8848330255204,8.08138838120861,
11.7805656415313));
#119748=CARTESIAN_POINT('Ctrl Pts',(-10.9638258998428,8.07344124306554,
11.6792471731147));
#119749=CARTESIAN_POINT('Ctrl Pts',(-10.9955312365917,8.06991996865626,
11.6318655206112));
#119750=CARTESIAN_POINT('Ctrl Pts',(-11.0341981948828,8.06493959727346,
11.5638982801113));
#119751=CARTESIAN_POINT('Ctrl Pts',(-11.0442094919244,8.06357223949637,
11.5451363438546));
#119752=CARTESIAN_POINT('Ctrl Pts',(-11.0608737487675,8.06114427115427,
11.5117610145093));
#119753=CARTESIAN_POINT('Ctrl Pts',(-11.0677461051274,8.06009102499601,
11.4972631714739));
#119754=CARTESIAN_POINT('Ctrl Pts',(-11.0774845391716,8.0585159330378,11.4755857098771));
#119755=CARTESIAN_POINT('Ctrl Pts',(-11.0805797182078,8.05800181820763,
11.4685105841374));
#119756=CARTESIAN_POINT('Ctrl Pts',(-11.0859783040471,8.05708021802041,
11.4558320776051));
#119757=CARTESIAN_POINT('Ctrl Pts',(-11.088308497504,8.05667364771427,11.4502403488778));
#119758=CARTESIAN_POINT('Ctrl Pts',(-11.0931513497016,8.05580961131835,
11.4383617515122));
#119759=CARTESIAN_POINT('Ctrl Pts',(-11.095653134681,8.05535180055128,11.4320707160929));
#119760=CARTESIAN_POINT('Ctrl Pts',(-11.1022157988622,8.05411930843729,
11.4151445394574));
#119761=CARTESIAN_POINT('Ctrl Pts',(-11.1061768648162,8.05334137488469,
11.4044717343481));
#119762=CARTESIAN_POINT('Ctrl Pts',(-11.1246360682623,8.04954343197783,
11.3524343236212));
#119763=CARTESIAN_POINT('Ctrl Pts',(-11.1369704328243,8.04645450635206,
11.3103443911239));
#119764=CARTESIAN_POINT('Ctrl Pts',(-11.1636685499137,8.03801779824824,
11.1959463093792));
#119765=CARTESIAN_POINT('Ctrl Pts',(-11.1736415620508,8.03257243928809,
11.1228145197623));
#119766=CARTESIAN_POINT('Ctrl Pts',(-11.1779946282035,8.02497180746589,
11.0187840070013));
#119767=CARTESIAN_POINT('Ctrl Pts',(-11.1780862793021,8.02276344467305,
10.9882890995139));
#119768=CARTESIAN_POINT('Ctrl Pts',(-11.1765702871003,8.01975319249104,
10.9459835267386));
#119769=CARTESIAN_POINT('Ctrl Pts',(-11.1759673801608,8.01891706467461,
10.9341504419125));
#119770=CARTESIAN_POINT('Ctrl Pts',(-11.1746030962002,8.01747091702478,
10.9135086773689));
#119771=CARTESIAN_POINT('Ctrl Pts',(-11.1739209164978,8.01685745661529,
10.9046958766725));
#119772=CARTESIAN_POINT('Ctrl Pts',(-11.1727604269661,8.01595385699603,
10.8916190080917));
#119773=CARTESIAN_POINT('Ctrl Pts',(-11.1723579483332,8.0156598477707,10.8873487643182));
#119774=CARTESIAN_POINT('Ctrl Pts',(-11.1716283226216,8.01515824444408,
10.880035411871));
#119775=CARTESIAN_POINT('Ctrl Pts',(-11.1713126327618,8.01495003274469,
10.8769912772895));
#119776=CARTESIAN_POINT('Ctrl Pts',(-11.1705631440484,8.01447514575751,
10.8700287367744));
#119777=CARTESIAN_POINT('Ctrl Pts',(-11.1701215350591,8.01420890454771,
10.8661112484281));
#119778=CARTESIAN_POINT('Ctrl Pts',(-11.1688465910538,8.01347590622786,
10.8552897112199));
#119779=CARTESIAN_POINT('Ctrl Pts',(-11.1679717506223,8.01301136043032,
10.84839057879));
#119780=CARTESIAN_POINT('Ctrl Pts',(-11.1627181641664,8.01042025516647,
10.8097085582477));
#119781=CARTESIAN_POINT('Ctrl Pts',(-11.1571028554689,8.00835439469295,
10.7781041898662));
#119782=CARTESIAN_POINT('Ctrl Pts',(-11.1365813725998,8.00231024781571,
10.6848945604035));
#119783=CARTESIAN_POINT('Ctrl Pts',(-11.1179889128614,7.99843557217222,
10.6242204245122));
#119784=CARTESIAN_POINT('Ctrl Pts',(-11.0783325469976,7.99176561236707,
10.5243551456662));
#119785=CARTESIAN_POINT('Ctrl Pts',(-11.059772838309,7.98900697270997,10.4843254965805));
#119786=CARTESIAN_POINT('Ctrl Pts',(-11.0304279102795,7.98501539574614,
10.4293460984991));
#119787=CARTESIAN_POINT('Ctrl Pts',(-11.0214698448081,7.98383719326704,
10.4134619732352));
#119788=CARTESIAN_POINT('Ctrl Pts',(-11.004862406242,7.9817165733481,10.3855493721757));
#119789=CARTESIAN_POINT('Ctrl Pts',(-10.9973565239308,7.98077911798206,
10.3734395757147));
#119790=CARTESIAN_POINT('Ctrl Pts',(-10.9856364938995,7.97934458121354,
10.3552751714333));
#119791=CARTESIAN_POINT('Ctrl Pts',(-10.9815819199564,7.97885331969403,
10.3491188027346));
#119792=CARTESIAN_POINT('Ctrl Pts',(-10.9741065406715,7.97795635819017,
10.3379970835156));
#119793=CARTESIAN_POINT('Ctrl Pts',(-10.9707048642027,7.97755137889554,
10.3330191319703));
#119794=CARTESIAN_POINT('Ctrl Pts',(-10.9632652970032,7.97667236070633,
10.322309670439));
#119795=CARTESIAN_POINT('Ctrl Pts',(-10.959214167537,7.97619783367544,10.3165876849829));
#119796=CARTESIAN_POINT('Ctrl Pts',(-10.9479909698979,7.97489416457215,
10.3010319604868));
#119797=CARTESIAN_POINT('Ctrl Pts',(-10.940717338681,7.97406118087562,10.2912729236704));
#119798=CARTESIAN_POINT('Ctrl Pts',(-10.8884637231021,7.96815711651826,
10.2233860466446));
#119799=CARTESIAN_POINT('Ctrl Pts',(-10.8382881672612,7.96287898735427,
10.1694782338457));
#119800=CARTESIAN_POINT('Ctrl Pts',(-10.7371596300048,7.95297393295788,
10.0793858653608));
#119801=CARTESIAN_POINT('Ctrl Pts',(-10.687710650999,7.9483936639308,10.0418825114237));
#119802=CARTESIAN_POINT('Ctrl Pts',(-10.620444846729,7.9426433214011,9.99876840340745));
#119803=CARTESIAN_POINT('Ctrl Pts',(-10.6051303297619,7.94136418514984,
9.98943883309905));
#119804=CARTESIAN_POINT('Ctrl Pts',(-10.5791490245254,7.93925066047584,
9.9744136098997));
#119805=CARTESIAN_POINT('Ctrl Pts',(-10.5685971188126,7.93840742719764,
9.96852611233574));
#119806=CARTESIAN_POINT('Ctrl Pts',(-10.553676949268,7.93723806798522,9.96049987630695));
#119807=CARTESIAN_POINT('Ctrl Pts',(-10.5493836168286,7.93690420644284,
9.95822444118138));
#119808=CARTESIAN_POINT('Ctrl Pts',(-10.5420132816432,7.93633570256747,
9.95437645209557));
#119809=CARTESIAN_POINT('Ctrl Pts',(-10.5389432447222,7.93610026526437,
9.95279076510248));
#119810=CARTESIAN_POINT('Ctrl Pts',(-10.5325256581536,7.93561100817818,
9.94951175249149));
#119811=CARTESIAN_POINT('Ctrl Pts',(-10.529176947732,7.93535733640226,9.94782088325067));
#119812=CARTESIAN_POINT('Ctrl Pts',(-10.5202101482378,7.93468225660047,
9.94334690110892));
#119813=CARTESIAN_POINT('Ctrl Pts',(-10.5145777251602,7.93426256434568,
9.94059255298898));
#119814=CARTESIAN_POINT('Ctrl Pts',(-10.48935751592,7.93240146725709,9.92850804807132));
#119815=CARTESIAN_POINT('Ctrl Pts',(-10.4695347933041,7.93098719496237,
9.91967458575304));
#119816=CARTESIAN_POINT('Ctrl Pts',(-10.3702975115948,7.92408979181832,
9.87870022746897));
#119817=CARTESIAN_POINT('Ctrl Pts',(-10.2877803202513,7.91890732163529,
9.85474082158606));
#119818=CARTESIAN_POINT('Ctrl Pts',(-10.1480111623576,7.91005607855261,
9.83023567037699));
#119819=CARTESIAN_POINT('Ctrl Pts',(-10.0920172380915,7.90649482521806,
9.82450541646872));
#119820=CARTESIAN_POINT('Ctrl Pts',(-10.0241131885421,7.90203748585756,
9.82243849792616));
#119821=CARTESIAN_POINT('Ctrl Pts',(-10.0123893482796,7.90126314686159,
9.82225680856534));
#119822=CARTESIAN_POINT('Ctrl Pts',(-9.99382119583592,7.90002830578992,
9.82224632299599));
#119823=CARTESIAN_POINT('Ctrl Pts',(-9.98697752892163,7.89957136504279,
9.82230211291889));
#119824=CARTESIAN_POINT('Ctrl Pts',(-9.97409001878083,7.89870729013057,
9.82251951785322));
#119825=CARTESIAN_POINT('Ctrl Pts',(-9.96804615437512,7.89830057412994,
9.82266803221052));
#119826=CARTESIAN_POINT('Ctrl Pts',(-9.95440574080568,7.89737916514482,
9.82310832417448));
#119827=CARTESIAN_POINT('Ctrl Pts',(-9.94681039618479,7.89686365393204,
9.82342713168355));
#119828=CARTESIAN_POINT('Ctrl Pts',(-9.923826157997,7.89529598211059,9.82461488221447));
#119829=CARTESIAN_POINT('Ctrl Pts',(-9.90845125909614,7.89423685099825,
9.82571237833746));
#119830=CARTESIAN_POINT('Ctrl Pts',(-9.86565153063747,7.89125793212587,
9.82961314496543));
#119831=CARTESIAN_POINT('Ctrl Pts',(-9.83831699479807,7.88932006193749,
9.8330761678256));
#119832=CARTESIAN_POINT('Ctrl Pts',(-9.81114930150157,7.88735883108162,
9.83748958018577));
#119833=CARTESIAN_POINT('Ctrl Pts',(-9.81114930150278,7.78890339972192,
9.83748958018558));
#119834=CARTESIAN_POINT('Ctrl Pts',(-9.82455959941259,7.78981154754944,
9.83531106712956));
#119835=CARTESIAN_POINT('Ctrl Pts',(-9.83799741169626,7.79070711032302,
9.83336601946057));
#119836=CARTESIAN_POINT('Ctrl Pts',(-9.93521180416505,7.79710149568767,
9.82100785844903));
#119837=CARTESIAN_POINT('Ctrl Pts',(-10.0198595166984,7.80223158742924,
9.81939454282834));
#119838=CARTESIAN_POINT('Ctrl Pts',(-10.1673483502748,7.81141878983337,
9.83246451178699));
#119839=CARTESIAN_POINT('Ctrl Pts',(-10.2301685310679,7.81541166472953,
9.8432089351587));
#119840=CARTESIAN_POINT('Ctrl Pts',(-10.3055645046629,7.82049322285603,
9.86249088603078));
#119841=CARTESIAN_POINT('Ctrl Pts',(-10.3192547339337,7.82142754999622,
9.86625706722847));
#119842=CARTESIAN_POINT('Ctrl Pts',(-10.3399335280042,7.8228581920035,9.87235003793819));
#119843=CARTESIAN_POINT('Ctrl Pts',(-10.3469741886334,7.82334873433376,
9.8744964910309));
#119844=CARTESIAN_POINT('Ctrl Pts',(-10.3597425380678,7.82424483746663,
9.87852031018943));
#119845=CARTESIAN_POINT('Ctrl Pts',(-10.3654768567892,7.82464968295685,
9.88037593219935));
#119846=CARTESIAN_POINT('Ctrl Pts',(-10.3778551841324,7.82552893260949,
9.88448677769641));
#119847=CARTESIAN_POINT('Ctrl Pts',(-10.3844937571763,7.82600382882605,
9.88675751234349));
#119848=CARTESIAN_POINT('Ctrl Pts',(-10.4026191950038,7.82730985537383,
9.8931388131751));
#119849=CARTESIAN_POINT('Ctrl Pts',(-10.4140628291687,7.82814485175348,
9.89736866668973));
#119850=CARTESIAN_POINT('Ctrl Pts',(-10.4913154723831,7.83385479028743,
9.92729536393068));
#119851=CARTESIAN_POINT('Ctrl Pts',(-10.5547511553008,7.83891983013832,
9.95868636168445));
#119852=CARTESIAN_POINT('Ctrl Pts',(-10.6585079027739,7.84780800796341,
10.0222132266455));
#119853=CARTESIAN_POINT('Ctrl Pts',(-10.700254280645,7.85157313324339,10.0516627286598));
#119854=CARTESIAN_POINT('Ctrl Pts',(-10.7704768756123,7.85814043338087,
10.108372721199));
#119855=CARTESIAN_POINT('Ctrl Pts',(-10.7997480578436,7.86095902758692,
10.134530455424));
#119856=CARTESIAN_POINT('Ctrl Pts',(-10.8313209784478,7.86404673599207,
10.1657177045761));
#119857=CARTESIAN_POINT('Ctrl Pts',(-10.8349565970713,7.86440302925653,
10.1693562731244));
#119858=CARTESIAN_POINT('Ctrl Pts',(-10.8416795705965,7.86506308161973,
10.1761734432601));
#119859=CARTESIAN_POINT('Ctrl Pts',(-10.8447730353988,7.86536727369523,
10.1793458612783));
#119860=CARTESIAN_POINT('Ctrl Pts',(-10.8478763011623,7.86567284703338,
10.1825644722537));
#119861=CARTESIAN_POINT('Ctrl Pts',(-10.8479040161325,7.86567557611347,
10.1825932202869));
#119862=CARTESIAN_POINT('Ctrl Pts',(-10.8479594469965,7.86568103443211,
10.182650723164));
#119863=CARTESIAN_POINT('Ctrl Pts',(-10.8479871628904,7.86568376367067,
10.1826794780087));
#119864=CARTESIAN_POINT('Ctrl Pts',(-10.8480426044558,7.86568922317803,
10.1827370036982));
#119865=CARTESIAN_POINT('Ctrl Pts',(-10.8480703300911,7.8656919534433,10.1827657745079));
#119866=CARTESIAN_POINT('Ctrl Pts',(-10.8481258001039,7.86569741588688,
10.1828233414389));
#119867=CARTESIAN_POINT('Ctrl Pts',(-10.8481535444954,7.86570014806661,
10.1828521375793));
#119868=CARTESIAN_POINT('Ctrl Pts',(-10.8482090611459,7.86570561523781,
10.1829097646572));
#119869=CARTESIAN_POINT('Ctrl Pts',(-10.8482368334248,7.86570835023132,
10.1829385956221));
#119870=CARTESIAN_POINT('Ctrl Pts',(-10.8482924151944,7.8657138239504,10.1829963020703));
#119871=CARTESIAN_POINT('Ctrl Pts',(-10.8483202246671,7.86571656267431,
10.1830251775434));
#119872=CARTESIAN_POINT('Ctrl Pts',(-10.8483758903419,7.86572204479174,
10.1830829829172));
#119873=CARTESIAN_POINT('Ctrl Pts',(-10.8484037465364,7.86572478818462,
10.1831119128204));
#119874=CARTESIAN_POINT('Ctrl Pts',(-10.8484595153598,7.86573028059603,
10.1831698371661));
#119875=CARTESIAN_POINT('Ctrl Pts',(-10.8484874279979,7.86573302961562,
10.1831988316308));
#119876=CARTESIAN_POINT('Ctrl Pts',(-10.8485433196438,7.86573853425927,
10.1832568954587));
#119877=CARTESIAN_POINT('Ctrl Pts',(-10.8485712986673,7.86574128988507,
10.1832859648531));
#119878=CARTESIAN_POINT('Ctrl Pts',(-10.8486273332923,7.86574680874696,
10.1833441891921));
#119879=CARTESIAN_POINT('Ctrl Pts',(-10.8486553888782,7.86574957198171,
10.1833733441376));
#119880=CARTESIAN_POINT('Ctrl Pts',(-10.8487115871372,7.86575510709709,
10.1834317505519));
#119881=CARTESIAN_POINT('Ctrl Pts',(-10.848739729728,7.86575787896983,10.1834610019547));
#119882=CARTESIAN_POINT('Ctrl Pts',(-10.8487961126792,7.86576343241388,
10.1835196124461));
#119883=CARTESIAN_POINT('Ctrl Pts',(-10.8488243530778,7.86576621398921,
10.1835489715962));
#119884=CARTESIAN_POINT('Ctrl Pts',(-10.8488809426915,7.86577178792717,
10.1836078091335));
#119885=CARTESIAN_POINT('Ctrl Pts',(-10.8489092918882,7.86577458028827,
10.1836372875256));
#119886=CARTESIAN_POINT('Ctrl Pts',(-10.8489661105019,7.86578017692176,
10.1836963754788));
#119887=CARTESIAN_POINT('Ctrl Pts',(-10.8489945798982,7.86578298119242,
10.183725985045));
#119888=CARTESIAN_POINT('Ctrl Pts',(-10.8490397479066,7.86578743035258,
10.1837729669049));
#119889=CARTESIAN_POINT('Ctrl Pts',(-10.8490564475233,7.86578907531805,
10.1837903382098));
#119890=CARTESIAN_POINT('Ctrl Pts',(-10.8490903572128,7.86579241555501,
10.183825613974));
#119891=CARTESIAN_POINT('Ctrl Pts',(-10.849107567269,7.86579411082561,10.1838435184823));
#119892=CARTESIAN_POINT('Ctrl Pts',(-10.8491425293516,7.8657975547794,10.1838798936415));
#119893=CARTESIAN_POINT('Ctrl Pts',(-10.8491602813417,7.86579930345982,
10.1838983643271));
#119894=CARTESIAN_POINT('Ctrl Pts',(-10.8491963615264,7.86580285760799,
10.1839359076824));
#119895=CARTESIAN_POINT('Ctrl Pts',(-10.849214689642,7.86580466306887,10.1839549803498));
#119896=CARTESIAN_POINT('Ctrl Pts',(-10.8492519591937,7.86580833443686,
10.1839937665355));
#119897=CARTESIAN_POINT('Ctrl Pts',(-10.8492709006929,7.86581020035118,
10.1840134802072));
#119898=CARTESIAN_POINT('Ctrl Pts',(-10.8493094376427,7.86581399663158,
10.1840535909564));
#119899=CARTESIAN_POINT('Ctrl Pts',(-10.8493290329534,7.86581592698497,
10.1840739879852));
#119900=CARTESIAN_POINT('Ctrl Pts',(-10.8516303308932,7.86604263205601,
10.1864696134258));
#119901=CARTESIAN_POINT('Ctrl Pts',(-10.8539020576687,7.86626664103343,
10.1888543983169));
#119902=CARTESIAN_POINT('Ctrl Pts',(-10.8589442226075,7.86676431689917,
10.194192157552));
#119903=CARTESIAN_POINT('Ctrl Pts',(-10.8617094587736,7.86703759542811,
10.1971499103889));
#119904=CARTESIAN_POINT('Ctrl Pts',(-10.8694055213413,7.86779933403846,
10.2054673453715));
#119905=CARTESIAN_POINT('Ctrl Pts',(-10.8743020707884,7.86828533617108,
10.2108586974559));
#119906=CARTESIAN_POINT('Ctrl Pts',(-10.9060015500266,7.87144331735458,
10.2464187080988));
#119907=CARTESIAN_POINT('Ctrl Pts',(-10.931291838951,7.87401856052288,10.2779059452729));
#119908=CARTESIAN_POINT('Ctrl Pts',(-10.9938858617977,7.88073282871563,
10.3646117965544));
#119909=CARTESIAN_POINT('Ctrl Pts',(-11.028207472582,7.88479433127492,10.4217983430664));
#119910=CARTESIAN_POINT('Ctrl Pts',(-11.0815754835307,7.89236417456196,
10.5306625875245));
#119911=CARTESIAN_POINT('Ctrl Pts',(-11.1021879780395,7.89583102351319,
10.581354963265));
#119912=CARTESIAN_POINT('Ctrl Pts',(-11.1228324791063,7.90018195630549,
10.6443625149175));
#119913=CARTESIAN_POINT('Ctrl Pts',(-11.1262954385048,7.90095146918993,
10.6554867690128));
#119914=CARTESIAN_POINT('Ctrl Pts',(-11.1315248528597,7.90218030264611,
10.6732077527523));
#119915=CARTESIAN_POINT('Ctrl Pts',(-11.1334000043344,7.90263612055324,
10.6797718120297));
#119916=CARTESIAN_POINT('Ctrl Pts',(-11.1368281333451,7.90349912087854,
10.6921795739737));
#119917=CARTESIAN_POINT('Ctrl Pts',(-11.1383933864498,7.90390589466667,
10.6980196781309));
#119918=CARTESIAN_POINT('Ctrl Pts',(-11.1418304736136,7.90482886021816,
10.7112503604493));
#119919=CARTESIAN_POINT('Ctrl Pts',(-11.1436756371562,7.90534588293109,
10.7186475216715));
#119920=CARTESIAN_POINT('Ctrl Pts',(-11.1490616225113,7.90692329730635,
10.7411685626707));
#119921=CARTESIAN_POINT('Ctrl Pts',(-11.1523750681196,7.90799078949189,
10.7563445305724));
#119922=CARTESIAN_POINT('Ctrl Pts',(-11.1725964188434,7.91521917885966,
10.8586280082206));
#119923=CARTESIAN_POINT('Ctrl Pts',(-11.1799102402493,7.92168257978313,
10.9473257299318));
#119924=CARTESIAN_POINT('Ctrl Pts',(-11.175794448457,7.93156845030165,11.0819707610842));
#119925=CARTESIAN_POINT('Ctrl Pts',(-11.1716952369856,7.93494244709309,
11.1278379183047));
#119926=CARTESIAN_POINT('Ctrl Pts',(-11.1626773278418,7.93933120050644,
11.1884388919986));
#119927=CARTESIAN_POINT('Ctrl Pts',(-11.1601388780749,7.94041482633825,
11.2034836960619));
#119928=CARTESIAN_POINT('Ctrl Pts',(-11.1553213341638,7.94223835962507,
11.2290031787678));
#119929=CARTESIAN_POINT('Ctrl Pts',(-11.1531903144072,7.94298444720246,
11.2395035697684));
#119930=CARTESIAN_POINT('Ctrl Pts',(-11.1499330595366,7.9440425809472,11.2545004471464));
#119931=CARTESIAN_POINT('Ctrl Pts',(-11.1489231895529,7.94436058267268,
11.2590212835579));
#119932=CARTESIAN_POINT('Ctrl Pts',(-11.1471215490648,7.94491074744287,
11.266868704701));
#119933=CARTESIAN_POINT('Ctrl Pts',(-11.1463419256541,7.94514357528036,
11.2701979729418));
#119934=CARTESIAN_POINT('Ctrl Pts',(-11.1446529155874,7.9456369958904,11.2772717298883));
#119935=CARTESIAN_POINT('Ctrl Pts',(-11.1437396437225,7.94589736917181,
11.2810151914074));
#119936=CARTESIAN_POINT('Ctrl Pts',(-11.1411791956604,7.94661021463223,
11.2912910743716));
#119937=CARTESIAN_POINT('Ctrl Pts',(-11.1394942869817,7.94706062100967,
11.2978140725663));
#119938=CARTESIAN_POINT('Ctrl Pts',(-11.1306855033547,7.94932563932087,
11.3307469838067));
#119939=CARTESIAN_POINT('Ctrl Pts',(-11.1226984854427,7.95109649518949,
11.356919670276));
#119940=CARTESIAN_POINT('Ctrl Pts',(-11.088988099235,7.95770414334222,11.4550063202625));
#119941=CARTESIAN_POINT('Ctrl Pts',(-11.0572042482329,7.96234511825067,
11.5246394917393));
#119942=CARTESIAN_POINT('Ctrl Pts',(-10.9894155815658,7.97076334873772,
11.6415666200688));
#119943=CARTESIAN_POINT('Ctrl Pts',(-10.956168205878,7.97447955965923,11.6901390824437));
#119944=CARTESIAN_POINT('Ctrl Pts',(-10.9120423961465,7.97911120965069,
11.7452608574559));
#119945=CARTESIAN_POINT('Ctrl Pts',(-10.9045090285455,7.97989253965028,
11.7543861602398));
#119946=CARTESIAN_POINT('Ctrl Pts',(-10.8923893047023,7.98113588678859,
11.7686244415405));
#119947=CARTESIAN_POINT('Ctrl Pts',(-10.8878933912457,7.98159425532175,
11.7738136246553));
#119948=CARTESIAN_POINT('Ctrl Pts',(-10.8793570912542,7.98245940580886,
11.7834938795296));
#119949=CARTESIAN_POINT('Ctrl Pts',(-10.8753270072697,7.98286575539433,
11.7879937697824));
#119950=CARTESIAN_POINT('Ctrl Pts',(-10.8661734314228,7.98378414452859,
11.7980575506553));
#119951=CARTESIAN_POINT('Ctrl Pts',(-10.861030641176,7.98429698176375,11.8036034456134));
#119952=CARTESIAN_POINT('Ctrl Pts',(-10.8457184535277,7.98581500406247,
11.8198001031613));
#119953=CARTESIAN_POINT('Ctrl Pts',(-10.8354026282505,7.9868263783012,11.8303097774268));
#119954=CARTESIAN_POINT('Ctrl Pts',(-10.7570588287762,7.99442782051142,
11.9071875813504));
#119955=CARTESIAN_POINT('Ctrl Pts',(-10.6814289663745,8.00137237734009,
11.9652849681981));
#119956=CARTESIAN_POINT('Ctrl Pts',(-10.5869380224639,8.00942628103826,
12.0211843216839));
#119957=CARTESIAN_POINT('Ctrl Pts',(-10.5740721515525,8.01050982666157,
12.0284720878005));
#119958=CARTESIAN_POINT('Ctrl Pts',(-10.5332838187965,8.0138988385519,12.0505723848025));
#119959=CARTESIAN_POINT('Ctrl Pts',(-10.5048985611086,8.01619110933585,
12.0645053651755));
#119960=CARTESIAN_POINT('Ctrl Pts',(-10.4648944824683,8.01930312637977,
12.0821807643669));
#119961=CARTESIAN_POINT('Ctrl Pts',(-10.4537280034242,8.02015937130397,
12.0869098447716));
#119962=CARTESIAN_POINT('Ctrl Pts',(-10.4341519198524,8.02163664500308,
12.0948461643435));
#119963=CARTESIAN_POINT('Ctrl Pts',(-10.4257750404953,8.02226130975367,
12.0981309758894));
#119964=CARTESIAN_POINT('Ctrl Pts',(-10.4133222435431,8.02317805353899,
12.102850143896));
#119965=CARTESIAN_POINT('Ctrl Pts',(-10.4092749875865,8.02347416353389,
12.1043585028967));
#119966=CARTESIAN_POINT('Ctrl Pts',(-10.4023435132963,8.02397804595496,
12.1068984331792));
#119967=CARTESIAN_POINT('Ctrl Pts',(-10.3994634649549,8.02418645297861,
12.1079410566525));
#119968=CARTESIAN_POINT('Ctrl Pts',(-10.3928890943683,8.02465999380218,
12.1102921151401));
#119969=CARTESIAN_POINT('Ctrl Pts',(-10.3891922801295,8.02492470734324,
12.1115933571329));
#119970=CARTESIAN_POINT('Ctrl Pts',(-10.3790117631796,8.02564958545834,
12.1151197846091));
#119971=CARTESIAN_POINT('Ctrl Pts',(-10.3725148991876,8.02610761667849,
12.1173068987812));
#119972=CARTESIAN_POINT('Ctrl Pts',(-10.3370901556295,8.02858224372151,
12.1288889907905));
#119973=CARTESIAN_POINT('Ctrl Pts',(-10.3078230775826,8.03054439582064,
12.1372182869896));
#119974=CARTESIAN_POINT('Ctrl Pts',(-10.2155404363481,8.0365709023081,12.1596569268928));
#119975=CARTESIAN_POINT('Ctrl Pts',(-10.1516661756112,8.04051807760335,
12.1697265493539));
#119976=CARTESIAN_POINT('Ctrl Pts',(-10.0428857337908,8.04728759105127,
12.1778107236893));
#119977=CARTESIAN_POINT('Ctrl Pts',(-9.99833775981535,8.05007201709087,
12.1785898646929));
#119978=CARTESIAN_POINT('Ctrl Pts',(-9.92653781385786,8.05467328388258,
12.1757745271147));
#119979=CARTESIAN_POINT('Ctrl Pts',(-9.8992681945726,8.05644698399625,12.1737526790412));
#119980=CARTESIAN_POINT('Ctrl Pts',(-9.86269184696954,8.05887356706985,
12.1697568172149));
#119981=CARTESIAN_POINT('Ctrl Pts',(-9.85330147482896,8.05950076661409,
12.1686163076164));
#119982=CARTESIAN_POINT('Ctrl Pts',(-9.837625365665,8.06055532761854,12.1665204452778));
#119983=CARTESIAN_POINT('Ctrl Pts',(-9.83133168169488,8.06098075053173,
12.1656270702256));
#119984=CARTESIAN_POINT('Ctrl Pts',(-9.81896063454365,8.06182112571567,
12.1637687371126));
#119985=CARTESIAN_POINT('Ctrl Pts',(-9.81288298623624,8.0622359643735,12.1628070115097));
#119986=CARTESIAN_POINT('Ctrl Pts',(-9.79818915049442,8.06324384590903,
12.1603636822542));
#119987=CARTESIAN_POINT('Ctrl Pts',(-9.78958149270925,8.06383838383765,
12.158833697613));
#119988=CARTESIAN_POINT('Ctrl Pts',(-9.76084233285919,8.06583766239594,
12.1533946498985));
#119989=CARTESIAN_POINT('Ctrl Pts',(-9.74079700728855,8.06725569344303,
12.149055841049));
#119990=CARTESIAN_POINT('Ctrl Pts',(-9.60964016392473,8.07669521747471,
12.1170604569864));
#119991=CARTESIAN_POINT('Ctrl Pts',(-9.50296639463868,8.08522691343523,
12.0738495023957));
#119992=CARTESIAN_POINT('Ctrl Pts',(-9.37510248382612,8.09596763905219,
11.9988686969892));
#119993=CARTESIAN_POINT('Ctrl Pts',(-9.34671561818705,8.09838262646952,
11.9805384020923));
#119994=CARTESIAN_POINT('Ctrl Pts',(-9.31355757967787,8.10120780484132,
11.9570469665376));
#119995=CARTESIAN_POINT('Ctrl Pts',(-9.30799633036576,8.10168177816619,
11.9530335877622));
#119996=CARTESIAN_POINT('Ctrl Pts',(-9.29934438527864,8.10241898268218,
11.946674084668));
#119997=CARTESIAN_POINT('Ctrl Pts',(-9.29622979375232,8.10268432947371,
11.9443609537213));
#119998=CARTESIAN_POINT('Ctrl Pts',(-9.29039683624144,8.10318110837887,
11.9399840743584));
#119999=CARTESIAN_POINT('Ctrl Pts',(-9.28767601930278,8.10341275734486,
11.9379239078558));
#120000=CARTESIAN_POINT('Ctrl Pts',(-9.2813849967981,8.10394825775878,11.9331172636118));
#120001=CARTESIAN_POINT('Ctrl Pts',(-9.27782154431709,8.10425150573368,
11.9303620963278));
#120002=CARTESIAN_POINT('Ctrl Pts',(-9.26619265962072,8.10524118627714,
11.9212638774465));
#120003=CARTESIAN_POINT('Ctrl Pts',(-9.2581940390486,8.10592202104284,11.9148356565452));
#120004=CARTESIAN_POINT('Ctrl Pts',(-9.19463388644543,8.11134248580574,
11.8623726725172));
#120005=CARTESIAN_POINT('Ctrl Pts',(-9.14331820871305,8.11578876267777,
11.8114187535035));
#120006=CARTESIAN_POINT('Ctrl Pts',(-9.0606804886135,8.12375148871338,11.7127215354358));
#120007=CARTESIAN_POINT('Ctrl Pts',(-9.02754788556678,8.12724995818143,
11.6668053763915));
#120008=CARTESIAN_POINT('Ctrl Pts',(-8.98671766308592,8.13220105524531,
11.6006683962578));
#120009=CARTESIAN_POINT('Ctrl Pts',(-8.97608063183501,8.13356319436307,
11.5823509806885));
#120010=CARTESIAN_POINT('Ctrl Pts',(-8.9582878503849,8.13598269385288,11.5497150732665));
#120011=CARTESIAN_POINT('Ctrl Pts',(-8.95091919347303,8.13703276207659,
11.5355187075051));
#120012=CARTESIAN_POINT('Ctrl Pts',(-8.94042951608006,8.13860392694681,
11.5142615338318));
#120013=CARTESIAN_POINT('Ctrl Pts',(-8.93708493779483,8.13911734779618,
11.5073126268758));
#120014=CARTESIAN_POINT('Ctrl Pts',(-8.93123653715304,8.14003808013725,
11.4948498646277));
#120015=CARTESIAN_POINT('Ctrl Pts',(-8.9287065197077,8.14044448177939,11.4893485514305));
#120016=CARTESIAN_POINT('Ctrl Pts',(-8.92343659845646,8.14130855580429,
11.4776527830768));
#120017=CARTESIAN_POINT('Ctrl Pts',(-8.92070749408236,8.14176657569642,
11.4714537327116));
#120018=CARTESIAN_POINT('Ctrl Pts',(-8.91352761370793,8.14300060126082,
11.4547558118809));
#120019=CARTESIAN_POINT('Ctrl Pts',(-8.90917569008422,8.14377987462503,
11.4442154923792));
#120020=CARTESIAN_POINT('Ctrl Pts',(-8.88882767518465,8.14758164296313,
11.3928298504512));
#120021=CARTESIAN_POINT('Ctrl Pts',(-8.87497077232577,8.15067314706299,
11.3511803378975));
#120022=CARTESIAN_POINT('Ctrl Pts',(-8.84416390001624,8.1591104171017,11.2378182849524));
#120023=CARTESIAN_POINT('Ctrl Pts',(-8.83156246872543,8.16455341843918,
11.165126740619));
#120024=CARTESIAN_POINT('Ctrl Pts',(-8.82345615444482,8.17214976019482,
11.0613782627539));
#120025=CARTESIAN_POINT('Ctrl Pts',(-8.82226223582677,8.17435631706544,
11.0309307902424));
#120026=CARTESIAN_POINT('Ctrl Pts',(-8.82224537383291,8.1773643130939,10.9886290527823));
#120027=CARTESIAN_POINT('Ctrl Pts',(-8.82241920929865,8.17819994535925,
10.9767887340886));
#120028=CARTESIAN_POINT('Ctrl Pts',(-8.82303447211169,8.17964529177416,
10.9561223164122));
#120029=CARTESIAN_POINT('Ctrl Pts',(-8.82339671242154,8.18025844228852,
10.9472949697062));
#120030=CARTESIAN_POINT('Ctrl Pts',(-8.82408224553932,8.1811616277269,10.9341905797099));
#120031=CARTESIAN_POINT('Ctrl Pts',(-8.82432961477614,8.18145552867865,
10.9299101161612));
#120032=CARTESIAN_POINT('Ctrl Pts',(-8.82479355294454,8.18195696254556,
10.922577586925));
#120033=CARTESIAN_POINT('Ctrl Pts',(-8.82499864502802,8.18216511252289,
10.9195249118278));
#120034=CARTESIAN_POINT('Ctrl Pts',(-8.8254951551086,8.18263987316357,10.9125416370593));
#120035=CARTESIAN_POINT('Ctrl Pts',(-8.82579440880514,8.18290604988816,
10.9086116710676));
#120036=CARTESIAN_POINT('Ctrl Pts',(-8.82667608214286,8.18363889590926,
10.8977533058052));
#120037=CARTESIAN_POINT('Ctrl Pts',(-8.82730014435008,8.18410335460577,
10.8908283141135));
#120038=CARTESIAN_POINT('Ctrl Pts',(-8.83114773140942,8.18669426191336,
10.8519843922683));
#120039=CARTESIAN_POINT('Ctrl Pts',(-8.83561335391948,8.18876001582665,
10.8201990241753));
#120040=CARTESIAN_POINT('Ctrl Pts',(-8.85274244974931,8.1948043352428,10.7263043808015));
#120041=CARTESIAN_POINT('Ctrl Pts',(-8.86912434214634,8.19867925876159,
10.6649921353747));
#120042=CARTESIAN_POINT('Ctrl Pts',(-8.90513726525193,8.20534962224792,
10.5637490293547));
#120043=CARTESIAN_POINT('Ctrl Pts',(-8.92223496403341,8.20810841112716,
10.5230708675062));
#120044=CARTESIAN_POINT('Ctrl Pts',(-8.94956905684076,8.2121001162128,10.467062509783));
#120045=CARTESIAN_POINT('Ctrl Pts',(-8.95794537512169,8.21327828838946,
10.450864642633));
#120046=CARTESIAN_POINT('Ctrl Pts',(-8.97352961147138,8.21539881153388,
10.422369892323));
#120047=CARTESIAN_POINT('Ctrl Pts',(-8.98059117399518,8.2163362000087,10.40999693485));
#120048=CARTESIAN_POINT('Ctrl Pts',(-8.99164390837769,8.2177705731562,10.3914218424864));
#120049=CARTESIAN_POINT('Ctrl Pts',(-8.99547193252056,8.21826173827777,
10.3851238020341));
#120050=CARTESIAN_POINT('Ctrl Pts',(-9.00253763565448,8.21915849055703,
10.3737410874142));
#120051=CARTESIAN_POINT('Ctrl Pts',(-9.00575574302143,8.21956335708555,
10.3686445145265));
#120052=CARTESIAN_POINT('Ctrl Pts',(-9.01279993431246,8.22044209064721,
10.3576759305739));
#120053=CARTESIAN_POINT('Ctrl Pts',(-9.01663957739453,8.22091644523291,
10.3518129471792));
#120054=CARTESIAN_POINT('Ctrl Pts',(-9.02728669257737,8.22221953176108,
10.3358675764086));
#120055=CARTESIAN_POINT('Ctrl Pts',(-9.03419825434873,8.22305210110015,
10.3258560811101));
#120056=CARTESIAN_POINT('Ctrl Pts',(-9.08393578203363,8.22895380345555,
10.256145609038));
#120057=CARTESIAN_POINT('Ctrl Pts',(-9.13210306648402,8.2342298310506,10.2004724156419));
#120058=CARTESIAN_POINT('Ctrl Pts',(-9.22556636435933,8.24369673948814,
10.110908375121));
#120059=CARTESIAN_POINT('Ctrl Pts',(-9.26871324064937,8.24783168250748,
10.075093935594));
#120060=CARTESIAN_POINT('Ctrl Pts',(-9.33178694130332,8.25344520761053,
10.0299216914241));
#120061=CARTESIAN_POINT('Ctrl Pts',(-9.34967189654596,8.25499261424565,
10.0178421279196));
#120062=CARTESIAN_POINT('Ctrl Pts',(-9.37954098227575,8.25749390594417,
9.99884233009303));
#120063=CARTESIAN_POINT('Ctrl Pts',(-9.39133261651085,8.25846095817066,
9.99162996360394));
#120064=CARTESIAN_POINT('Ctrl Pts',(-9.40766194614922,8.25976972872334,
9.98203296126532));
#120065=CARTESIAN_POINT('Ctrl Pts',(-9.41209175878697,8.26012175735873,
9.97946819533971));
#120066=CARTESIAN_POINT('Ctrl Pts',(-9.41958071637951,8.26071165414091,
9.97519719702706));
#120067=CARTESIAN_POINT('Ctrl Pts',(-9.42263097379942,8.26095046870445,
9.97347560255144));
#120068=CARTESIAN_POINT('Ctrl Pts',(-9.42888391418015,8.2614370062654,9.96998307228857));
#120069=CARTESIAN_POINT('Ctrl Pts',(-9.4320872381885,8.26168465083042,9.96821341802256));
#120070=CARTESIAN_POINT('Ctrl Pts',(-9.44043821854453,8.26232623107853,
9.96365065068852));
#120071=CARTESIAN_POINT('Ctrl Pts',(-9.44559862890257,8.26271873820317,
9.96088090945525));
#120072=CARTESIAN_POINT('Ctrl Pts',(-9.46677776166664,8.26431445062595,
9.94971614665113));
#120073=CARTESIAN_POINT('Ctrl Pts',(-9.48296909531626,8.26549906267782,
9.94165163708398));
#120074=CARTESIAN_POINT('Ctrl Pts',(-9.59831133306932,8.27373696194174,
9.88748171545327));
#120075=CARTESIAN_POINT('Ctrl Pts',(-9.70325428047283,8.28024757132826,
9.85501720676948));
#120076=CARTESIAN_POINT('Ctrl Pts',(-9.81114931547642,8.2871573923531,9.83748957791555));
#120077=CARTESIAN_POINT('Origin',(-10.,2.67563288526385,11.));
#120078=CARTESIAN_POINT('',(-9.81114930149917,8.88548556788545,9.83748958018616));
#120079=CARTESIAN_POINT('',(-9.81114930165995,8.78721751211607,9.83748958016004));
#120080=CARTESIAN_POINT('',(-9.81114930150157,2.67563288526385,9.83748958018577));
#120081=CARTESIAN_POINT('Ctrl Pts',(-9.81114930149677,8.88548556788545,
9.83748958018655));
#120082=CARTESIAN_POINT('Ctrl Pts',(-9.80762618945418,8.88523897046284,
9.83806191240723));
#120083=CARTESIAN_POINT('Ctrl Pts',(-9.80410562708024,8.88499317710299,
9.83865026884476));
#120084=CARTESIAN_POINT('Ctrl Pts',(-9.79682735519712,8.88448640325961,
9.8399006522627));
#120085=CARTESIAN_POINT('Ctrl Pts',(-9.79307007993808,8.88422554748418,
9.84056495246939));
#120086=CARTESIAN_POINT('Ctrl Pts',(-9.78593979417461,8.88373203747368,
9.84186137850437));
#120087=CARTESIAN_POINT('Ctrl Pts',(-9.78256633190168,8.88349920911067,
9.84248998337233));
#120088=CARTESIAN_POINT('Ctrl Pts',(-9.77456755615892,8.88294864188807,
9.84401666348539));
#120089=CARTESIAN_POINT('Ctrl Pts',(-9.76994481043406,8.8826316294304,9.84492776300372));
#120090=CARTESIAN_POINT('Ctrl Pts',(-9.75437541698459,8.88156752609765,
9.84809352145577));
#120091=CARTESIAN_POINT('Ctrl Pts',(-9.74345503743677,8.88082716630944,
9.85047632665062));
#120092=CARTESIAN_POINT('Ctrl Pts',(-9.71685097011188,8.87903453536867,
9.85667930940597));
#120093=CARTESIAN_POINT('Ctrl Pts',(-9.70120837818108,8.87798993734095,
9.86066721525621));
#120094=CARTESIAN_POINT('Ctrl Pts',(-9.6366799752234,8.87370147252014,9.87853853038114));
#120095=CARTESIAN_POINT('Ctrl Pts',(-9.58863338160591,8.87055638592843,
9.89525770444862));
#120096=CARTESIAN_POINT('Ctrl Pts',(-9.46649734425989,8.86235401681429,
9.94683607807214));
#120097=CARTESIAN_POINT('Ctrl Pts',(-9.39470610429211,8.85730647402275,
9.98639422558819));
#120098=CARTESIAN_POINT('Ctrl Pts',(-9.3145279572129,8.85094889821845,10.0421501260401));
#120099=CARTESIAN_POINT('Ctrl Pts',(-9.30164894425003,8.84990399896559,
10.0514990425551));
#120100=CARTESIAN_POINT('Ctrl Pts',(-9.28282703896273,8.84833900102623,
10.0657531029731));
#120101=CARTESIAN_POINT('Ctrl Pts',(-9.27673613712501,8.84782648683882,
10.070460490023));
#120102=CARTESIAN_POINT('Ctrl Pts',(-9.2659373844172,8.84690665673508,10.0789767623831));
#120103=CARTESIAN_POINT('Ctrl Pts',(-9.26121189594785,8.84650024225482,
10.0827629189775));
#120104=CARTESIAN_POINT('Ctrl Pts',(-9.25125403116214,8.84563537182702,
10.0908682342918));
#120105=CARTESIAN_POINT('Ctrl Pts',(-9.24602937887567,8.8451765623171,10.0951964896018));
#120106=CARTESIAN_POINT('Ctrl Pts',(-9.23208833818846,8.84393850204532,
10.1069502521495));
#120107=CARTESIAN_POINT('Ctrl Pts',(-9.2234425482013,8.84315594775777,10.114457973612));
#120108=CARTESIAN_POINT('Ctrl Pts',(-9.17708710588677,8.83887774955211,
10.1559124593417));
#120109=CARTESIAN_POINT('Ctrl Pts',(-9.14149672498564,8.83528770379986,
10.1921384604032));
#120110=CARTESIAN_POINT('Ctrl Pts',(-9.07652347718975,8.82810798254828,
10.2674290495427));
#120111=CARTESIAN_POINT('Ctrl Pts',(-9.04701199219257,8.82453104238795,
10.3062547558313));
#120112=CARTESIAN_POINT('Ctrl Pts',(-9.00697055141908,8.81923397101657,
10.3663291542726));
#120113=CARTESIAN_POINT('Ctrl Pts',(-8.99453650521917,8.8175136341516,10.3862496984175));
#120114=CARTESIAN_POINT('Ctrl Pts',(-8.96300826788446,8.812960324146,10.4402935940919));
#120115=CARTESIAN_POINT('Ctrl Pts',(-8.94500158508196,8.81015037346468,
10.475021797466));
#120116=CARTESIAN_POINT('Ctrl Pts',(-8.92572209310191,8.80691976101814,
10.5172212952883));
#120117=CARTESIAN_POINT('Ctrl Pts',(-8.92275173505512,8.80641482889997,
10.5238860626499));
#120118=CARTESIAN_POINT('Ctrl Pts',(-8.91824150702682,8.80563721013027,
10.5342642611305));
#120119=CARTESIAN_POINT('Ctrl Pts',(-8.9166584466116,8.80536208860369,10.5379585565227));
#120120=CARTESIAN_POINT('Ctrl Pts',(-8.91377438506867,8.80485688769931,
10.5447852382603));
#120121=CARTESIAN_POINT('Ctrl Pts',(-8.91246799714347,8.80462650396821,
10.5479151527524));
#120122=CARTESIAN_POINT('Ctrl Pts',(-8.90950943639207,8.8041011485641,10.5550904736861));
#120123=CARTESIAN_POINT('Ctrl Pts',(-8.90786623904451,8.80380670789217,
10.5591394714559));
#120124=CARTESIAN_POINT('Ctrl Pts',(-8.90281201491224,8.80289237355746,
10.5717952627027));
#120125=CARTESIAN_POINT('Ctrl Pts',(-8.899479811319,8.80227689470087,10.5804334390886));
#120126=CARTESIAN_POINT('Ctrl Pts',(-8.891859307521,8.80083651155446,10.6009039794139));
#120127=CARTESIAN_POINT('Ctrl Pts',(-8.88765803980652,8.80001589118787,
10.6127677455485));
#120128=CARTESIAN_POINT('Ctrl Pts',(-8.87297189302721,8.79703793250479,
10.656452232396));
#120129=CARTESIAN_POINT('Ctrl Pts',(-8.86365523343844,8.79492684340516,
10.6886508131516));
#120130=CARTESIAN_POINT('Ctrl Pts',(-8.83777034136093,8.78810517825263,
10.7948918325602));
#120131=CARTESIAN_POINT('Ctrl Pts',(-8.82697693399025,8.78348579031354,
10.8701385813785));
#120132=CARTESIAN_POINT('Ctrl Pts',(-8.82174874082086,8.77628818621676,
10.9838370535318));
#120133=CARTESIAN_POINT('Ctrl Pts',(-8.82184034095802,8.77384923116895,
11.0218321325642));
#120134=CARTESIAN_POINT('Ctrl Pts',(-8.82432447517397,8.77063170494138,
11.0707314943622));
#120135=CARTESIAN_POINT('Ctrl Pts',(-8.82503579236523,8.76990491460333,
11.0817005594148));
#120136=CARTESIAN_POINT('Ctrl Pts',(-8.82642647241378,8.76872847727069,
11.0993223604917));
#120137=CARTESIAN_POINT('Ctrl Pts',(-8.82700915674939,8.76828182575976,
11.1059822366553));
#120138=CARTESIAN_POINT('Ctrl Pts',(-8.82822964434318,8.76742582096936,
11.1186853853923));
#120139=CARTESIAN_POINT('Ctrl Pts',(-8.82885758339626,8.76701678683107,
11.1247294061596));
#120140=CARTESIAN_POINT('Ctrl Pts',(-8.83040718127812,8.76607395790491,
11.1385994014598));
#120141=CARTESIAN_POINT('Ctrl Pts',(-8.83136065948155,8.76553919141288,
11.1464214542385));
#120142=CARTESIAN_POINT('Ctrl Pts',(-8.8346042786644,8.76385049423788,11.1709769600508));
#120143=CARTESIAN_POINT('Ctrl Pts',(-8.83717582174272,8.7626879180939,11.1876704224937));
#120144=CARTESIAN_POINT('Ctrl Pts',(-8.84405037082682,8.7599341711747,11.2266996496627));
#120145=CARTESIAN_POINT('Ctrl Pts',(-8.84864311485029,8.75833466022537,
11.2489768713147));
#120146=CARTESIAN_POINT('Ctrl Pts',(-8.88020464939812,8.748586905063,11.3824058085627));
#120147=CARTESIAN_POINT('Ctrl Pts',(-8.92259681838964,8.73999294651563,
11.4892569028555));
#120148=CARTESIAN_POINT('Ctrl Pts',(-8.98906906594513,8.73050859717051,
11.6045364872519));
#120149=CARTESIAN_POINT('Ctrl Pts',(-8.99880926448154,8.72918917997709,
11.6205343863147));
#120150=CARTESIAN_POINT('Ctrl Pts',(-9.01213303747131,8.72747980964123,
11.6412870894377));
#120151=CARTESIAN_POINT('Ctrl Pts',(-9.01537635479602,8.72707071770304,
11.6462557912634));
#120152=CARTESIAN_POINT('Ctrl Pts',(-9.02069032290076,8.72641193486082,
11.6542638154006));
#120153=CARTESIAN_POINT('Ctrl Pts',(-9.02273785125503,8.72616079166128,
11.6573182466448));
#120154=CARTESIAN_POINT('Ctrl Pts',(-9.02675831227461,8.72567294687066,
11.6632555179733));
#120155=CARTESIAN_POINT('Ctrl Pts',(-9.0287298078646,8.72543616373811,11.6661392340347));
#120156=CARTESIAN_POINT('Ctrl Pts',(-9.03359227741294,8.72485799696642,
11.673184111837));
#120157=CARTESIAN_POINT('Ctrl Pts',(-9.03649737429108,8.72451754216638,
11.6773355352298));
#120158=CARTESIAN_POINT('Ctrl Pts',(-9.04721404379473,8.72327912575544,
11.692441331472));
#120159=CARTESIAN_POINT('Ctrl Pts',(-9.05518671524618,8.72239123851219,
11.7032808617595));
#120160=CARTESIAN_POINT('Ctrl Pts',(-9.07594258435097,8.72015612409244,
11.7305100008294));
#120161=CARTESIAN_POINT('Ctrl Pts',(-9.08897740306139,8.7188224352027,11.7467026840705));
#120162=CARTESIAN_POINT('Ctrl Pts',(-9.15827921012805,8.71203116242853,
11.8282756757284));
#120163=CARTESIAN_POINT('Ctrl Pts',(-9.22117731224348,8.70681900766609,
11.8876775071258));
#120164=CARTESIAN_POINT('Ctrl Pts',(-9.32655844285437,8.69852451393199,
11.9673007939717));
#120165=CARTESIAN_POINT('Ctrl Pts',(-9.36469164148997,8.6956006205728,11.9927622677969));
#120166=CARTESIAN_POINT('Ctrl Pts',(-9.41420744655112,8.69183332300374,
12.0218006305955));
#120167=CARTESIAN_POINT('Ctrl Pts',(-9.4242928046753,8.69106758265894,12.0275167414853));
#120168=CARTESIAN_POINT('Ctrl Pts',(-9.44043874495223,8.68984330320877,
12.0363554951789));
#120169=CARTESIAN_POINT('Ctrl Pts',(-9.44644506549921,8.68938822008444,
12.0395760875181));
#120170=CARTESIAN_POINT('Ctrl Pts',(-9.45729964499056,8.68856625835707,
12.0452755780688));
#120171=CARTESIAN_POINT('Ctrl Pts',(-9.46213781995304,8.68820005132003,
12.0477733452447));
#120172=CARTESIAN_POINT('Ctrl Pts',(-9.47354942318082,8.68733657947066,
12.0535648580537));
#120173=CARTESIAN_POINT('Ctrl Pts',(-9.48013665672341,8.68683836903946,
12.0568307433259));
#120174=CARTESIAN_POINT('Ctrl Pts',(-9.49949103045295,8.68537493784931,
12.0662017166269));
#120175=CARTESIAN_POINT('Ctrl Pts',(-9.51233776357368,8.68440404454503,
12.0721384435285));
#120176=CARTESIAN_POINT('Ctrl Pts',(-9.57046822454081,8.68001114498712,
12.0977407429037));
#120177=CARTESIAN_POINT('Ctrl Pts',(-9.61684906642373,8.67650404095868,
12.1147764395732));
#120178=CARTESIAN_POINT('Ctrl Pts',(-9.72894838356349,8.66804129298503,
12.1481270129227));
#120179=CARTESIAN_POINT('Ctrl Pts',(-9.79527847381412,8.6630401608305,12.1617887016182));
#120180=CARTESIAN_POINT('Ctrl Pts',(-9.90241328413659,8.65518380094803,
12.1743910778903));
#120181=CARTESIAN_POINT('Ctrl Pts',(-9.9426374825873,8.65228537603638,12.1770419773361));
#120182=CARTESIAN_POINT('Ctrl Pts',(-9.99026985957277,8.64896774822762,
12.1777327303041));
#120183=CARTESIAN_POINT('Ctrl Pts',(-9.99761843418222,8.64845916123766,
12.1777705186655));
#120184=CARTESIAN_POINT('Ctrl Pts',(-10.0089977252712,8.6476771206294,12.17772252657));
#120185=CARTESIAN_POINT('Ctrl Pts',(-10.0130283029126,8.64740118977913,
12.1776848361052));
#120186=CARTESIAN_POINT('Ctrl Pts',(-10.0204488864569,8.64689524780991,
12.177577344142));
#120187=CARTESIAN_POINT('Ctrl Pts',(-10.0238388007892,8.64666492521807,
12.1775135967354));
#120188=CARTESIAN_POINT('Ctrl Pts',(-10.0315816341863,8.64614065210239,
12.1773345414614));
#120189=CARTESIAN_POINT('Ctrl Pts',(-10.0359342316413,8.64584722378039,
12.177209732648));
#120190=CARTESIAN_POINT('Ctrl Pts',(-10.0494579645718,8.64493925685946,
12.1767468688972));
#120191=CARTESIAN_POINT('Ctrl Pts',(-10.0586261714613,8.64432904564143,
12.1763257493064));
#120192=CARTESIAN_POINT('Ctrl Pts',(-10.0802096149529,8.64290310138475,
12.1750813878483));
#120193=CARTESIAN_POINT('Ctrl Pts',(-10.0926187771136,8.64209153644679,
12.1741684883418));
#120194=CARTESIAN_POINT('Ctrl Pts',(-10.137783748469,8.63916034304198,12.1701253426909));
#120195=CARTESIAN_POINT('Ctrl Pts',(-10.1704209283632,8.63708543544754,
12.1658193236148));
#120196=CARTESIAN_POINT('Ctrl Pts',(-10.2784334676807,8.63024111258215,
12.1469347736578));
#120197=CARTESIAN_POINT('Ctrl Pts',(-10.352555209962,8.62556937034821,12.126361132316));
#120198=CARTESIAN_POINT('Ctrl Pts',(-10.4595501234848,8.61831641778901,
12.0850570290388));
#120199=CARTESIAN_POINT('Ctrl Pts',(-10.4942669592658,8.61587926387358,
12.0696891135994));
#120200=CARTESIAN_POINT('Ctrl Pts',(-10.5380014700812,8.61266378793713,
12.0477453157516));
#120201=CARTESIAN_POINT('Ctrl Pts',(-10.5477540234054,8.61193716141169,
12.0426798861601));
#120202=CARTESIAN_POINT('Ctrl Pts',(-10.5633226105629,8.61076092523297,
12.0343149351427));
#120203=CARTESIAN_POINT('Ctrl Pts',(-10.5691840681087,8.61031430918389,
12.03110098542));
#120204=CARTESIAN_POINT('Ctrl Pts',(-10.5803209617273,8.60945832992848,
12.0248705138584));
#120205=CARTESIAN_POINT('Ctrl Pts',(-10.5856010477627,8.60904928550928,
12.0218627105844));
#120206=CARTESIAN_POINT('Ctrl Pts',(-10.5976750166228,8.60810637154452,
12.0148604570776));
#120207=CARTESIAN_POINT('Ctrl Pts',(-10.604452491126,8.60757152969146,12.0108384408905));
#120208=CARTESIAN_POINT('Ctrl Pts',(-10.6256310474118,8.60588234745142,
11.9979811127385));
#120209=CARTESIAN_POINT('Ctrl Pts',(-10.6398821237549,8.60471935452055,
11.9889041032157));
#120210=CARTESIAN_POINT('Ctrl Pts',(-10.6728557531962,8.60196443770187,
11.9668908366225));
#120211=CARTESIAN_POINT('Ctrl Pts',(-10.691407878162,8.60036416394799,11.9537126315116));
#120212=CARTESIAN_POINT('Ctrl Pts',(-10.8009885285493,8.59060311523743,
11.8709954349345));
#120213=CARTESIAN_POINT('Ctrl Pts',(-10.8818388132592,8.58199514799618,
11.789031095193));
#120214=CARTESIAN_POINT('Ctrl Pts',(-10.9605674758953,8.57251176203849,
11.681725758351));
#120215=CARTESIAN_POINT('Ctrl Pts',(-10.9711973409604,8.57120360980147,
11.6664950890417));
#120216=CARTESIAN_POINT('Ctrl Pts',(-10.9847328751874,8.56950645637308,
11.646089169498));
#120217=CARTESIAN_POINT('Ctrl Pts',(-10.9879654151524,8.56909864423396,
11.6411352373319));
#120218=CARTESIAN_POINT('Ctrl Pts',(-10.9931445942054,8.56844141194949,
11.6330658490535));
#120219=CARTESIAN_POINT('Ctrl Pts',(-10.9951141729077,8.56819055162865,
11.6299653467071));
#120220=CARTESIAN_POINT('Ctrl Pts',(-10.9989297929028,8.56770282830961,
11.623896266055));
#120221=CARTESIAN_POINT('Ctrl Pts',(-11.0007771649701,8.56746588680947,
11.6209286178238));
#120222=CARTESIAN_POINT('Ctrl Pts',(-11.0052764737229,8.56688671483245,
11.613628613383));
#120223=CARTESIAN_POINT('Ctrl Pts',(-11.0079136891927,8.56654542079496,
11.6092871747092));
#120224=CARTESIAN_POINT('Ctrl Pts',(-11.0174783722114,8.56530034899717,
11.5933095396261));
#120225=CARTESIAN_POINT('Ctrl Pts',(-11.0242334006939,8.56440678741006,
11.5815706552271));
#120226=CARTESIAN_POINT('Ctrl Pts',(-11.0409292537588,8.5621540379627,11.5513629846424));
#120227=CARTESIAN_POINT('Ctrl Pts',(-11.0505822854791,8.56080866063369,
11.532739915685));
#120228=CARTESIAN_POINT('Ctrl Pts',(-11.0982776164641,8.55387523702402,
11.4343793643923));
#120229=CARTESIAN_POINT('Ctrl Pts',(-11.127757629865,8.54854249131078,11.3508041819735));
#120230=CARTESIAN_POINT('Ctrl Pts',(-11.1574643180958,8.54022787614708,
11.2220168769436));
#120231=CARTESIAN_POINT('Ctrl Pts',(-11.1649216446406,8.53742669604648,
11.1788073089057));
#120232=CARTESIAN_POINT('Ctrl Pts',(-11.1712617350419,8.53380270245219,
11.1239781735694));
#120233=CARTESIAN_POINT('Ctrl Pts',(-11.1724052552642,8.53305052383987,
11.112652306458));
#120234=CARTESIAN_POINT('Ctrl Pts',(-11.1739667728239,8.53184290347931,
11.0945669750115));
#120235=CARTESIAN_POINT('Ctrl Pts',(-11.1744909661526,8.53139075428198,
11.087817217321));
#120236=CARTESIAN_POINT('Ctrl Pts',(-11.1753738848613,8.53053058979536,
11.0750199371686));
#120237=CARTESIAN_POINT('Ctrl Pts',(-11.1757442009273,8.53012294739156,
11.068973413887));
#120238=CARTESIAN_POINT('Ctrl Pts',(-11.1764804572852,8.529192311222,11.0552126556707));
#120239=CARTESIAN_POINT('Ctrl Pts',(-11.1768171966594,8.52866843266695,
11.0474972046805));
#120240=CARTESIAN_POINT('Ctrl Pts',(-11.177619943559,8.52704886336656,11.0237436656819));
#120241=CARTESIAN_POINT('Ctrl Pts',(-11.1778340999152,8.52594550625948,
11.0076994992964));
#120242=CARTESIAN_POINT('Ctrl Pts',(-11.1775697980001,8.52335668895611,
10.9703916001467));
#120243=CARTESIAN_POINT('Ctrl Pts',(-11.176843243716,8.52186419163528,10.9491357725765));
#120244=CARTESIAN_POINT('Ctrl Pts',(-11.1720557862627,8.51631768209624,
10.8710661396924));
#120245=CARTESIAN_POINT('Ctrl Pts',(-11.1644513808421,8.51217138745534,
10.8145534424038));
#120246=CARTESIAN_POINT('Ctrl Pts',(-11.1381470439426,8.50275118543912,
10.6888250374552));
#120247=CARTESIAN_POINT('Ctrl Pts',(-11.117158036718,8.49747639814742,10.6203050939678));
#120248=CARTESIAN_POINT('Ctrl Pts',(-11.0861741516057,8.4917350538909,10.544558198444));
#120249=CARTESIAN_POINT('Ctrl Pts',(-11.0821423242241,8.49101699148367,
10.5350596485392));
#120250=CARTESIAN_POINT('Ctrl Pts',(-11.0761674354496,8.4899945522122,10.5214823949139));
#120251=CARTESIAN_POINT('Ctrl Pts',(-11.0743250657323,8.48968466578908,
10.5173602768911));
#120252=CARTESIAN_POINT('Ctrl Pts',(-11.071047614508,8.48914286379021,10.5101390684957));
#120253=CARTESIAN_POINT('Ctrl Pts',(-11.0696226927823,8.48891035524681,
10.5070354768976));
#120254=CARTESIAN_POINT('Ctrl Pts',(-11.0665520009576,8.48841578335709,
10.5004232698065));
#120255=CARTESIAN_POINT('Ctrl Pts',(-11.0649023977335,8.4881539535437,10.4969165432231));
#120256=CARTESIAN_POINT('Ctrl Pts',(-11.0602954675072,8.48743310686054,
10.487247326179));
#120257=CARTESIAN_POINT('Ctrl Pts',(-11.0573016999778,8.48697623251502,
10.4811022223591));
#120258=CARTESIAN_POINT('Ctrl Pts',(-11.0394045054744,8.48430962612694,
10.4451639370382));
#120259=CARTESIAN_POINT('Ctrl Pts',(-11.0232944593596,8.48216602103481,
10.4159848585458));
#120260=CARTESIAN_POINT('Ctrl Pts',(-10.9496225140483,8.4732028618118,10.2949813702684));
#120261=CARTESIAN_POINT('Ctrl Pts',(-10.8807787398329,8.46671843083733,
10.2106553488865));
#120262=CARTESIAN_POINT('Ctrl Pts',(-10.782753825613,8.45813689749599,10.119638085903));
#120263=CARTESIAN_POINT('Ctrl Pts',(-10.7635807229568,8.45648651170935,
10.1029576474153));
#120264=CARTESIAN_POINT('Ctrl Pts',(-10.7365295478375,8.45418551701674,
10.0809193280543));
#120265=CARTESIAN_POINT('Ctrl Pts',(-10.7291028809892,8.45355654443744,
10.0750167370988));
#120266=CARTESIAN_POINT('Ctrl Pts',(-10.7170792567233,8.45254215513233,
10.0656953345988));
#120267=CARTESIAN_POINT('Ctrl Pts',(-10.7125271476411,8.45215899055984,
10.0622191460015));
#120268=CARTESIAN_POINT('Ctrl Pts',(-10.7030460162611,8.45136263796221,
10.0550878267754));
#120269=CARTESIAN_POINT('Ctrl Pts',(-10.6981134313284,8.45094927144305,
10.051437745511));
#120270=CARTESIAN_POINT('Ctrl Pts',(-10.687239087346,8.45003988621903,10.0435215626047));
#120271=CARTESIAN_POINT('Ctrl Pts',(-10.6812856909329,8.44954326047079,
10.0392719596426));
#120272=CARTESIAN_POINT('Ctrl Pts',(-10.6616341081802,8.44790771690757,
10.0255189487917));
#120273=CARTESIAN_POINT('Ctrl Pts',(-10.6477742111607,8.44676009770651,
10.0162512849215));
#120274=CARTESIAN_POINT('Ctrl Pts',(-10.6146559595049,8.44403020957948,
9.99510955183233));
#120275=CARTESIAN_POINT('Ctrl Pts',(-10.59524349246,8.44243952015611,9.983490368511));
#120276=CARTESIAN_POINT('Ctrl Pts',(-10.5213122654469,8.43641647459734,
9.94208349821359));
#120277=CARTESIAN_POINT('Ctrl Pts',(-10.4648036764495,8.43187538666773,
9.91606741663069));
#120278=CARTESIAN_POINT('Ctrl Pts',(-10.347033757933,8.42266658175131,9.87275601001855));
#120279=CARTESIAN_POINT('Ctrl Pts',(-10.2858793673687,8.41801371882402,
9.85571596757049));
#120280=CARTESIAN_POINT('Ctrl Pts',(-10.2132312943913,8.41281932034774,
9.84166498923229));
#120281=CARTESIAN_POINT('Ctrl Pts',(-10.2027895777748,8.41208074154891,
9.83979140290306));
#120282=CARTESIAN_POINT('Ctrl Pts',(-10.1882217785839,8.41106272329828,
9.83738015247417));
#120283=CARTESIAN_POINT('Ctrl Pts',(-10.1841163829741,8.41077719939434,
9.83672294502803));
#120284=CARTESIAN_POINT('Ctrl Pts',(-10.17661474085,8.41025806943173,9.83556276164537));
#120285=CARTESIAN_POINT('Ctrl Pts',(-10.1732196125569,8.41002408990471,
9.83505286995433));
#120286=CARTESIAN_POINT('Ctrl Pts',(-10.16614682746,8.40953873757135,9.83402226032232));
#120287=CARTESIAN_POINT('Ctrl Pts',(-10.1624688760186,8.40928750473616,
9.83350408359654));
#120288=CARTESIAN_POINT('Ctrl Pts',(-10.1527428500748,8.40862605113666,
9.83218070299519));
#120289=CARTESIAN_POINT('Ctrl Pts',(-10.1466907672967,8.40821742662606,
9.83140506955573));
#120290=CARTESIAN_POINT('Ctrl Pts',(-10.1333138088881,8.40732024756581,
9.82979624301008));
#120291=CARTESIAN_POINT('Ctrl Pts',(-10.1259865324777,8.40683278088396,
9.82898471212525));
#120292=CARTESIAN_POINT('Ctrl Pts',(-10.0161996174005,8.39958173447358,
9.81786771765004));
#120293=CARTESIAN_POINT('Ctrl Pts',(-9.91282441641975,8.39341095337636,
9.82097238054841));
#120294=CARTESIAN_POINT('Ctrl Pts',(-9.81114929946652,8.38697610116898,
9.83748958051637));
#120295=CARTESIAN_POINT('Ctrl Pts',(-9.81114931547642,8.2871573923531,9.83748957791555));
#120296=CARTESIAN_POINT('Ctrl Pts',(-9.81679607853834,8.28751902272957,
9.83657225704743));
#120297=CARTESIAN_POINT('Ctrl Pts',(-9.82245093697995,8.28788160001983,
9.8356958495605));
#120298=CARTESIAN_POINT('Ctrl Pts',(-9.85065399390001,8.28969261320193,
9.83153520975173));
#120299=CARTESIAN_POINT('Ctrl Pts',(-9.8732851306851,8.29115452240905,9.82886489203476));
#120300=CARTESIAN_POINT('Ctrl Pts',(-9.91282461577387,8.2937343285415,9.82535897457222));
#120301=CARTESIAN_POINT('Ctrl Pts',(-9.92970024557085,8.29484346375028,
9.82422834526252));
#120302=CARTESIAN_POINT('Ctrl Pts',(-9.95446843504627,8.29648590351012,
9.82310404953484));
#120303=CARTESIAN_POINT('Ctrl Pts',(-9.96234638984553,8.29701046038242,
9.82282567041498));
#120304=CARTESIAN_POINT('Ctrl Pts',(-9.97629995671946,8.29794364132196,
9.82247281039204));
#120305=CARTESIAN_POINT('Ctrl Pts',(-9.9823745230772,8.29835126059794,9.82236622223877));
#120306=CARTESIAN_POINT('Ctrl Pts',(-9.99513005126263,8.2992101853748,9.82224111995086));
#120307=CARTESIAN_POINT('Ctrl Pts',(-10.0018108708652,8.29966178002077,
9.82223244504251));
#120308=CARTESIAN_POINT('Ctrl Pts',(-10.0194677069978,8.30086004411813,
9.82235974976683));
#120309=CARTESIAN_POINT('Ctrl Pts',(-10.0304421505515,8.30160965887142,
9.82259233401424));
#120310=CARTESIAN_POINT('Ctrl Pts',(-10.0792128906541,8.30496350330611,
9.82430824617389));
#120311=CARTESIAN_POINT('Ctrl Pts',(-10.1169243163701,8.3076180711371,9.82745834118891));
#120312=CARTESIAN_POINT('Ctrl Pts',(-10.2306115288349,8.3158082518639,9.84249372998667));
#120313=CARTESIAN_POINT('Ctrl Pts',(-10.3056328088298,8.32148312800247,
9.86000488135048));
#120314=CARTESIAN_POINT('Ctrl Pts',(-10.409588282637,8.32950916924227,9.89527518704539));
#120315=CARTESIAN_POINT('Ctrl Pts',(-10.4403173673678,8.33190047220863,
9.90715949277119));
#120316=CARTESIAN_POINT('Ctrl Pts',(-10.4819203658134,8.33513209142243,
9.92528945637227));
#120317=CARTESIAN_POINT('Ctrl Pts',(-10.4932519578149,8.33601162716575,
9.93044283711684));
#120318=CARTESIAN_POINT('Ctrl Pts',(-10.5127952712848,8.33752486269641,
9.93970742548203));
#120319=CARTESIAN_POINT('Ctrl Pts',(-10.5210444082844,8.33816243033933,
9.94373674144378));
#120320=CARTESIAN_POINT('Ctrl Pts',(-10.5331355857896,8.33909433586551,
9.94981884059448));
#120321=CARTESIAN_POINT('Ctrl Pts',(-10.5370144712871,8.33939289316836,
9.95179702368593));
#120322=CARTESIAN_POINT('Ctrl Pts',(-10.5438933998816,8.33992153201631,
9.95535339869649));
#120323=CARTESIAN_POINT('Ctrl Pts',(-10.546897695875,8.34015211795317,9.95692307892815));
#120324=CARTESIAN_POINT('Ctrl Pts',(-10.5534578378338,8.34065497254719,
9.9603867478662));
#120325=CARTESIAN_POINT('Ctrl Pts',(-10.5570107713701,8.34092691008848,
9.96228602492832));
#120326=CARTESIAN_POINT('Ctrl Pts',(-10.567011139677,8.34169137963912,9.96769803990997));
#120327=CARTESIAN_POINT('Ctrl Pts',(-10.5734357071145,8.34218138232288,
9.97125296313846));
#120328=CARTESIAN_POINT('Ctrl Pts',(-10.6147894482421,8.34533094511393,
9.99464312567753));
#120329=CARTESIAN_POINT('Ctrl Pts',(-10.6487216450408,8.34789474066395,
10.0161964272414));
#120330=CARTESIAN_POINT('Ctrl Pts',(-10.7390004364148,8.35484580053304,
10.0802468789802));
#120331=CARTESIAN_POINT('Ctrl Pts',(-10.7927317135713,8.35914074423533,
10.1261325001123));
#120332=CARTESIAN_POINT('Ctrl Pts',(-10.8778649470928,8.36676046191007,
10.2131873479139));
#120333=CARTESIAN_POINT('Ctrl Pts',(-10.9112599897202,8.37001928137387,
10.2521194758373));
#120334=CARTESIAN_POINT('Ctrl Pts',(-10.9488997690667,8.3741359637718,10.3022779985991));
#120335=CARTESIAN_POINT('Ctrl Pts',(-10.9556531288595,8.37489416657365,
10.3115569412462));
#120336=CARTESIAN_POINT('Ctrl Pts',(-10.9661840139989,8.37610910719644,
10.3264796931753));
#120337=CARTESIAN_POINT('Ctrl Pts',(-10.9700502936138,8.37656247965453,
10.3320601994038));
#120338=CARTESIAN_POINT('Ctrl Pts',(-10.9772716867776,8.37742347901851,
10.3426783558554));
#120339=CARTESIAN_POINT('Ctrl Pts',(-10.9806366465613,8.37783072036775,
10.3477090689604));
#120340=CARTESIAN_POINT('Ctrl Pts',(-10.9881860080057,8.37875836953882,
10.3591860352838));
#120341=CARTESIAN_POINT('Ctrl Pts',(-10.9923463526853,8.37927964210262,
10.3656477041397));
#120342=CARTESIAN_POINT('Ctrl Pts',(-11.0048941881421,8.3808833890068,10.3855620049134));
#120343=CARTESIAN_POINT('Ctrl Pts',(-11.0130732550673,8.38197331599752,
10.3991431812292));
#120344=CARTESIAN_POINT('Ctrl Pts',(-11.0624569043934,8.38884497066996,
10.4850198300692));
#120345=CARTESIAN_POINT('Ctrl Pts',(-11.096169650088,8.39488833686616,10.5613354085241));
#120346=CARTESIAN_POINT('Ctrl Pts',(-11.1425261878471,8.40603352208812,
10.7059772056802));
#120347=CARTESIAN_POINT('Ctrl Pts',(-11.1577318102823,8.41108787112069,
10.7731203176236));
#120348=CARTESIAN_POINT('Ctrl Pts',(-11.1682224058165,8.4165307433325,10.8502197582763));
#120349=CARTESIAN_POINT('Ctrl Pts',(-11.1693438025817,8.4171620342498,10.8592420722607));
#120350=CARTESIAN_POINT('Ctrl Pts',(-11.1708457290484,8.41808656839774,
10.8725866895361));
#120351=CARTESIAN_POINT('Ctrl Pts',(-11.1713070025415,8.41838393889068,
10.8768993086351));
#120352=CARTESIAN_POINT('Ctrl Pts',(-11.1720862080964,8.4189113089975,10.8845856802864));
#120353=CARTESIAN_POINT('Ctrl Pts',(-11.1724134151022,8.41914180312824,
10.8879583584144));
#120354=CARTESIAN_POINT('Ctrl Pts',(-11.1730989900469,8.4196454366688,10.8953570002676));
#120355=CARTESIAN_POINT('Ctrl Pts',(-11.1734511939247,8.41991823698202,
10.8993834281063));
#120356=CARTESIAN_POINT('Ctrl Pts',(-11.174389635909,8.42068748134716,10.9107877755314));
#120357=CARTESIAN_POINT('Ctrl Pts',(-11.1749270798201,8.42118134624302,
10.9181696761109));
#120358=CARTESIAN_POINT('Ctrl Pts',(-11.1781270633891,8.42453682724228,
10.9686944161239));
#120359=CARTESIAN_POINT('Ctrl Pts',(-11.1784826553976,8.42728717605689,
11.0119554798718));
#120360=CARTESIAN_POINT('Ctrl Pts',(-11.1755303080243,8.43123676183979,
11.0749431308556));
#120361=CARTESIAN_POINT('Ctrl Pts',(-11.1741024823302,8.43246867328965,
11.0947173248053));
#120362=CARTESIAN_POINT('Ctrl Pts',(-11.1673006187578,8.43680691062823,
11.1643829547109));
#120363=CARTESIAN_POINT('Ctrl Pts',(-11.1592391090024,8.43989277293091,
11.2139556748244));
#120364=CARTESIAN_POINT('Ctrl Pts',(-11.1371420866949,8.44609923009376,
11.3104634791576));
#120365=CARTESIAN_POINT('Ctrl Pts',(-11.1232944364729,8.4492106695294,11.3573352011814));
#120366=CARTESIAN_POINT('Ctrl Pts',(-11.1026972240125,8.45316127618904,
11.4138628714252));
#120367=CARTESIAN_POINT('Ctrl Pts',(-11.098661577485,8.45391061325622,11.4244600896895));
#120368=CARTESIAN_POINT('Ctrl Pts',(-11.0919771031511,8.45511466317859,
11.4412785494345));
#120369=CARTESIAN_POINT('Ctrl Pts',(-11.0894265614543,8.45556611668206,
11.447538284379));
#120370=CARTESIAN_POINT('Ctrl Pts',(-11.0844882975585,8.45642559101367,
11.45936575003));
#120371=CARTESIAN_POINT('Ctrl Pts',(-11.0821112165235,8.45683324463233,
11.4649377082649));
#120372=CARTESIAN_POINT('Ctrl Pts',(-11.0766009637549,8.45776479018088,
11.4775827366181));
#120373=CARTESIAN_POINT('Ctrl Pts',(-11.0734409038124,8.45828957480671,
11.4846437109426));
#120374=CARTESIAN_POINT('Ctrl Pts',(-11.0634817468255,8.45991528494975,
11.5063215482407));
#120375=CARTESIAN_POINT('Ctrl Pts',(-11.0564521731293,8.46102396340335,
11.5208298161523));
#120376=CARTESIAN_POINT('Ctrl Pts',(-11.0159326493457,8.4672120375939,11.6002600151921));
#120377=CARTESIAN_POINT('Ctrl Pts',(-10.9767615746854,8.47248722130337,
11.6620912002533));
#120378=CARTESIAN_POINT('Ctrl Pts',(-10.9020840994072,8.48143774327591,
11.758785078553));
#120379=CARTESIAN_POINT('Ctrl Pts',(-10.8696375019692,8.48505963192723,
11.7957646249844));
#120380=CARTESIAN_POINT('Ctrl Pts',(-10.811692936878,8.49100932255054,11.854013727516));
#120381=CARTESIAN_POINT('Ctrl Pts',(-10.7874348360801,8.49336837872976,
11.8764312212767));
#120382=CARTESIAN_POINT('Ctrl Pts',(-10.7570670618802,8.49613764545614,
11.902214504601));
#120383=CARTESIAN_POINT('Ctrl Pts',(-10.7518312583617,8.49660882388745,
11.9065822152277));
#120384=CARTESIAN_POINT('Ctrl Pts',(-10.743563837538,8.49734265846856,11.9133580160886));
#120385=CARTESIAN_POINT('Ctrl Pts',(-10.7405578756893,8.49760739967164,
11.9157969643366));
#120386=CARTESIAN_POINT('Ctrl Pts',(-10.7348775038153,8.49810370516149,
11.9203595918809));
#120387=CARTESIAN_POINT('Ctrl Pts',(-10.7322058921926,8.49833548069488,
11.9224864528827));
#120388=CARTESIAN_POINT('Ctrl Pts',(-10.7259770090227,8.49887211557101,
11.9274011373094));
#120389=CARTESIAN_POINT('Ctrl Pts',(-10.7224128942928,8.49917636298976,
11.9301801432769));
#120390=CARTESIAN_POINT('Ctrl Pts',(-10.710636291383,8.50017278712573,11.9392540611455));
#120391=CARTESIAN_POINT('Ctrl Pts',(-10.7023565678057,8.50085926029323,
11.9454614744132));
#120392=CARTESIAN_POINT('Ctrl Pts',(-10.6372387551582,8.50615896316596,
11.9929535123087));
#120393=CARTESIAN_POINT('Ctrl Pts',(-10.5768839080176,8.51049496240418,
12.0291926744667));
#120394=CARTESIAN_POINT('Ctrl Pts',(-10.4616199292691,8.51841845582033,
12.0850554129716));
#120395=CARTESIAN_POINT('Ctrl Pts',(-10.4078057816376,8.52199152730307,
12.106405008037));
#120396=CARTESIAN_POINT('Ctrl Pts',(-10.3321797296197,8.52703818106705,
12.1301379125482));
#120397=CARTESIAN_POINT('Ctrl Pts',(-10.3115452430198,8.52841704855334,
12.1359993633913));
#120398=CARTESIAN_POINT('Ctrl Pts',(-10.2751137668893,8.53086351430993,
12.1452808718164));
#120399=CARTESIAN_POINT('Ctrl Pts',(-10.2593847254968,8.53192358428407,
12.1489453352583));
#120400=CARTESIAN_POINT('Ctrl Pts',(-10.2360120616192,8.53350683901492,
12.153886171082));
#120401=CARTESIAN_POINT('Ctrl Pts',(-10.2284227698922,8.53402217128693,
12.1554124901795));
#120402=CARTESIAN_POINT('Ctrl Pts',(-10.2148681358126,8.53494502245415,
12.1579997631071));
#120403=CARTESIAN_POINT('Ctrl Pts',(-10.2089085606937,8.53535161523942,
12.1590897195966));
#120404=CARTESIAN_POINT('Ctrl Pts',(-10.1962856641109,8.53621471798645,
12.161297829394));
#120405=CARTESIAN_POINT('Ctrl Pts',(-10.1896206211694,8.53667156498084,
12.1624047174872));
#120406=CARTESIAN_POINT('Ctrl Pts',(-10.1717588021953,8.53789905458422,
12.1652133867625));
#120407=CARTESIAN_POINT('Ctrl Pts',(-10.1605466227965,8.53867290495318,
12.1668110769148));
#120408=CARTESIAN_POINT('Ctrl Pts',(-10.1067668585391,8.54240179143784,
12.1736846619688));
#120409=CARTESIAN_POINT('Ctrl Pts',(-10.0639600438863,8.5454226463176,12.1767936005867));
#120410=CARTESIAN_POINT('Ctrl Pts',(-9.9318331881085,8.55490549544547,12.1791592288951));
#120411=CARTESIAN_POINT('Ctrl Pts',(-9.84270097056296,8.56154883121804,
12.1706058066696));
#120412=CARTESIAN_POINT('Ctrl Pts',(-9.73480427928271,8.56952435227488,
12.1476974326235));
#120413=CARTESIAN_POINT('Ctrl Pts',(-9.71433287150389,8.57103292191426,
12.1427740649778));
#120414=CARTESIAN_POINT('Ctrl Pts',(-9.68089175215072,8.57347873015354,
12.1337765857428));
#120415=CARTESIAN_POINT('Ctrl Pts',(-9.66784146782375,8.5744284653335,12.1300221984775));
#120416=CARTESIAN_POINT('Ctrl Pts',(-9.64999773388478,8.57571786933657,
12.1245529429262));
#120417=CARTESIAN_POINT('Ctrl Pts',(-9.64514669553454,8.57606746816337,
12.1230316301923));
#120418=CARTESIAN_POINT('Ctrl Pts',(-9.63697686435524,8.5766544741878,12.120411301907));
#120419=CARTESIAN_POINT('Ctrl Pts',(-9.63365287252975,8.57689280744138,
12.119328846167));
#120420=CARTESIAN_POINT('Ctrl Pts',(-9.62684893492248,8.57737957068267,
12.1170795922912));
#120421=CARTESIAN_POINT('Ctrl Pts',(-9.62336955301328,8.57762791365505,
12.1159113048154));
#120422=CARTESIAN_POINT('Ctrl Pts',(-9.61430674992187,8.57827340915604,
12.1128210308439));
#120423=CARTESIAN_POINT('Ctrl Pts',(-9.60873213673921,8.57866910049231,
12.1108732567818));
#120424=CARTESIAN_POINT('Ctrl Pts',(-9.58576255012235,8.58029479756681,
12.1026533055393));
#120425=CARTESIAN_POINT('Ctrl Pts',(-9.56850080200281,8.58150532596359,
12.0960134626381));
#120426=CARTESIAN_POINT('Ctrl Pts',(-9.44543084244235,8.59010371441348,
12.0453150666999));
#120427=CARTESIAN_POINT('Ctrl Pts',(-9.34639144423488,8.59690633388872,
11.9864240202187));
#120428=CARTESIAN_POINT('Ctrl Pts',(-9.23974955710112,8.60563475777251,
11.8997956577013));
#120429=CARTESIAN_POINT('Ctrl Pts',(-9.22250624374912,8.60709498584035,
11.8849385992635));
#120430=CARTESIAN_POINT('Ctrl Pts',(-9.19322902106502,8.60967210110284,
11.8581964555101));
#120431=CARTESIAN_POINT('Ctrl Pts',(-9.18100038991453,8.61078025256616,
11.8465342053494));
#120432=CARTESIAN_POINT('Ctrl Pts',(-9.16344315195123,8.61242150769173,
11.8290535552397));
#120433=CARTESIAN_POINT('Ctrl Pts',(-9.15791501478316,8.61294588208986,
11.8234379333706));
#120434=CARTESIAN_POINT('Ctrl Pts',(-9.14822549268473,8.61387885713553,
11.8133954503379));
#120435=CARTESIAN_POINT('Ctrl Pts',(-9.14404118908444,8.61428645455235,
11.8089910268986));
#120436=CARTESIAN_POINT('Ctrl Pts',(-9.13532639241484,8.61514545433638,
11.7996744756803));
#120437=CARTESIAN_POINT('Ctrl Pts',(-9.13080326823792,8.61559714675613,
11.7947557820045));
#120438=CARTESIAN_POINT('Ctrl Pts',(-9.11895700031396,8.61679595447838,
11.7816514092818));
#120439=CARTESIAN_POINT('Ctrl Pts',(-9.11170623169963,8.61754601988317,
11.7734014869193));
#120440=CARTESIAN_POINT('Ctrl Pts',(-9.07964155799004,8.62093844524035,
11.7358725110338));
#120441=CARTESIAN_POINT('Ctrl Pts',(-9.05615485478083,8.62363277251214,
11.705495420198));
#120442=CARTESIAN_POINT('Ctrl Pts',(-8.9903641967241,8.63184698680208,11.6112250466583));
#120443=CARTESIAN_POINT('Ctrl Pts',(-8.95276731990563,8.63750243160193,
11.5442996649155));
#120444=CARTESIAN_POINT('Ctrl Pts',(-8.90875880724403,8.64549274175582,
11.4442508500947));
#120445=CARTESIAN_POINT('Ctrl Pts',(-8.89683491623107,8.6478688791902,11.4137550455752));
#120446=CARTESIAN_POINT('Ctrl Pts',(-8.88216639193007,8.65108222244006,
11.3710752012001));
#120447=CARTESIAN_POINT('Ctrl Pts',(-8.87832183314732,8.65195822724983,
11.3592866501721));
#120448=CARTESIAN_POINT('Ctrl Pts',(-8.87196402145976,8.65346601856556,
11.3386940495358));
#120449=CARTESIAN_POINT('Ctrl Pts',(-8.86936597935487,8.65410163734315,
11.3299174931273));
#120450=CARTESIAN_POINT('Ctrl Pts',(-8.86568472277536,8.65503125497131,
11.316927162763));
#120451=CARTESIAN_POINT('Ctrl Pts',(-8.86452218797081,8.6553294445303,11.3127364937871));
#120452=CARTESIAN_POINT('Ctrl Pts',(-8.86257955839264,8.65583564819996,
11.3055801109436));
#120453=CARTESIAN_POINT('Ctrl Pts',(-8.86178780182369,8.6560443133985,11.302617676156));
#120454=CARTESIAN_POINT('Ctrl Pts',(-8.86001555960837,8.65651678528478,
11.2958812956129));
#120455=CARTESIAN_POINT('Ctrl Pts',(-8.8590422363749,8.65678018411602,11.2921055428348));
#120456=CARTESIAN_POINT('Ctrl Pts',(-8.85643101076055,8.65749792195231,
11.2817637716496));
#120457=CARTESIAN_POINT('Ctrl Pts',(-8.85483088807857,8.6579501957944,11.2751882384675));
#120458=CARTESIAN_POINT('Ctrl Pts',(-8.84667118142944,8.6603264909574,11.2403525367526));
#120459=CARTESIAN_POINT('Ctrl Pts',(-8.84110019414229,8.66220107772388,
11.2118684889089));
#120460=CARTESIAN_POINT('Ctrl Pts',(-8.83453145209203,8.66488543934019,
11.170154822135));
#120461=CARTESIAN_POINT('Ctrl Pts',(-8.83269605008768,8.66571881788552,
11.1570703867563));
#120462=CARTESIAN_POINT('Ctrl Pts',(-8.82285691323287,8.67076928251592,
11.0771776993491));
#120463=CARTESIAN_POINT('Ctrl Pts',(-8.82037024494847,8.67487300323337,
11.0098151051508));
#120464=CARTESIAN_POINT('Ctrl Pts',(-8.82624350914554,8.68240500841242,
10.889433487855));
#120465=CARTESIAN_POINT('Ctrl Pts',(-8.83243976139679,8.68578522600619,
10.8365029577041));
#120466=CARTESIAN_POINT('Ctrl Pts',(-8.84431576322054,8.69003862415664,
10.7727927957167));
#120467=CARTESIAN_POINT('Ctrl Pts',(-8.84660560621155,8.69080359317017,
10.7614407292466));
#120468=CARTESIAN_POINT('Ctrl Pts',(-8.850507560211,8.69202684527201,10.7434681499615));
#120469=CARTESIAN_POINT('Ctrl Pts',(-8.85201040669254,8.6924816811359,10.7368244889986));
#120470=CARTESIAN_POINT('Ctrl Pts',(-8.85495641662997,8.69334387049026,
10.7243066193936));
#120471=CARTESIAN_POINT('Ctrl Pts',(-8.85638737502612,8.69375082457745,
10.7184297430666));
#120472=CARTESIAN_POINT('Ctrl Pts',(-8.85973005102203,8.69467563464132,
10.7051474978714));
#120473=CARTESIAN_POINT('Ctrl Pts',(-8.86166874612947,8.69519433490316,
10.6977492659351));
#120474=CARTESIAN_POINT('Ctrl Pts',(-8.8677959586814,8.69678211205941,10.6752627769738));
#120475=CARTESIAN_POINT('Ctrl Pts',(-8.87221330294783,8.69785842702708,
10.6602392307735));
#120476=CARTESIAN_POINT('Ctrl Pts',(-8.90311345343404,8.7049733097886,10.562398982531));
#120477=CARTESIAN_POINT('Ctrl Pts',(-8.93839419861791,8.71130072579013,
10.4826582039402));
#120478=CARTESIAN_POINT('Ctrl Pts',(-9.0159954478927,8.72262181892624,10.3493343297986));
#120479=CARTESIAN_POINT('Ctrl Pts',(-9.05480819377194,8.72756567297334,
10.2941351553612));
#120480=CARTESIAN_POINT('Ctrl Pts',(-9.10314577822001,8.73280540284141,
10.2365811313431));
#120481=CARTESIAN_POINT('Ctrl Pts',(-9.10821996473862,8.73334546988118,
10.2306598665274));
#120482=CARTESIAN_POINT('Ctrl Pts',(-9.1160376757059,8.73416196959699,10.2217183602025));
#120483=CARTESIAN_POINT('Ctrl Pts',(-9.11873858548639,8.73444129303964,
10.2186613908377));
#120484=CARTESIAN_POINT('Ctrl Pts',(-9.12371041990526,8.73495034065239,
10.2130926998654));
#120485=CARTESIAN_POINT('Ctrl Pts',(-9.12597631203077,8.73518040641653,
10.2105767164225));
#120486=CARTESIAN_POINT('Ctrl Pts',(-9.13113830732347,8.73570019787902,
10.2048944518533));
#120487=CARTESIAN_POINT('Ctrl Pts',(-9.13404088882153,8.73598943746571,
10.2017341965808));
#120488=CARTESIAN_POINT('Ctrl Pts',(-9.14164409642154,8.7367394482269,10.193546296282));
#120489=CARTESIAN_POINT('Ctrl Pts',(-9.14637171564984,8.73719829392061,
10.1885437836248));
#120490=CARTESIAN_POINT('Ctrl Pts',(-9.18750670985272,8.7411296442458,10.1457743171033));
#120491=CARTESIAN_POINT('Ctrl Pts',(-9.22636081116914,8.74443662049366,
10.110432285927));
#120492=CARTESIAN_POINT('Ctrl Pts',(-9.30563774023128,8.75073875225215,
10.0474586856642));
#120493=CARTESIAN_POINT('Ctrl Pts',(-9.34567597300713,8.75373375459912,
10.0195235691197));
#120494=CARTESIAN_POINT('Ctrl Pts',(-9.43392488733558,8.76016685352888,
9.96577058855639));
#120495=CARTESIAN_POINT('Ctrl Pts',(-9.48242921746681,8.76360869313542,
9.94066484789565));
#120496=CARTESIAN_POINT('Ctrl Pts',(-9.54611206531721,8.76813400013127,
9.9131233237625));
#120497=CARTESIAN_POINT('Ctrl Pts',(-9.55983860952306,8.76910947268172,
9.90749229522944));
#120498=CARTESIAN_POINT('Ctrl Pts',(-9.58064747193377,8.77059019873423,
9.89941170799842));
#120499=CARTESIAN_POINT('Ctrl Pts',(-9.58765312108235,8.77108903276959,
9.89676784927144));
#120500=CARTESIAN_POINT('Ctrl Pts',(-9.60029747688905,8.77199017875766,
9.89213326249202));
#120501=CARTESIAN_POINT('Ctrl Pts',(-9.60592708114431,8.77239167893117,
9.89011831827345));
#120502=CARTESIAN_POINT('Ctrl Pts',(-9.61808406746698,8.77325944369891,
9.88587125067659));
#120503=CARTESIAN_POINT('Ctrl Pts',(-9.6246161782072,8.77372615889111,9.88365344429567));
#120504=CARTESIAN_POINT('Ctrl Pts',(-9.64225647317828,8.77498796046651,
9.87783647656071));
#120505=CARTESIAN_POINT('Ctrl Pts',(-9.65339907596273,8.77578649181745,
9.87434499655869));
#120506=CARTESIAN_POINT('Ctrl Pts',(-9.71268718016144,8.78004465563389,
9.85673109983618));
#120507=CARTESIAN_POINT('Ctrl Pts',(-9.76163923892622,8.78359601191732,
9.84553252734959));
#120508=CARTESIAN_POINT('Ctrl Pts',(-9.81114930181833,8.78721751211607,
9.83748958013431));
#120509=CARTESIAN_POINT('Origin',(-10.,2.67563288526385,11.));
#120510=CARTESIAN_POINT('',(-9.81114929159341,9.38732021621766,9.83748958179536));
#120511=CARTESIAN_POINT('',(-9.81114930150155,9.28890850071391,9.83748958018577));
#120512=CARTESIAN_POINT('',(-9.81114930150157,2.67563288526385,9.83748958018577));
#120513=CARTESIAN_POINT('Ctrl Pts',(-9.81114929154307,9.38732021693139,
9.83748958180354));
#120514=CARTESIAN_POINT('Ctrl Pts',(-9.80032443062653,9.38653646503526,
9.83924808875628));
#120515=CARTESIAN_POINT('Ctrl Pts',(-9.7895231070358,9.38574897201044,9.84115795741129));
#120516=CARTESIAN_POINT('Ctrl Pts',(-9.72949114500639,9.38134292685675,
9.85263995832945));
#120517=CARTESIAN_POINT('Ctrl Pts',(-9.68088846556259,9.3776625054019,9.8651972060573));
#120518=CARTESIAN_POINT('Ctrl Pts',(-9.61392716259896,9.37249212111339,
9.88714073354232));
#120519=CARTESIAN_POINT('Ctrl Pts',(-9.59478384343625,9.37100253447649,
9.89396750737397));
#120520=CARTESIAN_POINT('Ctrl Pts',(-9.53605463055195,9.36641123538269,
9.91664072613371));
#120521=CARTESIAN_POINT('Ctrl Pts',(-9.49714120270248,9.36333749679626,
9.93414519946232));
#120522=CARTESIAN_POINT('Ctrl Pts',(-9.45322292166835,9.3598935556402,9.95684322497667));
#120523=CARTESIAN_POINT('Ctrl Pts',(-9.44721364051956,9.35942291712428,
9.96001515549274));
#120524=CARTESIAN_POINT('Ctrl Pts',(-9.43747741296814,9.35866175565437,
9.96526254873928));
#120525=CARTESIAN_POINT('Ctrl Pts',(-9.43373379599942,9.35836941849369,
9.9673065113007));
#120526=CARTESIAN_POINT('Ctrl Pts',(-9.42703847290861,9.35784729267967,
9.97100941970892));
#120527=CARTESIAN_POINT('Ctrl Pts',(-9.42408274486057,9.35761705203515,
9.97266079508712));
#120528=CARTESIAN_POINT('Ctrl Pts',(-9.41756052796343,9.35710956599148,
9.97634177502931));
#120529=CARTESIAN_POINT('Ctrl Pts',(-9.41399749646752,9.35683269637592,
9.97837728722175));
#120530=CARTESIAN_POINT('Ctrl Pts',(-9.40359605239276,9.35602529418844,
9.9843918136961));
#120531=CARTESIAN_POINT('Ctrl Pts',(-9.39678684758696,9.35549782406152,
9.98842125471743));
#120532=CARTESIAN_POINT('Ctrl Pts',(-9.33208877350592,9.35049136239869,
10.0275928432357));
#120533=CARTESIAN_POINT('Ctrl Pts',(-9.27728307350225,9.34628730934923,
10.0676030751559));
#120534=CARTESIAN_POINT('Ctrl Pts',(-9.16114682501842,9.33675164390476,
10.1688142367135));
#120535=CARTESIAN_POINT('Ctrl Pts',(-9.10251686948338,9.33144107663792,
10.2324933681102));
#120536=CARTESIAN_POINT('Ctrl Pts',(-9.04206810367296,9.32479866363295,
10.3146475357289));
#120537=CARTESIAN_POINT('Ctrl Pts',(-9.03301822573962,9.32376758093149,
10.3274765960256));
#120538=CARTESIAN_POINT('Ctrl Pts',(-9.01994002506405,9.32221930463233,
10.346826104499));
#120539=CARTESIAN_POINT('Ctrl Pts',(-9.01571430127629,9.32170945607147,
10.3532115099214));
#120540=CARTESIAN_POINT('Ctrl Pts',(-9.00826120605182,9.32079256083556,
10.3647159364668));
#120541=CARTESIAN_POINT('Ctrl Pts',(-9.00501042877679,9.32038639293661,
10.3698195277322));
#120542=CARTESIAN_POINT('Ctrl Pts',(-8.99818538797317,9.31952007059205,
10.3807190366764));
#120543=CARTESIAN_POINT('Ctrl Pts',(-8.99462178613516,9.31905954745268,
10.3865213352271));
#120544=CARTESIAN_POINT('Ctrl Pts',(-8.98514224464405,9.3178119243831,10.4022604794136));
#120545=CARTESIAN_POINT('Ctrl Pts',(-8.97932214949556,9.31702143201238,
10.4122538753469));
#120546=CARTESIAN_POINT('Ctrl Pts',(-8.947712153106,9.3125867776909,10.4684156433584));
#120547=CARTESIAN_POINT('Ctrl Pts',(-8.92491100156425,9.30883960906149,
10.5161881959716));
#120548=CARTESIAN_POINT('Ctrl Pts',(-8.87689532779373,9.2994320460074,10.637101560905));
#120549=CARTESIAN_POINT('Ctrl Pts',(-8.85552284764237,9.29369959223338,
10.7115029722206));
#120550=CARTESIAN_POINT('Ctrl Pts',(-8.83575232374524,9.28576801412107,
10.8192579941486));
#120551=CARTESIAN_POINT('Ctrl Pts',(-8.8312291121996,9.28345778429272,10.8512877085673));
#120552=CARTESIAN_POINT('Ctrl Pts',(-8.82734011420872,9.28072362762297,
10.8903989177766));
#120553=CARTESIAN_POINT('Ctrl Pts',(-8.82671224417878,9.28024184026102,
10.8973381625369));
#120554=CARTESIAN_POINT('Ctrl Pts',(-8.8258253427327,9.27949227928516,10.9082149180464));
#120555=CARTESIAN_POINT('Ctrl Pts',(-8.82552446578684,9.27922233189707,
10.9121487181704));
#120556=CARTESIAN_POINT('Ctrl Pts',(-8.8250253239318,9.27874494796017,10.9191363058126));
#120557=CARTESIAN_POINT('Ctrl Pts',(-8.82481919167721,9.27853709289594,
10.922189367428));
#120558=CARTESIAN_POINT('Ctrl Pts',(-8.8243529723141,9.27803975674625,10.9295195823278));
#120559=CARTESIAN_POINT('Ctrl Pts',(-8.82410432476527,9.27775090639987,
10.9337973913837));
#120560=CARTESIAN_POINT('Ctrl Pts',(-8.82341543058647,9.27687139981388,
10.9468816565464));
#120561=CARTESIAN_POINT('Ctrl Pts',(-8.82305071412459,9.27628469097743,
10.9556920183317));
#120562=CARTESIAN_POINT('Ctrl Pts',(-8.8224290377103,9.27492276813782,10.9763108857761));
#120563=CARTESIAN_POINT('Ctrl Pts',(-8.82225068144433,9.27415122991986,
10.9881209842543));
#120564=CARTESIAN_POINT('Ctrl Pts',(-8.82224825684961,9.27142209641782,
11.0302662602129));
#120565=CARTESIAN_POINT('Ctrl Pts',(-8.82341843592351,9.26950290299789,
11.060591207284));
#120566=CARTESIAN_POINT('Ctrl Pts',(-8.83141895204983,9.26301117334748,
11.1640107879518));
#120567=CARTESIAN_POINT('Ctrl Pts',(-8.84390629886187,9.25854333736454,
11.236492792907));
#120568=CARTESIAN_POINT('Ctrl Pts',(-8.87460691765328,9.25114500448191,
11.3500626974604));
#120569=CARTESIAN_POINT('Ctrl Pts',(-8.888552746776,9.24831696275417,11.3920941457527));
#120570=CARTESIAN_POINT('Ctrl Pts',(-8.90902603454186,9.24466285719496,
11.4438480047155));
#120571=CARTESIAN_POINT('Ctrl Pts',(-8.9133769642662,9.24390895673842,11.4543958713892));
#120572=CARTESIAN_POINT('Ctrl Pts',(-8.92055486561516,9.24269922125629,
11.4711042093946));
#120573=CARTESIAN_POINT('Ctrl Pts',(-8.92328302895718,9.24224669934713,
11.4773065422678));
#120574=CARTESIAN_POINT('Ctrl Pts',(-8.92855091868038,9.24138623949891,
11.4890077845142));
#120575=CARTESIAN_POINT('Ctrl Pts',(-8.93107985122903,9.24097867801445,
11.4945113349354));
#120576=CARTESIAN_POINT('Ctrl Pts',(-8.93692546247149,9.2400488027501,11.5069783808752));
#120577=CARTESIAN_POINT('Ctrl Pts',(-8.94026829368006,9.23952560963872,
11.5139292332034));
#120578=CARTESIAN_POINT('Ctrl Pts',(-8.95075152700913,9.23791033066491,
11.5351901157291));
#120579=CARTESIAN_POINT('Ctrl Pts',(-8.95811506419071,9.23681063723439,
11.5493874362331));
#120580=CARTESIAN_POINT('Ctrl Pts',(-8.9758952273204,9.23423194000081,11.5820248012439));
#120581=CARTESIAN_POINT('Ctrl Pts',(-8.98652444194508,9.23274597497384,
11.600342112871));
#120582=CARTESIAN_POINT('Ctrl Pts',(-9.02732142156539,9.22723674108767,
11.6664736264289));
#120583=CARTESIAN_POINT('Ctrl Pts',(-9.06042413937132,9.22312255442211,
11.7123809878747));
#120584=CARTESIAN_POINT('Ctrl Pts',(-9.14301221338996,9.21368443866707,
11.8110968882251));
#120585=CARTESIAN_POINT('Ctrl Pts',(-9.1943296466672,9.20835758239048,11.8620923834961));
#120586=CARTESIAN_POINT('Ctrl Pts',(-9.25790848101028,9.20257338460449,
11.9146040155316));
#120587=CARTESIAN_POINT('Ctrl Pts',(-9.26590445004343,9.2018594328693,11.9210342388325));
#120588=CARTESIAN_POINT('Ctrl Pts',(-9.27753084952769,9.20084174649476,
11.930136378442));
#120589=CARTESIAN_POINT('Ctrl Pts',(-9.28109391655605,9.20053257046305,
11.9328930274934));
#120590=CARTESIAN_POINT('Ctrl Pts',(-9.28738465713871,9.19999157366911,
11.9377025587014));
#120591=CARTESIAN_POINT('Ctrl Pts',(-9.29010556524019,9.1997591656601,11.9397641236829));
#120592=CARTESIAN_POINT('Ctrl Pts',(-9.29593909032316,9.19926430700382,
11.944144247833));
#120593=CARTESIAN_POINT('Ctrl Pts',(-9.29905423478611,9.19900209371778,
11.9464592757051));
#120594=CARTESIAN_POINT('Ctrl Pts',(-9.30770867270555,9.19827908156675,
11.952824678683));
#120595=CARTESIAN_POINT('Ctrl Pts',(-9.31327211390171,9.19782044641249,
11.9568421845638));
#120596=CARTESIAN_POINT('Ctrl Pts',(-9.34646771233953,9.19511803832189,
11.9803749105727));
#120597=CARTESIAN_POINT('Ctrl Pts',(-9.37489793246477,9.19294248760269,
11.9987428565288));
#120598=CARTESIAN_POINT('Ctrl Pts',(-9.50352620213314,9.18351288866872,
12.0741977795012));
#120599=CARTESIAN_POINT('Ctrl Pts',(-9.61099325259078,9.17662943643949,
12.1176148326397));
#120600=CARTESIAN_POINT('Ctrl Pts',(-9.74237888128779,9.16789052438256,
12.1494004825394));
#120601=CARTESIAN_POINT('Ctrl Pts',(-9.76181162144749,9.16659228391543,
12.1535841245591));
#120602=CARTESIAN_POINT('Ctrl Pts',(-9.78898579577522,9.16476446451009,
12.1587185217358));
#120603=CARTESIAN_POINT('Ctrl Pts',(-9.79664552326458,9.16424789895686,
12.160087306621));
#120604=CARTESIAN_POINT('Ctrl Pts',(-9.80993083688772,9.16334935247259,
12.162325760217));
#120605=CARTESIAN_POINT('Ctrl Pts',(-9.81555026832102,9.16296848411211,
12.1632307398739));
#120606=CARTESIAN_POINT('Ctrl Pts',(-9.82726513249515,9.16217271205424,
12.1650303348333));
#120607=CARTESIAN_POINT('Ctrl Pts',(-9.83336145262615,9.16175760201808,
12.1659179248929));
#120608=CARTESIAN_POINT('Ctrl Pts',(-9.84781736586806,9.16077077815284,
12.1679069320824));
#120609=CARTESIAN_POINT('Ctrl Pts',(-9.85618228128259,9.16019778146712,
12.168966472367));
#120610=CARTESIAN_POINT('Ctrl Pts',(-9.88451407831968,9.15824999734675,
12.1722464162348));
#120611=CARTESIAN_POINT('Ctrl Pts',(-9.90452520127499,9.15686235036861,
12.1740456275925));
#120612=CARTESIAN_POINT('Ctrl Pts',(-9.95318512760633,9.15345724902068,
12.1771684417553));
#120613=CARTESIAN_POINT('Ctrl Pts',(-9.9818541237806,9.15142503813535,12.1779591148728));
#120614=CARTESIAN_POINT('Ctrl Pts',(-10.0957748296821,9.14325183143161,
12.1769413524686));
#120615=CARTESIAN_POINT('Ctrl Pts',(-10.1806910440417,9.13691853979815,
12.1669243253631));
#120616=CARTESIAN_POINT('Ctrl Pts',(-10.2977059408063,9.12820794110521,
12.1400345203897));
#120617=CARTESIAN_POINT('Ctrl Pts',(-10.3312830901864,9.12571417624412,
12.1307340724643));
#120618=CARTESIAN_POINT('Ctrl Pts',(-10.3711536785797,9.12279631489549,
12.1177613447877));
#120619=CARTESIAN_POINT('Ctrl Pts',(-10.3778857917778,9.12230517062908,
12.1155033893213));
#120620=CARTESIAN_POINT('Ctrl Pts',(-10.3883545561332,9.12154425509543,
12.111886506565));
#120621=CARTESIAN_POINT('Ctrl Pts',(-10.3921053097964,9.12127220597862,
12.1105693548588));
#120622=CARTESIAN_POINT('Ctrl Pts',(-10.3990485585029,9.12076975484328,
12.1080915343766));
#120623=CARTESIAN_POINT('Ctrl Pts',(-10.4022427051574,9.12053907571623,
12.1069360447636));
#120624=CARTESIAN_POINT('Ctrl Pts',(-10.40959222389,9.12000932903487,12.1042413266143));
#120625=CARTESIAN_POINT('Ctrl Pts',(-10.4137439538197,9.11971082769298,
12.1026924501138));
#120626=CARTESIAN_POINT('Ctrl Pts',(-10.4268491618685,9.11877067259253,
12.0977188828527));
#120627=CARTESIAN_POINT('Ctrl Pts',(-10.4357698904588,9.11813379727521,
12.0942081930582));
#120628=CARTESIAN_POINT('Ctrl Pts',(-10.4824230609412,9.11481439641758,
12.0751870949907));
#120629=CARTESIAN_POINT('Ctrl Pts',(-10.5193774715623,9.11222375407902,
12.0578312965337));
#120630=CARTESIAN_POINT('Ctrl Pts',(-10.6199467083064,9.10508549124594,
12.0040544452816));
#120631=CARTESIAN_POINT('Ctrl Pts',(-10.6811708359302,9.10062669633543,
11.9635693210663));
#120632=CARTESIAN_POINT('Ctrl Pts',(-10.7729458945962,9.0932213028762,11.8897380979666));
#120633=CARTESIAN_POINT('Ctrl Pts',(-10.8060375073712,9.09037537518844,
11.8598733036482));
#120634=CARTESIAN_POINT('Ctrl Pts',(-10.8453921815564,9.08670119636175,
11.8200839666402));
#120635=CARTESIAN_POINT('Ctrl Pts',(-10.8533093116708,9.08594613614795,
11.8118428768242));
#120636=CARTESIAN_POINT('Ctrl Pts',(-10.8657303098235,9.08473497601275,
11.798531187456));
#120637=CARTESIAN_POINT('Ctrl Pts',(-10.8703125982674,9.08428220308995,
11.793534501295));
#120638=CARTESIAN_POINT('Ctrl Pts',(-10.8789059294,9.08342154344041,11.7840000674971));
#120639=CARTESIAN_POINT('Ctrl Pts',(-10.8829256228384,9.08301403556718,
11.7794703847859));
#120640=CARTESIAN_POINT('Ctrl Pts',(-10.8919805392111,9.08208466843235,
11.7691067329858));
#120641=CARTESIAN_POINT('Ctrl Pts',(-10.8969937519922,9.0815619334867,11.7632539898746));
#120642=CARTESIAN_POINT('Ctrl Pts',(-10.9122105214732,9.07994951831467,
11.7451319800931));
#120643=CARTESIAN_POINT('Ctrl Pts',(-10.9222220894851,9.07885226963748,
11.7327046319635));
#120644=CARTESIAN_POINT('Ctrl Pts',(-10.9448874849234,9.07628032012166,
11.7033694267971));
#120645=CARTESIAN_POINT('Ctrl Pts',(-10.9573448794097,9.07479870840918,
11.6863174170388));
#120646=CARTESIAN_POINT('Ctrl Pts',(-11.0012854501578,9.069314201956,11.622644799856));
#120647=CARTESIAN_POINT('Ctrl Pts',(-11.0298733643898,9.06522128825756,
11.5741243109414));
#120648=CARTESIAN_POINT('Ctrl Pts',(-11.0871772524861,9.05577279194797,
11.4587092898304));
#120649=CARTESIAN_POINT('Ctrl Pts',(-11.1133890861886,9.05041288245019,
11.3908133955653));
#120650=CARTESIAN_POINT('Ctrl Pts',(-11.1356975369001,9.04467060412752,
11.3120440255709));
#120651=CARTESIAN_POINT('Ctrl Pts',(-11.1381098155511,9.04402741239055,
11.3031277450942));
#120652=CARTESIAN_POINT('Ctrl Pts',(-11.1415318320646,9.0430814385073,11.2898621351395));
#120653=CARTESIAN_POINT('Ctrl Pts',(-11.1426220732322,9.04277453331848,
11.2855342017552));
#120654=CARTESIAN_POINT('Ctrl Pts',(-11.1444509633795,9.04225012659281,
11.2780958001991));
#120655=CARTESIAN_POINT('Ctrl Pts',(-11.1452015887949,9.0420319693341,11.2749883694095));
#120656=CARTESIAN_POINT('Ctrl Pts',(-11.1467523307558,9.04157507176851,
11.2684521384904));
#120657=CARTESIAN_POINT('Ctrl Pts',(-11.1475497398003,9.04133649510714,
11.2650227423568));
#120658=CARTESIAN_POINT('Ctrl Pts',(-11.1494882969301,9.04074719970246,
11.2565128276514));
#120659=CARTESIAN_POINT('Ctrl Pts',(-11.1506111714546,9.04039749437796,
11.2514281411649));
#120660=CARTESIAN_POINT('Ctrl Pts',(-11.1547225321603,9.0390839501421,11.232206207273));
#120661=CARTESIAN_POINT('Ctrl Pts',(-11.1574846318216,9.03813184777235,
11.2180211506746));
#120662=CARTESIAN_POINT('Ctrl Pts',(-11.1639590271024,9.03569431613876,
11.1811681515621));
#120663=CARTESIAN_POINT('Ctrl Pts',(-11.1672706957847,9.03422573141662,
11.1584353796791));
#120664=CARTESIAN_POINT('Ctrl Pts',(-11.183742724702,9.02518357582828,11.0163395930413));
#120665=CARTESIAN_POINT('Ctrl Pts',(-11.179248647086,9.01802501140546,10.8956516867982));
#120666=CARTESIAN_POINT('Ctrl Pts',(-11.1534124868851,9.00912652773981,
10.761217268834));
#120667=CARTESIAN_POINT('Ctrl Pts',(-11.1498875617642,9.00802411922803,
10.7447822360053));
#120668=CARTESIAN_POINT('Ctrl Pts',(-11.1442182103416,9.00639528232526,
10.720857943403));
#120669=CARTESIAN_POINT('Ctrl Pts',(-11.1423491737566,9.00587752541123,
10.7133051081505));
#120670=CARTESIAN_POINT('Ctrl Pts',(-11.138886357589,9.00495087840997,10.6998835176293));
#120671=CARTESIAN_POINT('Ctrl Pts',(-11.1373216871211,9.00454292749327,
10.6940074900681));
#120672=CARTESIAN_POINT('Ctrl Pts',(-11.1339456821418,9.0036844771404,10.6817128180174));
#120673=CARTESIAN_POINT('Ctrl Pts',(-11.1321251943536,9.00323369718965,
10.6752969334643));
#120674=CARTESIAN_POINT('Ctrl Pts',(-11.127181125936,9.00204032905196,10.6584199057474));
#120675=CARTESIAN_POINT('Ctrl Pts',(-11.1239664688353,9.00129483999836,
10.6479863433264));
#120676=CARTESIAN_POINT('Ctrl Pts',(-11.107550429658,8.99762885606164,10.5972250383851));
#120677=CARTESIAN_POINT('Ctrl Pts',(-11.0923227126164,8.99464359061973,
10.5575907389631));
#120678=CARTESIAN_POINT('Ctrl Pts',(-11.0310224673367,8.98388645580076,
10.4206277431398));
#120679=CARTESIAN_POINT('Ctrl Pts',(-10.9738006948832,8.97580669306645,
10.3288900123771));
#120680=CARTESIAN_POINT('Ctrl Pts',(-10.89444504035,8.96700241641876,10.2336246848445));
#120681=CARTESIAN_POINT('Ctrl Pts',(-10.8837056679637,8.96585233314149,
10.2212655059318));
#120682=CARTESIAN_POINT('Ctrl Pts',(-10.8689239135409,8.96432817388114,
10.2049540209413));
#120683=CARTESIAN_POINT('Ctrl Pts',(-10.865106294658,8.96393961009118,10.2008016651149));
#120684=CARTESIAN_POINT('Ctrl Pts',(-10.8590392579699,8.9633302595825,10.1942970735888));
#120685=CARTESIAN_POINT('Ctrl Pts',(-10.8568097312952,8.96310804387674,
10.1919265272448));
#120686=CARTESIAN_POINT('Ctrl Pts',(-10.8521807447933,8.96265025083665,
10.1870454500707));
#120687=CARTESIAN_POINT('Ctrl Pts',(-10.8497799757864,8.96241479143939,
10.1845362576202));
#120688=CARTESIAN_POINT('Ctrl Pts',(-10.8439253374822,8.96184524823,10.1784711445967));
#120689=CARTESIAN_POINT('Ctrl Pts',(-10.8404599976609,8.96151202830936,
10.1749262881278));
#120690=CARTESIAN_POINT('Ctrl Pts',(-10.8280262101665,8.96032973168817,
10.1623668171171));
#120691=CARTESIAN_POINT('Ctrl Pts',(-10.8189339106631,8.95948957535603,
10.1534753187875));
#120692=CARTESIAN_POINT('Ctrl Pts',(-10.7957378982657,8.95740094120697,
10.131515190174));
#120693=CARTESIAN_POINT('Ctrl Pts',(-10.7814545148012,8.95616385566662,
10.1186410536026));
#120694=CARTESIAN_POINT('Ctrl Pts',(-10.7124677317738,8.95037986688048,
10.0594570327741));
#120695=CARTESIAN_POINT('Ctrl Pts',(-10.6539249173861,8.94601280985897,
10.0178519062093));
#120696=CARTESIAN_POINT('Ctrl Pts',(-10.5385745927734,8.93771675750475,
9.95078803646274));
#120697=CARTESIAN_POINT('Ctrl Pts',(-10.4828383023102,8.93382430986824,
9.9240009086476));
#120698=CARTESIAN_POINT('Ctrl Pts',(-10.4139821795683,8.92898486131499,
9.89733950191145));
#120699=CARTESIAN_POINT('Ctrl Pts',(-10.4026342940805,8.92818660108786,
9.89314543563708));
#120700=CARTESIAN_POINT('Ctrl Pts',(-10.3846268725791,8.92691779300244,
9.88680363202755));
#120701=CARTESIAN_POINT('Ctrl Pts',(-10.3780091533756,8.92645106949463,
9.88453908127923));
#120702=CARTESIAN_POINT('Ctrl Pts',(-10.365649144957,8.92557836217799,9.8804321684641));
#120703=CARTESIAN_POINT('Ctrl Pts',(-10.3599120896341,8.92517288573222,
9.87857469618404));
#120704=CARTESIAN_POINT('Ctrl Pts',(-10.3471112000983,8.92426715143396,
9.87453853035606));
#120705=CARTESIAN_POINT('Ctrl Pts',(-10.3400406589412,8.9237661911404,9.87238213438821));
#120706=CARTESIAN_POINT('Ctrl Pts',(-10.3191873207458,8.92228644900763,
9.86623618273146));
#120707=CARTESIAN_POINT('Ctrl Pts',(-10.3053517942695,8.9213018002051,9.86243189683846));
#120708=CARTESIAN_POINT('Ctrl Pts',(-10.2421166925899,8.9167865152561,9.84628114990267));
#120709=CARTESIAN_POINT('Ctrl Pts',(-10.19202410238,8.91316507363937,9.83689502458227));
#120710=CARTESIAN_POINT('Ctrl Pts',(-10.0596815728429,8.90350742160279,
9.8208802736158));
#120711=CARTESIAN_POINT('Ctrl Pts',(-9.97706707226339,8.89737694700525,
9.81959384092877));
#120712=CARTESIAN_POINT('Ctrl Pts',(-9.86991334781599,8.88964401660275,
9.82918544241997));
#120713=CARTESIAN_POINT('Ctrl Pts',(-9.84490652880269,8.88785690149479,
9.83223482927368));
#120714=CARTESIAN_POINT('Ctrl Pts',(-9.81705786206104,8.88589957251103,
9.83654128177284));
#120715=CARTESIAN_POINT('Ctrl Pts',(-9.8141026859178,8.88569228767676,9.83700980064966));
#120716=CARTESIAN_POINT('Ctrl Pts',(-9.81114930149677,8.88548556788545,
9.83748958018655));
#120717=CARTESIAN_POINT('Ctrl Pts',(-9.81114930181833,8.78721751211607,
9.83748958013431));
#120718=CARTESIAN_POINT('Ctrl Pts',(-9.81217914363668,8.78729284169822,
9.83732228155093));
#120719=CARTESIAN_POINT('Ctrl Pts',(-9.81320922699522,8.78736820014809,
9.83715634831394));
#120720=CARTESIAN_POINT('Ctrl Pts',(-9.88853221837043,8.79287945254868,
9.82512545067859));
#120721=CARTESIAN_POINT('Ctrl Pts',(-9.96378569904865,8.79845834619609,
9.82040565303448));
#120722=CARTESIAN_POINT('Ctrl Pts',(-10.0741778762675,8.80647428336804,
9.82406059275664));
#120723=CARTESIAN_POINT('Ctrl Pts',(-10.1093171190298,8.80899797592169,
9.82680516450662));
#120724=CARTESIAN_POINT('Ctrl Pts',(-10.1513650234862,8.81194670009575,
9.83199546181664));
#120725=CARTESIAN_POINT('Ctrl Pts',(-10.1584384678307,8.81244028765832,
9.83293392229028));
#120726=CARTESIAN_POINT('Ctrl Pts',(-10.1694459948495,8.8132041202846,9.83449625635932));
#120727=CARTESIAN_POINT('Ctrl Pts',(-10.173386038307,8.81347667104483,9.83507588036449));
#120728=CARTESIAN_POINT('Ctrl Pts',(-10.1806791570613,8.81397948894335,
9.83618660052427));
#120729=CARTESIAN_POINT('Ctrl Pts',(-10.1840328817114,8.81421003820732,
9.83671220864987));
#120730=CARTESIAN_POINT('Ctrl Pts',(-10.1917458539907,8.81473876154773,
9.83795520478042));
#120731=CARTESIAN_POINT('Ctrl Pts',(-10.1961033845614,8.81503637667364,
9.83868262617167));
#120732=CARTESIAN_POINT('Ctrl Pts',(-10.2098356857319,8.81597112327116,
9.84105451590009));
#120733=CARTESIAN_POINT('Ctrl Pts',(-10.2191949504863,8.81660355255421,
9.84278816202906));
#120734=CARTESIAN_POINT('Ctrl Pts',(-10.2886398676579,8.82126842151982,
9.85652444856068));
#120735=CARTESIAN_POINT('Ctrl Pts',(-10.3477361577329,8.82508622012151,
9.87308790482921));
#120736=CARTESIAN_POINT('Ctrl Pts',(-10.490507686336,8.834506616183,9.92541336061975));
#120737=CARTESIAN_POINT('Ctrl Pts',(-10.57182759508,8.84007346692032,9.96639204573868));
#120738=CARTESIAN_POINT('Ctrl Pts',(-10.6604605161511,8.84698827101984,
10.0247447263933));
#120739=CARTESIAN_POINT('Ctrl Pts',(-10.6731214674889,8.84799742012946,
10.0334399155894));
#120740=CARTESIAN_POINT('Ctrl Pts',(-10.691779799166,8.84951903384249,10.0467983518149));
#120741=CARTESIAN_POINT('Ctrl Pts',(-10.6979083017919,8.85002452518385,
10.0512762939512));
#120742=CARTESIAN_POINT('Ctrl Pts',(-10.708837657432,8.85093655759052,10.0594253049012));
#120743=CARTESIAN_POINT('Ctrl Pts',(-10.7136543864796,8.85134225617695,
10.0630747116284));
#120744=CARTESIAN_POINT('Ctrl Pts',(-10.7238692363989,8.8522107973207,10.0709384898572));
#120745=CARTESIAN_POINT('Ctrl Pts',(-10.7292590903946,8.85267403317879,
10.0751631837498));
#120746=CARTESIAN_POINT('Ctrl Pts',(-10.7437964615153,8.85393719183602,
10.0867640135112));
#120747=CARTESIAN_POINT('Ctrl Pts',(-10.7528707186633,8.85474065505843,
10.0942302683194));
#120748=CARTESIAN_POINT('Ctrl Pts',(-10.8051857487542,8.85946293365098,
10.1386041311387));
#120749=CARTESIAN_POINT('Ctrl Pts',(-10.8458140074639,8.86350173378712,
10.1784625078228));
#120750=CARTESIAN_POINT('Ctrl Pts',(-10.9386581686194,8.87368125311974,
10.2837621182961));
#120751=CARTESIAN_POINT('Ctrl Pts',(-10.9870871983317,8.87990034135288,
10.3521309480626));
#120752=CARTESIAN_POINT('Ctrl Pts',(-11.0390812993549,8.887535395673,10.4450836393841));
#120753=CARTESIAN_POINT('Ctrl Pts',(-11.0497013912911,8.88916074056652,
10.4654447926757));
#120754=CARTESIAN_POINT('Ctrl Pts',(-11.0624977128322,8.89119645197451,
10.4918325153381));
#120755=CARTESIAN_POINT('Ctrl Pts',(-11.0652288145833,8.89163585668405,
10.4975826840628));
#120756=CARTESIAN_POINT('Ctrl Pts',(-11.0695037580035,8.892331304407,10.5067748987938));
#120757=CARTESIAN_POINT('Ctrl Pts',(-11.0710778701415,8.89258909784036,
10.5102026072492));
#120758=CARTESIAN_POINT('Ctrl Pts',(-11.07405838785,8.89308045723284,10.5167759175706));
#120759=CARTESIAN_POINT('Ctrl Pts',(-11.0754674816029,8.89331417324166,
10.5199201830323));
#120760=CARTESIAN_POINT('Ctrl Pts',(-11.0788085483953,8.89387184412986,
10.5274640053804));
#120761=CARTESIAN_POINT('Ctrl Pts',(-11.080727459549,8.89419502332695,10.5318693446502));
#120762=CARTESIAN_POINT('Ctrl Pts',(-11.0872454870586,8.89530327469764,
10.5470868043181));
#120763=CARTESIAN_POINT('Ctrl Pts',(-11.0917099141055,8.89608083444063,
10.5579563357465));
#120764=CARTESIAN_POINT('Ctrl Pts',(-11.1023309611704,8.89798231240072,
10.5849583130967));
#120765=CARTESIAN_POINT('Ctrl Pts',(-11.1082970667748,8.89909728313716,
10.6011631601668));
#120766=CARTESIAN_POINT('Ctrl Pts',(-11.1326041233348,8.90387890045194,
10.6719483590693));
#120767=CARTESIAN_POINT('Ctrl Pts',(-11.1472863828311,8.90742236888328,
10.7277044038575));
#120768=CARTESIAN_POINT('Ctrl Pts',(-11.1711486005192,8.91548468030999,
10.8558001469946));
#120769=CARTESIAN_POINT('Ctrl Pts',(-11.1778150171182,8.92000420582508,
10.9283570916866));
#120770=CARTESIAN_POINT('Ctrl Pts',(-11.1777349892736,8.92578529644395,
11.0171934049905));
#120771=CARTESIAN_POINT('Ctrl Pts',(-11.177388994329,8.92684428617756,11.0333231668098));
#120772=CARTESIAN_POINT('Ctrl Pts',(-11.1763870004886,8.92842623555848,
11.0571713668401));
#120773=CARTESIAN_POINT('Ctrl Pts',(-11.1759859894112,8.9289413618942,11.0648990604175));
#120774=CARTESIAN_POINT('Ctrl Pts',(-11.1751353144204,8.92986398440066,
11.0786686447434));
#120775=CARTESIAN_POINT('Ctrl Pts',(-11.174715121116,8.93027055621383,11.0847121286903));
#120776=CARTESIAN_POINT('Ctrl Pts',(-11.1737275778251,8.93113376175845,
11.0974900395759));
#120777=CARTESIAN_POINT('Ctrl Pts',(-11.173148851033,8.93159073364153,11.1042233409543));
#120778=CARTESIAN_POINT('Ctrl Pts',(-11.1714445329448,8.93281891897082,
11.1222342712521));
#120779=CARTESIAN_POINT('Ctrl Pts',(-11.1702140716586,8.93359334653481,
11.1335010178738));
#120780=CARTESIAN_POINT('Ctrl Pts',(-11.1628316821674,8.93772465065677,
11.1931128841886));
#120781=CARTESIAN_POINT('Ctrl Pts',(-11.1538468086768,8.94116825021961,
11.2410529378607));
#120782=CARTESIAN_POINT('Ctrl Pts',(-11.1296209295448,8.94830194390495,
11.3370107767009));
#120783=CARTESIAN_POINT('Ctrl Pts',(-11.1142172343292,8.95198927789017,
11.3848884305607));
#120784=CARTESIAN_POINT('Ctrl Pts',(-11.0885814999662,8.9571218461473,11.4499709215877));
#120785=CARTESIAN_POINT('Ctrl Pts',(-11.0808990260695,8.95856668779901,
11.4681248023011));
#120786=CARTESIAN_POINT('Ctrl Pts',(-11.0548603356207,8.96316956290856,
11.5255917255573));
#120787=CARTESIAN_POINT('Ctrl Pts',(-11.0347845379642,8.96629876578241,
11.5640911175499));
#120788=CARTESIAN_POINT('Ctrl Pts',(-11.0088492644349,8.9698365090596,11.6077606250268));
#120789=CARTESIAN_POINT('Ctrl Pts',(-11.0050108171361,8.97034870365302,
11.6140871925809));
#120790=CARTESIAN_POINT('Ctrl Pts',(-10.9989840952081,8.97113506074841,
11.6238126102224));
#120791=CARTESIAN_POINT('Ctrl Pts',(-10.9968376054625,8.97141174294187,
11.6272369446348));
#120792=CARTESIAN_POINT('Ctrl Pts',(-10.9928590160677,8.97191830728661,
11.6335120512491));
#120793=CARTESIAN_POINT('Ctrl Pts',(-10.9910322304903,8.9721485080222,11.6363659823849));
#120794=CARTESIAN_POINT('Ctrl Pts',(-10.9868389296037,8.97267154383687,
11.6428551964744));
#120795=CARTESIAN_POINT('Ctrl Pts',(-10.9844646271373,8.97296386591053,
11.6464853254508));
#120796=CARTESIAN_POINT('Ctrl Pts',(-10.9770508895488,8.97386516039381,
11.6576848105663));
#120797=CARTESIAN_POINT('Ctrl Pts',(-10.9719436663379,8.97446989501998,
11.6652091946876));
#120798=CARTESIAN_POINT('Ctrl Pts',(-10.9273617054979,8.97961943163362,
11.7292812366038));
#120799=CARTESIAN_POINT('Ctrl Pts',(-10.8830721135756,8.98388803988168,
11.782328060993));
#120800=CARTESIAN_POINT('Ctrl Pts',(-10.7758658888013,8.99328681619203,
11.8899456242137));
#120801=CARTESIAN_POINT('Ctrl Pts',(-10.7113105864744,8.99840182432431,
11.9423408921894));
#120802=CARTESIAN_POINT('Ctrl Pts',(-10.6284895198859,9.00483260099497,
11.9961664983533));
#120803=CARTESIAN_POINT('Ctrl Pts',(-10.6150140089508,9.00587439486937,
12.0045419349325));
#120804=CARTESIAN_POINT('Ctrl Pts',(-10.5947641559801,9.00743555144133,
12.0165676360184));
#120805=CARTESIAN_POINT('Ctrl Pts',(-10.5881162379497,9.00794738303571,
12.0204280698899));
#120806=CARTESIAN_POINT('Ctrl Pts',(-10.5761675167285,9.00886635981372,
12.0272111220553));
#120807=CARTESIAN_POINT('Ctrl Pts',(-10.5708810300333,9.00927260865949,
12.0301585042232));
#120808=CARTESIAN_POINT('Ctrl Pts',(-10.5596184156277,9.01013752015906,
12.0363244484792));
#120809=CARTESIAN_POINT('Ctrl Pts',(-10.553636732481,9.01059653919139,12.0395323461756));
#120810=CARTESIAN_POINT('Ctrl Pts',(-10.5374734492557,9.01183613629482,
12.0480214244391));
#120811=CARTESIAN_POINT('Ctrl Pts',(-10.5272420975913,9.01262003350744,
12.0532057582191));
#120812=CARTESIAN_POINT('Ctrl Pts',(-10.4709985435536,9.01692645603221,
12.0806800371523));
#120813=CARTESIAN_POINT('Ctrl Pts',(-10.4236541475633,9.02054491464231,
12.1001021948276));
#120814=CARTESIAN_POINT('Ctrl Pts',(-10.309276901016,9.02925880599954,12.1385429850584));
#120815=CARTESIAN_POINT('Ctrl Pts',(-10.2415186556002,9.03440446895688,
12.1548160630736));
#120816=CARTESIAN_POINT('Ctrl Pts',(-10.1601725931716,9.04039695468296,
12.1668765471568));
#120817=CARTESIAN_POINT('Ctrl Pts',(-10.1475887837073,9.04131846547583,
12.1685348527222));
#120818=CARTESIAN_POINT('Ctrl Pts',(-10.1056473190783,9.04436723267493,
12.1733735915057));
#120819=CARTESIAN_POINT('Ctrl Pts',(-10.0761945526865,9.04647166606036,
12.1756537142102));
#120820=CARTESIAN_POINT('Ctrl Pts',(-10.0398888750311,9.04899793501454,
12.1770939621699));
#120821=CARTESIAN_POINT('Ctrl Pts',(-10.0330906607521,9.04946804853283,
12.1773046894365));
#120822=CARTESIAN_POINT('Ctrl Pts',(-10.0223849300082,9.05020337792364,
12.1775437320413));
#120823=CARTESIAN_POINT('Ctrl Pts',(-10.0184785741322,9.05047064086738,
12.1776115103777));
#120824=CARTESIAN_POINT('Ctrl Pts',(-10.0115070684675,9.0509456597272,12.1776977729446));
#120825=CARTESIAN_POINT('Ctrl Pts',(-10.0084421776964,9.05115381097372,
12.1777237311734));
#120826=CARTESIAN_POINT('Ctrl Pts',(-10.0010400613329,9.05165491560924,
12.177757526471));
#120827=CARTESIAN_POINT('Ctrl Pts',(-9.99670284998123,9.05194720930854,
12.1777533711183));
#120828=CARTESIAN_POINT('Ctrl Pts',(-9.98327479863973,9.0528483264862,12.1776663269543));
#120829=CARTESIAN_POINT('Ctrl Pts',(-9.97418456748794,9.05345291457749,
12.1775021383639));
#120830=CARTESIAN_POINT('Ctrl Pts',(-9.89642719078224,9.05858501960186,
12.1751967484587));
#120831=CARTESIAN_POINT('Ctrl Pts',(-9.82805717397522,9.06283844932961,
12.1671559717956));
#120832=CARTESIAN_POINT('Ctrl Pts',(-9.67929824221765,9.07223888232213,
12.1362961018654));
#120833=CARTESIAN_POINT('Ctrl Pts',(-9.59985616958305,9.07737038382616,
12.1108111339311));
#120834=CARTESIAN_POINT('Ctrl Pts',(-9.50926675535917,9.0838190652842,12.0707601354034));
#120835=CARTESIAN_POINT('Ctrl Pts',(-9.49489895759711,9.08486007962245,
12.064057932262));
#120836=CARTESIAN_POINT('Ctrl Pts',(-9.47377365672992,9.08642029299866,
12.0536792491373));
#120837=CARTESIAN_POINT('Ctrl Pts',(-9.46690944300894,9.08693197449629,
12.0502231085752));
#120838=CARTESIAN_POINT('Ctrl Pts',(-9.45470076372537,9.08785078576587,
12.0439254938016));
#120839=CARTESIAN_POINT('Ctrl Pts',(-9.44934340405423,9.08825702047573,
12.0411095065844));
#120840=CARTESIAN_POINT('Ctrl Pts',(-9.43802323661951,9.08912201250749,
12.0350474721965));
#120841=CARTESIAN_POINT('Ctrl Pts',(-9.43206633614897,9.08958112705322,
12.0317909199131));
#120842=CARTESIAN_POINT('Ctrl Pts',(-9.4161165051537,9.09082125697064,12.0228914043181));
#120843=CARTESIAN_POINT('Ctrl Pts',(-9.4061775645365,9.09160559642151,12.0171537049903));
#120844=CARTESIAN_POINT('Ctrl Pts',(-9.35232447110803,9.09592055355682,
11.9850062652558));
#120845=CARTESIAN_POINT('Ctrl Pts',(-9.31009185543225,9.09954756707406,
11.9559008222945));
#120846=CARTESIAN_POINT('Ctrl Pts',(-9.21454110197612,9.10834226466559,
11.8804121310864));
#120847=CARTESIAN_POINT('Ctrl Pts',(-9.16323137527353,9.11356340557285,
11.8317983703183));
#120848=CARTESIAN_POINT('Ctrl Pts',(-9.09003100777206,9.1216238726878,11.7487746871832));
#120849=CARTESIAN_POINT('Ctrl Pts',(-9.06503253792432,9.12451260256411,
11.7173169748328));
#120850=CARTESIAN_POINT('Ctrl Pts',(-9.03742029580544,9.12782058198034,
11.6786672715583));
#120851=CARTESIAN_POINT('Ctrl Pts',(-9.03320870139038,9.12832865533921,
11.6726541043924));
#120852=CARTESIAN_POINT('Ctrl Pts',(-9.02677343916909,9.12911002906179,
11.6632807486305));
#120853=CARTESIAN_POINT('Ctrl Pts',(-9.0245104125778,9.12938580103322,11.6599479951163));
#120854=CARTESIAN_POINT('Ctrl Pts',(-9.02037471234452,9.1298915248187,11.6537896055271));
#120855=CARTESIAN_POINT('Ctrl Pts',(-9.0184971276118,9.13012178723625,11.6509674834636));
#120856=CARTESIAN_POINT('Ctrl Pts',(-9.01423536889355,9.13064600869969,
11.6445014471614));
#120857=CARTESIAN_POINT('Ctrl Pts',(-9.01185919538046,9.13093944504688,
11.6408523816671));
#120858=CARTESIAN_POINT('Ctrl Pts',(-9.00453574923229,9.1318477191234,11.6294682611041));
#120859=CARTESIAN_POINT('Ctrl Pts',(-8.99965851150791,9.1324582241955,11.6216882542368));
#120860=CARTESIAN_POINT('Ctrl Pts',(-8.98838345538847,9.13388502870457,
11.6032263555899));
#120861=CARTESIAN_POINT('Ctrl Pts',(-8.98206294536905,9.13469715239179,
11.5924983111881));
#120862=CARTESIAN_POINT('Ctrl Pts',(-8.95964337146803,9.13763143703435,
11.5530265832466));
#120863=CARTESIAN_POINT('Ctrl Pts',(-8.94458108286684,9.13970877253897,
11.5237094000783));
#120864=CARTESIAN_POINT('Ctrl Pts',(-8.89856897859478,9.14655858600484,
11.4240781093049));
#120865=CARTESIAN_POINT('Ctrl Pts',(-8.87326777545926,9.1512335043338,11.3513787597083));
#120866=CARTESIAN_POINT('Ctrl Pts',(-8.84632791663282,9.15848474035216,
11.2399354704662));
#120867=CARTESIAN_POINT('Ctrl Pts',(-8.83921268181324,9.16091634912756,
11.2027329897751));
#120868=CARTESIAN_POINT('Ctrl Pts',(-8.83236085205739,9.16412539061146,
11.154384053541));
#120869=CARTESIAN_POINT('Ctrl Pts',(-8.83097238584885,9.16485138825542,
11.1434922989329));
#120870=CARTESIAN_POINT('Ctrl Pts',(-8.82898428312476,9.1660267721978,11.1259440168871));
#120871=CARTESIAN_POINT('Ctrl Pts',(-8.82828865127806,9.1664731714854,11.1192988546944));
#120872=CARTESIAN_POINT('Ctrl Pts',(-8.82706852245927,9.16732884364298,
11.1066007565577));
#120873=CARTESIAN_POINT('Ctrl Pts',(-8.82653424564735,9.16773779882173,
11.1005489596915));
#120874=CARTESIAN_POINT('Ctrl Pts',(-8.82541446984163,9.16868066168069,
11.0866372534615));
#120875=CARTESIAN_POINT('Ctrl Pts',(-8.82486100618216,9.16921554265581,
11.0787751314072));
#120876=CARTESIAN_POINT('Ctrl Pts',(-8.8233687001217,9.17090545739777,11.0540336357764));
#120877=CARTESIAN_POINT('Ctrl Pts',(-8.82271438232854,9.1720691565603,11.0371399080642));
#120878=CARTESIAN_POINT('Ctrl Pts',(-8.82203258342463,9.17482616255882,
10.9974698286009));
#120879=CARTESIAN_POINT('Ctrl Pts',(-8.8223017294407,9.1764278383377,10.9746958016619));
#120880=CARTESIAN_POINT('Ctrl Pts',(-8.82791819165112,9.18621444235574,
10.8371597071616));
#120881=CARTESIAN_POINT('Ctrl Pts',(-8.84937208907464,9.1948494406038,10.7236990689699));
#120882=CARTESIAN_POINT('Ctrl Pts',(-8.89287407362688,9.20433134877922,
10.5978791993898));
#120883=CARTESIAN_POINT('Ctrl Pts',(-8.89924652861694,9.20561813660484,
10.5807496693198));
#120884=CARTESIAN_POINT('Ctrl Pts',(-8.90819297292411,9.20729201244887,
10.5583134133446));
#120885=CARTESIAN_POINT('Ctrl Pts',(-8.91041140763523,9.20769729797516,
10.5528687796668));
#120886=CARTESIAN_POINT('Ctrl Pts',(-8.91407869166553,9.20835142407162,
10.5440576755381));
#120887=CARTESIAN_POINT('Ctrl Pts',(-8.91550261325906,9.20860168130448,
10.5406810365197));
#120888=CARTESIAN_POINT('Ctrl Pts',(-8.91831703917647,9.20908904429194,
10.5340930563904));
#120889=CARTESIAN_POINT('Ctrl Pts',(-8.91970612645554,9.20932622276822,
10.5308811930303));
#120890=CARTESIAN_POINT('Ctrl Pts',(-8.92315572034549,9.209907144738,10.5230015800378));
#120891=CARTESIAN_POINT('Ctrl Pts',(-8.92523231546658,9.21024993784047,
10.5183408654161));
#120892=CARTESIAN_POINT('Ctrl Pts',(-8.93299860294191,9.21150737760295,
10.5012105258155));
#120893=CARTESIAN_POINT('Ctrl Pts',(-8.93887580535044,9.21241153989564,
10.4888264442241));
#120894=CARTESIAN_POINT('Ctrl Pts',(-8.9544472459475,9.21469746671847,10.4574418308564));
#120895=CARTESIAN_POINT('Ctrl Pts',(-8.96444411629919,9.21606489826338,
10.4385963583646));
#120896=CARTESIAN_POINT('Ctrl Pts',(-9.00262635101331,9.22097970736207,
10.3711120106389));
#120897=CARTESIAN_POINT('Ctrl Pts',(-9.03377275714509,9.22443176304719,
10.324233839698));
#120898=CARTESIAN_POINT('Ctrl Pts',(-9.11319847588293,9.23247497086787,
10.2214727945865));
#120899=CARTESIAN_POINT('Ctrl Pts',(-9.16360986827574,9.23707643729784,
10.1675511771322));
#120900=CARTESIAN_POINT('Ctrl Pts',(-9.22782401362489,9.24270007268017,
10.1106253613136));
#120901=CARTESIAN_POINT('Ctrl Pts',(-9.2370497229487,9.24350255706174,10.1026985686418));
#120902=CARTESIAN_POINT('Ctrl Pts',(-9.25178173602707,9.24477651551689,
10.0904321891394));
#120903=CARTESIAN_POINT('Ctrl Pts',(-9.25720701603082,9.24524411094678,
10.0859963060825));
#120904=CARTESIAN_POINT('Ctrl Pts',(-9.26737167552583,9.24611749872227,
10.0778356261446));
#120905=CARTESIAN_POINT('Ctrl Pts',(-9.27210071086898,9.24652277504439,
10.0740982682803));
#120906=CARTESIAN_POINT('Ctrl Pts',(-9.28267589301659,9.24742684423489,
10.0658717884464));
#120907=CARTESIAN_POINT('Ctrl Pts',(-9.28853587268803,9.24792632851136,
10.0614009474974));
#120908=CARTESIAN_POINT('Ctrl Pts',(-9.3058460340239,9.24939771624038,10.0484494989833));
#120909=CARTESIAN_POINT('Ctrl Pts',(-9.31740825911904,9.25037538841595,
10.0401215863885));
#120910=CARTESIAN_POINT('Ctrl Pts',(-9.34410875904977,9.25262250546335,
10.0216164376162));
#120911=CARTESIAN_POINT('Ctrl Pts',(-9.35933779205176,9.25389667782512,
10.0115772219069));
#120912=CARTESIAN_POINT('Ctrl Pts',(-9.41217788882717,9.25829315417297,
9.97847846988859));
#120913=CARTESIAN_POINT('Ctrl Pts',(-9.45084518532322,9.26147075531366,
9.95718200696276));
#120914=CARTESIAN_POINT('Ctrl Pts',(-9.54778864323472,9.26930893028266,
9.91067848726169));
#120915=CARTESIAN_POINT('Ctrl Pts',(-9.60708604374026,9.27400087647328,
9.88791408701438));
#120916=CARTESIAN_POINT('Ctrl Pts',(-9.69863510623786,9.28090725149277,
9.86100981115744));
#120917=CARTESIAN_POINT('Ctrl Pts',(-9.72970082172079,9.28319361425112,
9.85324012855308));
#120918=CARTESIAN_POINT('Ctrl Pts',(-9.76785147060816,9.28590375011514,
9.84533537028877));
#120919=CARTESIAN_POINT('Ctrl Pts',(-9.77466819106758,9.28638423353661,
9.84398575765425));
#120920=CARTESIAN_POINT('Ctrl Pts',(-9.78536858929546,9.28713216592202,
9.84196548139005));
#120921=CARTESIAN_POINT('Ctrl Pts',(-9.7892442349903,9.28740177464927,9.84125386843765));
#120922=CARTESIAN_POINT('Ctrl Pts',(-9.79613558635934,9.28787879477103,
9.84002425664583));
#120923=CARTESIAN_POINT('Ctrl Pts',(-9.79914975141056,9.28808662216013,
9.83949855566299));
#120924=CARTESIAN_POINT('Ctrl Pts',(-9.80515848643411,9.28849933375342,
9.83847468308996));
#120925=CARTESIAN_POINT('Ctrl Pts',(-9.8081529288778,9.28870422647288,9.83797634318877));
#120926=CARTESIAN_POINT('Ctrl Pts',(-9.81114930150154,9.28890850071391,
9.83748958018578));
#120927=CARTESIAN_POINT('Origin',(-10.,2.67563288526385,11.));
#120928=CARTESIAN_POINT('',(-9.81114930121628,9.88702732255485,9.83748958023212));
#120929=CARTESIAN_POINT('',(-9.81114931871882,9.78720258982876,9.83748957738882));
#120930=CARTESIAN_POINT('',(-9.81114930150157,2.67563288526385,9.83748958018577));
#120931=CARTESIAN_POINT('Ctrl Pts',(-9.811149300931,9.88702732255485,9.83748958027846));
#120932=CARTESIAN_POINT('Ctrl Pts',(-9.80938824931081,9.8869156335339,9.83777566444935));
#120933=CARTESIAN_POINT('Ctrl Pts',(-9.80762778878882,9.88680387632169,
9.83806575984527));
#120934=CARTESIAN_POINT('Ctrl Pts',(-9.75742776987676,9.88361396124912,
9.84645513374948));
#120935=CARTESIAN_POINT('Ctrl Pts',(-9.70954676787389,9.8804854382945,9.8575714057799));
#120936=CARTESIAN_POINT('Ctrl Pts',(-9.65162148964359,9.8765154451205,9.87489712639537));
#120937=CARTESIAN_POINT('Ctrl Pts',(-9.64078796236252,9.87576491170119,
9.87830897301879));
#120938=CARTESIAN_POINT('Ctrl Pts',(-9.62358365976746,9.87455931229639,
9.88400198881191));
#120939=CARTESIAN_POINT('Ctrl Pts',(-9.61718009036813,9.87410751926147,
9.88618235974566));
#120940=CARTESIAN_POINT('Ctrl Pts',(-9.6050772592325,9.87324763554169,9.89041998859629));
#120941=CARTESIAN_POINT('Ctrl Pts',(-9.59937437796505,9.87283991432368,
9.89246630683284));
#120942=CARTESIAN_POINT('Ctrl Pts',(-9.58643003504639,9.8719085437726,9.89722407751386));
#120943=CARTESIAN_POINT('Ctrl Pts',(-9.57919904028137,9.87138400438727,
9.89996300130681));
#120944=CARTESIAN_POINT('Ctrl Pts',(-9.5570009627198,9.8697602920866,9.90862198605889));
#120945=CARTESIAN_POINT('Ctrl Pts',(-9.54212839488076,9.86865339581668,
9.91477759641596));
#120946=CARTESIAN_POINT('Ctrl Pts',(-9.46390490726167,9.86272700280551,
9.94904775201491));
#120947=CARTESIAN_POINT('Ctrl Pts',(-9.40301170560974,9.85773306371417,
9.98240445600521));
#120948=CARTESIAN_POINT('Ctrl Pts',(-9.29670362250005,9.84837455696655,
10.0534788470948));
#120949=CARTESIAN_POINT('Ctrl Pts',(-9.25049208672881,9.84404770574388,
10.0896339673903));
#120950=CARTESIAN_POINT('Ctrl Pts',(-9.19331958916606,9.83847620862531,
10.1416805933299));
#120951=CARTESIAN_POINT('Ctrl Pts',(-9.17977839627417,9.83713907676591,
10.1546112798479));
#120952=CARTESIAN_POINT('Ctrl Pts',(-9.15773930903832,9.83494077863843,
10.1766850480223));
#120953=CARTESIAN_POINT('Ctrl Pts',(-9.14906838188003,9.83406989640862,
10.1856499561546));
#120954=CARTESIAN_POINT('Ctrl Pts',(-9.13717745249645,9.83286918669891,
10.1983413965465));
#120955=CARTESIAN_POINT('Ctrl Pts',(-9.13383628550524,9.8325310782292,10.2019525785877));
#120956=CARTESIAN_POINT('Ctrl Pts',(-9.12817997426074,9.83195760129593,
10.2081433731584));
#120957=CARTESIAN_POINT('Ctrl Pts',(-9.12585343206928,9.83172140273937,
10.2107124390951));
#120958=CARTESIAN_POINT('Ctrl Pts',(-9.12104807035986,9.83123294197615,
10.216066032842));
#120959=CARTESIAN_POINT('Ctrl Pts',(-9.11857108944876,9.83098081051642,
10.2188521035691));
#120960=CARTESIAN_POINT('Ctrl Pts',(-9.11203413565804,9.83031433618123,
10.2262754542908));
#120961=CARTESIAN_POINT('Ctrl Pts',(-9.10799719766506,9.82990163320605,
10.2309329979921));
#120962=CARTESIAN_POINT('Ctrl Pts',(-9.09048630659057,9.82810541686445,
10.2514592501817));
#120963=CARTESIAN_POINT('Ctrl Pts',(-9.07739697725658,9.82674683075645,
10.2676529502166));
#120964=CARTESIAN_POINT('Ctrl Pts',(-9.05353078340538,9.82422037300306,
10.2988356816681));
#120965=CARTESIAN_POINT('Ctrl Pts',(-9.04266388283144,9.82304877474012,
10.3137471332485));
#120966=CARTESIAN_POINT('Ctrl Pts',(-8.96819436241842,9.81481842660564,
10.4211471059183));
#120967=CARTESIAN_POINT('Ctrl Pts',(-8.91775298506138,9.80809368591901,
10.5220501560005));
#120968=CARTESIAN_POINT('Ctrl Pts',(-8.87619595746399,9.79956484730944,
10.647096763609));
#120969=CARTESIAN_POINT('Ctrl Pts',(-8.87050078497368,9.79828826798496,
10.6657730217614));
#120970=CARTESIAN_POINT('Ctrl Pts',(-8.86303937459166,9.79644526134415,
10.6926156541589));
#120971=CARTESIAN_POINT('Ctrl Pts',(-8.86089153545792,9.79589099534867,
10.7006732556792));
#120972=CARTESIAN_POINT('Ctrl Pts',(-8.85730990284954,9.79492353956979,
10.7147068799046));
#120973=CARTESIAN_POINT('Ctrl Pts',(-8.85583696553106,9.79451161141421,
10.7206726461291));
#120974=CARTESIAN_POINT('Ctrl Pts',(-8.85290378181932,9.7936613347415,10.7329653781374));
#120975=CARTESIAN_POINT('Ctrl Pts',(-8.85144904174875,9.79322282734327,
10.7392934284883));
#120976=CARTESIAN_POINT('Ctrl Pts',(-8.84786508979036,9.79209785469609,
10.7554959175359));
#120977=CARTESIAN_POINT('Ctrl Pts',(-8.84581049053718,9.79140906533196,
10.7653861408711));
#120978=CARTESIAN_POINT('Ctrl Pts',(-8.8381308239319,9.7886481850616,10.8048994545932));
#120979=CARTESIAN_POINT('Ctrl Pts',(-8.83351746386396,9.78654504603491,
10.8347050643838));
#120980=CARTESIAN_POINT('Ctrl Pts',(-8.81950279461284,9.77790934261126,
10.9558483313827));
#120981=CARTESIAN_POINT('Ctrl Pts',(-8.81965306652895,9.77111114552344,
11.0479571288892));
#120982=CARTESIAN_POINT('Ctrl Pts',(-8.83557524991109,9.76127932385518,
11.1818299339724));
#120983=CARTESIAN_POINT('Ctrl Pts',(-8.84299697499609,9.75817718903045,
11.2242586803145));
#120984=CARTESIAN_POINT('Ctrl Pts',(-8.85436350056308,9.75467670583731,
11.2732481884474));
#120985=CARTESIAN_POINT('Ctrl Pts',(-8.85606627222088,9.75417547762376,
11.2802912669989));
#120986=CARTESIAN_POINT('Ctrl Pts',(-8.85880094149647,9.7534054319023,11.291162294782));
#120987=CARTESIAN_POINT('Ctrl Pts',(-8.85978731182509,9.75313419177258,
11.2950013557914));
#120988=CARTESIAN_POINT('Ctrl Pts',(-8.8616553517524,9.75263244678719,11.3021226131765));
#120989=CARTESIAN_POINT('Ctrl Pts',(-8.86253184545969,9.75240167205826,
11.3054059747728));
#120990=CARTESIAN_POINT('Ctrl Pts',(-8.86456900976734,9.75187570795753,
11.3129067935924));
#120991=CARTESIAN_POINT('Ctrl Pts',(-8.86573897534929,9.75158104895785,
11.317121624209));
#120992=CARTESIAN_POINT('Ctrl Pts',(-8.86953295951012,9.75064831401181,
11.33049990041));
#120993=CARTESIAN_POINT('Ctrl Pts',(-8.87224482589534,9.75001498240701,
11.3396383301106));
#120994=CARTESIAN_POINT('Ctrl Pts',(-8.89935199139144,9.74398271811706,
11.4270772666833));
#120995=CARTESIAN_POINT('Ctrl Pts',(-8.93175595000109,9.73897057855183,
11.5026725423464));
#120996=CARTESIAN_POINT('Ctrl Pts',(-9.00678218522363,9.7294448070713,11.637002626922));
#120997=CARTESIAN_POINT('Ctrl Pts',(-9.04746392409348,9.72496551226715,
11.6963671231838));
#120998=CARTESIAN_POINT('Ctrl Pts',(-9.10237112481543,9.71934806547782,
11.7626006015593));
#120999=CARTESIAN_POINT('Ctrl Pts',(-9.11164377099181,9.71841232085094,
11.7733824779468));
#121000=CARTESIAN_POINT('Ctrl Pts',(-9.12601252731676,9.71697986905652,
11.7894904822132));
#121001=CARTESIAN_POINT('Ctrl Pts',(-9.13096738043261,9.71648895547584,
11.7949412719888));
#121002=CARTESIAN_POINT('Ctrl Pts',(-9.14006995512849,9.71559235675428,
11.8047681211574));
#121003=CARTESIAN_POINT('Ctrl Pts',(-9.14420079903002,9.71518738933212,
11.8091595245777));
#121004=CARTESIAN_POINT('Ctrl Pts',(-9.15321082706596,9.71430808338907,
11.8185917009442));
#121005=CARTESIAN_POINT('Ctrl Pts',(-9.15810167538714,9.71383325421941,
11.8236209586879));
#121006=CARTESIAN_POINT('Ctrl Pts',(-9.1716137492505,9.71252794521055,11.8372693067875));
#121007=CARTESIAN_POINT('Ctrl Pts',(-9.18032412316014,9.71169360776905,
11.845798504434));
#121008=CARTESIAN_POINT('Ctrl Pts',(-9.24123195425378,9.70590573268996,
11.9036148668312));
#121009=CARTESIAN_POINT('Ctrl Pts',(-9.29769931890522,9.70075540754787,
11.948166224931));
#121010=CARTESIAN_POINT('Ctrl Pts',(-9.40197001623249,9.69166421459674,
12.0159842333896));
#121011=CARTESIAN_POINT('Ctrl Pts',(-9.44795292833287,9.68778112580812,
12.0416851315213));
#121012=CARTESIAN_POINT('Ctrl Pts',(-9.51786634525496,9.68216169301164,
12.0748278239055));
#121013=CARTESIAN_POINT('Ctrl Pts',(-9.54056239666864,9.68037948953561,
12.0847234462328));
#121014=CARTESIAN_POINT('Ctrl Pts',(-9.57315318296372,9.67789388313698,
12.0977265836197));
#121015=CARTESIAN_POINT('Ctrl Pts',(-9.58280194678847,9.67716694804327,
12.1014298245006));
#121016=CARTESIAN_POINT('Ctrl Pts',(-9.59995898745751,9.67589157060576,
12.1077569580108));
#121017=CARTESIAN_POINT('Ctrl Pts',(-9.60744733867339,9.67534065663029,
12.1104326663095));
#121018=CARTESIAN_POINT('Ctrl Pts',(-9.61884810997145,9.6745111756803,12.1143765989523));
#121019=CARTESIAN_POINT('Ctrl Pts',(-9.6227408417162,9.67422958139862,12.1157004509928));
#121020=CARTESIAN_POINT('Ctrl Pts',(-9.62985133715946,9.67371828228539,
12.1180771400863));
#121021=CARTESIAN_POINT('Ctrl Pts',(-9.63306674281682,9.67348821673665,
12.1191365015956));
#121022=CARTESIAN_POINT('Ctrl Pts',(-9.64033459636005,9.67297075619939,
12.1214963093425));
#121023=CARTESIAN_POINT('Ctrl Pts',(-9.64438955983057,9.67268382662395,
12.1227886669808));
#121024=CARTESIAN_POINT('Ctrl Pts',(-9.65490677957797,9.67194400630748,
12.1260779182545));
#121025=CARTESIAN_POINT('Ctrl Pts',(-9.66137949645554,9.67149295539119,
12.1280412087164));
#121026=CARTESIAN_POINT('Ctrl Pts',(-9.70773442002203,9.66829069942655,
12.1416665260476));
#121027=CARTESIAN_POINT('Ctrl Pts',(-9.74819687954295,9.66564254480248,
12.1512678284537));
#121028=CARTESIAN_POINT('Ctrl Pts',(-9.81005817730761,9.66169899906717,
12.1625280847824));
#121029=CARTESIAN_POINT('Ctrl Pts',(-9.83113008269472,9.66037386493225,
12.1657754661205));
#121030=CARTESIAN_POINT('Ctrl Pts',(-9.90177779370762,9.65596023070978,
12.1747070938877));
#121031=CARTESIAN_POINT('Ctrl Pts',(-9.95162309117121,9.65289167874183,
12.1778131822629));
#121032=CARTESIAN_POINT('Ctrl Pts',(-10.0507397367808,9.64668007169886,
12.1776857268401));
#121033=CARTESIAN_POINT('Ctrl Pts',(-10.0999071147109,9.64354461129797,
12.1745364546185));
#121034=CARTESIAN_POINT('Ctrl Pts',(-10.1600029562102,9.6395667982176,12.1668861415174));
#121035=CARTESIAN_POINT('Ctrl Pts',(-10.1712547301108,9.63881583493078,
12.1652879541012));
#121036=CARTESIAN_POINT('Ctrl Pts',(-10.1891656188076,9.63760970747759,
12.1624789074373));
#121037=CARTESIAN_POINT('Ctrl Pts',(-10.195840656077,9.63715782137835,12.1613730131975));
#121038=CARTESIAN_POINT('Ctrl Pts',(-10.2084740802709,9.63629786443558,
12.1591679461558));
#121039=CARTESIAN_POINT('Ctrl Pts',(-10.2144342571239,9.63589016395301,
12.1580801857217));
#121040=CARTESIAN_POINT('Ctrl Pts',(-10.2279789546812,9.63495898598467,
12.1555000686678));
#121041=CARTESIAN_POINT('Ctrl Pts',(-10.2355576426227,9.63443461982638,
12.1539789445838));
#121042=CARTESIAN_POINT('Ctrl Pts',(-10.25885618064,9.63281199419249,12.1490636047662));
#121043=CARTESIAN_POINT('Ctrl Pts',(-10.2745213486091,9.63170602633101,
12.1454220510301));
#121044=CARTESIAN_POINT('Ctrl Pts',(-10.3632770509769,9.6253511766851,12.1228644725453));
#121045=CARTESIAN_POINT('Ctrl Pts',(-10.4344777476678,9.61989167528658,
12.0972785932153));
#121046=CARTESIAN_POINT('Ctrl Pts',(-10.5455791774064,9.61088622699447,
12.0448366447072));
#121047=CARTESIAN_POINT('Ctrl Pts',(-10.5871702586243,9.60739663019113,
12.022042838848));
#121048=CARTESIAN_POINT('Ctrl Pts',(-10.6457337716462,9.60238843756634,
11.9851896098343));
#121049=CARTESIAN_POINT('Ctrl Pts',(-10.6638666214858,9.600823927387,11.9730631501648));
#121050=CARTESIAN_POINT('Ctrl Pts',(-10.6930108621532,9.59829821309417,
11.9523785905249));
#121051=CARTESIAN_POINT('Ctrl Pts',(-10.7042252179912,9.59732354345189,
11.944116475514));
#121052=CARTESIAN_POINT('Ctrl Pts',(-10.7193700438529,9.59600620759629,
11.9325385598934));
#121053=CARTESIAN_POINT('Ctrl Pts',(-10.723428785002,9.59565306244783,11.9293934695019));
#121054=CARTESIAN_POINT('Ctrl Pts',(-10.7302243973425,9.59506178793847,
11.9240561055544));
#121055=CARTESIAN_POINT('Ctrl Pts',(-10.7329722507951,9.59482270310337,
11.9218779948758));
#121056=CARTESIAN_POINT('Ctrl Pts',(-10.7382184127105,9.59436631045113,
11.9176812916052));
#121057=CARTESIAN_POINT('Ctrl Pts',(-10.7407182402411,9.59414885991354,
11.9156647132149));
#121058=CARTESIAN_POINT('Ctrl Pts',(-10.7474165622467,9.59356616441293,
11.9102158820014));
#121059=CARTESIAN_POINT('Ctrl Pts',(-10.7515997160089,9.59320223059599,
11.9067647650251));
#121060=CARTESIAN_POINT('Ctrl Pts',(-10.7671104385141,9.59185201939796,
11.8937872767119));
#121061=CARTESIAN_POINT('Ctrl Pts',(-10.7782824933457,9.59087791954824,
11.884076088594));
#121062=CARTESIAN_POINT('Ctrl Pts',(-10.8774973694459,9.58218125482287,
11.7944957305467));
#121063=CARTESIAN_POINT('Ctrl Pts',(-10.9531667791192,9.57515033779875,
11.7019301158193));
#121064=CARTESIAN_POINT('Ctrl Pts',(-11.0254070192671,9.5661392839539,11.5797968084552));
#121065=CARTESIAN_POINT('Ctrl Pts',(-11.0365315895107,9.56466423778319,
11.5596660249203));
#121066=CARTESIAN_POINT('Ctrl Pts',(-11.0548575163695,9.56206336091851,
11.5240809007806));
#121067=CARTESIAN_POINT('Ctrl Pts',(-11.0623259920012,9.56094649535609,
11.5087716673341));
#121068=CARTESIAN_POINT('Ctrl Pts',(-11.0727710896248,9.55929466312735,
11.4861273066937));
#121069=CARTESIAN_POINT('Ctrl Pts',(-11.0760101599535,9.5587685887106,11.4789151278091));
#121070=CARTESIAN_POINT('Ctrl Pts',(-11.0816112371478,9.55783359713573,
11.4660999463765));
#121071=CARTESIAN_POINT('Ctrl Pts',(-11.0840029504198,9.55742569707559,
11.4605101838789));
#121072=CARTESIAN_POINT('Ctrl Pts',(-11.0889283883621,9.55656708229574,
11.448747754238));
#121073=CARTESIAN_POINT('Ctrl Pts',(-11.0914531445738,9.5561160850303,11.4425715896387));
#121074=CARTESIAN_POINT('Ctrl Pts',(-11.0979756315731,9.55492150871984,
11.4262206924616));
#121075=CARTESIAN_POINT('Ctrl Pts',(-11.1018843336454,9.55417501819788,
11.4160113790721));
#121076=CARTESIAN_POINT('Ctrl Pts',(-11.1185015566555,9.55086046105451,
11.3707301402732));
#121077=CARTESIAN_POINT('Ctrl Pts',(-11.1296805368603,9.54824352599374,
11.3351237540807));
#121078=CARTESIAN_POINT('Ctrl Pts',(-11.1587413611797,9.54007383858363,
11.2244244284301));
#121079=CARTESIAN_POINT('Ctrl Pts',(-11.1709500611552,9.53437801229778,
11.1480594504365));
#121080=CARTESIAN_POINT('Ctrl Pts',(-11.1776042310567,9.52631363124162,
11.0379739509555));
#121081=CARTESIAN_POINT('Ctrl Pts',(-11.1782066204,9.52390616780706,11.0048159962228));
#121082=CARTESIAN_POINT('Ctrl Pts',(-11.1771087191378,9.52065502650292,
10.9591788541713));
#121083=CARTESIAN_POINT('Ctrl Pts',(-11.1766091740062,9.51977168284805,
10.9466878854261));
#121084=CARTESIAN_POINT('Ctrl Pts',(-11.1753963307118,9.51825254499728,
10.9250109701606));
#121085=CARTESIAN_POINT('Ctrl Pts',(-11.1747739508,9.51761284497638,10.9158212233339));
#121086=CARTESIAN_POINT('Ctrl Pts',(-11.1736981446166,9.51667838729771,
10.9022925691619));
#121087=CARTESIAN_POINT('Ctrl Pts',(-11.1733283391365,9.51637937913493,
10.8979476270582));
#121088=CARTESIAN_POINT('Ctrl Pts',(-11.1726280720717,9.51585019771711,
10.8902276644476));
#121089=CARTESIAN_POINT('Ctrl Pts',(-11.1723071575084,9.51561951675379,
10.8868519089815));
#121090=CARTESIAN_POINT('Ctrl Pts',(-11.1715733453109,9.51511674748456,
10.8794713025378));
#121091=CARTESIAN_POINT('Ctrl Pts',(-11.1711544906633,9.51484498810846,
10.8754671506735));
#121092=CARTESIAN_POINT('Ctrl Pts',(-11.1699154753331,9.51408170758592,
10.8641820091554));
#121093=CARTESIAN_POINT('Ctrl Pts',(-11.1690478752164,9.5135927026095,10.8569062608117));
#121094=CARTESIAN_POINT('Ctrl Pts',(-11.1630311639878,9.51046835065218,
10.8101641641057));
#121095=CARTESIAN_POINT('Ctrl Pts',(-11.1559515967004,9.50792700618369,
10.7709677882233));
#121096=CARTESIAN_POINT('Ctrl Pts',(-11.1416878321562,9.50398642726335,
10.7098804828271));
#121097=CARTESIAN_POINT('Ctrl Pts',(-11.1358253549166,9.50256099574795,
10.6877160602979));
#121098=CARTESIAN_POINT('Ctrl Pts',(-11.1153314344916,9.49808507274521,
10.6184767497435));
#121099=CARTESIAN_POINT('Ctrl Pts',(-11.098390801648,9.49505381190256,10.5721428750308));
#121100=CARTESIAN_POINT('Ctrl Pts',(-11.058501922491,9.48883299390727,10.4811815766583));
#121101=CARTESIAN_POINT('Ctrl Pts',(-11.0355086020152,9.48564782222594,
10.4366884536217));
#121102=CARTESIAN_POINT('Ctrl Pts',(-11.0038844657147,9.48161398404501,
10.3840119663873));
#121103=CARTESIAN_POINT('Ctrl Pts',(-10.997869255619,9.4808599884961,10.3743146063176));
#121104=CARTESIAN_POINT('Ctrl Pts',(-10.9880591204501,9.47965013620202,
10.3590006606479));
#121105=CARTESIAN_POINT('Ctrl Pts',(-10.9843548758562,9.47919759371051,
10.3533266251816));
#121106=CARTESIAN_POINT('Ctrl Pts',(-10.9772473260628,9.47833711750577,
10.342642098877));
#121107=CARTESIAN_POINT('Ctrl Pts',(-10.9738539175789,9.47792956044399,
10.3376252636655));
#121108=CARTESIAN_POINT('Ctrl Pts',(-10.9660518678124,9.47699972697495,
10.3262802278948));
#121109=CARTESIAN_POINT('Ctrl Pts',(-10.961619496813,9.47647657153617,10.3199687646263));
#121110=CARTESIAN_POINT('Ctrl Pts',(-10.9478081524572,9.47486152815741,
10.300707191248));
#121111=CARTESIAN_POINT('Ctrl Pts',(-10.9382275221866,9.47376203587114,
10.287904641652));
#121112=CARTESIAN_POINT('Ctrl Pts',(-10.8794063405429,9.46712951223174,
10.2125505680206));
#121113=CARTESIAN_POINT('Ctrl Pts',(-10.8241956202042,9.46135953916051,
10.1549381568791));
#121114=CARTESIAN_POINT('Ctrl Pts',(-10.7101598844336,9.45037270736284,
10.0578233839667));
#121115=CARTESIAN_POINT('Ctrl Pts',(-10.6527429110041,9.4451979678151,10.0171713005949));
#121116=CARTESIAN_POINT('Ctrl Pts',(-10.5830947380716,9.43954538229104,
9.97667076833222));
#121117=CARTESIAN_POINT('Ctrl Pts',(-10.5740787112456,9.43882503169663,
9.97158576367232));
#121118=CARTESIAN_POINT('Ctrl Pts',(-10.5610299748844,9.43779994810624,
9.96445141798547));
#121119=CARTESIAN_POINT('Ctrl Pts',(-10.557050969699,9.43748966744028,9.96230557615531));
#121120=CARTESIAN_POINT('Ctrl Pts',(-10.5500438966177,9.43694741795186,
9.95857864350278));
#121121=CARTESIAN_POINT('Ctrl Pts',(-10.5470211620447,9.43671485298764,
9.95698773763269));
#121122=CARTESIAN_POINT('Ctrl Pts',(-10.540557163981,9.43622043737663,9.95362147967522));
#121123=CARTESIAN_POINT('Ctrl Pts',(-10.5371140321778,9.43595881815429,
9.95184992827973));
#121124=CARTESIAN_POINT('Ctrl Pts',(-10.5275820135217,9.43523915997629,
9.94700484282948));
#121125=CARTESIAN_POINT('Ctrl Pts',(-10.5214749527171,9.43478325195569,
9.94396711170502));
#121126=CARTESIAN_POINT('Ctrl Pts',(-10.4856374110203,9.43213595062314,
9.92652775980064));
#121127=CARTESIAN_POINT('Ctrl Pts',(-10.4553350358479,9.43000956888852,
9.91332765108223));
#121128=CARTESIAN_POINT('Ctrl Pts',(-10.3786117831148,9.42480384980121,
9.88368019931818));
#121129=CARTESIAN_POINT('Ctrl Pts',(-10.3316398728185,9.4217714470221,9.86883588281473));
#121130=CARTESIAN_POINT('Ctrl Pts',(-10.213079165508,9.41421278653319,9.83939088186083));
#121131=CARTESIAN_POINT('Ctrl Pts',(-10.1408115597129,9.40967965837839,
9.82842557594697));
#121132=CARTESIAN_POINT('Ctrl Pts',(-10.0519013977926,9.403884019448,9.82328368204909));
#121133=CARTESIAN_POINT('Ctrl Pts',(-10.035787476563,9.40282556943374,9.82268344788408));
#121134=CARTESIAN_POINT('Ctrl Pts',(-10.011930228533,9.40124418740033,9.82228500679487));
#121135=CARTESIAN_POINT('Ctrl Pts',(-10.0041926112593,9.40072907836155,
9.82223204627822));
#121136=CARTESIAN_POINT('Ctrl Pts',(-9.99039569824927,9.39980637588931,
9.82227357268185));
#121137=CARTESIAN_POINT('Ctrl Pts',(-9.98433654090951,9.39939970596728,
9.82233857415405));
#121138=CARTESIAN_POINT('Ctrl Pts',(-9.97151793132222,9.39853617381677,
9.82257503350508));
#121139=CARTESIAN_POINT('Ctrl Pts',(-9.96475893638935,9.39807897235682,
9.82275795007639));
#121140=CARTESIAN_POINT('Ctrl Pts',(-9.94666581100367,9.39684987552481,
9.82340355268593));
#121141=CARTESIAN_POINT('Ctrl Pts',(-9.93533640440357,9.39607475907768,
9.82397179482884));
#121142=CARTESIAN_POINT('Ctrl Pts',(-9.88620080417885,9.39268818701886,
9.82714840212198));
#121143=CARTESIAN_POINT('Ctrl Pts',(-9.8485346392725,9.39002702650581,9.83141630341042));
#121144=CARTESIAN_POINT('Ctrl Pts',(-9.81114929154307,9.38732021693139,
9.83748958180354));
#121145=CARTESIAN_POINT('Ctrl Pts',(-9.81114930150154,9.28890850071391,
9.83748958018578));
#121146=CARTESIAN_POINT('Ctrl Pts',(-9.81238629142768,9.28899283107266,
9.83728863023504));
#121147=CARTESIAN_POINT('Ctrl Pts',(-9.81362361031034,9.28907705602562,
9.83708965331073));
#121148=CARTESIAN_POINT('Ctrl Pts',(-9.82359200226222,9.28975459758873,
9.83550292480142));
#121149=CARTESIAN_POINT('Ctrl Pts',(-9.83233844276262,9.29034283247144,
9.83421149710092));
#121150=CARTESIAN_POINT('Ctrl Pts',(-9.85284227527573,9.29170894531513,
9.83141960910498));
#121151=CARTESIAN_POINT('Ctrl Pts',(-9.86460959421868,9.29248311559321,
9.82999786872615));
#121152=CARTESIAN_POINT('Ctrl Pts',(-9.90673070950593,9.29522551132414,
9.8255527714253));
#121153=CARTESIAN_POINT('Ctrl Pts',(-9.93717967547182,9.29715493064775,
9.82353099498969));
#121154=CARTESIAN_POINT('Ctrl Pts',(-10.0412499298315,9.30366930523765,
9.82067354204818));
#121155=CARTESIAN_POINT('Ctrl Pts',(-10.1148519412607,9.30814998712544,
9.82555470571068));
#121156=CARTESIAN_POINT('Ctrl Pts',(-10.2308040256384,9.31553851517843,
9.84425478538658));
#121157=CARTESIAN_POINT('Ctrl Pts',(-10.2736623297318,9.31834136498324,
9.85364674809787));
#121158=CARTESIAN_POINT('Ctrl Pts',(-10.3268599785669,9.32196710360418,
9.86845804913041));
#121159=CARTESIAN_POINT('Ctrl Pts',(-10.3377805921385,9.32271926092387,
9.87166986702973));
#121160=CARTESIAN_POINT('Ctrl Pts',(-10.3551180510158,9.32392677524327,
9.87704316684379));
#121161=CARTESIAN_POINT('Ctrl Pts',(-10.3615659568139,9.32437883932188,
9.87910262069208));
#121162=CARTESIAN_POINT('Ctrl Pts',(-10.3737484558308,9.32523879438062,
9.8831097503593));
#121163=CARTESIAN_POINT('Ctrl Pts',(-10.3794864966331,9.32564631228905,
9.88504630835882));
#121164=CARTESIAN_POINT('Ctrl Pts',(-10.3925041217116,9.32657659596062,
9.8895518171993));
#121165=CARTESIAN_POINT('Ctrl Pts',(-10.3997738333531,9.32710024538058,
9.89214823667424));
#121166=CARTESIAN_POINT('Ctrl Pts',(-10.4220632404085,9.32871883598333,
9.90035698235124));
#121167=CARTESIAN_POINT('Ctrl Pts',(-10.43699373059,9.32982143210397,9.90620450688179));
#121168=CARTESIAN_POINT('Ctrl Pts',(-10.4714222035734,9.33240824503439,
9.92050583338112));
#121169=CARTESIAN_POINT('Ctrl Pts',(-10.4908195203022,9.33389948543975,
9.92918598631351));
#121170=CARTESIAN_POINT('Ctrl Pts',(-10.5612391302604,9.3394392120374,9.96301363600086));
#121171=CARTESIAN_POINT('Ctrl Pts',(-10.6106511984772,9.34357974063689,
9.99132069741985));
#121172=CARTESIAN_POINT('Ctrl Pts',(-10.717221910682,9.35300188196796,10.0630815203742));
#121173=CARTESIAN_POINT('Ctrl Pts',(-10.7728563816388,9.35828472116328,
10.1084181076414));
#121174=CARTESIAN_POINT('Ctrl Pts',(-10.8314057349917,9.36403376904416,
10.165754161119));
#121175=CARTESIAN_POINT('Ctrl Pts',(-10.838685887661,9.36475215224898,10.1730733915267));
#121176=CARTESIAN_POINT('Ctrl Pts',(-10.8490108498607,9.36577491067181,
10.1837304215292));
#121177=CARTESIAN_POINT('Ctrl Pts',(-10.8521339238325,9.36608480126634,
10.1869912513043));
#121178=CARTESIAN_POINT('Ctrl Pts',(-10.857585585026,9.36662655446492,10.1927493055179));
#121179=CARTESIAN_POINT('Ctrl Pts',(-10.8599221778803,9.36685901045488,
10.1952388127088));
#121180=CARTESIAN_POINT('Ctrl Pts',(-10.8648864308651,9.36735340002429,
10.2005742518597));
#121181=CARTESIAN_POINT('Ctrl Pts',(-10.867510905161,9.36761510074435,10.2034230133923));
#121182=CARTESIAN_POINT('Ctrl Pts',(-10.8747238124734,9.36833542899742,
10.2113302625527));
#121183=CARTESIAN_POINT('Ctrl Pts',(-10.8792824622557,9.36879191828701,
10.2164158884212));
#121184=CARTESIAN_POINT('Ctrl Pts',(-10.9057577346191,9.37145239801626,
10.246473682744));
#121185=CARTESIAN_POINT('Ctrl Pts',(-10.9266561299168,9.37359060940483,
10.2723270984589));
#121186=CARTESIAN_POINT('Ctrl Pts',(-10.9760894162227,9.37884609551523,
10.3390711057403));
#121187=CARTESIAN_POINT('Ctrl Pts',(-11.0031746124824,9.3819150234878,10.3809533597151));
#121188=CARTESIAN_POINT('Ctrl Pts',(-11.0627383223666,9.3894569353155,10.4872879247389));
#121189=CARTESIAN_POINT('Ctrl Pts',(-11.0921034161813,9.3939371444805,10.5532396097895));
#121190=CARTESIAN_POINT('Ctrl Pts',(-11.1204557258939,9.39967719255917,
10.6367706329338));
#121191=CARTESIAN_POINT('Ctrl Pts',(-11.1253375165846,9.40073874903828,
10.6521896500369));
#121192=CARTESIAN_POINT('Ctrl Pts',(-11.1320854756154,9.40232379989139,
10.6751345936017));
#121193=CARTESIAN_POINT('Ctrl Pts',(-11.1341974472289,9.40283941534969,
10.6825867011463));
#121194=CARTESIAN_POINT('Ctrl Pts',(-11.1378302078953,9.40376258109945,
10.6959043060874));
#121195=CARTESIAN_POINT('Ctrl Pts',(-11.1393795399129,9.40416920287083,
10.701761781885));
#121196=CARTESIAN_POINT('Ctrl Pts',(-11.1425601881775,9.40503216497761,
10.714173315404));
#121197=CARTESIAN_POINT('Ctrl Pts',(-11.1441804551736,9.40548884081071,
10.7207299515587));
#121198=CARTESIAN_POINT('Ctrl Pts',(-11.1483638524071,9.40671537699297,
10.7383064236898));
#121199=CARTESIAN_POINT('Ctrl Pts',(-11.1508246795661,9.40748843639763,
10.7493496323047));
#121200=CARTESIAN_POINT('Ctrl Pts',(-11.1629723306005,9.4115955565733,10.8078191931531));
#121201=CARTESIAN_POINT('Ctrl Pts',(-11.1698863373508,9.41501511004576,
10.8557677110338));
#121202=CARTESIAN_POINT('Ctrl Pts',(-11.17794527137,9.42213971779147,10.9543077727452));
#121203=CARTESIAN_POINT('Ctrl Pts',(-11.1788210162106,9.42584364395567,
11.0048250846842));
#121204=CARTESIAN_POINT('Ctrl Pts',(-11.1756170966727,9.43085599160356,
11.0730601327088));
#121205=CARTESIAN_POINT('Ctrl Pts',(-11.1743755187243,9.43216400385614,
11.0908597688378));
#121206=CARTESIAN_POINT('Ctrl Pts',(-11.1685499119349,9.43677666740589,
11.153754076008));
#121207=CARTESIAN_POINT('Ctrl Pts',(-11.1617676936868,9.44005090836022,
11.1986100867019));
#121208=CARTESIAN_POINT('Ctrl Pts',(-11.1510155608579,9.44368161513569,
11.2496082848223));
#121209=CARTESIAN_POINT('Ctrl Pts',(-11.1495581366562,9.44415166514316,
11.2562366347419));
#121210=CARTESIAN_POINT('Ctrl Pts',(-11.147092251452,9.44491202646718,11.2670067302964));
#121211=CARTESIAN_POINT('Ctrl Pts',(-11.1461184821012,9.44520414656266,
11.271156142804));
#121212=CARTESIAN_POINT('Ctrl Pts',(-11.1443310072684,9.44572598464449,
11.2785912142597));
#121213=CARTESIAN_POINT('Ctrl Pts',(-11.1435256451383,9.44595615325374,
11.2818787303616));
#121214=CARTESIAN_POINT('Ctrl Pts',(-11.1417124622674,9.44646359308379,
11.2891445259963));
#121215=CARTESIAN_POINT('Ctrl Pts',(-11.1406980143352,9.4467404877925,11.2931210411702));
#121216=CARTESIAN_POINT('Ctrl Pts',(-11.1376657066151,9.4475482652233,11.3047531462902));
#121217=CARTESIAN_POINT('Ctrl Pts',(-11.1355913686239,9.44807608027455,
11.3123939692873));
#121218=CARTESIAN_POINT('Ctrl Pts',(-11.1306476377437,9.44928043925828,
11.32990392391));
#121219=CARTESIAN_POINT('Ctrl Pts',(-11.1277257652357,9.4499543738738,11.3397576988492));
#121220=CARTESIAN_POINT('Ctrl Pts',(-11.1173886278384,9.4522199414502,11.3730152565905));
#121221=CARTESIAN_POINT('Ctrl Pts',(-11.1093704072429,9.45378589460911,
11.3962261742062));
#121222=CARTESIAN_POINT('Ctrl Pts',(-11.0818519377761,9.45866124432687,
11.4684824062941));
#121223=CARTESIAN_POINT('Ctrl Pts',(-11.0597783991114,9.46190256023911,
11.5164780669949));
#121224=CARTESIAN_POINT('Ctrl Pts',(-11.0001925798052,9.4696271910506,11.6260044437626));
#121225=CARTESIAN_POINT('Ctrl Pts',(-10.9601167798413,9.47412503617093,
11.685886694406));
#121226=CARTESIAN_POINT('Ctrl Pts',(-10.9071435538109,9.47963662738325,
11.751222175606));
#121227=CARTESIAN_POINT('Ctrl Pts',(-10.8993060127274,9.48044225257185,
11.7605871821846));
#121228=CARTESIAN_POINT('Ctrl Pts',(-10.8867367344808,9.48172009868814,
11.77514017396));
#121229=CARTESIAN_POINT('Ctrl Pts',(-10.8821016597997,9.48218840086363,
11.7804107788587));
#121230=CARTESIAN_POINT('Ctrl Pts',(-10.8733994507242,9.48306244547943,
11.7901296008024));
#121231=CARTESIAN_POINT('Ctrl Pts',(-10.869344725099,9.48346766560511,11.7945886566156));
#121232=CARTESIAN_POINT('Ctrl Pts',(-10.8602645522863,9.48437076364838,
11.8044215898332));
#121233=CARTESIAN_POINT('Ctrl Pts',(-10.8552226475359,9.48486932560902,
11.8097798546553));
#121234=CARTESIAN_POINT('Ctrl Pts',(-10.8403155372915,9.48633524745779,
11.8253278180035));
#121235=CARTESIAN_POINT('Ctrl Pts',(-10.8303163784592,9.48730831110135,
11.835386671333));
#121236=CARTESIAN_POINT('Ctrl Pts',(-10.7793192723676,9.49222283153462,
11.8848679885892));
#121237=CARTESIAN_POINT('Ctrl Pts',(-10.735690918824,9.49628043828416,11.9214592019986));
#121238=CARTESIAN_POINT('Ctrl Pts',(-10.6426288268623,9.50462518840194,
11.9886758949842));
#121239=CARTESIAN_POINT('Ctrl Pts',(-10.593222306063,9.50890396462073,12.0190872509067));
#121240=CARTESIAN_POINT('Ctrl Pts',(-10.5224185054236,9.51471832836415,
12.0557696286537));
#121241=CARTESIAN_POINT('Ctrl Pts',(-10.5027801228185,9.51629896694799,
12.0652618629947));
#121242=CARTESIAN_POINT('Ctrl Pts',(-10.4623261614532,9.51947685725525,
12.0834472032572));
#121243=CARTESIAN_POINT('Ctrl Pts',(-10.4415008164873,9.52107225972215,
12.0920991298801));
#121244=CARTESIAN_POINT('Ctrl Pts',(-10.4145260736668,9.52307654590144,
12.1024079359971));
#121245=CARTESIAN_POINT('Ctrl Pts',(-10.4085954839624,9.523513412781,12.1046197798526));
#121246=CARTESIAN_POINT('Ctrl Pts',(-10.3991101626343,9.52420578940791,
12.1080705333613));
#121247=CARTESIAN_POINT('Ctrl Pts',(-10.3955669260566,9.52446302384449,
12.1093403611312));
#121248=CARTESIAN_POINT('Ctrl Pts',(-10.3887655488734,9.52495403055696,
12.1117411137708));
#121249=CARTESIAN_POINT('Ctrl Pts',(-10.3855084713862,9.52518794741127,
12.1128747345613));
#121250=CARTESIAN_POINT('Ctrl Pts',(-10.3776835927793,9.52574708342137,
12.1155596967004));
#121251=CARTESIAN_POINT('Ctrl Pts',(-10.3731110897487,9.52607151593239,
12.1170973323241));
#121252=CARTESIAN_POINT('Ctrl Pts',(-10.3572575782142,9.52718884455906,
12.1223203303473));
#121253=CARTESIAN_POINT('Ctrl Pts',(-10.3459299714877,9.52797406230489,
12.1258633941903));
#121254=CARTESIAN_POINT('Ctrl Pts',(-10.3177707674791,9.52989816047619,
12.1342059178023));
#121255=CARTESIAN_POINT('Ctrl Pts',(-10.3008816874889,9.5310278151308,12.138802704707));
#121256=CARTESIAN_POINT('Ctrl Pts',(-10.2265451070646,9.53591896598004,
12.1572658948226));
#121257=CARTESIAN_POINT('Ctrl Pts',(-10.1681998259575,9.53955154362894,
12.167174731793));
#121258=CARTESIAN_POINT('Ctrl Pts',(-10.038871725141,9.54759043266453,12.179234907543));
#121259=CARTESIAN_POINT('Ctrl Pts',(-9.96794915061524,9.55199645186888,
12.1794393019217));
#121260=CARTESIAN_POINT('Ctrl Pts',(-9.88136498698978,9.55765241025506,
12.171870827871));
#121261=CARTESIAN_POINT('Ctrl Pts',(-9.86531935612558,9.55871176965451,
12.1701352857376));
#121262=CARTESIAN_POINT('Ctrl Pts',(-9.84163951467993,9.56029416574665,
12.167080508595));
#121263=CARTESIAN_POINT('Ctrl Pts',(-9.83397407809116,9.56080936256901,
12.1660147277523));
#121264=CARTESIAN_POINT('Ctrl Pts',(-9.82032788384395,9.56173206333001,
12.1639801093673));
#121265=CARTESIAN_POINT('Ctrl Pts',(-9.81434299574059,9.56213864231125,
12.1630405146676));
#121266=CARTESIAN_POINT('Ctrl Pts',(-9.80169826008948,9.56300181262123,
12.1609552732107));
#121267=CARTESIAN_POINT('Ctrl Pts',(-9.79504051250955,9.56345874171839,
12.1597984012973));
#121268=CARTESIAN_POINT('Ctrl Pts',(-9.77724693005966,9.56468668869176,
12.1565485360494));
#121269=CARTESIAN_POINT('Ctrl Pts',(-9.76613096313191,9.56546091850695,
12.1543520712756));
#121270=CARTESIAN_POINT('Ctrl Pts',(-9.70742681919636,9.56958871082519,
12.141869685641));
#121271=CARTESIAN_POINT('Ctrl Pts',(-9.66048501027235,9.57302881705548,
12.1288019709701));
#121272=CARTESIAN_POINT('Ctrl Pts',(-9.56698193258889,9.58016120064225,
12.0964116141803));
#121273=CARTESIAN_POINT('Ctrl Pts',(-9.52057760629516,9.58385095451787,
12.0769292836869));
#121274=CARTESIAN_POINT('Ctrl Pts',(-9.45812615238472,9.58896874711957,
12.0458714257684));
#121275=CARTESIAN_POINT('Ctrl Pts',(-9.44090671964008,9.59039638886854,
12.036768552548));
#121276=CARTESIAN_POINT('Ctrl Pts',(-9.38586246771766,9.5950011854037,12.0058996530843));
#121277=CARTESIAN_POINT('Ctrl Pts',(-9.34901527086668,9.59814925777463,
11.9824554717117));
#121278=CARTESIAN_POINT('Ctrl Pts',(-9.30753739171142,9.60170471643013,
11.9527042382854));
#121279=CARTESIAN_POINT('Ctrl Pts',(-9.30156449979356,9.60221697683924,
11.9483341650216));
#121280=CARTESIAN_POINT('Ctrl Pts',(-9.2923938897724,9.60300341349259,11.9414908335166));
#121281=CARTESIAN_POINT('Ctrl Pts',(-9.28916717104804,9.6032801101994,11.9390570202812));
#121282=CARTESIAN_POINT('Ctrl Pts',(-9.28325824022292,9.60378668801218,
11.9345521893084));
#121283=CARTESIAN_POINT('Ctrl Pts',(-9.28057242145093,9.60401688782949,
11.9324861953485));
#121284=CARTESIAN_POINT('Ctrl Pts',(-9.27446906357078,9.60453990502997,
11.9277492843404));
#121285=CARTESIAN_POINT('Ctrl Pts',(-9.27105732883218,9.60483220956044,
11.9250710556238));
#121286=CARTESIAN_POINT('Ctrl Pts',(-9.26053991250686,9.60573339441751,
11.916720516071));
#121287=CARTESIAN_POINT('Ctrl Pts',(-9.25348486085126,9.60633803844235,
11.91098456903));
#121288=CARTESIAN_POINT('Ctrl Pts',(-9.19362004216394,9.61147679519786,
11.8611503113386));
#121289=CARTESIAN_POINT('Ctrl Pts',(-9.14469421838923,9.61573601777523,
11.8125781180138));
#121290=CARTESIAN_POINT('Ctrl Pts',(-9.04666147102512,9.6251358133601,11.6965242266218));
#121291=CARTESIAN_POINT('Ctrl Pts',(-8.99991314899424,9.63026101880993,
11.627554501938));
#121292=CARTESIAN_POINT('Ctrl Pts',(-8.95335061639721,9.63670286611648,
11.5402514233177));
#121293=CARTESIAN_POINT('Ctrl Pts',(-8.94617166786187,9.63774418015345,
11.5261105779438));
#121294=CARTESIAN_POINT('Ctrl Pts',(-8.93594044338544,9.63930475615475,
11.5049073162581));
#121295=CARTESIAN_POINT('Ctrl Pts',(-8.93266812627908,9.63981649536579,
11.4979526129023));
#121296=CARTESIAN_POINT('Ctrl Pts',(-8.92694109934899,9.64073537026862,
11.4854650250478));
#121297=CARTESIAN_POINT('Ctrl Pts',(-8.92446050673897,9.64114161040775,
11.4799442581331));
#121298=CARTESIAN_POINT('Ctrl Pts',(-8.91928820152738,9.64200657144456,
11.4681913644485));
#121299=CARTESIAN_POINT('Ctrl Pts',(-8.91660760805679,9.64246564924087,
11.4619546155768));
#121300=CARTESIAN_POINT('Ctrl Pts',(-8.90954178747643,9.64370557415027,
11.4451152560814));
#121301=CARTESIAN_POINT('Ctrl Pts',(-8.90525742805021,9.64448974344235,
11.4344713908661));
#121302=CARTESIAN_POINT('Ctrl Pts',(-8.88270771544209,9.6488014127095,11.3759977023578));
#121303=CARTESIAN_POINT('Ctrl Pts',(-8.86742305291574,9.65242513017925,
11.3270848210618));
#121304=CARTESIAN_POINT('Ctrl Pts',(-8.83884901407342,9.66118851389804,
11.2091542571005));
#121305=CARTESIAN_POINT('Ctrl Pts',(-8.82845434770677,9.66638037877928,
11.1396315267862));
#121306=CARTESIAN_POINT('Ctrl Pts',(-8.82191201484686,9.67444408567743,
11.0291231763896));
#121307=CARTESIAN_POINT('Ctrl Pts',(-8.82160750270993,9.67736266253232,
10.9885414829633));
#121308=CARTESIAN_POINT('Ctrl Pts',(-8.82372239782677,9.68070006440941,
10.940668469199));
#121309=CARTESIAN_POINT('Ctrl Pts',(-8.82411613454022,9.68120945654215,
10.9333188952218));
#121310=CARTESIAN_POINT('Ctrl Pts',(-8.82483221621325,9.68199242526599,
10.9219487108479));
#121311=CARTESIAN_POINT('Ctrl Pts',(-8.82510635104722,9.6822684888089,10.9179254079559));
#121312=CARTESIAN_POINT('Ctrl Pts',(-8.8256489176753,9.6827744809635,10.9105232688751));
#121313=CARTESIAN_POINT('Ctrl Pts',(-8.82591127053541,9.68300472273815,
10.9071441663436));
#121314=CARTESIAN_POINT('Ctrl Pts',(-8.82654357041775,9.68352856045989,
10.8994316961168));
#121315=CARTESIAN_POINT('Ctrl Pts',(-8.82692293512729,9.68382163683827,
10.895099202829));
#121316=CARTESIAN_POINT('Ctrl Pts',(-8.82817520730296,9.68472765255914,
10.8816551778761));
#121317=CARTESIAN_POINT('Ctrl Pts',(-8.82913036305045,9.68533629005852,
10.8725513922389));
#121318=CARTESIAN_POINT('Ctrl Pts',(-8.83162912416268,9.68675798246277,
10.8511433260401));
#121319=CARTESIAN_POINT('Ctrl Pts',(-8.83326112528838,9.68756690224357,
10.8388502641155));
#121320=CARTESIAN_POINT('Ctrl Pts',(-8.83990671039832,9.69048472615131,
10.7942086970315));
#121321=CARTESIAN_POINT('Ctrl Pts',(-8.84607437837803,9.6925493375411,10.7620452431849));
#121322=CARTESIAN_POINT('Ctrl Pts',(-8.86413699526466,9.69747139202525,
10.685300279843));
#121323=CARTESIAN_POINT('Ctrl Pts',(-8.87732570999502,9.70030494745551,
10.6410804229618));
#121324=CARTESIAN_POINT('Ctrl Pts',(-8.91572911921611,9.70728282471766,
10.5354012316572));
#121325=CARTESIAN_POINT('Ctrl Pts',(-8.94360883301637,9.71144941376279,
10.4750891845998));
#121326=CARTESIAN_POINT('Ctrl Pts',(-8.98244228216605,9.71659414637436,
10.4068559184069));
#121327=CARTESIAN_POINT('Ctrl Pts',(-8.98863473234494,9.71739824935399,
10.3963578145763));
#121328=CARTESIAN_POINT('Ctrl Pts',(-8.99864542462074,9.7186742113475,10.3799731731409));
#121329=CARTESIAN_POINT('Ctrl Pts',(-9.00235536146342,9.71914217107062,
10.3740212277713));
#121330=CARTESIAN_POINT('Ctrl Pts',(-9.0093519642638,9.72001589700007,10.3630165940065));
#121331=CARTESIAN_POINT('Ctrl Pts',(-9.01262470218902,9.72042114393834,
10.3579552903564));
#121332=CARTESIAN_POINT('Ctrl Pts',(-9.01606784208457,9.72084400708484,
10.3527190496997));
#121333=CARTESIAN_POINT('Ctrl Pts',(-9.01619965170182,9.72086018980727,
10.35251873024));
#121334=CARTESIAN_POINT('Ctrl Pts',(-9.0164529526398,9.72089127837934,10.3521340286093));
#121335=CARTESIAN_POINT('Ctrl Pts',(-9.01657443466254,9.72090618388388,
10.3519496403075));
#121336=CARTESIAN_POINT('Ctrl Pts',(-9.01680845570551,9.72093488907301,
10.3515946549447));
#121337=CARTESIAN_POINT('Ctrl Pts',(-9.01692098730145,9.72094868848224,
10.3514240529745));
#121338=CARTESIAN_POINT('Ctrl Pts',(-9.01713825082408,9.72097532352946,
10.3510948600706));
#121339=CARTESIAN_POINT('Ctrl Pts',(-9.01724297674637,9.72098815894416,
10.3509362651746));
#121340=CARTESIAN_POINT('Ctrl Pts',(-9.01744558753614,9.72101298498382,
10.3506295967978));
#121341=CARTESIAN_POINT('Ctrl Pts',(-9.01754346751164,9.72102497542761,
10.3504815200642));
#121342=CARTESIAN_POINT('Ctrl Pts',(-9.01773319653839,9.72104821198619,
10.35019463143));
#121343=CARTESIAN_POINT('Ctrl Pts',(-9.01782504155932,9.72105945795176,
10.350055816845));
#121344=CARTESIAN_POINT('Ctrl Pts',(-9.01800339037561,9.72108129100874,
10.3497863845396));
#121345=CARTESIAN_POINT('Ctrl Pts',(-9.01808989080319,9.72109187797388,
10.3496557646131));
#121346=CARTESIAN_POINT('Ctrl Pts',(-9.01825814153266,9.72111246621133,
10.3494018077736));
#121347=CARTESIAN_POINT('Ctrl Pts',(-9.01833988902623,9.72112246737942,
10.3492784689915));
#121348=CARTESIAN_POINT('Ctrl Pts',(-9.02241617728978,9.72162107085455,
10.343130773052));
#121349=CARTESIAN_POINT('Ctrl Pts',(-9.02646599233686,9.72211171933589,
10.3371434215258));
#121350=CARTESIAN_POINT('Ctrl Pts',(-9.03977072564902,9.7237088020395,10.3178583123283));
#121351=CARTESIAN_POINT('Ctrl Pts',(-9.04924463038598,9.72482338908638,
10.3047146461059));
#121352=CARTESIAN_POINT('Ctrl Pts',(-9.0720775327723,9.72745936479107,10.2743768893543));
#121353=CARTESIAN_POINT('Ctrl Pts',(-9.0856478372066,9.72898839171479,10.2573499996535));
#121354=CARTESIAN_POINT('Ctrl Pts',(-9.13796206439732,9.73474772757883,
10.1953190792775));
#121355=CARTESIAN_POINT('Ctrl Pts',(-9.17961663506222,9.73907834493517,
10.1528928404179));
#121356=CARTESIAN_POINT('Ctrl Pts',(-9.27539260322614,9.7484170785229,10.0690585304199));
#121357=CARTESIAN_POINT('Ctrl Pts',(-9.33027625887786,9.75341676628223,
10.0288256232234));
#121358=CARTESIAN_POINT('Ctrl Pts',(-9.39639606303814,9.75884661397003,
9.98864124952498));
#121359=CARTESIAN_POINT('Ctrl Pts',(-9.40452474727897,9.75950448171555,
9.98383393483351));
#121360=CARTESIAN_POINT('Ctrl Pts',(-9.41705058008964,9.76050252805791,
9.97662807134143));
#121361=CARTESIAN_POINT('Ctrl Pts',(-9.42140645578641,9.76084673776016,
9.9741590555037));
#121362=CARTESIAN_POINT('Ctrl Pts',(-9.42878724976407,9.76142499916493,
9.9700374105656));
#121363=CARTESIAN_POINT('Ctrl Pts',(-9.43180388728355,9.76165994844305,
9.96837016311263));
#121364=CARTESIAN_POINT('Ctrl Pts',(-9.43806089312858,9.7621443322034,9.96494778775583));
#121365=CARTESIAN_POINT('Ctrl Pts',(-9.44130223938692,9.76239364799356,
9.96319459148318));
#121366=CARTESIAN_POINT('Ctrl Pts',(-9.44981804728157,9.76304459025896,
9.95864004898167));
#121367=CARTESIAN_POINT('Ctrl Pts',(-9.45510576232724,9.76344470970256,
9.95586351363371));
#121368=CARTESIAN_POINT('Ctrl Pts',(-9.47924698774396,9.76525408402404,
9.94342049702607));
#121369=CARTESIAN_POINT('Ctrl Pts',(-9.4983393879207,9.76663715191732,9.93422295496629));
#121370=CARTESIAN_POINT('Ctrl Pts',(-9.61124012854633,9.77459945010247,
9.88354116297366));
#121371=CARTESIAN_POINT('Ctrl Pts',(-9.70989195838233,9.7807355707276,9.8539389107558));
#121372=CARTESIAN_POINT('Ctrl Pts',(-9.81114931872029,9.78720258982885,
9.83748957738858));
#121373=CARTESIAN_POINT('Origin',(-10.,2.67563288526385,11.));
#121374=CARTESIAN_POINT('',(-9.81114930150097,10.385472315614,9.83748958018587));
#121375=CARTESIAN_POINT('',(-9.81114930150157,10.287171250943,9.83748958018577));
#121376=CARTESIAN_POINT('',(-9.81114930150157,2.67563288526385,9.83748958018577));
#121377=CARTESIAN_POINT('Ctrl Pts',(-9.81114930150037,10.385472315614,9.83748958018597));
#121378=CARTESIAN_POINT('Ctrl Pts',(-9.80901865393688,10.3853241363018,
9.83783570549699));
#121379=CARTESIAN_POINT('Ctrl Pts',(-9.80688893621724,10.3851762668984,
9.83818769190922));
#121380=CARTESIAN_POINT('Ctrl Pts',(-9.80137111344281,10.3847938131546,
9.83911523474365));
#121381=CARTESIAN_POINT('Ctrl Pts',(-9.79798450088191,10.3845597242658,
9.83969977499039));
#121382=CARTESIAN_POINT('Ctrl Pts',(-9.79085865717225,10.3840685805468,
9.84096186392286));
#121383=CARTESIAN_POINT('Ctrl Pts',(-9.78712009935092,10.3838117083245,
9.84164269282486));
#121384=CARTESIAN_POINT('Ctrl Pts',(-9.77700493425228,10.383118727767,9.84353539120436));
#121385=CARTESIAN_POINT('Ctrl Pts',(-9.77063483055417,10.3826844973983,
9.84478191906313));
#121386=CARTESIAN_POINT('Ctrl Pts',(-9.74039221174691,10.380631922259,9.8509599405518));
#121387=CARTESIAN_POINT('Ctrl Pts',(-9.71666447833965,10.379048130933,9.85657950056329));
#121388=CARTESIAN_POINT('Ctrl Pts',(-9.68157964884264,10.3767230771455,
9.86604824544442));
#121389=CARTESIAN_POINT('Ctrl Pts',(-9.67008068569605,10.3759637879132,
9.86934029724323));
#121390=CARTESIAN_POINT('Ctrl Pts',(-9.60005324488689,10.3713457699839,
9.89054786214394));
#121391=CARTESIAN_POINT('Ctrl Pts',(-9.54294276551046,10.3676007600548,
9.91282899400435));
#121392=CARTESIAN_POINT('Ctrl Pts',(-9.43275573165214,10.3600018520841,
9.9660423712307));
#121393=CARTESIAN_POINT('Ctrl Pts',(-9.37985172576072,10.3561585951765,
9.99688026163735));
#121394=CARTESIAN_POINT('Ctrl Pts',(-9.31783649874031,10.3512341924403,
10.0398165853582));
#121395=CARTESIAN_POINT('Ctrl Pts',(-9.30623802895158,10.3502940166443,
10.0481630753736));
#121396=CARTESIAN_POINT('Ctrl Pts',(-9.28888383701256,10.348856164818,10.0611372141539));
#121397=CARTESIAN_POINT('Ctrl Pts',(-9.28301478567254,10.3483643506024,
10.0656115763813));
#121398=CARTESIAN_POINT('Ctrl Pts',(-9.27242774770514,10.3474668119295,
10.0738412464389));
#121399=CARTESIAN_POINT('Ctrl Pts',(-9.26769577783842,10.3470618128797,
10.0775782184907));
#121400=CARTESIAN_POINT('Ctrl Pts',(-9.25752961857975,10.3461832474682,
10.0857342554353));
#121401=CARTESIAN_POINT('Ctrl Pts',(-9.25210576233181,10.3457091969369,
10.0901657708273));
#121402=CARTESIAN_POINT('Ctrl Pts',(-9.23738924506434,10.34440811294,10.1024102878799));
#121403=CARTESIAN_POINT('Ctrl Pts',(-9.22817757358346,10.3435772629782,
10.1103188336145));
#121404=CARTESIAN_POINT('Ctrl Pts',(-9.17059101114898,10.3382758630526,
10.1613264229501));
#121405=CARTESIAN_POINT('Ctrl Pts',(-9.12572741545361,10.3336473690437,
10.2082061006038));
#121406=CARTESIAN_POINT('Ctrl Pts',(-9.0301413438192,10.3225841260118,10.3261687593772));
#121407=CARTESIAN_POINT('Ctrl Pts',(-8.98299996017106,10.3161000792904,
10.3996782553392));
#121408=CARTESIAN_POINT('Ctrl Pts',(-8.93849786779084,10.3090165172813,
10.4896228477336));
#121409=CARTESIAN_POINT('Ctrl Pts',(-8.9328071225575,10.3080874931541,10.5016316487003));
#121410=CARTESIAN_POINT('Ctrl Pts',(-8.92523864428582,10.3068212502874,
10.5183273758546));
#121411=CARTESIAN_POINT('Ctrl Pts',(-8.92318621215167,10.3064745484479,
10.5229333828439));
#121412=CARTESIAN_POINT('Ctrl Pts',(-8.91976399584554,10.3058909326453,
10.5307480342843));
#121413=CARTESIAN_POINT('Ctrl Pts',(-8.91837878477369,10.3056531171588,
10.5339498095624));
#121414=CARTESIAN_POINT('Ctrl Pts',(-8.91555962669803,10.3051658888952,
10.5405462826958));
#121415=CARTESIAN_POINT('Ctrl Pts',(-8.91412735710677,10.304916574061,10.5439416200212));
#121416=CARTESIAN_POINT('Ctrl Pts',(-8.91041692483366,10.3042658446329,
10.5528541480393));
#121417=CARTESIAN_POINT('Ctrl Pts',(-8.90816469160973,10.3038659345682,
10.5583821180139));
#121418=CARTESIAN_POINT('Ctrl Pts',(-8.89890668807222,10.3022001189235,
10.5816091455266));
#121419=CARTESIAN_POINT('Ctrl Pts',(-8.8922880690545,10.3009549055186,10.5994606568881));
#121420=CARTESIAN_POINT('Ctrl Pts',(-8.88015178480883,10.2985434794403,
10.6348001258412));
#121421=CARTESIAN_POINT('Ctrl Pts',(-8.87460404174534,10.297376393813,10.652271699045));
#121422=CARTESIAN_POINT('Ctrl Pts',(-8.85231468746043,10.2923578204032,
10.7286010092507));
#121423=CARTESIAN_POINT('Ctrl Pts',(-8.8397657908465,10.2886140266636,10.7885851805867));
#121424=CARTESIAN_POINT('Ctrl Pts',(-8.82638754072009,10.2821221852604,
10.8922618935437));
#121425=CARTESIAN_POINT('Ctrl Pts',(-8.82321816208708,10.2794083401122,
10.9355191768748));
#121426=CARTESIAN_POINT('Ctrl Pts',(-8.82211597393611,10.2754756646011,
10.9968866780313));
#121427=CARTESIAN_POINT('Ctrl Pts',(-8.82220646974194,10.2743097013499,
11.0149271686104));
#121428=CARTESIAN_POINT('Ctrl Pts',(-8.82310657662545,10.2722091344293,
11.0470799920346));
#121429=CARTESIAN_POINT('Ctrl Pts',(-8.82375598102475,10.2712793549658,
11.0611934288648));
#121430=CARTESIAN_POINT('Ctrl Pts',(-8.82512879344959,10.269854175078,11.0826238295905));
#121431=CARTESIAN_POINT('Ctrl Pts',(-8.82566710723015,10.2693644769871,
11.0899516651189));
#121432=CARTESIAN_POINT('Ctrl Pts',(-8.82677182083556,10.2684691421378,
11.1032813645461));
#121433=CARTESIAN_POINT('Ctrl Pts',(-8.82731580772734,10.2680642127124,
11.1092848733099));
#121434=CARTESIAN_POINT('Ctrl Pts',(-8.82859404398805,10.2671838847777,
11.1222807376632));
#121435=CARTESIAN_POINT('Ctrl Pts',(-8.82934486372115,10.2667079867487,
11.1292711908589));
#121436=CARTESIAN_POINT('Ctrl Pts',(-8.83157650266895,10.2653968716313,
11.1484314161075));
#121437=CARTESIAN_POINT('Ctrl Pts',(-8.83318478637407,10.264557740133,11.1605851549259));
#121438=CARTESIAN_POINT('Ctrl Pts',(-8.84550380420088,10.2587672285939,
11.2436826790302));
#121439=CARTESIAN_POINT('Ctrl Pts',(-8.862486347632,10.2536194438306,11.3135316183597));
#121440=CARTESIAN_POINT('Ctrl Pts',(-8.90277680409362,10.2445255288309,
11.4312459212113));
#121441=CARTESIAN_POINT('Ctrl Pts',(-8.92316751660878,10.2406368184134,
11.4798996261221));
#121442=CARTESIAN_POINT('Ctrl Pts',(-8.96310822090906,10.2341549052335,
11.5597206450897));
#121443=CARTESIAN_POINT('Ctrl Pts',(-8.98098407378706,10.2315339282751,
11.5916408262308));
#121444=CARTESIAN_POINT('Ctrl Pts',(-9.00401565860117,10.2285040565285,
11.6286168683901));
#121445=CARTESIAN_POINT('Ctrl Pts',(-9.00776621475628,10.2280205314956,
11.6345203675979));
#121446=CARTESIAN_POINT('Ctrl Pts',(-9.01369505309372,10.2272717736742,
11.6436714217074));
#121447=CARTESIAN_POINT('Ctrl Pts',(-9.01583722032277,10.2270043198606,
11.6469420156628));
#121448=CARTESIAN_POINT('Ctrl Pts',(-9.01987692689434,10.2265057688019,
11.6530432114334));
#121449=CARTESIAN_POINT('Ctrl Pts',(-9.02177045959044,10.2262744359305,
11.6558762391433));
#121450=CARTESIAN_POINT('Ctrl Pts',(-9.02616906100948,10.2257423962922,
11.6623958252496));
#121451=CARTESIAN_POINT('Ctrl Pts',(-9.02868279048243,10.2254422662415,
11.6660764274075));
#121452=CARTESIAN_POINT('Ctrl Pts',(-9.0368979624016,10.2244737006971,11.6779596700908));
#121453=CARTESIAN_POINT('Ctrl Pts',(-9.04268306253631,10.2238105373222,
11.6861043262969));
#121454=CARTESIAN_POINT('Ctrl Pts',(-9.09388370336655,10.2180932540946,
11.7562793942878));
#121455=CARTESIAN_POINT('Ctrl Pts',(-9.14517478797374,10.2133749096299,
11.8138074119133));
#121456=CARTESIAN_POINT('Ctrl Pts',(-9.25195686906547,10.2043889820855,
11.912247829077));
#121457=CARTESIAN_POINT('Ctrl Pts',(-9.30612918828313,10.2001455722198,
11.9540998653966));
#121458=CARTESIAN_POINT('Ctrl Pts',(-9.37997676132295,10.1944644593128,
12.0015208861984));
#121459=CARTESIAN_POINT('Ctrl Pts',(-9.39658964797795,10.1931933308712,
12.0116169133594));
#121460=CARTESIAN_POINT('Ctrl Pts',(-9.42066292059268,10.1913568153999,
12.0254427886401));
#121461=CARTESIAN_POINT('Ctrl Pts',(-9.4279254211099,10.190803469697,12.0295120371455));
#121462=CARTESIAN_POINT('Ctrl Pts',(-9.44062055374436,10.189837089304,12.0364494337988));
#121463=CARTESIAN_POINT('Ctrl Pts',(-9.44603368236305,10.1894253081422,
12.0393527361814));
#121464=CARTESIAN_POINT('Ctrl Pts',(-9.45721943217093,10.1885748378738,
12.0452399448286));
#121465=CARTESIAN_POINT('Ctrl Pts',(-9.46299452244783,10.1881359862442,
12.0482186800673));
#121466=CARTESIAN_POINT('Ctrl Pts',(-9.47782986725035,10.1870090845652,
12.05571583124));
#121467=CARTESIAN_POINT('Ctrl Pts',(-9.4869241182467,10.186318694758,12.0601654080086));
#121468=CARTESIAN_POINT('Ctrl Pts',(-9.52350079821706,10.1835428887661,
12.0774805583007));
#121469=CARTESIAN_POINT('Ctrl Pts',(-9.55141639784078,10.1814259962953,
12.0893981398639));
#121470=CARTESIAN_POINT('Ctrl Pts',(-9.6653653704601,10.1727864107622,12.1329220490494));
#121471=CARTESIAN_POINT('Ctrl Pts',(-9.75448857278884,10.1660001839393,
12.1555140137383));
#121472=CARTESIAN_POINT('Ctrl Pts',(-9.88440660426491,10.1564431663294,
12.1727269753214));
#121473=CARTESIAN_POINT('Ctrl Pts',(-9.92374220836997,10.1535978001401,
12.1759403722289));
#121474=CARTESIAN_POINT('Ctrl Pts',(-9.9725950795899,10.1501759802145,12.1774688878563));
#121475=CARTESIAN_POINT('Ctrl Pts',(-9.98202532438966,10.1495206518886,
12.1776506003725));
#121476=CARTESIAN_POINT('Ctrl Pts',(-9.99585925486454,10.1485678807776,
12.1777509485204));
#121477=CARTESIAN_POINT('Ctrl Pts',(-10.0002616464349,10.1482659533288,
12.1777581991312));
#121478=CARTESIAN_POINT('Ctrl Pts',(-10.0080582213571,10.1477336207909,
12.1777273233041));
#121479=CARTESIAN_POINT('Ctrl Pts',(-10.0114523193918,10.1475026837675,
12.1776992096452));
#121480=CARTESIAN_POINT('Ctrl Pts',(-10.0188413690828,10.1470016950095,
12.1776060579574));
#121481=CARTESIAN_POINT('Ctrl Pts',(-10.0228361440019,10.146731953355,12.1775353653439));
#121482=CARTESIAN_POINT('Ctrl Pts',(-10.0340185504667,10.1459797913893,
12.1772805506011));
#121483=CARTESIAN_POINT('Ctrl Pts',(-10.0412051151877,10.1454997732333,
12.1770509340774));
#121484=CARTESIAN_POINT('Ctrl Pts',(-10.0848526923941,10.1426024266976,
12.1752561027433));
#121485=CARTESIAN_POINT('Ctrl Pts',(-10.1212306846842,10.1402639367501,
12.1720625316576));
#121486=CARTESIAN_POINT('Ctrl Pts',(-10.2682742420256,10.1309134072535,
12.1522323949297));
#121487=CARTESIAN_POINT('Ctrl Pts',(-10.376443399477,10.124213050488,12.1215623876192));
#121488=CARTESIAN_POINT('Ctrl Pts',(-10.4972292166454,10.1156668605729,
12.0678347207529));
#121489=CARTESIAN_POINT('Ctrl Pts',(-10.5155757364185,10.1143394506538,
12.0590984211393));
#121490=CARTESIAN_POINT('Ctrl Pts',(-10.5412354941172,10.1124360206062,
12.0460549311523));
#121491=CARTESIAN_POINT('Ctrl Pts',(-10.5487429254111,10.1118733096992,
12.0421362553317));
#121492=CARTESIAN_POINT('Ctrl Pts',(-10.5616432108252,10.1108959462641,
12.0352246122339));
#121493=CARTESIAN_POINT('Ctrl Pts',(-10.5670560878653,10.1104826301208,
12.0322695795174));
#121494=CARTESIAN_POINT('Ctrl Pts',(-10.5780825109515,10.1096339268534,
12.0261370663789));
#121495=CARTESIAN_POINT('Ctrl Pts',(-10.5836936507828,10.1091984132654,
12.0229557114803));
#121496=CARTESIAN_POINT('Ctrl Pts',(-10.5978500056684,10.1080902677247,
12.0147750706219));
#121497=CARTESIAN_POINT('Ctrl Pts',(-10.6063586987922,10.1074154466459,
12.0097139155532));
#121498=CARTESIAN_POINT('Ctrl Pts',(-10.639127271279,10.1047816295369,11.9896588946422));
#121499=CARTESIAN_POINT('Ctrl Pts',(-10.6629014561146,10.1027951030559,
11.973894150424));
#121500=CARTESIAN_POINT('Ctrl Pts',(-10.7544619628815,10.0948339223381,
11.9082733543169));
#121501=CARTESIAN_POINT('Ctrl Pts',(-10.8173896212803,10.0886374248943,
11.852082107418));
#121502=CARTESIAN_POINT('Ctrl Pts',(-10.8788028811276,10.0819307434755,
11.7841278894994));
#121503=CARTESIAN_POINT('Ctrl Pts',(-10.8837669353067,10.0813834925766,
11.7785287770944));
#121504=CARTESIAN_POINT('Ctrl Pts',(-10.9088181494688,10.0785964622036,
11.7497243463314));
#121505=CARTESIAN_POINT('Ctrl Pts',(-10.9280474112327,10.0763724346722,
11.7257859697885));
#121506=CARTESIAN_POINT('Ctrl Pts',(-10.9534046025276,10.0733431379989,
11.6915607932475));
#121507=CARTESIAN_POINT('Ctrl Pts',(-10.9603435967534,10.0725032124597,
11.6818921226765));
#121508=CARTESIAN_POINT('Ctrl Pts',(-10.9721963356003,10.0710511755734,
11.664836823074));
#121509=CARTESIAN_POINT('Ctrl Pts',(-10.9771753009775,10.0704355872511,
11.6574968890905));
#121510=CARTESIAN_POINT('Ctrl Pts',(-10.9844417902834,10.0695294800027,
11.6465198143342));
#121511=CARTESIAN_POINT('Ctrl Pts',(-10.9867929604971,10.0692350607974,
11.6429254726311));
#121512=CARTESIAN_POINT('Ctrl Pts',(-10.9907860906683,10.0687330044068,
11.6367474813839));
#121513=CARTESIAN_POINT('Ctrl Pts',(-10.992437697833,10.0685247463666,11.6341702052227));
#121514=CARTESIAN_POINT('Ctrl Pts',(-10.9961911124559,10.0680500924463,
11.6282625548572));
#121515=CARTESIAN_POINT('Ctrl Pts',(-10.9982862814403,10.0677841280645,
11.6249280532942));
#121516=CARTESIAN_POINT('Ctrl Pts',(-11.0040250740278,10.0670526390294,
11.6156921423218));
#121517=CARTESIAN_POINT('Ctrl Pts',(-11.0076334262963,10.0665893109604,
11.6097688474448));
#121518=CARTESIAN_POINT('Ctrl Pts',(-11.0274612749347,10.0640221138178,
11.5765637306348));
#121519=CARTESIAN_POINT('Ctrl Pts',(-11.042626660284,10.0619776231043,11.5486642410104));
#121520=CARTESIAN_POINT('Ctrl Pts',(-11.0847374688505,10.0559372745275,
11.4631246474535));
#121521=CARTESIAN_POINT('Ctrl Pts',(-11.1081608318639,10.0520477490289,
11.4038814842948));
#121522=CARTESIAN_POINT('Ctrl Pts',(-11.1395540968116,10.0453574677012,
11.3007710908776));
#121523=CARTESIAN_POINT('Ctrl Pts',(-11.1500325435245,10.0425936214176,
11.2578206525288));
#121524=CARTESIAN_POINT('Ctrl Pts',(-11.161396683861,10.038595204308,11.196433499557));
#121525=CARTESIAN_POINT('Ctrl Pts',(-11.1643019695358,10.0374155875785,
11.178407532631));
#121526=CARTESIAN_POINT('Ctrl Pts',(-11.1687282071296,10.0352926518581,
11.146194385809));
#121527=CARTESIAN_POINT('Ctrl Pts',(-11.1704125890949,10.0343543110073,
11.1320331904748));
#121528=CARTESIAN_POINT('Ctrl Pts',(-11.172577253173,10.0329186951408,11.1105080484999));
#121529=CARTESIAN_POINT('Ctrl Pts',(-11.1732461847603,10.032427253641,11.1031640889303));
#121530=CARTESIAN_POINT('Ctrl Pts',(-11.1743366042695,10.0315301043074,
11.089805097426));
#121531=CARTESIAN_POINT('Ctrl Pts',(-11.1747809539501,10.0311251186999,
11.0837921450878));
#121532=CARTESIAN_POINT('Ctrl Pts',(-11.1756419443467,10.0302462485327,
11.0707827835452));
#121533=CARTESIAN_POINT('Ctrl Pts',(-11.1760423382264,10.0297718771316,
11.0637855687921));
#121534=CARTESIAN_POINT('Ctrl Pts',(-11.1769665991841,10.028469052508,11.0446383274545));
#121535=CARTESIAN_POINT('Ctrl Pts',(-11.1773647549391,10.027636765878,11.0324833880006));
#121536=CARTESIAN_POINT('Ctrl Pts',(-11.1788670097181,10.0216375951394,
10.9454462200042));
#121537=CARTESIAN_POINT('Ctrl Pts',(-11.1730144356616,10.016255100776,10.8706287511743));
#121538=CARTESIAN_POINT('Ctrl Pts',(-11.1496065400018,10.0063241740616,
10.7369326639045));
#121539=CARTESIAN_POINT('Ctrl Pts',(-11.1344779464935,10.001827147489,10.6778823269995));
#121540=CARTESIAN_POINT('Ctrl Pts',(-11.109123790337,9.99616905279425,10.6034458767436));
#121541=CARTESIAN_POINT('Ctrl Pts',(-11.1030148535012,9.9949017499612,10.5867578717978));
#121542=CARTESIAN_POINT('Ctrl Pts',(-11.0921506344577,9.99280558923922,
10.5590395762574));
#121543=CARTESIAN_POINT('Ctrl Pts',(-11.0876001892522,9.99196805981675,
10.5479325716764));
#121544=CARTESIAN_POINT('Ctrl Pts',(-11.0809749711376,9.99080518356035,
10.5324407420751));
#121545=CARTESIAN_POINT('Ctrl Pts',(-11.0790418797436,9.9904722115102,10.527996640135));
#121546=CARTESIAN_POINT('Ctrl Pts',(-11.0756844832104,9.98990474565607,
10.5204065481754));
#121547=CARTESIAN_POINT('Ctrl Pts',(-11.0742736859224,9.98966946422608,
10.5172546888228));
#121548=CARTESIAN_POINT('Ctrl Pts',(-11.071299258808,9.98918002301297,10.5106871438213));
#121549=CARTESIAN_POINT('Ctrl Pts',(-11.069733128387,9.98892601494905,10.5072726837606));
#121550=CARTESIAN_POINT('Ctrl Pts',(-11.0654998021698,9.9882490559596,10.4981585581365));
#121551=CARTESIAN_POINT('Ctrl Pts',(-11.0628031733358,9.98782783755301,
10.4924725817508));
#121552=CARTESIAN_POINT('Ctrl Pts',(-11.050422214748,9.98593709943094,10.4668981762408));
#121553=CARTESIAN_POINT('Ctrl Pts',(-11.0402236369813,9.98449585061446,
10.4472619807246));
#121554=CARTESIAN_POINT('Ctrl Pts',(-11.018858366515,9.98167188384095,10.4088142360255));
#121555=CARTESIAN_POINT('Ctrl Pts',(-11.0077090153751,9.98028923564516,
10.390003598347));
#121556=CARTESIAN_POINT('Ctrl Pts',(-10.9847977925115,9.97759709328722,
10.3536932939783));
#121557=CARTESIAN_POINT('Ctrl Pts',(-10.9730771274872,9.97628726498755,
10.3361777383488));
#121558=CARTESIAN_POINT('Ctrl Pts',(-10.9320107305756,9.97188542225476,
10.2782341718334));
#121559=CARTESIAN_POINT('Ctrl Pts',(-10.9005664146903,9.96881344615436,
10.2393621733329));
#121560=CARTESIAN_POINT('Ctrl Pts',(-10.8334741801638,9.96260284621545,
10.1664345447527));
#121561=CARTESIAN_POINT('Ctrl Pts',(-10.7979709371211,9.95947212324639,
10.1323871331149));
#121562=CARTESIAN_POINT('Ctrl Pts',(-10.7517733962769,9.95549965017358,
10.0933242745445));
#121563=CARTESIAN_POINT('Ctrl Pts',(-10.7429934385777,9.95474898025505,
10.0861155182275));
#121564=CARTESIAN_POINT('Ctrl Pts',(-10.7288207624926,9.953543213175,10.074818328926));
#121565=CARTESIAN_POINT('Ctrl Pts',(-10.7234945635506,9.95309139058837,
10.0706472996617));
#121566=CARTESIAN_POINT('Ctrl Pts',(-10.7133306329849,9.95223148362811,
10.0628280948171));
#121567=CARTESIAN_POINT('Ctrl Pts',(-10.7085000897431,9.95182376900533,
10.0591709016499));
#121568=CARTESIAN_POINT('Ctrl Pts',(-10.6974416438909,9.95089245966032,
10.0509320402588));
#121569=CARTESIAN_POINT('Ctrl Pts',(-10.6911964655906,9.95036797532428,
10.0463741405225));
#121570=CARTESIAN_POINT('Ctrl Pts',(-10.671816708427,9.94874460840205,10.0325206508186));
#121571=CARTESIAN_POINT('Ctrl Pts',(-10.6585366243807,9.94763800722059,
10.0234328231667));
#121572=CARTESIAN_POINT('Ctrl Pts',(-10.5870542269926,9.94170913329293,
9.9766371438205));
#121573=CARTESIAN_POINT('Ctrl Pts',(-10.5258014668674,9.9367121835445,9.94385883884487));
#121574=CARTESIAN_POINT('Ctrl Pts',(-10.4065664149515,9.92722568950665,
9.89300642346206));
#121575=CARTESIAN_POINT('Ctrl Pts',(-10.3493652962279,9.92277150964326,
9.87364511897384));
#121576=CARTESIAN_POINT('Ctrl Pts',(-10.2737964126132,9.91716098639665,
9.85438082680134));
#121577=CARTESIAN_POINT('Ctrl Pts',(-10.2565638544502,9.915899863062,9.85039884223858));
#121578=CARTESIAN_POINT('Ctrl Pts',(-10.2275369426201,9.91381277906313,
9.84437677578661));
#121579=CARTESIAN_POINT('Ctrl Pts',(-10.2157897183693,9.91297823677459,
9.8421256883715));
#121580=CARTESIAN_POINT('Ctrl Pts',(-10.1992433630736,9.91181875781252,
9.83921553878035));
#121581=CARTESIAN_POINT('Ctrl Pts',(-10.1944718062914,9.91148625344596,
9.83840661083375));
#121582=CARTESIAN_POINT('Ctrl Pts',(-10.1862883879155,9.91091933285136,
9.83707110485011));
#121583=CARTESIAN_POINT('Ctrl Pts',(-10.1828789821384,9.91068413285715,
9.83653007868065));
#121584=CARTESIAN_POINT('Ctrl Pts',(-10.175751902392,9.91019459231923,9.83543121182761));
#121585=CARTESIAN_POINT('Ctrl Pts',(-10.1720338830041,9.90994040546051,
9.83487617066981));
#121586=CARTESIAN_POINT('Ctrl Pts',(-10.1620728356242,9.90926244725283,
9.83343786596021));
#121587=CARTESIAN_POINT('Ctrl Pts',(-10.1558251604455,9.9088404173545,9.83258690244145));
#121588=CARTESIAN_POINT('Ctrl Pts',(-10.1274951240876,9.90693994117975,
9.82895970213356));
#121589=CARTESIAN_POINT('Ctrl Pts',(-10.1053420673119,9.90549012543356,
9.82675936551118));
#121590=CARTESIAN_POINT('Ctrl Pts',(-10.0613550350741,9.90265958900217,
9.82364651981266));
#121591=CARTESIAN_POINT('Ctrl Pts',(-10.039532018702,9.9012786418376,9.82271105470953));
#121592=CARTESIAN_POINT('Ctrl Pts',(-9.99674692403357,9.89859585072934,
9.82206817432506));
#121593=CARTESIAN_POINT('Ctrl Pts',(-9.97579404795538,9.89729357032893,
9.82231240126855));
#121594=CARTESIAN_POINT('Ctrl Pts',(-9.90670392384635,9.89300823891411,
9.82496248113367));
#121595=CARTESIAN_POINT('Ctrl Pts',(-9.85871097048288,9.89004376809584,
9.82976315099974));
#121596=CARTESIAN_POINT('Ctrl Pts',(-9.811149300931,9.88702732255485,9.83748958027846));
#121597=CARTESIAN_POINT('Ctrl Pts',(-9.81114931871824,9.78720258982872,
9.83748957738891));
#121598=CARTESIAN_POINT('Ctrl Pts',(-9.8523278733838,9.78983254678884,9.83080009060967));
#121599=CARTESIAN_POINT('Ctrl Pts',(-9.89381879494177,9.79250430083039,
9.82630478299562));
#121600=CARTESIAN_POINT('Ctrl Pts',(-9.94356232370296,9.79577764382975,
9.82357508836557));
#121601=CARTESIAN_POINT('Ctrl Pts',(-9.95166122798493,9.79631274306618,
9.8232144877574));
#121602=CARTESIAN_POINT('Ctrl Pts',(-9.96582342516913,9.79725254629638,
9.82273036422669));
#121603=CARTESIAN_POINT('Ctrl Pts',(-9.97188521447495,9.79765611754449,
9.82257000627575));
#121604=CARTESIAN_POINT('Ctrl Pts',(-9.9836655472331,9.79844308986436,9.82234939334581));
#121605=CARTESIAN_POINT('Ctrl Pts',(-9.98938383241838,9.79882632102659,
9.82228396430817));
#121606=CARTESIAN_POINT('Ctrl Pts',(-10.0007332813967,9.7995894818911,9.82223676679376));
#121607=CARTESIAN_POINT('Ctrl Pts',(-10.0063642896939,9.7999693623216,9.8222537348324));
#121608=CARTESIAN_POINT('Ctrl Pts',(-10.0195317398902,9.80086066579966,
9.82238784660003));
#121609=CARTESIAN_POINT('Ctrl Pts',(-10.0270675365127,9.80137306094949,
9.82253695744159));
#121610=CARTESIAN_POINT('Ctrl Pts',(-10.0530039667011,9.8031448019985,9.82329927544956));
#121611=CARTESIAN_POINT('Ctrl Pts',(-10.0713905314373,9.80441507000134,
9.8242715697791));
#121612=CARTESIAN_POINT('Ctrl Pts',(-10.1324181164698,9.80868100564058,
9.8289355019231));
#121613=CARTESIAN_POINT('Ctrl Pts',(-10.1748762279876,9.81173137673236,
9.83451975368101));
#121614=CARTESIAN_POINT('Ctrl Pts',(-10.311795516664,9.82181489848881,9.86017823505895));
#121615=CARTESIAN_POINT('Ctrl Pts',(-10.4041093057615,9.82903379542414,
9.88954724361765));
#121616=CARTESIAN_POINT('Ctrl Pts',(-10.5054153235497,9.83692809199575,
9.93610394986887));
#121617=CARTESIAN_POINT('Ctrl Pts',(-10.5189067352052,9.83797792414632,
9.94261865595356));
#121618=CARTESIAN_POINT('Ctrl Pts',(-10.5369787281021,9.83937869249076,
9.95177447073537));
#121619=CARTESIAN_POINT('Ctrl Pts',(-10.5416705550233,9.83974184712636,
9.95419125692172));
#121620=CARTESIAN_POINT('Ctrl Pts',(-10.5494772870861,9.84034505006163,
9.95827918027376));
#121621=CARTESIAN_POINT('Ctrl Pts',(-10.552601155317,9.84058613876326,9.95993292548676));
#121622=CARTESIAN_POINT('Ctrl Pts',(-10.5585232240598,9.84104257664747,
9.96310222458633));
#121623=CARTESIAN_POINT('Ctrl Pts',(-10.5613227945275,9.84125809491405,
9.96461509117329));
#121624=CARTESIAN_POINT('Ctrl Pts',(-10.5687422680068,9.84182867680468,
9.96866345622333));
#121625=CARTESIAN_POINT('Ctrl Pts',(-10.5733514098863,9.84218252587693,
9.97121868342542));
#121626=CARTESIAN_POINT('Ctrl Pts',(-10.5899552324494,9.8434555838853,9.98056979818936));
#121627=CARTESIAN_POINT('Ctrl Pts',(-10.601848045967,9.84436433026698,9.98754551590718));
#121628=CARTESIAN_POINT('Ctrl Pts',(-10.6795426477743,9.8502990617593,10.0349702014326));
#121629=CARTESIAN_POINT('Ctrl Pts',(-10.7413588424396,9.85502021041961,
10.0816042601525));
#121630=CARTESIAN_POINT('Ctrl Pts',(-10.8344700822246,9.86286215657187,
10.1674185152224));
#121631=CARTESIAN_POINT('Ctrl Pts',(-10.8686302721791,9.8659355375177,10.2031228682169));
#121632=CARTESIAN_POINT('Ctrl Pts',(-10.913048807546,9.87033822437074,10.2558097441577));
#121633=CARTESIAN_POINT('Ctrl Pts',(-10.9252753294953,9.87159875525423,
10.2710673813529));
#121634=CARTESIAN_POINT('Ctrl Pts',(-10.9461591585574,9.87384668091376,
10.2985010274177));
#121635=CARTESIAN_POINT('Ctrl Pts',(-10.9549752892441,9.87482801611236,
10.3105508530133));
#121636=CARTESIAN_POINT('Ctrl Pts',(-10.9678306337069,9.87631056658614,
10.3288412306251));
#121637=CARTESIAN_POINT('Ctrl Pts',(-10.9720439284502,9.87680522282221,
10.3349580267463));
#121638=CARTESIAN_POINT('Ctrl Pts',(-10.9762546223322,9.87730869480909,
10.341196550739));
#121639=CARTESIAN_POINT('Ctrl Pts',(-10.9763102281505,9.87731534522267,
10.3412789582898));
#121640=CARTESIAN_POINT('Ctrl Pts',(-10.9764240026447,9.87732895591257,
10.3414476175867));
#121641=CARTESIAN_POINT('Ctrl Pts',(-10.9764821703287,9.87733591622579,
10.341533870003));
#121642=CARTESIAN_POINT('Ctrl Pts',(-10.9766012020463,9.87735016316377,
10.3417104235061));
#121643=CARTESIAN_POINT('Ctrl Pts',(-10.9766620649907,9.87735744982969,
10.341800725337));
#121644=CARTESIAN_POINT('Ctrl Pts',(-10.9767866285292,9.87737236691389,
10.3419855945139));
#121645=CARTESIAN_POINT('Ctrl Pts',(-10.9768503279104,9.87737999737614,
10.3420801626625));
#121646=CARTESIAN_POINT('Ctrl Pts',(-10.9769807137374,9.87739562052947,
10.3422737942382));
#121647=CARTESIAN_POINT('Ctrl Pts',(-10.9770473988811,9.8774036132734,10.3423728586042));
#121648=CARTESIAN_POINT('Ctrl Pts',(-10.9771839144923,9.87741998059714,
10.3425757264834));
#121649=CARTESIAN_POINT('Ctrl Pts',(-10.9772537434496,9.87742835522663,
10.3426795309249));
#121650=CARTESIAN_POINT('Ctrl Pts',(-10.9773967138817,9.8774455070784,10.3428921371793));
#121651=CARTESIAN_POINT('Ctrl Pts',(-10.9774698537432,9.87745428436218,
10.343000940099));
#121652=CARTESIAN_POINT('Ctrl Pts',(-10.9776196228563,9.87747226352813,
10.3432238171254));
#121653=CARTESIAN_POINT('Ctrl Pts',(-10.9776962503026,9.87748146547562,
10.3433378924218));
#121654=CARTESIAN_POINT('Ctrl Pts',(-10.9778180379123,9.87749609555491,
10.343519266237));
#121655=CARTESIAN_POINT('Ctrl Pts',(-10.9778632111151,9.8775015232052,10.3435865560364));
#121656=CARTESIAN_POINT('Ctrl Pts',(-10.9779649073965,9.87751374467584,
10.3437380761536));
#121657=CARTESIAN_POINT('Ctrl Pts',(-10.9780214265277,9.87752053864082,
10.3438223090943));
#121658=CARTESIAN_POINT('Ctrl Pts',(-10.9781486559982,9.877535836301,10.3440119777118));
#121659=CARTESIAN_POINT('Ctrl Pts',(-10.9782193601631,9.87754434022368,
10.3441174175063));
#121660=CARTESIAN_POINT('Ctrl Pts',(-10.9783785031417,9.87756348714072,
10.3443548274198));
#121661=CARTESIAN_POINT('Ctrl Pts',(-10.9784669322995,9.87757413049253,
10.3444868039972));
#121662=CARTESIAN_POINT('Ctrl Pts',(-10.9786659356483,9.87759809204481,
10.3447839376166));
#121663=CARTESIAN_POINT('Ctrl Pts',(-10.9787764947074,9.87761141080147,
10.3449491047165));
#121664=CARTESIAN_POINT('Ctrl Pts',(-10.9790252299308,9.87764139010588,
10.3453209004046));
#121665=CARTESIAN_POINT('Ctrl Pts',(-10.9791633824834,9.87765805152672,
10.3455275447418));
#121666=CARTESIAN_POINT('Ctrl Pts',(-10.9794469019112,9.87769226561721,
10.3459519150913));
#121667=CARTESIAN_POINT('Ctrl Pts',(-10.9795922616295,9.87770981855088,
10.3461696458624));
#121668=CARTESIAN_POINT('Ctrl Pts',(-10.9831001393132,9.87813368960713,
10.3514278058397));
#121669=CARTESIAN_POINT('Ctrl Pts',(-10.9864237285865,9.87854143680692,
10.35649397805));
#121670=CARTESIAN_POINT('Ctrl Pts',(-10.9939073677419,9.87947384170192,
10.3680955591872));
#121671=CARTESIAN_POINT('Ctrl Pts',(-10.9980422857103,9.87999939824166,
10.3746467646654));
#121672=CARTESIAN_POINT('Ctrl Pts',(-11.0106126574739,9.88162996072876,
10.3950050379172));
#121673=CARTESIAN_POINT('Ctrl Pts',(-11.0188281461086,9.88274278676537,
10.4089450014902));
#121674=CARTESIAN_POINT('Ctrl Pts',(-11.0628089117876,9.88897389469459,
10.4872140778996));
#121675=CARTESIAN_POINT('Ctrl Pts',(-11.0927642357806,9.89429109071009,
10.5546067557565));
#121676=CARTESIAN_POINT('Ctrl Pts',(-11.1317571717245,9.90324854645872,
10.670470585973));
#121677=CARTESIAN_POINT('Ctrl Pts',(-11.1444073466782,9.90683471397212,
10.7175182015803));
#121678=CARTESIAN_POINT('Ctrl Pts',(-11.1606612122813,9.91273817709745,
10.797415594826));
#121679=CARTESIAN_POINT('Ctrl Pts',(-11.1658621579242,9.91508608094091,
10.8298801871881));
#121680=CARTESIAN_POINT('Ctrl Pts',(-11.1704936316568,9.91784418016715,
10.869286204795));
#121681=CARTESIAN_POINT('Ctrl Pts',(-11.1712298969036,9.91831478905645,
10.8760565769925));
#121682=CARTESIAN_POINT('Ctrl Pts',(-11.1722923280178,9.91904793676694,
10.8866830547739));
#121683=CARTESIAN_POINT('Ctrl Pts',(-11.1726582731051,9.9193125544387,10.8905349005046));
#121684=CARTESIAN_POINT('Ctrl Pts',(-11.1733114952172,9.91980876409739,
10.8977901076806));
#121685=CARTESIAN_POINT('Ctrl Pts',(-11.1736029502361,9.92004056618484,
10.9011929029623));
#121686=CARTESIAN_POINT('Ctrl Pts',(-11.1742459513468,9.92057743569713,
10.9091046694058));
#121687=CARTESIAN_POINT('Ctrl Pts',(-11.1745863336722,9.92088188945316,
10.9136144583462));
#121688=CARTESIAN_POINT('Ctrl Pts',(-11.1756213021207,9.92187970981186,
10.9284664014418));
#121689=CARTESIAN_POINT('Ctrl Pts',(-11.1762053611257,9.92256735084233,
10.9388161115897));
#121690=CARTESIAN_POINT('Ctrl Pts',(-11.1796683774466,9.92784359227748,
11.0189848508572));
#121691=CARTESIAN_POINT('Ctrl Pts',(-11.1764653806438,9.93215805823227,
11.0889369088581));
#121692=CARTESIAN_POINT('Ctrl Pts',(-11.1626694761059,9.93851154953261,
11.1907124679081));
#121693=CARTESIAN_POINT('Ctrl Pts',(-11.1569056978916,9.94053939612312,
11.2230262157098));
#121694=CARTESIAN_POINT('Ctrl Pts',(-11.1380310498144,9.94598213135829,
11.3081135517474));
#121695=CARTESIAN_POINT('Ctrl Pts',(-11.1226047891467,9.94942977090415,
11.3602860059021));
#121696=CARTESIAN_POINT('Ctrl Pts',(-11.0995712052823,9.95375907795563,
11.4221061557952));
#121697=CARTESIAN_POINT('Ctrl Pts',(-11.0953476050538,9.95452760333169,
11.4329480922691));
#121698=CARTESIAN_POINT('Ctrl Pts',(-11.0883934437932,9.95575522382811,
11.4500459222704));
#121699=CARTESIAN_POINT('Ctrl Pts',(-11.0857678665593,9.95621082836442,
11.4563439024372));
#121700=CARTESIAN_POINT('Ctrl Pts',(-11.0807126090511,9.95707365166353,
11.4681793268876));
#121701=CARTESIAN_POINT('Ctrl Pts',(-11.0782947100244,9.95748046379671,
11.4737215864668));
#121702=CARTESIAN_POINT('Ctrl Pts',(-11.0727299135412,9.9584038260772,11.4862137358509));
#121703=CARTESIAN_POINT('Ctrl Pts',(-11.0695579749783,9.95892121004558,
11.4931521040812));
#121704=CARTESIAN_POINT('Ctrl Pts',(-11.0597124394219,9.96050085258223,
11.5141465871658));
#121705=CARTESIAN_POINT('Ctrl Pts',(-11.0528277266683,9.96157024113716,
11.5281012263174));
#121706=CARTESIAN_POINT('Ctrl Pts',(-11.005004702315,9.96877616834009,11.6203796534567));
#121707=CARTESIAN_POINT('Ctrl Pts',(-10.9556451671787,9.97521245360292,
11.6940043920953));
#121708=CARTESIAN_POINT('Ctrl Pts',(-10.8558418246479,9.98654185796914,
11.8117820910479));
#121709=CARTESIAN_POINT('Ctrl Pts',(-10.8089862925539,9.99138505794548,
11.85848615138));
#121710=CARTESIAN_POINT('Ctrl Pts',(-10.7524728406437,9.99653527007772,
11.9060578842726));
#121711=CARTESIAN_POINT('Ctrl Pts',(-10.7464375382498,9.99707714665545,
11.9110363742705));
#121712=CARTESIAN_POINT('Ctrl Pts',(-10.73717635193,9.99789580571806,11.9185220581034));
#121713=CARTESIAN_POINT('Ctrl Pts',(-10.7339864318326,9.99817550161973,
11.9210731047092));
#121714=CARTESIAN_POINT('Ctrl Pts',(-10.7281281629122,9.99868490442716,
11.9257083253272));
#121715=CARTESIAN_POINT('Ctrl Pts',(-10.725464075222,9.998914956155,11.9277976079804));
#121716=CARTESIAN_POINT('Ctrl Pts',(-10.719408138791,9.99943431236045,11.932504878962));
#121717=CARTESIAN_POINT('Ctrl Pts',(-10.7160109838593,9.99972313437981,
11.9351158708311));
#121718=CARTESIAN_POINT('Ctrl Pts',(-10.7071365837252,10.0004713252565,
11.941859859105));
#121719=CARTESIAN_POINT('Ctrl Pts',(-10.7016372443882,10.0009287839368,
11.9459637017154));
#121720=CARTESIAN_POINT('Ctrl Pts',(-10.6561166846949,10.004667726416,11.9793177181599));
#121721=CARTESIAN_POINT('Ctrl Pts',(-10.6143159712585,10.0078016495747,
12.0060663199458));
#121722=CARTESIAN_POINT('Ctrl Pts',(-10.5618754311339,10.0115400676978,
12.0351322030602));
#121723=CARTESIAN_POINT('Ctrl Pts',(-10.5527360003429,10.0121848153562,
12.0400411511428));
#121724=CARTESIAN_POINT('Ctrl Pts',(-10.4827227561273,10.0170807842753,
12.0764629054364));
#121725=CARTESIAN_POINT('Ctrl Pts',(-10.4192701796792,10.021280905765,12.1027264754644));
#121726=CARTESIAN_POINT('Ctrl Pts',(-10.3314743089277,10.0271215432245,
12.1303859642725));
#121727=CARTESIAN_POINT('Ctrl Pts',(-10.3088482741071,10.0286282484068,
12.1367762685141));
#121728=CARTESIAN_POINT('Ctrl Pts',(-10.2692477311084,10.0312796280453,
12.1466911684563));
#121729=CARTESIAN_POINT('Ctrl Pts',(-10.2523582714307,10.0324148327803,
12.1505260663637));
#121730=CARTESIAN_POINT('Ctrl Pts',(-10.2275951058526,10.034088635895,12.1555772740474));
#121731=CARTESIAN_POINT('Ctrl Pts',(-10.2197833835956,10.0346179916649,
12.1570884268811));
#121732=CARTESIAN_POINT('Ctrl Pts',(-10.2059711900595,10.0355566080363,
12.1596154370835));
#121733=CARTESIAN_POINT('Ctrl Pts',(-10.1999769735943,10.0359648227329,
12.1606641636243));
#121734=CARTESIAN_POINT('Ctrl Pts',(-10.1874206812549,10.036821876427,12.1627608126972));
#121735=CARTESIAN_POINT('Ctrl Pts',(-10.1808573424513,10.0372709812275,
12.1637997413075));
#121736=CARTESIAN_POINT('Ctrl Pts',(-10.1635930599042,10.0384554030377,
12.1663829838843));
#121737=CARTESIAN_POINT('Ctrl Pts',(-10.1528792395733,10.039193544145,12.1678355530397));
#121738=CARTESIAN_POINT('Ctrl Pts',(-10.1057119781914,10.0424578006168,
12.1735702759618));
#121739=CARTESIAN_POINT('Ctrl Pts',(-10.0690933233369,10.0450311957578,
12.1762941077919));
#121740=CARTESIAN_POINT('Ctrl Pts',(-9.95543740293148,10.0531413809449,
12.1794229851852));
#121741=CARTESIAN_POINT('Ctrl Pts',(-9.87844784428245,10.0588232812969,
12.1739877377011));
#121742=CARTESIAN_POINT('Ctrl Pts',(-9.76919844508157,10.0669295751954,
12.1554091045433));
#121743=CARTESIAN_POINT('Ctrl Pts',(-9.73610446858114,10.0693882137826,
12.1483026625576));
#121744=CARTESIAN_POINT('Ctrl Pts',(-9.69110731905805,10.0727008095166,
12.1365916959968));
#121745=CARTESIAN_POINT('Ctrl Pts',(-9.67890584703845,10.0735958694567,
12.1332051645396));
#121746=CARTESIAN_POINT('Ctrl Pts',(-9.65784012121549,10.0751330090084,
12.1269907650452));
#121747=CARTESIAN_POINT('Ctrl Pts',(-9.64895053646607,10.0757791147434,
12.124253465524));
#121748=CARTESIAN_POINT('Ctrl Pts',(-9.635926360528,10.0767210347194,12.1200734822325));
#121749=CARTESIAN_POINT('Ctrl Pts',(-9.63176615112178,10.0770211951966,
12.1187126774297));
#121750=CARTESIAN_POINT('Ctrl Pts',(-9.62439622793677,10.0775515576935,
12.1162564086244));
#121751=CARTESIAN_POINT('Ctrl Pts',(-9.62118355133466,10.077782277421,12.1151702392938));
#121752=CARTESIAN_POINT('Ctrl Pts',(-9.6141809173022,10.0782841235858,12.1127689741043));
#121753=CARTESIAN_POINT('Ctrl Pts',(-9.61039295635534,10.0785549294332,
12.1114483825353));
#121754=CARTESIAN_POINT('Ctrl Pts',(-9.59976390686338,10.079313152015,12.1076817746339));
#121755=CARTESIAN_POINT('Ctrl Pts',(-9.59293845562154,10.0797981039373,
12.1051917253199));
#121756=CARTESIAN_POINT('Ctrl Pts',(-9.55022372314629,10.0828233882771,
12.0891592026522));
#121757=CARTESIAN_POINT('Ctrl Pts',(-9.51498703366338,10.0852764778098,
12.0739318136012));
#121758=CARTESIAN_POINT('Ctrl Pts',(-9.40341724966897,10.0930962619891,
12.0191030064842));
#121759=CARTESIAN_POINT('Ctrl Pts',(-9.33066260023107,10.098297230063,11.9728669711294));
#121760=CARTESIAN_POINT('Ctrl Pts',(-9.2328997028319,10.1062143586153,11.8945380307947));
#121761=CARTESIAN_POINT('Ctrl Pts',(-9.20346716003467,10.1087390786546,
11.8684331266418));
#121762=CARTESIAN_POINT('Ctrl Pts',(-9.16777638611086,10.1120262851994,
11.833434364177));
#121763=CARTESIAN_POINT('Ctrl Pts',(-9.16025782038972,10.1127323963158,
11.8258583670641));
#121764=CARTESIAN_POINT('Ctrl Pts',(-9.14824794525244,10.1138833698487,
11.8134231736636));
#121765=CARTESIAN_POINT('Ctrl Pts',(-9.14369268611624,10.1143254696866,
11.8086263682286));
#121766=CARTESIAN_POINT('Ctrl Pts',(-9.13501885193152,10.115178193465,11.7993371113518));
#121767=CARTESIAN_POINT('Ctrl Pts',(-9.13089425444719,10.1155885435035,
11.7948505549792));
#121768=CARTESIAN_POINT('Ctrl Pts',(-9.12151276665089,10.116533267278,11.7844854576798));
#121769=CARTESIAN_POINT('Ctrl Pts',(-9.11627977627321,10.1170686079563,
11.7785857778109));
#121770=CARTESIAN_POINT('Ctrl Pts',(-9.10240657725098,10.1185108256013,
11.7626250588449));
#121771=CARTESIAN_POINT('Ctrl Pts',(-9.09387661543735,10.1194220954155,
11.752470145627));
#121772=CARTESIAN_POINT('Ctrl Pts',(-9.02465384580525,10.1270269828836,
11.6671763377686));
#121773=CARTESIAN_POINT('Ctrl Pts',(-8.97325535110623,10.1340900363597,
11.584989409425));
#121774=CARTESIAN_POINT('Ctrl Pts',(-8.9150803558295,10.1441918107109,11.4601520121544));
#121775=CARTESIAN_POINT('Ctrl Pts',(-8.89965608253601,10.1472017765896,
11.4219409759152));
#121776=CARTESIAN_POINT('Ctrl Pts',(-8.87934460717991,10.1516673060155,
11.3628764650067));
#121777=CARTESIAN_POINT('Ctrl Pts',(-8.87297098728736,10.1531700722691,
11.3425690872504));
#121778=CARTESIAN_POINT('Ctrl Pts',(-8.86551506679084,10.1550600291455,
11.3163459626639));
#121779=CARTESIAN_POINT('Ctrl Pts',(-8.86392321440222,10.1554724463104,
11.310580702532));
#121780=CARTESIAN_POINT('Ctrl Pts',(-8.86142112596248,10.156135212824,11.3012421011723));
#121781=CARTESIAN_POINT('Ctrl Pts',(-8.86048365568388,10.1563870464388,
11.2976762635915));
#121782=CARTESIAN_POINT('Ctrl Pts',(-8.8587024910475,10.1568723600284,11.2907695495652));
#121783=CARTESIAN_POINT('Ctrl Pts',(-8.8578566939894,10.1571059496638,11.2874293022541));
#121784=CARTESIAN_POINT('Ctrl Pts',(-8.85581923698841,10.1576765687429,
11.2792319023384));
#121785=CARTESIAN_POINT('Ctrl Pts',(-8.85464381426869,10.1580126914523,
11.2743707050295));
#121786=CARTESIAN_POINT('Ctrl Pts',(-8.85134348863313,10.1589773496186,
11.2603306437367));
#121787=CARTESIAN_POINT('Ctrl Pts',(-8.84929765658777,10.1596017446629,
11.251133341962));
#121788=CARTESIAN_POINT('Ctrl Pts',(-8.83329312878412,10.1647241202077,
11.1748766409154));
#121789=CARTESIAN_POINT('Ctrl Pts',(-8.82509679049962,10.1689582632367,
11.1067320987606));
#121790=CARTESIAN_POINT('Ctrl Pts',(-8.82095568837646,10.1768457733572,
10.979303972472));
#121791=CARTESIAN_POINT('Ctrl Pts',(-8.82347091754177,10.1804870927864,
10.9202972995075));
#121792=CARTESIAN_POINT('Ctrl Pts',(-8.83294116683044,10.1856208900694,
10.8401902323332));
#121793=CARTESIAN_POINT('Ctrl Pts',(-8.83608190059323,10.1870147651435,
10.818726573289));
#121794=CARTESIAN_POINT('Ctrl Pts',(-8.84261573541903,10.1894853929018,
10.7813175109578));
#121795=CARTESIAN_POINT('Ctrl Pts',(-8.84575062497382,10.1905544019334,
10.765332777549));
#121796=CARTESIAN_POINT('Ctrl Pts',(-8.85086845922819,10.1921484547219,
10.7418293284208));
#121797=CARTESIAN_POINT('Ctrl Pts',(-8.85259605824133,10.1926654864226,
10.7342565461324));
#121798=CARTESIAN_POINT('Ctrl Pts',(-8.85580495739395,10.1935902279562,
10.7208056097592));
#121799=CARTESIAN_POINT('Ctrl Pts',(-8.8572569853549,10.193996997212,10.7149207071626));
#121800=CARTESIAN_POINT('Ctrl Pts',(-8.860419829456,10.1948592682948,10.7025146256794));
#121801=CARTESIAN_POINT('Ctrl Pts',(-8.86214133748237,10.1953150980078,
10.6959964245187));
#121802=CARTESIAN_POINT('Ctrl Pts',(-8.86688668985026,10.1965369223158,
10.6786341284507));
#121803=CARTESIAN_POINT('Ctrl Pts',(-8.87001015262367,10.1973060730905,
10.6678182325631));
#121804=CARTESIAN_POINT('Ctrl Pts',(-8.88546464750051,10.2009557548812,
10.6170448916394));
#121805=CARTESIAN_POINT('Ctrl Pts',(-8.89976164395921,10.203898639096,10.5777222481572));
#121806=CARTESIAN_POINT('Ctrl Pts',(-8.95903547831701,10.214760540718,10.4382856343051));
#121807=CARTESIAN_POINT('Ctrl Pts',(-9.01584269607229,10.2230047644088,
10.3438282343092));
#121808=CARTESIAN_POINT('Ctrl Pts',(-9.09435318104939,10.2318362655084,
10.2469231591729));
#121809=CARTESIAN_POINT('Ctrl Pts',(-9.10403626307838,10.2328895148301,
10.2354282746097));
#121810=CARTESIAN_POINT('Ctrl Pts',(-9.11741813464309,10.2342940610156,
10.2201460185641));
#121811=CARTESIAN_POINT('Ctrl Pts',(-9.12092581791159,10.2346576582772,
10.2161941780932));
#121812=CARTESIAN_POINT('Ctrl Pts',(-9.12682498134826,10.2352613926566,
10.2096374557708));
#121813=CARTESIAN_POINT('Ctrl Pts',(-9.1292017762616,10.2355025739433,10.2070195342156));
#121814=CARTESIAN_POINT('Ctrl Pts',(-9.1337391810844,10.235959028747,10.2020668105704));
#121815=CARTESIAN_POINT('Ctrl Pts',(-9.13589751156172,10.2361744724633,
10.1997300010209));
#121816=CARTESIAN_POINT('Ctrl Pts',(-9.14106649854063,10.2366865323853,
10.194178867366));
#121817=CARTESIAN_POINT('Ctrl Pts',(-9.14408579511978,10.2369825093353,
10.190972600499));
#121818=CARTESIAN_POINT('Ctrl Pts',(-9.15332467460925,10.237879010605,10.181271215327));
#121819=CARTESIAN_POINT('Ctrl Pts',(-9.15960089012562,10.2384755316472,
10.1748301524246));
#121820=CARTESIAN_POINT('Ctrl Pts',(-9.22051271687433,10.2441539608153,
10.1137343983395));
#121821=CARTESIAN_POINT('Ctrl Pts',(-9.28033704181194,10.2488953106951,
10.0645023815691));
#121822=CARTESIAN_POINT('Ctrl Pts',(-9.40126392457704,10.2579010206164,
9.98350217287021));
#121823=CARTESIAN_POINT('Ctrl Pts',(-9.46115375799348,10.2621402473397,
9.95052581331259));
#121824=CARTESIAN_POINT('Ctrl Pts',(-9.5411564253882,10.2678047917668,9.91513690097317));
#121825=CARTESIAN_POINT('Ctrl Pts',(-9.55894219038821,10.2690634563514,
9.90778513538494));
#121826=CARTESIAN_POINT('Ctrl Pts',(-9.58463674049259,10.2708850305245,
9.89789421352575));
#121827=CARTESIAN_POINT('Ctrl Pts',(-9.59240525612902,10.2714361700404,
9.89499759237496));
#121828=CARTESIAN_POINT('Ctrl Pts',(-9.60597488514384,10.2723998853838,
9.89010049203051));
#121829=CARTESIAN_POINT('Ctrl Pts',(-9.61176231837995,10.2728112264164,
9.88806285740814));
#121830=CARTESIAN_POINT('Ctrl Pts',(-9.62372006744907,10.2736619035269,
9.8839575183728));
#121831=CARTESIAN_POINT('Ctrl Pts',(-9.62989211583079,10.2741014102278,
9.88189555068189));
#121832=CARTESIAN_POINT('Ctrl Pts',(-9.64575649916026,10.275232351951,9.87674130084371));
#121833=CARTESIAN_POINT('Ctrl Pts',(-9.6554722211877,10.2759261608883,9.87372331929939));
#121834=CARTESIAN_POINT('Ctrl Pts',(-9.69472931081829,10.2787350804978,
9.8620844257641));
#121835=CARTESIAN_POINT('Ctrl Pts',(-9.7245619785955,10.2808826337338,9.85449764532584));
#121836=CARTESIAN_POINT('Ctrl Pts',(-9.77340835366934,10.2844217488063,
9.84409389574778));
#121837=CARTESIAN_POINT('Ctrl Pts',(-9.79224544531752,10.2857918682406,
9.84056052594576));
#121838=CARTESIAN_POINT('Ctrl Pts',(-9.81114930150156,10.287171250943,9.83748958018577));
#121839=CARTESIAN_POINT('Origin',(-10.,2.67563288526385,11.));
#121840=CARTESIAN_POINT('',(-9.81114929229234,10.8872795026091,9.83748958168182));
#121841=CARTESIAN_POINT('',(-9.81114930150156,10.7889089429636,9.83748958018577));
#121842=CARTESIAN_POINT('',(-9.81114930150157,2.67563288526385,9.83748958018577));
#121843=CARTESIAN_POINT('',(-11.1777495366547,10.524431373431,11.0010447055591));
#121844=CARTESIAN_POINT('Ctrl Pts',(-9.81114928308311,10.8872795026091,
9.83748958317786));
#121845=CARTESIAN_POINT('Ctrl Pts',(-9.80153143050108,10.886581170619,9.83905201077338));
#121846=CARTESIAN_POINT('Ctrl Pts',(-9.79193198703791,10.8858799908288,
9.84073395523692));
#121847=CARTESIAN_POINT('Ctrl Pts',(-9.73454387667587,10.8816639673094,
9.85152507374089));
#121848=CARTESIAN_POINT('Ctrl Pts',(-9.68733980702918,10.878092617641,9.86346810946966));
#121849=CARTESIAN_POINT('Ctrl Pts',(-9.61862962080496,10.8727994259501,
9.88545794616421));
#121850=CARTESIAN_POINT('Ctrl Pts',(-9.59646596281431,10.871077343618,9.89328970252864));
#121851=CARTESIAN_POINT('Ctrl Pts',(-9.53814242378295,10.8665256973153,
9.91588415171789));
#121852=CARTESIAN_POINT('Ctrl Pts',(-9.50245360370961,10.8637190923385,
9.93179223450883));
#121853=CARTESIAN_POINT('Ctrl Pts',(-9.46111108032463,10.8604917661137,
9.95274310511545));
#121854=CARTESIAN_POINT('Ctrl Pts',(-9.45463498253787,10.8599869658328,
9.95610092631087));
#121855=CARTESIAN_POINT('Ctrl Pts',(-9.44464001173203,10.8592095066125,
9.96140166779736));
#121856=CARTESIAN_POINT('Ctrl Pts',(-9.44109931656387,10.8589344143202,
9.96330272524422));
#121857=CARTESIAN_POINT('Ctrl Pts',(-9.43458838920588,10.8584292400594,
9.9668416014475));
#121858=CARTESIAN_POINT('Ctrl Pts',(-9.43161548894146,10.8581988539951,
9.96847413303503));
#121859=CARTESIAN_POINT('Ctrl Pts',(-9.42482808376164,10.8576734589406,
9.9722396059433));
#121860=CARTESIAN_POINT('Ctrl Pts',(-9.4210183597356,10.8573789812727,9.97438095640616));
#121861=CARTESIAN_POINT('Ctrl Pts',(-9.40917292602147,10.8564644137249,
9.98112601609021));
#121862=CARTESIAN_POINT('Ctrl Pts',(-9.40117930666043,10.8558487418699,
9.98580346246934));
#121863=CARTESIAN_POINT('Ctrl Pts',(-9.3824511212313,10.8544078290771,9.99706084809407));
#121864=CARTESIAN_POINT('Ctrl Pts',(-9.37176507247056,10.8535868763449,
10.0037196863953));
#121865=CARTESIAN_POINT('Ctrl Pts',(-9.33302344769064,10.8506071935734,
10.0287321780463));
#121866=CARTESIAN_POINT('Ctrl Pts',(-9.30564659797557,10.8484947695667,
10.0481110469272));
#121867=CARTESIAN_POINT('Ctrl Pts',(-9.21909402639469,10.841666990973,10.1151017832191));
#121868=CARTESIAN_POINT('Ctrl Pts',(-9.16369123535825,10.8370428942522,
10.1672655872992));
#121869=CARTESIAN_POINT('Ctrl Pts',(-9.0887470444682,10.8298456373801,10.2529068388566));
#121870=CARTESIAN_POINT('Ctrl Pts',(-9.0651919648464,10.8274125294662,10.2825993906165));
#121871=CARTESIAN_POINT('Ctrl Pts',(-9.03670650156127,10.824201660183,10.3222970124379));
#121872=CARTESIAN_POINT('Ctrl Pts',(-9.03042836863093,10.8234754028843,
10.3313098312222));
#121873=CARTESIAN_POINT('Ctrl Pts',(-9.02053430677979,10.8222996200945,
10.3459459594557));
#121874=CARTESIAN_POINT('Ctrl Pts',(-9.01683850421292,10.8218530839732,
10.3515146861777));
#121875=CARTESIAN_POINT('Ctrl Pts',(-9.00987316797461,10.8209971622053,
10.3622062644311));
#121876=CARTESIAN_POINT('Ctrl Pts',(-9.00659548694875,10.8205880945474,
10.3673235710855));
#121877=CARTESIAN_POINT('Ctrl Pts',(-8.99915710356788,10.8196449885876,
10.3791371260857));
#121878=CARTESIAN_POINT('Ctrl Pts',(-8.99502377827826,10.8191099766161,
10.3858501810727));
#121879=CARTESIAN_POINT('Ctrl Pts',(-8.98223805815542,10.8174196990585,
10.4070905700987));
#121880=CARTESIAN_POINT('Ctrl Pts',(-8.97383126500324,10.816255764924,10.421762472407));
#121881=CARTESIAN_POINT('Ctrl Pts',(-8.95484813297215,10.8134982057211,
10.4566111793496));
#121882=CARTESIAN_POINT('Ctrl Pts',(-8.94453585665193,10.8118962088725,
10.4769233705708));
#121883=CARTESIAN_POINT('Ctrl Pts',(-8.88578020292007,10.8021048689982,
10.6014765030514));
#121884=CARTESIAN_POINT('Ctrl Pts',(-8.8522305608705,10.7934649515813,10.712031056074));
#121885=CARTESIAN_POINT('Ctrl Pts',(-8.83252593215987,10.7839836806918,
10.8436953957469));
#121886=CARTESIAN_POINT('Ctrl Pts',(-8.83024808484026,10.7827010860466,
10.8617705748012));
#121887=CARTESIAN_POINT('Ctrl Pts',(-8.82779138592134,10.7810317029888,
10.8857348701571));
#121888=CARTESIAN_POINT('Ctrl Pts',(-8.82723614640671,10.7806268377514,
10.8915818183274));
#121889=CARTESIAN_POINT('Ctrl Pts',(-8.82640557873414,10.7799731757505,
10.9010827583738));
#121890=CARTESIAN_POINT('Ctrl Pts',(-8.82610353136468,10.7797229665814,
10.9047342234988));
#121891=CARTESIAN_POINT('Ctrl Pts',(-8.82554615933276,10.7792355110843,
10.9118779327996));
#121892=CARTESIAN_POINT('Ctrl Pts',(-8.82528936169787,10.7789981933083,
10.9153699859307));
#121893=CARTESIAN_POINT('Ctrl Pts',(-8.82469614236506,10.7784166522687,
10.9239604639775));
#121894=CARTESIAN_POINT('Ctrl Pts',(-8.82437731249267,10.7780733833853,
10.9290601112762));
#121895=CARTESIAN_POINT('Ctrl Pts',(-8.82332299153975,10.7768125269855,
10.9478908897555));
#121896=CARTESIAN_POINT('Ctrl Pts',(-8.82279476504904,10.7759054961799,
10.9616331329053));
#121897=CARTESIAN_POINT('Ctrl Pts',(-8.82205953126637,10.7736106941078,
10.9968000460305));
#121898=CARTESIAN_POINT('Ctrl Pts',(-8.82219617177542,10.7722373946901,
11.0182274442435));
#121899=CARTESIAN_POINT('Ctrl Pts',(-8.82481080651115,10.7673141750267,
11.0958664378761));
#121900=CARTESIAN_POINT('Ctrl Pts',(-8.83073061865043,10.7638592873141,
11.1518875045451));
#121901=CARTESIAN_POINT('Ctrl Pts',(-8.85355814146852,10.7558262112603,
11.2795715011196));
#121902=CARTESIAN_POINT('Ctrl Pts',(-8.87321595123649,10.7512377776358,
11.350492253662));
#121903=CARTESIAN_POINT('Ctrl Pts',(-8.90367827560027,10.7456281366656,
11.4304902706779));
#121904=CARTESIAN_POINT('Ctrl Pts',(-8.90818539614777,10.7448251341771,
11.4417963890945));
#121905=CARTESIAN_POINT('Ctrl Pts',(-8.91556357633511,10.7435504554451,
11.4595017496197));
#121906=CARTESIAN_POINT('Ctrl Pts',(-8.91831804225275,10.7430826638112,
11.4659488744341));
#121907=CARTESIAN_POINT('Ctrl Pts',(-8.92354805095531,10.7422089697321,
11.4778939374242));
#121908=CARTESIAN_POINT('Ctrl Pts',(-8.92600858208183,10.741803584186,11.4833982270904));
#121909=CARTESIAN_POINT('Ctrl Pts',(-8.93157117864938,10.7408993464107,
11.4955898069945));
#121910=CARTESIAN_POINT('Ctrl Pts',(-8.93469396357023,10.7403998030501,
11.5022673068844));
#121911=CARTESIAN_POINT('Ctrl Pts',(-8.9440353234591,10.738928477035,11.5217630074455));
#121912=CARTESIAN_POINT('Ctrl Pts',(-8.95042385449657,10.7379509281313,
11.5344978185298));
#121913=CARTESIAN_POINT('Ctrl Pts',(-8.96551232342165,10.7357042241271,
11.5632608740115));
#121914=CARTESIAN_POINT('Ctrl Pts',(-8.97435651781146,10.7344303451847,
11.5792089005859));
#121915=CARTESIAN_POINT('Ctrl Pts',(-9.00584089217265,10.7300356105158,
11.6329983879148));
#121916=CARTESIAN_POINT('Ctrl Pts',(-9.03023208735937,10.7268595116441,
11.6697677160261));
#121917=CARTESIAN_POINT('Ctrl Pts',(-9.09455620556723,10.7190268830814,
11.7558313891755));
#121918=CARTESIAN_POINT('Ctrl Pts',(-9.13652072817729,10.7143390375931,
11.8034382888994));
#121919=CARTESIAN_POINT('Ctrl Pts',(-9.20519247688796,10.7074309187343,
11.8697155240066));
#121920=CARTESIAN_POINT('Ctrl Pts',(-9.22917710046181,10.7051392245171,
11.8910423954008));
#121921=CARTESIAN_POINT('Ctrl Pts',(-9.2593858576292,10.7024236515511,11.9157696817498));
#121922=CARTESIAN_POINT('Ctrl Pts',(-9.26480590931729,10.701942808905,11.9201266612523));
#121923=CARTESIAN_POINT('Ctrl Pts',(-9.27335865475094,10.7011943951677,
11.9268780709642));
#121924=CARTESIAN_POINT('Ctrl Pts',(-9.27646521624351,10.7009246606986,
11.9293051279843));
#121925=CARTESIAN_POINT('Ctrl Pts',(-9.28200511121423,10.7004474618356,
11.9335886507282));
#121926=CARTESIAN_POINT('Ctrl Pts',(-9.28443350408976,10.700239580793,11.9354512383713));
#121927=CARTESIAN_POINT('Ctrl Pts',(-9.2902826891068,10.6997419384228,11.939901482977));
#121928=CARTESIAN_POINT('Ctrl Pts',(-9.29371038808442,10.699452810147,11.9424799438871));
#121929=CARTESIAN_POINT('Ctrl Pts',(-9.30424461500359,10.6985715909525,
11.9503144918047));
#121930=CARTESIAN_POINT('Ctrl Pts',(-9.31139648250242,10.697983469806,11.9555094956221));
#121931=CARTESIAN_POINT('Ctrl Pts',(-9.32827007757079,10.6966177181266,
11.9674783442409));
#121932=CARTESIAN_POINT('Ctrl Pts',(-9.33803702378796,10.6958437918539,
11.9741870850089));
#121933=CARTESIAN_POINT('Ctrl Pts',(-9.37328879626928,10.6931028093784,
11.9976258807716));
#121934=CARTESIAN_POINT('Ctrl Pts',(-9.39932121479374,10.6911745127712,
12.0135134864214));
#121935=CARTESIAN_POINT('Ctrl Pts',(-9.49019137339902,10.6846625222036,
12.0642388996812));
#121936=CARTESIAN_POINT('Ctrl Pts',(-9.55765934409957,10.6801831461707,
12.094003785954));
#121937=CARTESIAN_POINT('Ctrl Pts',(-9.63835134843804,10.6748324453237,
12.1209090144417));
#121938=CARTESIAN_POINT('Ctrl Pts',(-9.64929058076807,10.6741074783455,
12.1243796775402));
#121939=CARTESIAN_POINT('Ctrl Pts',(-9.69287426794037,10.671217023402,12.1375094506139));
#121940=CARTESIAN_POINT('Ctrl Pts',(-9.72587768746345,10.6690230704251,
12.145910376039));
#121941=CARTESIAN_POINT('Ctrl Pts',(-9.76951185348409,10.6660908351589,
12.1550243840701));
#121942=CARTESIAN_POINT('Ctrl Pts',(-9.77985547593401,10.6653935086531,
12.1570404012885));
#121943=CARTESIAN_POINT('Ctrl Pts',(-9.79670622308358,10.6642532300046,
12.1600905534317));
#121944=CARTESIAN_POINT('Ctrl Pts',(-9.80319757083106,10.6638129428923,
12.1612093923107));
#121945=CARTESIAN_POINT('Ctrl Pts',(-9.81572377817318,10.6629612055448,
12.1632603413709));
#121946=CARTESIAN_POINT('Ctrl Pts',(-9.82175718592707,10.6625500090232,
12.1642000878541));
#121947=CARTESIAN_POINT('Ctrl Pts',(-9.83580384266115,10.6615903544599,
12.1662762047317));
#121948=CARTESIAN_POINT('Ctrl Pts',(-9.84382195966752,10.661040805725,12.167376964766));
#121949=CARTESIAN_POINT('Ctrl Pts',(-9.86978787312542,10.6592551208576,
12.1706693737516));
#121950=CARTESIAN_POINT('Ctrl Pts',(-9.88777421279505,10.6580088634585,
12.1725302941356));
#121951=CARTESIAN_POINT('Ctrl Pts',(-9.98358219291365,10.6513173183515,
12.1802183103532));
#121952=CARTESIAN_POINT('Ctrl Pts',(-10.0617841774874,10.6456509560254,
12.1787127307168));
#121953=CARTESIAN_POINT('Ctrl Pts',(-10.2072553001873,10.634903055233,12.1613917014821));
#121954=CARTESIAN_POINT('Ctrl Pts',(-10.2744314189326,10.6298598732395,
12.1473772335697));
#121955=CARTESIAN_POINT('Ctrl Pts',(-10.3490350731491,10.6243918157777,
12.1248814923333));
#121956=CARTESIAN_POINT('Ctrl Pts',(-10.3580241556568,10.62373537929,12.1220528381882));
#121957=CARTESIAN_POINT('Ctrl Pts',(-10.3717318398115,10.6227390654846,
12.1175578391822));
#121958=CARTESIAN_POINT('Ctrl Pts',(-10.3764751520759,10.6223951773419,
12.1159688825327));
#121959=CARTESIAN_POINT('Ctrl Pts',(-10.3844692567733,10.6218172470295,
12.1132341763298));
#121960=CARTESIAN_POINT('Ctrl Pts',(-10.3877253718202,10.6215823102871,
12.1121043017626));
#121961=CARTESIAN_POINT('Ctrl Pts',(-10.3944555622792,10.6210977307217,
12.1097357677851));
#121962=CARTESIAN_POINT('Ctrl Pts',(-10.3979288436736,10.6208482082355,
12.108495061437));
#121963=CARTESIAN_POINT('Ctrl Pts',(-10.4070213558203,10.6201963169081,
12.1051988409286));
#121964=CARTESIAN_POINT('Ctrl Pts',(-10.4126309382986,10.6197954624359,
12.1031167547413));
#121965=CARTESIAN_POINT('Ctrl Pts',(-10.4378768845288,10.6179963720566,
12.0935267894348));
#121966=CARTESIAN_POINT('Ctrl Pts',(-10.4573272872385,10.6166238660957,
12.0855362214911));
#121967=CARTESIAN_POINT('Ctrl Pts',(-10.5135890942475,10.6126647079295,
12.060641962421));
#121968=CARTESIAN_POINT('Ctrl Pts',(-10.549756490421,10.6101330615061,12.0423547473091));
#121969=CARTESIAN_POINT('Ctrl Pts',(-10.6694055598791,10.6015767872125,
11.973893085681));
#121970=CARTESIAN_POINT('Ctrl Pts',(-10.7475699967837,10.5956360590842,
11.9152642954634));
#121971=CARTESIAN_POINT('Ctrl Pts',(-10.8281670359103,10.588332451929,11.8375253964328));
#121972=CARTESIAN_POINT('Ctrl Pts',(-10.8385142832949,10.587369857886,11.8271657603227));
#121973=CARTESIAN_POINT('Ctrl Pts',(-10.8538982195933,10.5858984230248,
11.8111780631434));
#121974=CARTESIAN_POINT('Ctrl Pts',(-10.8590785766533,10.5853957396488,
11.8056897754421));
#121975=CARTESIAN_POINT('Ctrl Pts',(-10.8683098558573,10.5844866465242,
11.7957195166096));
#121976=CARTESIAN_POINT('Ctrl Pts',(-10.872379750164,10.5840810546809,11.7912554101402));
#121977=CARTESIAN_POINT('Ctrl Pts',(-10.8810112988154,10.583210408159,11.7816402585063));
#121978=CARTESIAN_POINT('Ctrl Pts',(-10.885562498689,10.5827449418544,11.7764801734794));
#121979=CARTESIAN_POINT('Ctrl Pts',(-10.8970210576773,10.5815564274281,
11.7632568429367));
#121980=CARTESIAN_POINT('Ctrl Pts',(-10.9038649516957,10.5808308452378,
11.7551396708653));
#121981=CARTESIAN_POINT('Ctrl Pts',(-10.9399341336241,10.5769202644692,
11.7111670539386));
#121982=CARTESIAN_POINT('Ctrl Pts',(-10.9671340813768,10.5736570979384,
11.6737102112708));
#121983=CARTESIAN_POINT('Ctrl Pts',(-11.0230820954715,10.5661896681983,
11.5862690988688));
#121984=CARTESIAN_POINT('Ctrl Pts',(-11.0505072397248,10.5619584967098,
11.5355764471843));
#121985=CARTESIAN_POINT('Ctrl Pts',(-11.096154081084,10.5537977302198,11.4340833091441));
#121986=CARTESIAN_POINT('Ctrl Pts',(-11.1148163967447,10.5498772141991,
11.3836243613011));
#121987=CARTESIAN_POINT('Ctrl Pts',(-11.1329455086723,10.5453638767865,
11.3219332329409));
#121988=CARTESIAN_POINT('Ctrl Pts',(-11.1357860654532,10.5446288134673,
11.3117636362784));
#121989=CARTESIAN_POINT('Ctrl Pts',(-11.139552127202,10.5436147947911,11.2975453453061));
#121990=CARTESIAN_POINT('Ctrl Pts',(-11.1405934667704,10.5433298157008,
11.2935282405269));
#121991=CARTESIAN_POINT('Ctrl Pts',(-11.1424570178325,10.5428113598447,
11.2861796611299));
#121992=CARTESIAN_POINT('Ctrl Pts',(-11.1432859438448,10.5425775131625,
11.2828499387873));
#121993=CARTESIAN_POINT('Ctrl Pts',(-11.1449827410332,10.542092036483,11.2759047103736));
#121994=CARTESIAN_POINT('Ctrl Pts',(-11.1458480588564,10.5418405493249,
11.2722886583205));
#121995=CARTESIAN_POINT('Ctrl Pts',(-11.147581113616,10.5413286144644,11.2648918576034));
#121996=CARTESIAN_POINT('Ctrl Pts',(-11.1484473265979,10.5410682527546,
11.2611107956759));
#121997=CARTESIAN_POINT('Ctrl Pts',(-11.1505613326278,10.5404212435453,
11.2516689927708));
#121998=CARTESIAN_POINT('Ctrl Pts',(-11.1517860611162,10.5400357985367,
11.2460031192622));
#121999=CARTESIAN_POINT('Ctrl Pts',(-11.1551432723351,10.5389474879925,
11.2298969834078));
#122000=CARTESIAN_POINT('Ctrl Pts',(-11.1571760272035,10.5382494113297,
11.2194362368922));
#122001=CARTESIAN_POINT('Ctrl Pts',(-11.1714346956862,10.5330273145064,
11.140341574944));
#122002=CARTESIAN_POINT('Ctrl Pts',(-11.1776876846325,10.5287459337407,
11.0707736257504));
#122003=CARTESIAN_POINT('Ctrl Pts',(-11.1777495366547,10.5244313734309,
11.001044705558));
#122004=CARTESIAN_POINT('Ctrl Pts',(-11.1777495366547,10.524431373431,11.0010447055599));
#122005=CARTESIAN_POINT('Ctrl Pts',(-11.1778014625253,10.5208092234631,
10.9425060392978));
#122006=CARTESIAN_POINT('Ctrl Pts',(-11.1734900406971,10.5171760859007,
10.8840597268698));
#122007=CARTESIAN_POINT('Ctrl Pts',(-11.1614407031938,10.5119409805812,
10.8033164228629));
#122008=CARTESIAN_POINT('Ctrl Pts',(-11.1573588302156,10.5104425498072,
10.7805703663003));
#122009=CARTESIAN_POINT('Ctrl Pts',(-11.150974721311,10.5084003519483,10.7501687844275));
#122010=CARTESIAN_POINT('Ctrl Pts',(-11.149259657729,10.5078746211142,10.7423943334408));
#122011=CARTESIAN_POINT('Ctrl Pts',(-11.1457910342312,10.5068532469504,
10.7273954729512));
#122012=CARTESIAN_POINT('Ctrl Pts',(-11.1440476297423,10.5063579412863,
10.7201690886765));
#122013=CARTESIAN_POINT('Ctrl Pts',(-11.1407656902538,10.5054567320525,
10.7071090723435));
#122014=CARTESIAN_POINT('Ctrl Pts',(-11.1392505067385,10.505051583652,10.7012697937131));
#122015=CARTESIAN_POINT('Ctrl Pts',(-11.1358902237492,10.5041757601692,
10.6887172797469));
#122016=CARTESIAN_POINT('Ctrl Pts',(-11.1340303318796,10.5037046253151,
10.6820082782195));
#122017=CARTESIAN_POINT('Ctrl Pts',(-11.1288157203648,10.5024193294463,
10.6638259078731));
#122018=CARTESIAN_POINT('Ctrl Pts',(-11.1253457076169,10.5016015038199,
10.652386751018));
#122019=CARTESIAN_POINT('Ctrl Pts',(-11.1043786990478,10.4968630574732,
10.586874434735));
#122020=CARTESIAN_POINT('Ctrl Pts',(-11.0831625836609,10.4928229155626,
10.5340792737668));
#122021=CARTESIAN_POINT('Ctrl Pts',(-11.0278595206646,10.4836838374943,
10.4208759623487));
#122022=CARTESIAN_POINT('Ctrl Pts',(-10.9920816027849,10.4785602159411,
10.3615225610974));
#122023=CARTESIAN_POINT('Ctrl Pts',(-10.9309621471302,10.471036847189,10.2777846963343));
#122024=CARTESIAN_POINT('Ctrl Pts',(-10.9094043283811,10.4685644605243,
10.2508206447563));
#122025=CARTESIAN_POINT('Ctrl Pts',(-10.8818106844505,10.4656432975802,
10.2192567823819));
#122026=CARTESIAN_POINT('Ctrl Pts',(-10.8768771136236,10.4651298141408,
10.2137197766276));
#122027=CARTESIAN_POINT('Ctrl Pts',(-10.8691372000435,10.4643382643406,
10.2051966442339));
#122028=CARTESIAN_POINT('Ctrl Pts',(-10.8663671232169,10.4640576992096,
10.2021780550008));
#122029=CARTESIAN_POINT('Ctrl Pts',(-10.8612788985222,10.4635473943146,
10.1966911011804));
#122030=CARTESIAN_POINT('Ctrl Pts',(-10.8589658351801,10.463317302713,10.194218253757));
#122031=CARTESIAN_POINT('Ctrl Pts',(-10.8537098982712,10.4627986961576,
10.1886475935271));
#122032=CARTESIAN_POINT('Ctrl Pts',(-10.8507608068258,10.4625106563633,
10.1855557914169));
#122033=CARTESIAN_POINT('Ctrl Pts',(-10.8430610771185,10.4617660111174,
10.177570920186));
#122034=CARTESIAN_POINT('Ctrl Pts',(-10.8382845706704,10.4613112854978,
10.172702861725));
#122035=CARTESIAN_POINT('Ctrl Pts',(-10.8003082299016,10.457749557439,10.1346652593722));
#122036=CARTESIAN_POINT('Ctrl Pts',(-10.7651908179347,10.4547746531926,
10.103461333031));
#122037=CARTESIAN_POINT('Ctrl Pts',(-10.6664374598311,10.4469257599335,
10.0257552737279));
#122038=CARTESIAN_POINT('Ctrl Pts',(-10.5998516165015,10.4421380705178,
9.98340285229885));
#122039=CARTESIAN_POINT('Ctrl Pts',(-10.4971142958291,10.4348584924731,
9.93168818361229));
#122040=CARTESIAN_POINT('Ctrl Pts',(-10.4639558608616,10.43252635496,9.91687612547961));
#122041=CARTESIAN_POINT('Ctrl Pts',(-10.4196031719364,10.4293978659463,
9.89947419113913));
#122042=CARTESIAN_POINT('Ctrl Pts',(-10.4089785677588,10.4286478604088,
9.89548182706895));
#122043=CARTESIAN_POINT('Ctrl Pts',(-10.3919338614074,10.4274429094518,
9.88935665192368));
#122044=CARTESIAN_POINT('Ctrl Pts',(-10.3855500367186,10.4269912307043,
9.88712446144455));
#122045=CARTESIAN_POINT('Ctrl Pts',(-10.3734107658169,10.4261314367687,
9.88299678738927));
#122046=CARTESIAN_POINT('Ctrl Pts',(-10.3676592054947,10.4257236899488,
9.88109049370623));
#122047=CARTESIAN_POINT('Ctrl Pts',(-10.3545321260789,10.4247920822244,
9.87685180393833));
#122048=CARTESIAN_POINT('Ctrl Pts',(-10.3471478878776,10.4242673295688,
9.8745475408788));
#122049=CARTESIAN_POINT('Ctrl Pts',(-10.3243150668196,10.4226422787787,
9.86766860884956));
#122050=CARTESIAN_POINT('Ctrl Pts',(-10.3087954522306,10.4215342388315,
9.86333823581042));
#122051=CARTESIAN_POINT('Ctrl Pts',(-10.2171369372544,10.4149666843821,
9.83977880192476));
#122052=CARTESIAN_POINT('Ctrl Pts',(-10.1393298372915,10.4092775572933,
9.82788871955721));
#122053=CARTESIAN_POINT('Ctrl Pts',(-10.0079361810192,10.3996280394529,
9.82108174312774));
#122054=CARTESIAN_POINT('Ctrl Pts',(-9.95481241391698,10.3957208987762,
9.82192113401668));
#122055=CARTESIAN_POINT('Ctrl Pts',(-9.88545199811531,10.3907234091425,
9.82771716130987));
#122056=CARTESIAN_POINT('Ctrl Pts',(-9.86900947669093,10.3895467188059,
9.82944037382131));
#122057=CARTESIAN_POINT('Ctrl Pts',(-9.84132069371484,10.3875842958606,
9.83293300639602));
#122058=CARTESIAN_POINT('Ctrl Pts',(-9.8300542156052,10.3867911682803,9.83452029446056));
#122059=CARTESIAN_POINT('Ctrl Pts',(-9.81625646134559,10.3858278533388,
9.8366685495508));
#122060=CARTESIAN_POINT('Ctrl Pts',(-9.81370221395765,10.3856498620175,
9.83707485762302));
#122061=CARTESIAN_POINT('Ctrl Pts',(-9.81114930150037,10.385472315614,9.83748958018597));
#122062=CARTESIAN_POINT('Ctrl Pts',(-9.81114930150156,10.287171250943,9.83748958018577));
#122063=CARTESIAN_POINT('Ctrl Pts',(-9.8822558631217,10.292359777568,9.82593826537525));
#122064=CARTESIAN_POINT('Ctrl Pts',(-9.95430619677359,10.2976918666623,
9.82092997109078));
#122065=CARTESIAN_POINT('Ctrl Pts',(-10.0656605648505,10.3058135681201,
9.82342593242662));
#122066=CARTESIAN_POINT('Ctrl Pts',(-10.1048644736454,10.3086470262399,
9.82627009030703));
#122067=CARTESIAN_POINT('Ctrl Pts',(-10.1531977265903,10.3120561606732,
9.83221829899421));
#122068=CARTESIAN_POINT('Ctrl Pts',(-10.1625253172695,10.3127101124164,
9.8334798845329));
#122069=CARTESIAN_POINT('Ctrl Pts',(-10.1761879738484,10.3136612222668,
9.83549486825425));
#122070=CARTESIAN_POINT('Ctrl Pts',(-10.1805352679866,10.3139628446267,
9.83616091208098));
#122071=CARTESIAN_POINT('Ctrl Pts',(-10.1882297125398,10.3144947882491,
9.83738391977375));
#122072=CARTESIAN_POINT('Ctrl Pts',(-10.1915783048973,10.3147256393405,
9.83793101375094));
#122073=CARTESIAN_POINT('Ctrl Pts',(-10.1988658090097,10.3152266079621,
9.83915400550776));
#122074=CARTESIAN_POINT('Ctrl Pts',(-10.2028036771766,10.3154964142574,
9.83983548467139));
#122075=CARTESIAN_POINT('Ctrl Pts',(-10.2138236043379,10.3162491340243,
9.84180039301222));
#122076=CARTESIAN_POINT('Ctrl Pts',(-10.2208976233688,10.3167296388762,
9.84312874107009));
#122077=CARTESIAN_POINT('Ctrl Pts',(-10.2639683208791,10.3196412690377,
9.85162597113228));
#122078=CARTESIAN_POINT('Ctrl Pts',(-10.2996296432167,10.3219926312374,
9.8604102313947));
#122079=CARTESIAN_POINT('Ctrl Pts',(-10.441995630875,10.331348659916,9.90262578346285));
#122080=CARTESIAN_POINT('Ctrl Pts',(-10.5440916072857,10.3380446635281,
9.94949733627392));
#122081=CARTESIAN_POINT('Ctrl Pts',(-10.655052839223,10.3465801570331,10.0210158899088));
#122082=CARTESIAN_POINT('Ctrl Pts',(-10.6717666783701,10.3479016175868,
10.0324083703543));
#122083=CARTESIAN_POINT('Ctrl Pts',(-10.695037332062,10.3497978935837,10.0491637318292));
#122084=CARTESIAN_POINT('Ctrl Pts',(-10.7018429804912,10.3503595359576,
10.0541760595204));
#122085=CARTESIAN_POINT('Ctrl Pts',(-10.7135165484209,10.3513355529462,
10.0629689557677));
#122086=CARTESIAN_POINT('Ctrl Pts',(-10.7184098905328,10.351748600042,10.0667153331077));
#122087=CARTESIAN_POINT('Ctrl Pts',(-10.7277602072342,10.3525455621152,
10.0739911111412));
#122088=CARTESIAN_POINT('Ctrl Pts',(-10.7322214817457,10.3529292429321,
10.0775147257552));
#122089=CARTESIAN_POINT('Ctrl Pts',(-10.7427099497199,10.3538395357452,
10.0859227733466));
#122090=CARTESIAN_POINT('Ctrl Pts',(-10.7487146751093,10.3543672275123,
10.0908346817073));
#122091=CARTESIAN_POINT('Ctrl Pts',(-10.7698230334699,10.3562459062084,
10.1084524073393));
#122092=CARTESIAN_POINT('Ctrl Pts',(-10.7846546037202,10.3576096319008,
10.1214775560349));
#122093=CARTESIAN_POINT('Ctrl Pts',(-10.8839942794638,10.3670548098794,
10.2132409732851));
#122094=CARTESIAN_POINT('Ctrl Pts',(-10.956837739388,10.3756609084894,10.3036616795177));
#122095=CARTESIAN_POINT('Ctrl Pts',(-11.0324911879688,10.3864797851252,
10.4323714859524));
#122096=CARTESIAN_POINT('Ctrl Pts',(-11.048375278236,10.3888997911129,10.4622733747698));
#122097=CARTESIAN_POINT('Ctrl Pts',(-11.0659054601722,10.3917299785873,
10.4990132830507));
#122098=CARTESIAN_POINT('Ctrl Pts',(-11.0688061076328,10.3922041977594,
10.5052317204052));
#122099=CARTESIAN_POINT('Ctrl Pts',(-11.0732618410511,10.3929416986472,
10.515006041832));
#122100=CARTESIAN_POINT('Ctrl Pts',(-11.0748539238431,10.3932070986589,
10.5185447451649));
#122101=CARTESIAN_POINT('Ctrl Pts',(-11.0778133172067,10.3937039194524,
10.5252104022605));
#122102=CARTESIAN_POINT('Ctrl Pts',(-11.0791845221947,10.3939355575783,
10.5283354197459));
#122103=CARTESIAN_POINT('Ctrl Pts',(-11.0823335246481,10.3944709595313,
10.5355977174437));
#122104=CARTESIAN_POINT('Ctrl Pts',(-11.0841012021118,10.39477412062,10.5397392870799));
#122105=CARTESIAN_POINT('Ctrl Pts',(-11.0898158919151,10.3957632164203,
10.5533440783053));
#122106=CARTESIAN_POINT('Ctrl Pts',(-11.093663216687,10.3964435624502,10.5628490231141));
#122107=CARTESIAN_POINT('Ctrl Pts',(-11.1238760031118,10.401916838432,10.6403872692997));
#122108=CARTESIAN_POINT('Ctrl Pts',(-11.1439949601166,10.406409666529,10.7106955278433));
#122109=CARTESIAN_POINT('Ctrl Pts',(-11.167820599171,10.4143875245765,10.8374438994735));
#122110=CARTESIAN_POINT('Ctrl Pts',(-11.1742264520675,10.4178526365535,
10.8931305790753));
#122111=CARTESIAN_POINT('Ctrl Pts',(-11.1775585844599,10.422760974927,10.9700959178083));
#122112=CARTESIAN_POINT('Ctrl Pts',(-11.1779049748196,10.4241155330458,
10.9911531855618));
#122113=CARTESIAN_POINT('Ctrl Pts',(-11.1775216859798,10.4265228001002,
11.0281298659052));
#122114=CARTESIAN_POINT('Ctrl Pts',(-11.1770337598879,10.4275683225547,
11.0440465569254));
#122115=CARTESIAN_POINT('Ctrl Pts',(-11.1758314714931,10.4291339897832,
11.067636379727));
#122116=CARTESIAN_POINT('Ctrl Pts',(-11.1753642482087,10.4296465384176,
11.075320704655));
#122117=CARTESIAN_POINT('Ctrl Pts',(-11.1743951046497,10.4305663065676,
11.0890384683117));
#122118=CARTESIAN_POINT('Ctrl Pts',(-11.1739219299493,10.4309726236499,
11.0950737120102));
#122119=CARTESIAN_POINT('Ctrl Pts',(-11.1728201305206,10.4318371538744,
11.1078609593253));
#122120=CARTESIAN_POINT('Ctrl Pts',(-11.1721796795132,10.4322957193756,
11.1146116953859));
#122121=CARTESIAN_POINT('Ctrl Pts',(-11.1703022486991,10.4335327869764,
11.1327349621216));
#122122=CARTESIAN_POINT('Ctrl Pts',(-11.1689578388091,10.4343145848187,
11.1440953801079));
#122123=CARTESIAN_POINT('Ctrl Pts',(-11.1615402081611,10.4381810954351,
11.1998083865065));
#122124=CARTESIAN_POINT('Ctrl Pts',(-11.1531078234111,10.4413378830274,
11.2438042452301));
#122125=CARTESIAN_POINT('Ctrl Pts',(-11.1208717102869,10.4508392694634,
11.3720031245035));
#122126=CARTESIAN_POINT('Ctrl Pts',(-11.0901766388471,10.4573447157126,
11.4541504932501));
#122127=CARTESIAN_POINT('Ctrl Pts',(-11.0412388012425,10.4651745503363,
11.5507750310746));
#122128=CARTESIAN_POINT('Ctrl Pts',(-11.0313063147132,10.4666711852939,
11.5691561860265));
#122129=CARTESIAN_POINT('Ctrl Pts',(-11.0141567372982,10.4690999003144,
11.5989686936526));
#122130=CARTESIAN_POINT('Ctrl Pts',(-11.0072227350167,10.4700442738613,
11.6105569462091));
#122131=CARTESIAN_POINT('Ctrl Pts',(-10.997411347687,10.4713276728443,11.6263317020142));
#122132=CARTESIAN_POINT('Ctrl Pts',(-10.9947042170087,10.4716765118662,
11.6306221693421));
#122133=CARTESIAN_POINT('Ctrl Pts',(-10.9900860704306,10.472262615208,11.6378376289855));
#122134=CARTESIAN_POINT('Ctrl Pts',(-10.9881896276822,10.4725007992281,
11.6407718227033));
#122135=CARTESIAN_POINT('Ctrl Pts',(-10.9845178957631,10.4729571170824,
11.6463976881193));
#122136=CARTESIAN_POINT('Ctrl Pts',(-10.9827445797068,10.4731753820059,
11.6490905560654));
#122137=CARTESIAN_POINT('Ctrl Pts',(-10.9779217700138,10.4737633902271,
11.6563491591512));
#122138=CARTESIAN_POINT('Ctrl Pts',(-10.9748513254613,10.4741317785629,
11.6609009783329));
#122139=CARTESIAN_POINT('Ctrl Pts',(-10.9631138726958,10.4755183581334,
11.6780415299478));
#122140=CARTESIAN_POINT('Ctrl Pts',(-10.9542335140878,10.4765235096128,
11.6904832382428));
#122141=CARTESIAN_POINT('Ctrl Pts',(-10.8745257732511,10.4852058857344,
11.797680535715));
#122142=CARTESIAN_POINT('Ctrl Pts',(-10.7900328601207,10.4922062853714,
11.8814448889436));
#122143=CARTESIAN_POINT('Ctrl Pts',(-10.6759144941456,10.5011795155759,
11.9647601165845));
#122144=CARTESIAN_POINT('Ctrl Pts',(-10.6569749062222,10.5026526648774,
11.9777557773459));
#122145=CARTESIAN_POINT('Ctrl Pts',(-10.6233635567393,10.5052504532086,
11.9994010354373));
#122146=CARTESIAN_POINT('Ctrl Pts',(-10.6088614147608,10.5063661556958,
12.0083016828432));
#122147=CARTESIAN_POINT('Ctrl Pts',(-10.5873498777719,10.5080165017209,
12.0208710091174));
#122148=CARTESIAN_POINT('Ctrl Pts',(-10.5804878206124,10.508542274165,12.0247884568163));
#122149=CARTESIAN_POINT('Ctrl Pts',(-10.5682785916075,10.5094768281883,
12.0315965519764));
#122150=CARTESIAN_POINT('Ctrl Pts',(-10.5629474338271,10.5098845945755,
12.0345154363843));
#122151=CARTESIAN_POINT('Ctrl Pts',(-10.5517175285242,10.5107430270575,
12.0405514599651));
#122152=CARTESIAN_POINT('Ctrl Pts',(-10.5458144255501,10.51119397629,12.0436599933981));
#122153=CARTESIAN_POINT('Ctrl Pts',(-10.5301678785782,10.5123886520457,
12.0517303046131));
#122154=CARTESIAN_POINT('Ctrl Pts',(-10.5203813924906,10.5131352922613,
12.0566067411761));
#122155=CARTESIAN_POINT('Ctrl Pts',(-10.4768731673793,10.5164530272218,
12.0775350684553));
#122156=CARTESIAN_POINT('Ctrl Pts',(-10.442470186839,10.5190731147247,12.0921123798651));
#122157=CARTESIAN_POINT('Ctrl Pts',(-10.3350675051766,10.5272445997452,
12.1317128675599));
#122158=CARTESIAN_POINT('Ctrl Pts',(-10.2602579016275,10.5329387616071,
12.1512201603543));
#122159=CARTESIAN_POINT('Ctrl Pts',(-10.151365695603,10.5410002008411,12.1684524512969));
#122160=CARTESIAN_POINT('Ctrl Pts',(-10.1184360468283,10.5434064844935,
12.1722482226635));
#122161=CARTESIAN_POINT('Ctrl Pts',(-10.0729260691632,10.5466561430441,
12.1755564540803));
#122162=CARTESIAN_POINT('Ctrl Pts',(-10.0604497383667,10.5475391541488,
12.1762640199792));
#122163=CARTESIAN_POINT('Ctrl Pts',(-10.0387645628158,10.5490577455538,
12.1771478841248));
#122164=CARTESIAN_POINT('Ctrl Pts',(-10.0295607028759,10.5496972288833,
12.1774149694714));
#122165=CARTESIAN_POINT('Ctrl Pts',(-10.0159957339912,10.5506313826146,
12.1776494392883));
#122166=CARTESIAN_POINT('Ctrl Pts',(-10.0116366852185,10.5509303007438,
12.1777005792833));
#122167=CARTESIAN_POINT('Ctrl Pts',(-10.0038874455616,10.5514593265673,
12.177748463072));
#122168=CARTESIAN_POINT('Ctrl Pts',(-10.0004974442092,10.5516899416526,
12.1777547741499));
#122169=CARTESIAN_POINT('Ctrl Pts',(-9.99308262972192,10.5521925649602,
12.1777365625432));
#122170=CARTESIAN_POINT('Ctrl Pts',(-9.98905793755075,10.5524642444608,
12.1777060470415));
#122171=CARTESIAN_POINT('Ctrl Pts',(-9.97770945961987,10.5532272880305,
12.1775618213777));
#122172=CARTESIAN_POINT('Ctrl Pts',(-9.97038631254256,10.5537161375682,
12.1774004193765));
#122173=CARTESIAN_POINT('Ctrl Pts',(-9.92330816030469,10.5568387602093,
12.1759232884624));
#122174=CARTESIAN_POINT('Ctrl Pts',(-9.8836354588537,10.5593786414759,12.1726624518815));
#122175=CARTESIAN_POINT('Ctrl Pts',(-9.82253681388627,10.5632508353322,
12.1645082756874));
#122176=CARTESIAN_POINT('Ctrl Pts',(-9.80095791407728,10.5646106390706,
12.1610146440701));
#122177=CARTESIAN_POINT('Ctrl Pts',(-9.73363879272821,10.5688600877953,
12.1481834829735));
#122178=CARTESIAN_POINT('Ctrl Pts',(-9.6883501272944,10.571731118984,12.1367268285679));
#122179=CARTESIAN_POINT('Ctrl Pts',(-9.59294936299341,10.5779851341149,
12.1064618020151));
#122180=CARTESIAN_POINT('Ctrl Pts',(-9.54320120686809,10.5813760060638,
12.0868678553168));
#122181=CARTESIAN_POINT('Ctrl Pts',(-9.48448844479286,10.5856414004614,
12.0589982103215));
#122182=CARTESIAN_POINT('Ctrl Pts',(-9.4740930775466,10.5864069409019,12.0538744073007));
#122183=CARTESIAN_POINT('Ctrl Pts',(-9.45770904950382,10.5876308949159,
12.0454960593669));
#122184=CARTESIAN_POINT('Ctrl Pts',(-9.45166993447215,10.5880858543134,
12.0423414129229));
#122185=CARTESIAN_POINT('Ctrl Pts',(-9.44032220527155,10.5889481451443,
12.0362878028507));
#122186=CARTESIAN_POINT('Ctrl Pts',(-9.43500786965713,10.5893550760111,
12.0333999876922));
#122187=CARTESIAN_POINT('Ctrl Pts',(-9.42302716809412,10.5902796514208,
12.0267696230198));
#122188=CARTESIAN_POINT('Ctrl Pts',(-9.4163745813716,10.5907981385546,12.0230028707085));
#122189=CARTESIAN_POINT('Ctrl Pts',(-9.39622287864518,10.5923845968865,
12.0113322603697));
#122190=CARTESIAN_POINT('Ctrl Pts',(-9.38284460710379,10.5934597885788,
12.0032242687634));
#122191=CARTESIAN_POINT('Ctrl Pts',(-9.29597862485375,10.6005905617704,
11.9481834421076));
#122192=CARTESIAN_POINT('Ctrl Pts',(-9.22774829709035,10.6069368624258,
11.8934874740305));
#122193=CARTESIAN_POINT('Ctrl Pts',(-9.11877638770217,10.6182605058637,
11.7842493365551));
#122194=CARTESIAN_POINT('Ctrl Pts',(-9.0755086792396,10.6231879643457,11.7327481310584));
#122195=CARTESIAN_POINT('Ctrl Pts',(-9.03237766019328,10.6284123542835,
11.6714631679281));
#122196=CARTESIAN_POINT('Ctrl Pts',(-9.02795627252195,10.6289520339248,
11.6650464482634));
#122197=CARTESIAN_POINT('Ctrl Pts',(-9.02131839222845,10.6297680712681,
11.6552053135649));
#122198=CARTESIAN_POINT('Ctrl Pts',(-9.01905556464106,10.6300473148976,
11.6518126328265));
#122199=CARTESIAN_POINT('Ctrl Pts',(-9.01494619491756,10.6305562865526,
11.6455815430454));
#122200=CARTESIAN_POINT('Ctrl Pts',(-9.01309425486463,10.6307863554798,
11.6427469007652));
#122201=CARTESIAN_POINT('Ctrl Pts',(-9.00892242291732,10.6313062409033,
11.6363008106253));
#122202=CARTESIAN_POINT('Ctrl Pts',(-9.00661002683278,10.6315955705008,
11.6326846355474));
#122203=CARTESIAN_POINT('Ctrl Pts',(-9.00063882496331,10.6323459737338,
11.6232332935644));
#122204=CARTESIAN_POINT('Ctrl Pts',(-8.99701128075046,10.6328051185808,
11.6173784341347));
#122205=CARTESIAN_POINT('Ctrl Pts',(-8.96460145395669,10.6369405581506,
11.5640292570794));
#122206=CARTESIAN_POINT('Ctrl Pts',(-8.93915674306324,10.6404309797261,
11.5145798361444));
#122207=CARTESIAN_POINT('Ctrl Pts',(-8.89925486206284,10.6467321821857,
11.4213743181669));
#122208=CARTESIAN_POINT('Ctrl Pts',(-8.8836904635516,10.6495496716591,11.3782184703491));
#122209=CARTESIAN_POINT('Ctrl Pts',(-8.85379889377512,10.6561070903127,
11.2772294633044));
#122210=CARTESIAN_POINT('Ctrl Pts',(-8.84126401347867,10.6598651851965,
11.2190038811722));
#122211=CARTESIAN_POINT('Ctrl Pts',(-8.83156835102912,10.6645439927616,
11.1483348257683));
#122212=CARTESIAN_POINT('Ctrl Pts',(-8.83013383291588,10.6653271303463,
11.1365608776609));
#122213=CARTESIAN_POINT('Ctrl Pts',(-8.82814942484362,10.6665726972816,
11.1179343681861));
#122214=CARTESIAN_POINT('Ctrl Pts',(-8.82748126609069,10.6670314554784,
11.1110950086928));
#122215=CARTESIAN_POINT('Ctrl Pts',(-8.82633837094896,10.6678969397748,
11.0982340292899));
#122216=CARTESIAN_POINT('Ctrl Pts',(-8.82585002949443,10.6683032299063,
11.0922138192027));
#122217=CARTESIAN_POINT('Ctrl Pts',(-8.82485517237363,10.6692209458802,
11.0786560016849));
#122218=CARTESIAN_POINT('Ctrl Pts',(-8.82437483500912,10.6697331644927,
11.0711168006841));
#122219=CARTESIAN_POINT('Ctrl Pts',(-8.82317449755367,10.671247616402,11.0489120604837));
#122220=CARTESIAN_POINT('Ctrl Pts',(-8.82265620555464,10.6722559954407,
11.0342375355609));
#122221=CARTESIAN_POINT('Ctrl Pts',(-8.82082804806691,10.6798795027076,
10.9241625131865));
#122222=CARTESIAN_POINT('Ctrl Pts',(-8.83084171807125,10.6868523262554,
10.8289451005862));
#122223=CARTESIAN_POINT('Ctrl Pts',(-8.86160456831754,10.6969196260929,
10.6951988981057));
#122224=CARTESIAN_POINT('Ctrl Pts',(-8.87315872536738,10.6999815748667,
10.6549245923035));
#122225=CARTESIAN_POINT('Ctrl Pts',(-8.89385403063312,10.7045132595249,
10.5950331161816));
#122226=CARTESIAN_POINT('Ctrl Pts',(-8.90142954844151,10.7060316547431,
10.5749115550463));
#122227=CARTESIAN_POINT('Ctrl Pts',(-8.91181951610866,10.707938130686,10.5494511036793));
#122228=CARTESIAN_POINT('Ctrl Pts',(-8.91412935227894,10.7083519622754,
10.5439122740749));
#122229=CARTESIAN_POINT('Ctrl Pts',(-8.91792828598864,10.7090164424341,
10.5349951672435));
#122230=CARTESIAN_POINT('Ctrl Pts',(-8.9193910715358,10.709268588812,10.5316058994573));
#122231=CARTESIAN_POINT('Ctrl Pts',(-8.92224906389396,10.7097540569526,
10.5250685964608));
#122232=CARTESIAN_POINT('Ctrl Pts',(-8.92364216928187,10.7099874916057,
10.5219197358682));
#122233=CARTESIAN_POINT('Ctrl Pts',(-8.9270871418914,10.7105570805657,10.5142243920073));
#122234=CARTESIAN_POINT('Ctrl Pts',(-8.92915415204224,10.7108923359316,
10.5096846784443));
#122235=CARTESIAN_POINT('Ctrl Pts',(-8.93630399369179,10.7120305775245,
10.4942425870194));
#122236=CARTESIAN_POINT('Ctrl Pts',(-8.94152517004917,10.7128257778488,
10.4834045912768));
#122237=CARTESIAN_POINT('Ctrl Pts',(-8.98223900118111,10.7187773744916,
10.4021016714969));
#122238=CARTESIAN_POINT('Ctrl Pts',(-9.0245704751313,10.7236001869118,10.3352741847902));
#122239=CARTESIAN_POINT('Ctrl Pts',(-9.1132685123151,10.7324999027994,10.2221809461214));
#122240=CARTESIAN_POINT('Ctrl Pts',(-9.15740015321717,10.7365403265275,
10.1745792647244));
#122241=CARTESIAN_POINT('Ctrl Pts',(-9.21867823586108,10.7419254490531,
10.1185444088313));
#122242=CARTESIAN_POINT('Ctrl Pts',(-9.2324202294947,10.7431196426774,10.10655224203));
#122243=CARTESIAN_POINT('Ctrl Pts',(-9.2526742612774,10.7448642044167,10.0896894899659));
#122244=CARTESIAN_POINT('Ctrl Pts',(-9.25896741171793,10.7454041602719,
10.0845592962692));
#122245=CARTESIAN_POINT('Ctrl Pts',(-9.27008738376275,10.7463549107081,
10.0756840632185));
#122246=CARTESIAN_POINT('Ctrl Pts',(-9.27489129054688,10.7467645679853,
10.0719107071985));
#122247=CARTESIAN_POINT('Ctrl Pts',(-9.2842910225191,10.7475641829805,10.0646449667689));
#122248=CARTESIAN_POINT('Ctrl Pts',(-9.28888360357225,10.7479539717054,
10.0611486553634));
#122249=CARTESIAN_POINT('Ctrl Pts',(-9.30128566488355,10.7490043161214,
10.0518502273855));
#122250=CARTESIAN_POINT('Ctrl Pts',(-9.30914150517322,10.7496672585339,
10.0461109898473));
#122251=CARTESIAN_POINT('Ctrl Pts',(-9.33921292896529,10.7521966381418,
10.0247080585079));
#122252=CARTESIAN_POINT('Ctrl Pts',(-9.36189582820236,10.754087879968,10.0097188369469));
#122253=CARTESIAN_POINT('Ctrl Pts',(-9.45786738299857,10.7620274195192,
9.95096626927944));
#122254=CARTESIAN_POINT('Ctrl Pts',(-9.53527964146946,10.7683110628135,
9.91445376356915));
#122255=CARTESIAN_POINT('Ctrl Pts',(-9.66159725545541,10.7780965895773,
9.87088038894103));
#122256=CARTESIAN_POINT('Ctrl Pts',(-9.70818308542766,10.7816070953586,
9.85795300187527));
#122257=CARTESIAN_POINT('Ctrl Pts',(-9.76558789828214,10.7857245918511,
9.84576703056778));
#122258=CARTESIAN_POINT('Ctrl Pts',(-9.77576890968408,10.7864469620291,
9.84374604101449));
#122259=CARTESIAN_POINT('Ctrl Pts',(-9.79047333763238,10.7874776997161,
9.84102866319185));
#122260=CARTESIAN_POINT('Ctrl Pts',(-9.79497584213038,10.7877916203952,
9.84022369474705));
#122261=CARTESIAN_POINT('Ctrl Pts',(-9.80284477362347,10.788337169576,9.83886412595221));
#122262=CARTESIAN_POINT('Ctrl Pts',(-9.80620908263723,10.788569429329,9.83829789411524));
#122263=CARTESIAN_POINT('Ctrl Pts',(-9.81010032997558,10.7888369096174,
9.83766035075839));
#122264=CARTESIAN_POINT('Ctrl Pts',(-9.81062478641594,10.788872936198,9.83757478805884));
#122265=CARTESIAN_POINT('Ctrl Pts',(-9.81114930150155,10.7889089429636,
9.83748958018577));
#122266=CARTESIAN_POINT('Origin',(-10.,2.67563288526385,11.));
#122267=CARTESIAN_POINT('',(-9.81114930150156,11.3870771460943,9.83748958018577));
#122268=CARTESIAN_POINT('',(-9.81114930150157,11.2872494929995,9.83748958018577));
#122269=CARTESIAN_POINT('',(-9.81114930150157,2.67563288526385,9.83748958018577));
#122270=CARTESIAN_POINT('Ctrl Pts',(-9.81114930150155,11.3870771460943,
9.83748958018577));
#122271=CARTESIAN_POINT('Ctrl Pts',(-9.79272746796521,11.3859061337436,
9.84048222100143));
#122272=CARTESIAN_POINT('Ctrl Pts',(-9.7743691874173,11.3847269668944,9.84391397489799));
#122273=CARTESIAN_POINT('Ctrl Pts',(-9.72569745290075,11.3815573166116,
9.85421717594312));
#122274=CARTESIAN_POINT('Ctrl Pts',(-9.69557359308454,11.3795499570249,
9.86185041831245));
#122275=CARTESIAN_POINT('Ctrl Pts',(-9.65599864501995,11.3768330240802,
9.87356208966352));
#122276=CARTESIAN_POINT('Ctrl Pts',(-9.64624710610495,11.376157038407,9.87658637297539));
#122277=CARTESIAN_POINT('Ctrl Pts',(-9.63033811278735,11.3750429059349,
9.88174796488936));
#122278=CARTESIAN_POINT('Ctrl Pts',(-9.62415676711958,11.3746071942134,
9.88381032691575));
#122279=CARTESIAN_POINT('Ctrl Pts',(-9.6121903838679,11.373758058577,9.88791349585017));
#122280=CARTESIAN_POINT('Ctrl Pts',(-9.60640353951357,11.3733448384497,
9.88994841789864));
#122281=CARTESIAN_POINT('Ctrl Pts',(-9.59284943961911,11.3723707621606,
9.89483397725119));
#122282=CARTESIAN_POINT('Ctrl Pts',(-9.58509588766303,11.3718087134616,
9.89772141081544));
#122283=CARTESIAN_POINT('Ctrl Pts',(-9.55951523736213,11.3699379487286,
9.90755581714999));
#122284=CARTESIAN_POINT('Ctrl Pts',(-9.54182781918716,11.3686177170514,
9.91485517215457));
#122285=CARTESIAN_POINT('Ctrl Pts',(-9.46398871692444,11.3626842815403,
9.94922062592171));
#122286=CARTESIAN_POINT('Ctrl Pts',(-9.40600385123646,11.3579218238942,
9.98087705193931));
#122287=CARTESIAN_POINT('Ctrl Pts',(-9.28416219350759,11.3472324609399,
10.0613397514326));
#122288=CARTESIAN_POINT('Ctrl Pts',(-9.22201389194342,11.3412985578297,
10.1121676349345));
#122289=CARTESIAN_POINT('Ctrl Pts',(-9.1586272881331,11.3350052465293,10.1758143939991));
#122290=CARTESIAN_POINT('Ctrl Pts',(-9.15183895734867,11.3343280044603,
10.1828018511508));
#122291=CARTESIAN_POINT('Ctrl Pts',(-9.14210276620221,11.3333529041161,
10.1930756742565));
#122292=CARTESIAN_POINT('Ctrl Pts',(-9.13908565519734,11.3330501961127,
10.196295437537));
#122293=CARTESIAN_POINT('Ctrl Pts',(-9.13377420425991,11.3325164583443,
10.2020278768188));
#122294=CARTESIAN_POINT('Ctrl Pts',(-9.13147256388948,11.3322848935339,
10.2045336384126));
#122295=CARTESIAN_POINT('Ctrl Pts',(-9.12653041968114,11.3317870959178,
10.2099611009863));
#122296=CARTESIAN_POINT('Ctrl Pts',(-9.12389368625927,11.3315211371819,
10.2128860960097));
#122297=CARTESIAN_POINT('Ctrl Pts',(-9.11652737105877,11.3307768789678,
10.221140611296));
#122298=CARTESIAN_POINT('Ctrl Pts',(-9.11183131522705,11.3303009559553,
10.2265000148463));
#122299=CARTESIAN_POINT('Ctrl Pts',(-9.08129755363035,11.3271942630137,
10.2619916120838));
#122300=CARTESIAN_POINT('Ctrl Pts',(-9.05694569003653,11.3246578082542,
10.2933743205045));
#122301=CARTESIAN_POINT('Ctrl Pts',(-9.00520173043543,11.3189755801465,
10.3675107705387));
#122302=CARTESIAN_POINT('Ctrl Pts',(-8.97889512240055,11.3158605820624,
10.4109232619296));
#122303=CARTESIAN_POINT('Ctrl Pts',(-8.92291456639828,11.308350612603,10.5183910309816));
#122304=CARTESIAN_POINT('Ctrl Pts',(-8.89603948827621,11.3039385307278,
10.583671384167));
#122305=CARTESIAN_POINT('Ctrl Pts',(-8.87154388323513,11.2985224291015,
10.6626118351759));
#122306=CARTESIAN_POINT('Ctrl Pts',(-8.86810875893508,11.2977173423505,
10.6743219664268));
#122307=CARTESIAN_POINT('Ctrl Pts',(-8.86298571508327,11.2964400837106,
10.6928472172144));
#122308=CARTESIAN_POINT('Ctrl Pts',(-8.86117564954436,11.2959718230462,
10.6996278786175));
#122309=CARTESIAN_POINT('Ctrl Pts',(-8.85792353649532,11.2950976932142,
10.7122626884846));
#122310=CARTESIAN_POINT('Ctrl Pts',(-8.8564656241279,11.2946923451227,10.7181125440605));
#122311=CARTESIAN_POINT('Ctrl Pts',(-8.85332711594917,11.2937887526367,
10.7311309429709));
#122312=CARTESIAN_POINT('Ctrl Pts',(-8.85166871262495,11.2932898220047,
10.7383045223447));
#122313=CARTESIAN_POINT('Ctrl Pts',(-8.84700850419926,11.2918221278411,
10.7593604398945));
#122314=CARTESIAN_POINT('Ctrl Pts',(-8.84419051911569,11.2908476412599,
10.7732816711453));
#122315=CARTESIAN_POINT('Ctrl Pts',(-8.82992302083362,11.2853847642603,
10.8509649057126));
#122316=CARTESIAN_POINT('Ctrl Pts',(-8.82349952669627,11.280742163358,10.9155263878737));
#122317=CARTESIAN_POINT('Ctrl Pts',(-8.82128489779045,11.2710903312503,
11.0477676259102));
#122318=CARTESIAN_POINT('Ctrl Pts',(-8.82595839374699,11.2660917158784,
11.1152283383518));
#122319=CARTESIAN_POINT('Ctrl Pts',(-8.84044223454589,11.2593432209551,
11.2078724492724));
#122320=CARTESIAN_POINT('Ctrl Pts',(-8.84536754271233,11.2574768950459,
11.2336863150586));
#122321=CARTESIAN_POINT('Ctrl Pts',(-8.85261869556331,11.2551886982754,
11.2658111016204));
#122322=CARTESIAN_POINT('Ctrl Pts',(-8.85413988014996,11.2547287197831,
11.2722939411926));
#122323=CARTESIAN_POINT('Ctrl Pts',(-8.85662413841964,11.2540083558031,
11.2824914554336));
#122324=CARTESIAN_POINT('Ctrl Pts',(-8.85755049499621,11.2537460061904,
11.2862148018765));
#122325=CARTESIAN_POINT('Ctrl Pts',(-8.85933823718161,11.2532514223385,
11.2932533666002));
#122326=CARTESIAN_POINT('Ctrl Pts',(-8.86019588497293,11.2530189998139,
11.2965693407176));
#122327=CARTESIAN_POINT('Ctrl Pts',(-8.86225654724447,11.252471749424,11.3043956088194));
#122328=CARTESIAN_POINT('Ctrl Pts',(-8.86347192693217,11.2521576229194,
11.3089025605685));
#122329=CARTESIAN_POINT('Ctrl Pts',(-8.86761921668051,11.2511135674627,
11.3239259351954));
#122330=CARTESIAN_POINT('Ctrl Pts',(-8.87067065077571,11.2503900302297,
11.3344091682097));
#122331=CARTESIAN_POINT('Ctrl Pts',(-8.8784476400569,11.2486459915908,11.359805565952));
#122332=CARTESIAN_POINT('Ctrl Pts',(-8.88332547588599,11.2476326300367,
11.3746702515226));
#122333=CARTESIAN_POINT('Ctrl Pts',(-8.90438899898507,11.2435480306065,
11.4347886260867));
#122334=CARTESIAN_POINT('Ctrl Pts',(-8.92304212565801,11.2405662064929,
11.4791315488177));
#122335=CARTESIAN_POINT('Ctrl Pts',(-8.98233876458414,11.2322890143681,
11.5989987525076));
#122336=CARTESIAN_POINT('Ctrl Pts',(-9.0285826415389,11.2270154786977,11.6714016635962));
#122337=CARTESIAN_POINT('Ctrl Pts',(-9.0921286174542,11.2204129489149,11.7504080386997));
#122338=CARTESIAN_POINT('Ctrl Pts',(-9.1022351409386,11.2193795033654,11.7624702562932));
#122339=CARTESIAN_POINT('Ctrl Pts',(-9.11761871959068,11.2178283662472,
11.7801006831076));
#122340=CARTESIAN_POINT('Ctrl Pts',(-9.12271367120461,11.2173180604035,
11.7858259937624));
#122341=CARTESIAN_POINT('Ctrl Pts',(-9.13193104138223,11.2164006628796,
11.7959823920354));
#122342=CARTESIAN_POINT('Ctrl Pts',(-9.13603245714807,11.215994453862,11.8004322381772));
#122343=CARTESIAN_POINT('Ctrl Pts',(-9.14481828769405,11.2151283863368,
11.8098182566846));
#122344=CARTESIAN_POINT('Ctrl Pts',(-9.14951153879956,11.2146681617618,
11.8147458155361));
#122345=CARTESIAN_POINT('Ctrl Pts',(-9.16228133093817,11.2134222056775,
11.8279225627887));
#122346=CARTESIAN_POINT('Ctrl Pts',(-9.17043671795362,11.2126330972982,
11.8360939439518));
#122347=CARTESIAN_POINT('Ctrl Pts',(-9.21633715964392,11.2082265685633,
11.8807516670098));
#122348=CARTESIAN_POINT('Ctrl Pts',(-9.25636370237924,11.2045077203375,
11.9147975774346));
#122349=CARTESIAN_POINT('Ctrl Pts',(-9.36225645454631,11.1949779082525,
11.9933144294481));
#122350=CARTESIAN_POINT('Ctrl Pts',(-9.43059862275343,11.1890842163386,
12.0340075001627));
#122351=CARTESIAN_POINT('Ctrl Pts',(-9.53042256950844,11.1811217645572,
12.0805278330715));
#122352=CARTESIAN_POINT('Ctrl Pts',(-9.55883707669991,11.1789243982566,
12.0924371825522));
#122353=CARTESIAN_POINT('Ctrl Pts',(-9.59413595809878,11.1763036470834,
12.1056296038588));
#122354=CARTESIAN_POINT('Ctrl Pts',(-9.6006048061927,11.1758277648368,12.1079828185775));
#122355=CARTESIAN_POINT('Ctrl Pts',(-9.61079534325875,11.1750853773126,
12.1115890483473));
#122356=CARTESIAN_POINT('Ctrl Pts',(-9.61450317690428,11.1748167629088,
12.1128803519465));
#122357=CARTESIAN_POINT('Ctrl Pts',(-9.62111497469947,11.1743405287551,
12.1151459910997));
#122358=CARTESIAN_POINT('Ctrl Pts',(-9.62401629098665,11.174132502201,12.1161275441228));
#122359=CARTESIAN_POINT('Ctrl Pts',(-9.63101119437675,11.1736332095339,
12.1184636403855));
#122360=CARTESIAN_POINT('Ctrl Pts',(-9.63510843031541,11.1733425888863,
12.119807035779));
#122361=CARTESIAN_POINT('Ctrl Pts',(-9.64773799338084,11.1724521404418,
12.1238713193084));
#122362=CARTESIAN_POINT('Ctrl Pts',(-9.65629428472368,11.171856404055,12.1265174906952));
#122363=CARTESIAN_POINT('Ctrl Pts',(-9.6764334797956,11.1704699667828,12.1324950356505));
#122364=CARTESIAN_POINT('Ctrl Pts',(-9.68803915802647,11.1696831261186,
12.1357467834655));
#122365=CARTESIAN_POINT('Ctrl Pts',(-9.72996032999592,11.1668776194249,
12.1468013964896));
#122366=CARTESIAN_POINT('Ctrl Pts',(-9.76053584938151,11.1648996891446,
12.1535736052226));
#122367=CARTESIAN_POINT('Ctrl Pts',(-9.80670408327826,11.161966914709,12.161884347791));
#122368=CARTESIAN_POINT('Ctrl Pts',(-9.82211498184402,11.1609968521491,
12.1643433706988));
#122369=CARTESIAN_POINT('Ctrl Pts',(-9.93122761341439,11.154165377668,12.1795368450491));
#122370=CARTESIAN_POINT('Ctrl Pts',(-10.0261035645613,11.1483817612358,
12.181250781766));
#122371=CARTESIAN_POINT('Ctrl Pts',(-10.1348632709454,11.1412526725535,
12.1700963246834));
#122372=CARTESIAN_POINT('Ctrl Pts',(-10.1495358962874,11.140281135277,12.1683118141402));
#122373=CARTESIAN_POINT('Ctrl Pts',(-10.1716725003214,11.1387987313983,
12.1651956958818));
#122374=CARTESIAN_POINT('Ctrl Pts',(-10.179163942804,11.1382941638889,12.1640673237334));
#122375=CARTESIAN_POINT('Ctrl Pts',(-10.1926108222015,11.1373830321057,
12.1619090566164));
#122376=CARTESIAN_POINT('Ctrl Pts',(-10.1985702534752,11.1369773017429,
12.1609054383492));
#122377=CARTESIAN_POINT('Ctrl Pts',(-10.2112783240323,11.1361078551258,
12.1586645783361));
#122378=CARTESIAN_POINT('Ctrl Pts',(-10.2180243781897,11.1356437388738,
12.1574141447096));
#122379=CARTESIAN_POINT('Ctrl Pts',(-10.2363462909496,11.1343760208711,
12.153852171281));
#122380=CARTESIAN_POINT('Ctrl Pts',(-10.2478986783004,11.1335688366078,
12.1514254774599));
#122381=CARTESIAN_POINT('Ctrl Pts',(-10.3160322140127,11.1287600229732,
12.1360404827966));
#122382=CARTESIAN_POINT('Ctrl Pts',(-10.3716207032903,11.1246330203112,
12.1190891564534));
#122383=CARTESIAN_POINT('Ctrl Pts',(-10.4963313629057,11.1149267169187,
12.0707401985779));
#122384=CARTESIAN_POINT('Ctrl Pts',(-10.5641290084596,11.1093050131847,
12.0366230969395));
#122385=CARTESIAN_POINT('Ctrl Pts',(-10.6523989116582,11.1017761560084,
11.980964019803));
#122386=CARTESIAN_POINT('Ctrl Pts',(-10.6760539964246,11.0997374268553,
11.9648139930955));
#122387=CARTESIAN_POINT('Ctrl Pts',(-10.7045273187046,11.0972778822531,
11.943812385895));
#122388=CARTESIAN_POINT('Ctrl Pts',(-10.709921447103,11.0968116881393,11.9397617287672));
#122389=CARTESIAN_POINT('Ctrl Pts',(-10.7183748560127,11.0960810817562,
11.9332994150732));
#122390=CARTESIAN_POINT('Ctrl Pts',(-10.7214573842745,11.0958146646942,
11.9309186192726));
#122391=CARTESIAN_POINT('Ctrl Pts',(-10.7269471251834,11.0953402772547,
11.9266349628011));
#122392=CARTESIAN_POINT('Ctrl Pts',(-10.7293587158861,11.0951319195112,
11.9247379850288));
#122393=CARTESIAN_POINT('Ctrl Pts',(-10.7351780436037,11.094629185484,11.920123525881));
#122394=CARTESIAN_POINT('Ctrl Pts',(-10.7385781451713,11.0943354803106,
11.9173965247727));
#122395=CARTESIAN_POINT('Ctrl Pts',(-10.7491073078336,11.0934257747851,
11.9088552854706));
#122396=CARTESIAN_POINT('Ctrl Pts',(-10.7561836443658,11.0928141255971,
11.9029761887233));
#122397=CARTESIAN_POINT('Ctrl Pts',(-10.7726960913151,11.0913842430596,
11.8889272028956));
#122398=CARTESIAN_POINT('Ctrl Pts',(-10.7820728106409,11.090570209226,11.8806889162199));
#122399=CARTESIAN_POINT('Ctrl Pts',(-10.8158073448324,11.0876263052474,
11.8500863349232));
#122400=CARTESIAN_POINT('Ctrl Pts',(-10.8393528450589,11.0855415689328,
11.8268467299764));
#122401=CARTESIAN_POINT('Ctrl Pts',(-10.9143410623074,11.0786744622705,
11.7463234589442));
#122402=CARTESIAN_POINT('Ctrl Pts',(-10.9611433970977,11.0739892884291,
11.6849975471589));
#122403=CARTESIAN_POINT('Ctrl Pts',(-11.0213865364239,11.0667442577068,
11.5876013288456));
#122404=CARTESIAN_POINT('Ctrl Pts',(-11.0396032752786,11.0643312433426,
11.5547345085694));
#122405=CARTESIAN_POINT('Ctrl Pts',(-11.0610643460701,11.0611432712156,
11.5112313846294));
#122406=CARTESIAN_POINT('Ctrl Pts',(-11.0657735785254,11.0604188728548,
11.5013399457858));
#122407=CARTESIAN_POINT('Ctrl Pts',(-11.0731299533268,11.0592453726583,
11.4853161366395));
#122408=CARTESIAN_POINT('Ctrl Pts',(-11.0758641813459,11.0587992389096,
11.4792242788184));
#122409=CARTESIAN_POINT('Ctrl Pts',(-11.0809882343679,11.0579436051517,
11.4675429919504));
#122410=CARTESIAN_POINT('Ctrl Pts',(-11.0833868833319,11.0575344191036,
11.4619576504541));
#122411=CARTESIAN_POINT('Ctrl Pts',(-11.0888016531507,11.0565903397104,
11.4490750137273));
#122412=CARTESIAN_POINT('Ctrl Pts',(-11.0917878117162,11.0560544657919,
11.4417655224118));
#122413=CARTESIAN_POINT('Ctrl Pts',(-11.100962218157,11.0543586312355,11.4186471822516));
#122414=CARTESIAN_POINT('Ctrl Pts',(-11.1068820398805,11.0531899206166,
11.4027348592538));
#122415=CARTESIAN_POINT('Ctrl Pts',(-11.1199736667424,11.0504189415259,
11.3650730484422));
#122416=CARTESIAN_POINT('Ctrl Pts',(-11.1268589372337,11.0488081894755,
11.3432319351265));
#122417=CARTESIAN_POINT('Ctrl Pts',(-11.1650240896711,11.0388568114994,
11.2085982426991));
#122418=CARTESIAN_POINT('Ctrl Pts',(-11.1799769951264,11.0300474056564,
11.0918834662697));
#122419=CARTESIAN_POINT('Ctrl Pts',(-11.1771332988819,11.0205753676004,
10.9585233022005));
#122420=CARTESIAN_POINT('Ctrl Pts',(-11.1764429523605,11.0194251399042,
10.9421625932513));
#122421=CARTESIAN_POINT('Ctrl Pts',(-11.1750563531718,11.0179008211877,
10.9201911895189));
#122422=CARTESIAN_POINT('Ctrl Pts',(-11.174660636672,11.0175122386487,10.9145642275563));
#122423=CARTESIAN_POINT('Ctrl Pts',(-11.1739728896703,11.0169028658525,
10.905695668058));
#122424=CARTESIAN_POINT('Ctrl Pts',(-11.17370783061,11.0166806464345,10.9024521567633));
#122425=CARTESIAN_POINT('Ctrl Pts',(-11.1731321422063,11.0162228520569,
10.8957498262941));
#122426=CARTESIAN_POINT('Ctrl Pts',(-11.1728196555916,11.0159873949953,
10.8922912371738));
#122427=CARTESIAN_POINT('Ctrl Pts',(-11.1720239975761,11.0154178674021,
10.8838992565372));
#122428=CARTESIAN_POINT('Ctrl Pts',(-11.1715249619692,11.0150846606449,
10.8789673630975));
#122429=CARTESIAN_POINT('Ctrl Pts',(-11.1696349682116,11.0139024641359,
10.8613971084884));
#122430=CARTESIAN_POINT('Ctrl Pts',(-11.1680704565681,11.0130623927603,
10.8487777760091));
#122431=CARTESIAN_POINT('Ctrl Pts',(-11.1636281513183,11.0109740164168,
10.8171500932583));
#122432=CARTESIAN_POINT('Ctrl Pts',(-11.1604887097481,11.009737100129,10.7981817626773));
#122433=CARTESIAN_POINT('Ctrl Pts',(-11.1434602758955,11.0039546723689,
10.7089214109206));
#122434=CARTESIAN_POINT('Ctrl Pts',(-11.1236399454783,10.9995889118622,
10.6399128527113));
#122435=CARTESIAN_POINT('Ctrl Pts',(-11.0752779747691,10.9912927308428,
10.5155530809471));
#122436=CARTESIAN_POINT('Ctrl Pts',(-11.0483945116772,10.9873987249763,
10.4598342649403));
#122437=CARTESIAN_POINT('Ctrl Pts',(-11.0111714760072,10.9825575506522,
10.3960350369925));
#122438=CARTESIAN_POINT('Ctrl Pts',(-11.004914218444,10.9817592599538,10.3856801921034));
#122439=CARTESIAN_POINT('Ctrl Pts',(-10.9947894379346,10.9804904141443,
10.3694938854948));
#122440=CARTESIAN_POINT('Ctrl Pts',(-10.9910274523769,10.9800236837695,
10.3635971626855));
#122441=CARTESIAN_POINT('Ctrl Pts',(-10.9839247349748,10.9791509701349,
10.3526797219019));
#122442=CARTESIAN_POINT('Ctrl Pts',(-10.9805975180125,10.9787454942994,
10.3476504526822));
#122443=CARTESIAN_POINT('Ctrl Pts',(-10.9731061311413,10.9778397697463,
10.3365136320482));
#122444=CARTESIAN_POINT('Ctrl Pts',(-10.9689228169994,10.977338818661,10.3304193302415));
#122445=CARTESIAN_POINT('Ctrl Pts',(-10.9564516846754,10.9758591312999,
10.312612849279));
#122446=CARTESIAN_POINT('Ctrl Pts',(-10.9480071430515,10.9748745287189,
10.3010126286232));
#122447=CARTESIAN_POINT('Ctrl Pts',(-10.9086419514347,10.9703596274273,
10.2489627222537));
#122448=CARTESIAN_POINT('Ctrl Pts',(-10.8753341775915,10.9667385411551,
10.2103950176387));
#122449=CARTESIAN_POINT('Ctrl Pts',(-10.7818982931113,10.9570856641998,
10.1154038814592));
#122450=CARTESIAN_POINT('Ctrl Pts',(-10.7181625000867,10.9509598380189,
10.0629208912601));
#122451=CARTESIAN_POINT('Ctrl Pts',(-10.6284213187806,10.9432267710343,
10.0035971179078));
#122452=CARTESIAN_POINT('Ctrl Pts',(-10.6069232326493,10.941435618148,9.99035825081243));
#122453=CARTESIAN_POINT('Ctrl Pts',(-10.5793148119248,10.9392260709056,
9.97455739320516));
#122454=CARTESIAN_POINT('Ctrl Pts',(-10.5735876910458,10.9387725074589,
9.97134293528797));
#122455=CARTESIAN_POINT('Ctrl Pts',(-10.5644899632893,10.9380598930056,
9.96633626767257));
#122456=CARTESIAN_POINT('Ctrl Pts',(-10.5611371215611,10.9377989456487,
9.96451230715521));
#122457=CARTESIAN_POINT('Ctrl Pts',(-10.5547534261991,10.9373053710769,
9.9610796606097));
#122458=CARTESIAN_POINT('Ctrl Pts',(-10.551724422581,10.9370725688616,9.95946792586443));
#122459=CARTESIAN_POINT('Ctrl Pts',(-10.5445217493021,10.9365222107504,
9.95567567313349));
#122460=CARTESIAN_POINT('Ctrl Pts',(-10.5403419802501,10.9362053796808,
9.95350691286821));
#122461=CARTESIAN_POINT('Ctrl Pts',(-10.5262128007504,10.9351425447922,
9.94628291603847));
#122462=CARTESIAN_POINT('Ctrl Pts',(-10.5162042222657,10.9344032503157,
9.94134385759972));
#122463=CARTESIAN_POINT('Ctrl Pts',(-10.4915811537853,10.9326137074118,
9.92962505603652));
#122464=CARTESIAN_POINT('Ctrl Pts',(-10.4768945548228,10.9315710975809,
9.92300130560755));
#122465=CARTESIAN_POINT('Ctrl Pts',(-10.415500051688,10.9272958590718,9.89681426892766));
#122466=CARTESIAN_POINT('Ctrl Pts',(-10.3676878529283,10.9241613900453,
9.87997077982901));
#122467=CARTESIAN_POINT('Ctrl Pts',(-10.2399934623775,10.9159544989636,
9.84404868849485));
#122468=CARTESIAN_POINT('Ctrl Pts',(-10.1589562433228,10.910892454728,9.83014905191553));
#122469=CARTESIAN_POINT('Ctrl Pts',(-10.0612671311687,10.9045191209752,
9.82373713324707));
#122470=CARTESIAN_POINT('Ctrl Pts',(-10.0453786679518,10.903474847725,9.82301710697184));
#122471=CARTESIAN_POINT('Ctrl Pts',(-10.0217874163671,10.9019106070592,
9.82242639266425));
#122472=CARTESIAN_POINT('Ctrl Pts',(-10.0140921974884,10.9013982132125,
9.82230916727659));
#122473=CARTESIAN_POINT('Ctrl Pts',(-10.0003416268194,10.9004785159569,
9.82223448481794));
#122474=CARTESIAN_POINT('Ctrl Pts',(-9.99428665641062,10.9000721129608,
9.82224829406564));
#122475=CARTESIAN_POINT('Ctrl Pts',(-9.98144680430788,10.8992071787009,
9.8223765937133));
#122476=CARTESIAN_POINT('Ctrl Pts',(-9.97466229012247,10.8987482932007,
9.8225030338731));
#122477=CARTESIAN_POINT('Ctrl Pts',(-9.95642824684165,10.8975098091194,
9.82300051376034));
#122478=CARTESIAN_POINT('Ctrl Pts',(-9.94498265842873,10.896726903093,9.82347997707295));
#122479=CARTESIAN_POINT('Ctrl Pts',(-9.89253117305323,10.8931127066122,
9.82644424029201));
#122480=CARTESIAN_POINT('Ctrl Pts',(-9.85167674298975,10.8902221159927,
9.83090586595053));
#122481=CARTESIAN_POINT('Ctrl Pts',(-9.81114928308311,10.8872795026091,
9.83748958317786));
#122482=CARTESIAN_POINT('Ctrl Pts',(-9.81114930150155,10.7889089429636,
9.83748958018577));
#122483=CARTESIAN_POINT('Ctrl Pts',(-9.8144593237119,10.7891361684467,9.8369518645698));
#122484=CARTESIAN_POINT('Ctrl Pts',(-9.81777168141626,10.7893626048123,
9.83642827959523));
#122485=CARTESIAN_POINT('Ctrl Pts',(-9.827712887307,10.7900394733218,9.83490036371816));
#122486=CARTESIAN_POINT('Ctrl Pts',(-9.83434825740727,10.790487630429,9.83393845916146));
#122487=CARTESIAN_POINT('Ctrl Pts',(-9.86875879015411,10.7927946712871,
9.82924975546467));
#122488=CARTESIAN_POINT('Ctrl Pts',(-9.89665466635841,10.794607506475,9.82645817476321));
#122489=CARTESIAN_POINT('Ctrl Pts',(-10.0038528350274,10.8014447613579,
9.81958357764544));
#122490=CARTESIAN_POINT('Ctrl Pts',(-10.0833946392679,10.8062607968729,
9.82252611025464));
#122491=CARTESIAN_POINT('Ctrl Pts',(-10.2122743425764,10.814381625533,9.84042814460704));
#122492=CARTESIAN_POINT('Ctrl Pts',(-10.2620005807527,10.8175921965828,
9.8506427437954));
#122493=CARTESIAN_POINT('Ctrl Pts',(-10.3247215447131,10.8218373602538,
9.86780919294558));
#122494=CARTESIAN_POINT('Ctrl Pts',(-10.3384622984233,10.8227795059351,
9.87184072538561));
#122495=CARTESIAN_POINT('Ctrl Pts',(-10.3591728371484,10.8242196756507,
9.8783296057735));
#122496=CARTESIAN_POINT('Ctrl Pts',(-10.3661989455015,10.8247118067191,
9.88060376613859));
#122497=CARTESIAN_POINT('Ctrl Pts',(-10.3789207118352,10.8256095685739,
9.88485404674034));
#122498=CARTESIAN_POINT('Ctrl Pts',(-10.3846235101295,10.8260144704899,
9.88680812252446));
#122499=CARTESIAN_POINT('Ctrl Pts',(-10.3969120176277,10.8268924168771,
9.89112450529975));
#122500=CARTESIAN_POINT('Ctrl Pts',(-10.4034921508497,10.8273659419933,
9.89350187842935));
#122501=CARTESIAN_POINT('Ctrl Pts',(-10.4214047022346,10.8286645296677,
9.90015463003992));
#122502=CARTESIAN_POINT('Ctrl Pts',(-10.4326927044636,10.829493385962,9.90454631982017));
#122503=CARTESIAN_POINT('Ctrl Pts',(-10.5111654495748,10.8353314633858,
9.9364788905191));
#122504=CARTESIAN_POINT('Ctrl Pts',(-10.5757332186308,10.8405424995343,
9.97000238888947));
#122505=CARTESIAN_POINT('Ctrl Pts',(-10.6814364158687,10.8497287349869,
10.0379419583048));
#122506=CARTESIAN_POINT('Ctrl Pts',(-10.7240880825547,10.8536451428551,
10.0696195402373));
#122507=CARTESIAN_POINT('Ctrl Pts',(-10.7912349182959,10.86005092236,10.1269127512082));
#122508=CARTESIAN_POINT('Ctrl Pts',(-10.8169766463867,10.8625727204107,
10.1509512934915));
#122509=CARTESIAN_POINT('Ctrl Pts',(-10.8465956363163,10.8655195731447,
10.1812071173854));
#122510=CARTESIAN_POINT('Ctrl Pts',(-10.8515399137799,10.8660130843019,
10.1863503594516));
#122511=CARTESIAN_POINT('Ctrl Pts',(-10.8591708012771,10.8667768243067,
10.1944340784882));
#122512=CARTESIAN_POINT('Ctrl Pts',(-10.8618896488329,10.8670493579885,
10.1973436886935));
#122513=CARTESIAN_POINT('Ctrl Pts',(-10.8668988871079,10.8675521607834,
10.2027591917504));
#122514=CARTESIAN_POINT('Ctrl Pts',(-10.8691932052722,10.8677827118702,
10.2052612006607));
#122515=CARTESIAN_POINT('Ctrl Pts',(-10.8744486211256,10.8683114604281,
10.211042339073));
#122516=CARTESIAN_POINT('Ctrl Pts',(-10.8774021178296,10.8686090987479,
10.2143282447963));
#122517=CARTESIAN_POINT('Ctrl Pts',(-10.8866609276319,10.8695439936189,
10.2247464379767));
#122518=CARTESIAN_POINT('Ctrl Pts',(-10.8928984840552,10.8701765458684,
10.2319388062561));
#122519=CARTESIAN_POINT('Ctrl Pts',(-10.9386339562835,10.8748420891566,
10.2859855236954));
#122520=CARTESIAN_POINT('Ctrl Pts',(-10.9745136452726,10.8786603880657,
10.3357895456284));
#122521=CARTESIAN_POINT('Ctrl Pts',(-11.0535043594221,10.8880804548332,
10.4657151140089));
#122522=CARTESIAN_POINT('Ctrl Pts',(-11.0915251390269,10.893646528456,10.5484442323766));
#122523=CARTESIAN_POINT('Ctrl Pts',(-11.1244341133799,10.9005605155922,
10.6493165169617));
#122524=CARTESIAN_POINT('Ctrl Pts',(-11.1289116907196,10.9015697454868,
10.6640099111066));
#122525=CARTESIAN_POINT('Ctrl Pts',(-11.135170650419,10.9030914571677,10.6860887533817));
#122526=CARTESIAN_POINT('Ctrl Pts',(-11.1371701273765,10.9035969643369,
10.6934110680076));
#122527=CARTESIAN_POINT('Ctrl Pts',(-11.1406341138578,10.9045090139546,
10.7065968639862));
#122528=CARTESIAN_POINT('Ctrl Pts',(-11.14212454616,10.9049147137898,10.7124533069996));
#122529=CARTESIAN_POINT('Ctrl Pts',(-11.1452076572052,10.9057832452661,
10.7249702184464));
#122530=CARTESIAN_POINT('Ctrl Pts',(-11.1467874397167,10.9062464701126,
10.7316336020427));
#122531=CARTESIAN_POINT('Ctrl Pts',(-11.150919788985,10.9075095671303,10.7497665785463));
#122532=CARTESIAN_POINT('Ctrl Pts',(-11.1533589090503,10.908312979138,10.7612609468987));
#122533=CARTESIAN_POINT('Ctrl Pts',(-11.1665897087619,10.913034048415,10.8285547238772));
#122534=CARTESIAN_POINT('Ctrl Pts',(-11.1735014294451,10.9170716159459,
10.885031825212));
#122535=CARTESIAN_POINT('Ctrl Pts',(-11.1804451077102,10.9272568225237,
11.0253254308749));
#122536=CARTESIAN_POINT('Ctrl Pts',(-11.1756680193083,10.9334833199346,
11.1090702660529));
#122537=CARTESIAN_POINT('Ctrl Pts',(-11.158336334938,10.9411198425625,11.2141867536234));
#122538=CARTESIAN_POINT('Ctrl Pts',(-11.1539544793022,10.9427403094235,
11.2366606330973));
#122539=CARTESIAN_POINT('Ctrl Pts',(-11.1475214520918,10.9447709004562,
11.2651980843082));
#122540=CARTESIAN_POINT('Ctrl Pts',(-11.1460726737853,10.9452098898798,
11.2713907475448));
#122541=CARTESIAN_POINT('Ctrl Pts',(-11.1436851393827,10.9459048350956,
11.2812358102571));
#122542=CARTESIAN_POINT('Ctrl Pts',(-11.1427789075989,10.946162537087,11.2848958553062));
#122543=CARTESIAN_POINT('Ctrl Pts',(-11.1410108050414,10.9466538382636,
11.2918925840473));
#122544=CARTESIAN_POINT('Ctrl Pts',(-11.1401518526684,10.9468875866058,
11.2952298951571));
#122545=CARTESIAN_POINT('Ctrl Pts',(-11.1380593964943,10.9474454947647,
11.3032144289846));
#122546=CARTESIAN_POINT('Ctrl Pts',(-11.1368120431204,10.9477688771236,
11.3078580200561));
#122547=CARTESIAN_POINT('Ctrl Pts',(-11.1324137013399,10.9488785959615,
11.3238406549219));
#122548=CARTESIAN_POINT('Ctrl Pts',(-11.1291211003856,10.9496573933126,
11.3351404589956));
#122549=CARTESIAN_POINT('Ctrl Pts',(-11.1205704794178,10.9515625215844,
11.3629273495246));
#122550=CARTESIAN_POINT('Ctrl Pts',(-11.1151173285943,10.952679860437,11.3793519044553));
#122551=CARTESIAN_POINT('Ctrl Pts',(-11.0898808950359,10.9574789713828,
11.4501083624561));
#122552=CARTESIAN_POINT('Ctrl Pts',(-11.0664727513307,10.9610366562839,
11.5030653410641));
#122553=CARTESIAN_POINT('Ctrl Pts',(-11.0052148020642,10.9690935171345,
11.6179622217489));
#122554=CARTESIAN_POINT('Ctrl Pts',(-10.9653508562184,10.9735932756457,
11.6785500139398));
#122555=CARTESIAN_POINT('Ctrl Pts',(-10.9101012266667,10.9793535925768,
11.7477109429893));
#122556=CARTESIAN_POINT('Ctrl Pts',(-10.8997629076585,10.9804137361944,
11.7601200998497));
#122557=CARTESIAN_POINT('Ctrl Pts',(-10.8840966259385,10.9819970799163,
11.7781568918825));
#122558=CARTESIAN_POINT('Ctrl Pts',(-10.8789627613031,10.9825124262236,
11.7839511795043));
#122559=CARTESIAN_POINT('Ctrl Pts',(-10.8697099841708,10.9834352929785,
11.7941890901225));
#122560=CARTESIAN_POINT('Ctrl Pts',(-10.8656131645881,10.9838418871966,
11.7986523739334));
#122561=CARTESIAN_POINT('Ctrl Pts',(-10.856875235057,10.9847049829542,11.808025705275));
#122562=CARTESIAN_POINT('Ctrl Pts',(-10.8522259604238,10.9851618214502,
11.8129278061044));
#122563=CARTESIAN_POINT('Ctrl Pts',(-10.8396714015447,10.9863892637121,
11.8259390095289));
#122564=CARTESIAN_POINT('Ctrl Pts',(-10.8316910701045,10.9871630748054,
11.8339743751608));
#122565=CARTESIAN_POINT('Ctrl Pts',(-10.7888658749981,10.991283449389,11.8758688518904));
#122566=CARTESIAN_POINT('Ctrl Pts',(-10.7520710145602,10.9947161786266,
11.9076583514454));
#122567=CARTESIAN_POINT('Ctrl Pts',(-10.6733618378722,11.0018457784109,
11.9675815230439));
#122568=CARTESIAN_POINT('Ctrl Pts',(-10.6313883231267,11.0055406254961,
11.9954789746541));
#122569=CARTESIAN_POINT('Ctrl Pts',(-10.57134985927,11.0106243083954,12.0300548876868));
#122570=CARTESIAN_POINT('Ctrl Pts',(-10.5547124072893,11.0120127402581,
12.0391091848679));
#122571=CARTESIAN_POINT('Ctrl Pts',(-10.4985494486609,11.0166204464434,
12.0679402708649));
#122572=CARTESIAN_POINT('Ctrl Pts',(-10.4581258493629,11.0198101379962,
12.0858957395375));
#122573=CARTESIAN_POINT('Ctrl Pts',(-10.410458730477,11.0233601789877,12.1039313549433));
#122574=CARTESIAN_POINT('Ctrl Pts',(-10.4041123207451,11.0238286104358,
12.1062703301498));
#122575=CARTESIAN_POINT('Ctrl Pts',(-10.3937407970433,11.0245868870124,
12.1099916006046));
#122576=CARTESIAN_POINT('Ctrl Pts',(-10.3897278236745,11.0248785250987,
12.1114069432687));
#122577=CARTESIAN_POINT('Ctrl Pts',(-10.382509348481,11.0253998624469,12.1139089350421));
#122578=CARTESIAN_POINT('Ctrl Pts',(-10.3793067593123,11.0256300082825,
12.1150035427895));
#122579=CARTESIAN_POINT('Ctrl Pts',(-10.3722047134575,11.0261378292643,
12.1173967981541));
#122580=CARTESIAN_POINT('Ctrl Pts',(-10.3683031477281,11.0264151242766,
12.1186888512445));
#122581=CARTESIAN_POINT('Ctrl Pts',(-10.3568383159114,11.0272252609451,
12.1224190948198));
#122582=CARTESIAN_POINT('Ctrl Pts',(-10.3492568645201,11.0277550076889,
12.1248012531785));
#122583=CARTESIAN_POINT('Ctrl Pts',(-10.3317693823475,11.0289644734875,
12.1301021066745));
#122584=CARTESIAN_POINT('Ctrl Pts',(-10.3218477920664,11.0296415517963,
12.1329676558844));
#122585=CARTESIAN_POINT('Ctrl Pts',(-10.2880462969432,11.0319214656636,
12.1422503065539));
#122586=CARTESIAN_POINT('Ctrl Pts',(-10.2640013017299,11.0334982650823,
12.1480461235296));
#122587=CARTESIAN_POINT('Ctrl Pts',(-10.1882547885436,11.038375355526,12.1637980723468));
#122588=CARTESIAN_POINT('Ctrl Pts',(-10.1360568300788,11.0416087234541,
12.171048597162));
#122589=CARTESIAN_POINT('Ctrl Pts',(-10.0120533944585,11.0493107767507,
12.1798673576524));
#122590=CARTESIAN_POINT('Ctrl Pts',(-9.94025454983669,11.0537940229939,
12.1784145241942));
#122591=CARTESIAN_POINT('Ctrl Pts',(-9.8568507494053,11.0592927079498,12.1690824397815));
#122592=CARTESIAN_POINT('Ctrl Pts',(-9.84468561160191,11.0601017044701,
12.1675285355699));
#122593=CARTESIAN_POINT('Ctrl Pts',(-9.8255883191371,11.0613837231064,12.164785411527));
#122594=CARTESIAN_POINT('Ctrl Pts',(-9.81863854099204,11.0618527832158,
12.1637235526157));
#122595=CARTESIAN_POINT('Ctrl Pts',(-9.80575001255119,11.0627275359033,
12.1616360537669));
#122596=CARTESIAN_POINT('Ctrl Pts',(-9.79980879365612,11.0631326994353,
12.160626924394));
#122597=CARTESIAN_POINT('Ctrl Pts',(-9.78664565985859,11.064034773709,12.1582870597943));
#122598=CARTESIAN_POINT('Ctrl Pts',(-9.77942796904358,11.0645323607029,
12.1569342947126));
#122599=CARTESIAN_POINT('Ctrl Pts',(-9.7583769236949,11.0659925158156,12.1527846851136));
#122600=CARTESIAN_POINT('Ctrl Pts',(-9.74458103501503,11.0669607195338,
12.1498066635739));
#122601=CARTESIAN_POINT('Ctrl Pts',(-9.71330299284559,11.0691825278767,
12.1424642118172));
#122602=CARTESIAN_POINT('Ctrl Pts',(-9.69586113915025,11.0704407090283,
12.1379451403868));
#122603=CARTESIAN_POINT('Ctrl Pts',(-9.63691182354621,11.0747595160042,
12.1212196909126));
#122604=CARTESIAN_POINT('Ctrl Pts',(-9.59597932292998,11.077873305584,12.1071283804173));
#122605=CARTESIAN_POINT('Ctrl Pts',(-9.49947310251629,11.085464492693,12.067839860856));
#122606=CARTESIAN_POINT('Ctrl Pts',(-9.44489799808155,11.0899706133088,
12.0405146790893));
#122607=CARTESIAN_POINT('Ctrl Pts',(-9.36233027863264,11.0969654688663,
11.9908215694962));
#122608=CARTESIAN_POINT('Ctrl Pts',(-9.33281399558934,11.0995040147299,
11.9711917455431));
#122609=CARTESIAN_POINT('Ctrl Pts',(-9.29846126704067,11.102467409513,11.9460388466418));
#122610=CARTESIAN_POINT('Ctrl Pts',(-9.29273585919675,11.1029615962512,
11.9417661783215));
#122611=CARTESIAN_POINT('Ctrl Pts',(-9.28387819621269,11.1037261551844,
11.9350296781316));
#122612=CARTESIAN_POINT('Ctrl Pts',(-9.28071908400707,11.1039988398429,
11.9326016844901));
#122613=CARTESIAN_POINT('Ctrl Pts',(-9.27489142543986,11.1045017762716,
11.9280755034191));
#122614=CARTESIAN_POINT('Ctrl Pts',(-9.2722196233885,11.1047323113588,11.9259818080442));
#122615=CARTESIAN_POINT('Ctrl Pts',(-9.26609352574576,11.105260837501,11.9211383399846));
#122616=CARTESIAN_POINT('Ctrl Pts',(-9.26264560281176,11.1055582711769,
11.9183806666404));
#122617=CARTESIAN_POINT('Ctrl Pts',(-9.25182539224047,11.1064918583267,
11.9096263661507));
#122618=CARTESIAN_POINT('Ctrl Pts',(-9.24450991058488,11.1071233261193,
11.9035596873271));
#122619=CARTESIAN_POINT('Ctrl Pts',(-9.20673439790415,11.1103903856575,
11.8714531340525));
#122620=CARTESIAN_POINT('Ctrl Pts',(-9.17754145612012,11.1129372616593,
11.843957051111));
#122621=CARTESIAN_POINT('Ctrl Pts',(-9.08483336891261,11.1213279952747,
11.7472481667146));
#122622=CARTESIAN_POINT('Ctrl Pts',(-9.02820134341422,11.1270042573511,
11.6719503984445));
#122623=CARTESIAN_POINT('Ctrl Pts',(-8.96708243901817,11.1347964440785,
11.5665320148384));
#122624=CARTESIAN_POINT('Ctrl Pts',(-8.95392220947762,11.1366086433628,
11.5418470942804));
#122625=CARTESIAN_POINT('Ctrl Pts',(-8.93734161571641,11.1390987676831,
11.5078866208787));
#122626=CARTESIAN_POINT('Ctrl Pts',(-8.93314037037807,11.1397499794866,
11.4990011847919));
#122627=CARTESIAN_POINT('Ctrl Pts',(-8.92637376313749,11.140833757778,11.4842139621393));
#122628=CARTESIAN_POINT('Ctrl Pts',(-8.92374463302754,11.141264145885,11.4783417605577));
#122629=CARTESIAN_POINT('Ctrl Pts',(-8.91868733941256,11.1421107105515,
11.4667934277452));
#122630=CARTESIAN_POINT('Ctrl Pts',(-8.91625542921269,11.1425267442592,
11.4611191569752));
#122631=CARTESIAN_POINT('Ctrl Pts',(-8.91057630777647,11.1435200909674,
11.4475751952879));
#122632=CARTESIAN_POINT('Ctrl Pts',(-8.90736963220345,11.1440987344948,
11.4396889916674));
#122633=CARTESIAN_POINT('Ctrl Pts',(-8.89669452749624,11.146087814776,11.4125975107195));
#122634=CARTESIAN_POINT('Ctrl Pts',(-8.88964512756509,11.1475118667593,
11.3932322932649));
#122635=CARTESIAN_POINT('Ctrl Pts',(-8.87368895003519,11.1510263661408,
11.3455425441044));
#122636=CARTESIAN_POINT('Ctrl Pts',(-8.86533859051338,11.1531328585483,
11.3170480581416));
#122637=CARTESIAN_POINT('Ctrl Pts',(-8.84499918826781,11.15910264228,11.2364775756994));
#122638=CARTESIAN_POINT('Ctrl Pts',(-8.83546410649209,11.1630197180775,
11.1838584316372));
#122639=CARTESIAN_POINT('Ctrl Pts',(-8.82293588981713,11.1712990794932,
11.0717305397439));
#122640=CARTESIAN_POINT('Ctrl Pts',(-8.82081545381712,11.1756506918968,
11.01226257693));
#122641=CARTESIAN_POINT('Ctrl Pts',(-8.82361997367075,11.1805727147056,
10.9422150672314));
#122642=CARTESIAN_POINT('Ctrl Pts',(-8.82419219630213,11.1813162300303,
10.9315522572618));
#122643=CARTESIAN_POINT('Ctrl Pts',(-8.82518929670315,11.1823398133931,
10.9167399006612));
#122644=CARTESIAN_POINT('Ctrl Pts',(-8.82549129422022,11.1826260520454,
10.9125829874173));
#122645=CARTESIAN_POINT('Ctrl Pts',(-8.82608242579897,11.1831460213998,
10.9050032114331));
#122646=CARTESIAN_POINT('Ctrl Pts',(-8.82636447943263,11.1833801305476,
10.9015798448634));
#122647=CARTESIAN_POINT('Ctrl Pts',(-8.82698210887803,11.1838651664396,
10.8944640578267));
#122648=CARTESIAN_POINT('Ctrl Pts',(-8.82732014744257,11.184115957482,10.8907719251042));
#122649=CARTESIAN_POINT('Ctrl Pts',(-8.8282579717746,11.1847751490537,10.8810354052362));
#122650=CARTESIAN_POINT('Ctrl Pts',(-8.82888710013355,11.1851819721369,
10.8749938593626));
#122651=CARTESIAN_POINT('Ctrl Pts',(-8.83204392164894,11.1870714275878,
10.8467980071097));
#122652=CARTESIAN_POINT('Ctrl Pts',(-8.83515387707686,11.1885249577439,
10.8247119081072));
#122653=CARTESIAN_POINT('Ctrl Pts',(-8.84634500104037,11.1928158873806,
10.7588435220824));
#122654=CARTESIAN_POINT('Ctrl Pts',(-8.85628293923035,11.1955870238585,
10.7154157750965));
#122655=CARTESIAN_POINT('Ctrl Pts',(-8.89396411720842,11.2039865621445,
10.5851862525209));
#122656=CARTESIAN_POINT('Ctrl Pts',(-8.92932579221778,11.2095696708637,
10.5009603958658));
#122657=CARTESIAN_POINT('Ctrl Pts',(-8.98156221155184,11.2165015554414,
10.4082951756153));
#122658=CARTESIAN_POINT('Ctrl Pts',(-8.98935089181854,11.2175089957556,
10.3950880451457));
#122659=CARTESIAN_POINT('Ctrl Pts',(-9.00137470629132,11.2190285370869,
10.3755801753981));
#122660=CARTESIAN_POINT('Ctrl Pts',(-9.00541673844993,11.2195336934714,
10.3691618861101));
#122661=CARTESIAN_POINT('Ctrl Pts',(-9.01278975502116,11.2204453618026,
10.3577013869853));
#122662=CARTESIAN_POINT('Ctrl Pts',(-9.01609811198099,11.2208510341149,
10.3526448822301));
#122663=CARTESIAN_POINT('Ctrl Pts',(-9.02324046569379,11.2217197805876,
10.3419097180139));
#122664=CARTESIAN_POINT('Ctrl Pts',(-9.02708538487016,11.2221832500721,
10.336238630722));
#122665=CARTESIAN_POINT('Ctrl Pts',(-9.03766716634926,11.2234477166518,
10.3209204556042));
#122666=CARTESIAN_POINT('Ctrl Pts',(-9.04449931818464,11.2242522666304,
10.3113404760051));
#122667=CARTESIAN_POINT('Ctrl Pts',(-9.08538431838967,11.2290003874276,
10.2557917829051));
#122668=CARTESIAN_POINT('Ctrl Pts',(-9.12260148474596,11.2330655416056,
10.2122577939222));
#122669=CARTESIAN_POINT('Ctrl Pts',(-9.21989597293735,11.2430980929595,
10.1139325299781));
#122670=CARTESIAN_POINT('Ctrl Pts',(-9.28276766226697,11.2491322247577,
10.0623139069738));
#122671=CARTESIAN_POINT('Ctrl Pts',(-9.37104826978553,11.2567349955457,
10.0039453485187));
#122672=CARTESIAN_POINT('Ctrl Pts',(-9.39207716277581,11.2584869077926,
9.99097315477275));
#122673=CARTESIAN_POINT('Ctrl Pts',(-9.41915158789648,11.2606551767727,
9.97542562214886));
#122674=CARTESIAN_POINT('Ctrl Pts',(-9.42483003208833,11.2611052125408,
9.97222714257835));
#122675=CARTESIAN_POINT('Ctrl Pts',(-9.43386560808367,11.2618135180266,
9.96723604273454));
#122676=CARTESIAN_POINT('Ctrl Pts',(-9.43720527916555,11.2620736475487,
9.96541233122933));
#122677=CARTESIAN_POINT('Ctrl Pts',(-9.44357529998175,11.2625665614581,
9.961973793474));
#122678=CARTESIAN_POINT('Ctrl Pts',(-9.44660386016015,11.2627995136631,
9.96035603934288));
#122679=CARTESIAN_POINT('Ctrl Pts',(-9.45382122468548,11.2633514243431,
9.95654124209201));
#122680=CARTESIAN_POINT('Ctrl Pts',(-9.45801625725096,11.2636696455486,
9.95435615118438));
#122681=CARTESIAN_POINT('Ctrl Pts',(-9.47226945304297,11.2647425489247,
9.94704082977616));
#122682=CARTESIAN_POINT('Ctrl Pts',(-9.48238854890885,11.2654903467187,
9.94202979577966));
#122683=CARTESIAN_POINT('Ctrl Pts',(-9.50734571199425,11.2673046553543,
9.93011468490168));
#122684=CARTESIAN_POINT('Ctrl Pts',(-9.52225892809573,11.2683632469225,
9.92337269303126));
#122685=CARTESIAN_POINT('Ctrl Pts',(-9.58522062988033,11.2727461682114,
9.89647489275286));
#122686=CARTESIAN_POINT('Ctrl Pts',(-9.63444177812688,11.2759672246033,
9.8792067198233));
#122687=CARTESIAN_POINT('Ctrl Pts',(-9.72630295517816,11.281865198734,9.85367799378828));
#122688=CARTESIAN_POINT('Ctrl Pts',(-9.76853434469116,11.2845348228597,
9.84441241220771));
#122689=CARTESIAN_POINT('Ctrl Pts',(-9.81114930150156,11.2872494929995,
9.83748958018577));
#122690=CARTESIAN_POINT('Origin',(-10.,2.67563288526385,11.));
#122691=CARTESIAN_POINT('',(-9.81114930150145,11.8854636688711,9.83748958018579));
#122692=CARTESIAN_POINT('',(-9.81114930150157,11.7871268320303,9.83748958018577));
#122693=CARTESIAN_POINT('',(-9.81114930150157,2.67563288526385,9.83748958018577));
#122694=CARTESIAN_POINT('Ctrl Pts',(-9.81114930150134,11.8854636688711,
9.83748958018581));
#122695=CARTESIAN_POINT('Ctrl Pts',(-9.81028034253745,11.8854036452282,
9.83763074322788));
#122696=CARTESIAN_POINT('Ctrl Pts',(-9.80941153764504,11.8853436757721,
9.83777288125349));
#122697=CARTESIAN_POINT('Ctrl Pts',(-9.8051592648706,11.8850503775531,9.83847345699382));
#122698=CARTESIAN_POINT('Ctrl Pts',(-9.80177808428253,11.8848178402371,
9.83904569658545));
#122699=CARTESIAN_POINT('Ctrl Pts',(-9.79431956583179,11.8843063002129,
9.84034152911374));
#122700=CARTESIAN_POINT('Ctrl Pts',(-9.7902434079324,11.8840276693685,9.84107188166586));
#122701=CARTESIAN_POINT('Ctrl Pts',(-9.77584363062652,11.8830463778862,
9.8437304479553));
#122702=CARTESIAN_POINT('Ctrl Pts',(-9.76554167624368,11.8823498413611,
9.84577529568974));
#122703=CARTESIAN_POINT('Ctrl Pts',(-9.68979036946538,11.8772595760648,
9.86186738544853));
#122704=CARTESIAN_POINT('Ctrl Pts',(-9.62560862157251,11.8731161131964,
9.88133590927951));
#122705=CARTESIAN_POINT('Ctrl Pts',(-9.4895706949893,11.8640534254544,9.9356317142924));
#122706=CARTESIAN_POINT('Ctrl Pts',(-9.41890224580094,11.8591486421966,
9.97250712471857));
#122707=CARTESIAN_POINT('Ctrl Pts',(-9.33740316682762,11.8528193148595,
10.0261484995713));
#122708=CARTESIAN_POINT('Ctrl Pts',(-9.32254677400131,11.8516363426646,
10.0364241709241));
#122709=CARTESIAN_POINT('Ctrl Pts',(-9.30138719889297,11.8499051317427,
10.0517908114712));
#122710=CARTESIAN_POINT('Ctrl Pts',(-9.29489053862493,11.8493670766408,
10.0566118756708));
#122711=CARTESIAN_POINT('Ctrl Pts',(-9.28357883487237,11.8484184213404,
10.0651882243561));
#122712=CARTESIAN_POINT('Ctrl Pts',(-9.27874231461894,11.8480089413352,
10.0689147780067));
#122713=CARTESIAN_POINT('Ctrl Pts',(-9.26874756454997,11.8471545321851,
10.0767403694604));
#122714=CARTESIAN_POINT('Ctrl Pts',(-9.26359432985219,11.8467093763934,
10.0808454125286));
#122715=CARTESIAN_POINT('Ctrl Pts',(-9.2502838525281,11.8455472845629,10.091632263477));
#122716=CARTESIAN_POINT('Ctrl Pts',(-9.24218157301851,11.844827717133,10.0983806425474));
#122717=CARTESIAN_POINT('Ctrl Pts',(-9.20826274022853,11.8417623484875,
10.1274118051074));
#122718=CARTESIAN_POINT('Ctrl Pts',(-9.18333211589294,11.8393761168736,
10.1506995763677));
#122719=CARTESIAN_POINT('Ctrl Pts',(-9.10395718997506,11.8313155425491,
10.2315740540055));
#122720=CARTESIAN_POINT('Ctrl Pts',(-9.05431675740454,11.8254727493145,
10.2935640824585));
#122721=CARTESIAN_POINT('Ctrl Pts',(-9.00960631724414,11.8194516363058,
10.3626422498798));
#122722=CARTESIAN_POINT('Ctrl Pts',(-9.0079429460058,11.8192263878441,10.3652344131719));
#122723=CARTESIAN_POINT('Ctrl Pts',(-8.98893583222473,11.8166383092667,
10.3951119076177));
#122724=CARTESIAN_POINT('Ctrl Pts',(-8.97271134679763,11.8142918187697,
10.4230956290713));
#122725=CARTESIAN_POINT('Ctrl Pts',(-8.95193045769536,11.8111141827451,
10.4626019474309));
#122726=CARTESIAN_POINT('Ctrl Pts',(-8.94637355575669,11.8102450593589,
10.4735802296974));
#122727=CARTESIAN_POINT('Ctrl Pts',(-8.93700799218333,11.8087478526672,
10.4928256271242));
#122728=CARTESIAN_POINT('Ctrl Pts',(-8.93312130133838,11.8081160065524,
10.5010534015022));
#122729=CARTESIAN_POINT('Ctrl Pts',(-8.9275223659849,11.8071907708689,10.5132704891912));
#122730=CARTESIAN_POINT('Ctrl Pts',(-8.92573629903351,11.8068932463396,
10.5172253171035));
#122731=CARTESIAN_POINT('Ctrl Pts',(-8.9225940982975,11.8063656524613,10.5242867730151));
#122732=CARTESIAN_POINT('Ctrl Pts',(-8.92122947480075,11.8061350877485,
10.5273894771897));
#122733=CARTESIAN_POINT('Ctrl Pts',(-8.9182668239128,11.8056313511507,10.5342052625401));
#122734=CARTESIAN_POINT('Ctrl Pts',(-8.91667450368135,11.8053585181383,
10.5379207081678));
#122735=CARTESIAN_POINT('Ctrl Pts',(-8.91222132012836,11.8045892987304,
10.548461110488));
#122736=CARTESIAN_POINT('Ctrl Pts',(-8.90940554724136,11.8040954903982,
10.5553050802943));
#122737=CARTESIAN_POINT('Ctrl Pts',(-8.89046314763234,11.8007181830896,
10.6026084688807));
#122738=CARTESIAN_POINT('Ctrl Pts',(-8.87652527228846,11.7979477180871,
10.64391364079));
#122739=CARTESIAN_POINT('Ctrl Pts',(-8.8597009490363,11.7939973870626,10.7047134290204));
#122740=CARTESIAN_POINT('Ctrl Pts',(-8.8549635257435,11.7927843266876,10.7236531378988));
#122741=CARTESIAN_POINT('Ctrl Pts',(-8.8397277432039,11.7884620453546,10.7917085209231));
#122742=CARTESIAN_POINT('Ctrl Pts',(-8.83190244486421,11.7853733852593,
10.8413651900117));
#122743=CARTESIAN_POINT('Ctrl Pts',(-8.82277260143998,11.7791679894831,
10.9399267378273));
#122744=CARTESIAN_POINT('Ctrl Pts',(-8.82129526246719,11.7760606716317,
10.9887115453498));
#122745=CARTESIAN_POINT('Ctrl Pts',(-8.82320581161219,11.7721145824843,
11.0487753805916));
#122746=CARTESIAN_POINT('Ctrl Pts',(-8.82372985148856,11.7713653725679,
11.0601009375571));
#122747=CARTESIAN_POINT('Ctrl Pts',(-8.82482722149161,11.7701613985238,
11.0781645903157));
#122748=CARTESIAN_POINT('Ctrl Pts',(-8.82529522992912,11.7697098916066,
11.084908553678));
#122749=CARTESIAN_POINT('Ctrl Pts',(-8.82629281142983,11.7688502316105,
11.0976894001496));
#122750=CARTESIAN_POINT('Ctrl Pts',(-8.82681097183119,11.7684424452403,
11.1037269744835));
#122751=CARTESIAN_POINT('Ctrl Pts',(-8.82809702725269,11.7675104766752,
11.1174665635128));
#122752=CARTESIAN_POINT('Ctrl Pts',(-8.82889429644162,11.7669854001541,
11.1251654793574));
#122753=CARTESIAN_POINT('Ctrl Pts',(-8.83158762091886,11.76535831786,11.1488890628285));
#122754=CARTESIAN_POINT('Ctrl Pts',(-8.83373709420384,11.7642485422381,
11.1648824748614));
#122755=CARTESIAN_POINT('Ctrl Pts',(-8.84679718553935,11.7583452385116,
11.2489364556803));
#122756=CARTESIAN_POINT('Ctrl Pts',(-8.86333697585634,11.7533794604482,
11.3159753838638));
#122757=CARTESIAN_POINT('Ctrl Pts',(-8.90524442624838,11.7439043163671,
11.4384917550157));
#122758=CARTESIAN_POINT('Ctrl Pts',(-8.92924369472445,11.7394290007836,
11.4942126197188));
#122759=CARTESIAN_POINT('Ctrl Pts',(-8.96566871418012,11.7337950029776,
11.5635317501745));
#122760=CARTESIAN_POINT('Ctrl Pts',(-8.9742673410289,11.7325308236331,11.5790352517634));
#122761=CARTESIAN_POINT('Ctrl Pts',(-8.98925894164514,11.7304392497548,
11.6046826502418));
#122762=CARTESIAN_POINT('Ctrl Pts',(-8.99546253674041,11.7296032292092,
11.6149334167827));
#122763=CARTESIAN_POINT('Ctrl Pts',(-9.00439207257219,11.7284420684382,
11.6291926335334));
#122764=CARTESIAN_POINT('Ctrl Pts',(-9.00698772801648,11.7281093320967,
11.6332812526857));
#122765=CARTESIAN_POINT('Ctrl Pts',(-9.01147697085825,11.7275421408303,
11.6402571384975));
#122766=CARTESIAN_POINT('Ctrl Pts',(-9.01335815202916,11.7273069002274,
11.6431522740763));
#122767=CARTESIAN_POINT('Ctrl Pts',(-9.01731338322248,11.7268174085978,
11.6491811739911));
#122768=CARTESIAN_POINT('Ctrl Pts',(-9.01938972912648,11.7265633102804,
11.6523133304703));
#122769=CARTESIAN_POINT('Ctrl Pts',(-9.0249865416234,11.7258858470152,11.6606689757945));
#122770=CARTESIAN_POINT('Ctrl Pts',(-9.02853404065055,11.7254642190908,
11.6658743378164));
#122771=CARTESIAN_POINT('Ctrl Pts',(-9.04476545377029,11.7235686142606,
11.6892853821426));
#122772=CARTESIAN_POINT('Ctrl Pts',(-9.05792142102435,11.7221230874706,
11.7071601500283));
#122773=CARTESIAN_POINT('Ctrl Pts',(-9.08501927550016,11.7192958439277,
11.7418778447711));
#122774=CARTESIAN_POINT('Ctrl Pts',(-9.09894033775112,11.7179140488507,
11.758725272201));
#122775=CARTESIAN_POINT('Ctrl Pts',(-9.15150426656147,11.7129066822172,
11.8188499664151));
#122776=CARTESIAN_POINT('Ctrl Pts',(-9.19286110719524,11.7093554758552,
11.8596437846266));
#122777=CARTESIAN_POINT('Ctrl Pts',(-9.28317543329782,11.7019802131619,
11.9364414023846));
#122778=CARTESIAN_POINT('Ctrl Pts',(-9.33224345092774,11.6981607195572,
11.972038963412));
#122779=CARTESIAN_POINT('Ctrl Pts',(-9.39411452647769,11.6934021673654,
12.0100215886035));
#122780=CARTESIAN_POINT('Ctrl Pts',(-9.40449948119461,11.6926055214441,
12.0161790841453));
#122781=CARTESIAN_POINT('Ctrl Pts',(-9.42104261215629,11.6913387120742,
12.025647234455));
#122782=CARTESIAN_POINT('Ctrl Pts',(-9.42713893860623,11.6908723525591,
12.0290646759476));
#122783=CARTESIAN_POINT('Ctrl Pts',(-9.43855173667663,11.689999979859,12.0353295508228));
#122784=CARTESIAN_POINT('Ctrl Pts',(-9.44386038758146,11.6895944707809,
12.0381908111614));
#122785=CARTESIAN_POINT('Ctrl Pts',(-9.45573075577258,11.6886882183188,
12.0444715405973));
#122786=CARTESIAN_POINT('Ctrl Pts',(-9.46230314780352,11.6881867685885,
12.047870173327));
#122787=CARTESIAN_POINT('Ctrl Pts',(-9.48174513550563,11.6867041131371,
12.0576926989053));
#122788=CARTESIAN_POINT('Ctrl Pts',(-9.49470049620781,11.6857170053869,
12.0639428225465));
#122789=CARTESIAN_POINT('Ctrl Pts',(-9.59853530514978,11.677809068555,12.1117121355898));
#122790=CARTESIAN_POINT('Ctrl Pts',(-9.69423296583647,11.6704904530913,
12.1417426824959));
#122791=CARTESIAN_POINT('Ctrl Pts',(-9.84835908816711,11.6590120022976,
12.1693224725322));
#122792=CARTESIAN_POINT('Ctrl Pts',(-9.90482820035644,11.654880916073,12.1752675551682));
#122793=CARTESIAN_POINT('Ctrl Pts',(-9.96840185063562,11.6504484221341,
12.1773462305951));
#122794=CARTESIAN_POINT('Ctrl Pts',(-9.97529421870459,11.6499707885057,
12.1775110274237));
#122795=CARTESIAN_POINT('Ctrl Pts',(-9.98648217224949,11.6492006250307,
12.1776802521799));
#122796=CARTESIAN_POINT('Ctrl Pts',(-9.9907769170129,11.6489062118566,12.1777217176579));
#122797=CARTESIAN_POINT('Ctrl Pts',(-9.99845886655501,11.6483819139084,
12.1777538619372));
#122798=CARTESIAN_POINT('Ctrl Pts',(-10.0018458942518,11.6481515597413,
12.1777534240991));
#122799=CARTESIAN_POINT('Ctrl Pts',(-10.0093110125854,11.6476456463955,
12.1777202545384));
#122800=CARTESIAN_POINT('Ctrl Pts',(-10.013388966867,11.6473704478051,12.1776809541314));
#122801=CARTESIAN_POINT('Ctrl Pts',(-10.0252549566938,11.6465728558468,
12.1775049553073));
#122802=CARTESIAN_POINT('Ctrl Pts',(-10.0330421209843,11.6460534129845,
12.1773121756059));
#122803=CARTESIAN_POINT('Ctrl Pts',(-10.0508847032444,11.6448711830845,
12.1766932852275));
#122804=CARTESIAN_POINT('Ctrl Pts',(-10.060937839997,11.6442108710305,12.1762155138652));
#122805=CARTESIAN_POINT('Ctrl Pts',(-10.1801453303351,11.6364368577523,
12.1690176931791));
#122806=CARTESIAN_POINT('Ctrl Pts',(-10.2878685893985,11.6299235233656,
12.1472544420701));
#122807=CARTESIAN_POINT('Ctrl Pts',(-10.4309949411495,11.6203661613851,
12.0968735333952));
#122808=CARTESIAN_POINT('Ctrl Pts',(-10.470146632485,11.6176560439965,12.0806709661132));
#122809=CARTESIAN_POINT('Ctrl Pts',(-10.5185255479391,11.6141339782369,
12.0575225114229));
#122810=CARTESIAN_POINT('Ctrl Pts',(-10.5286419979848,11.6133876161545,
12.0525018905266));
#122811=CARTESIAN_POINT('Ctrl Pts',(-10.5446875665734,11.6121871408178,
12.0442490549877));
#122812=CARTESIAN_POINT('Ctrl Pts',(-10.5506639616384,11.6117362510378,
12.0411099039856));
#122813=CARTESIAN_POINT('Ctrl Pts',(-10.5619549162205,11.6108770728547,
12.0350548190162));
#122814=CARTESIAN_POINT('Ctrl Pts',(-10.5672746121441,11.610469145213,12.0321488837836));
#122815=CARTESIAN_POINT('Ctrl Pts',(-10.5793500626143,11.6095358801171,
12.0254310003598));
#122816=CARTESIAN_POINT('Ctrl Pts',(-10.5860910056058,11.6090096390513,
12.021593147842));
#122817=CARTESIAN_POINT('Ctrl Pts',(-10.6068139275105,11.6073752272377,
12.0095222590645));
#122818=CARTESIAN_POINT('Ctrl Pts',(-10.6206635399159,11.6062591849552,
12.0010669602879));
#122819=CARTESIAN_POINT('Ctrl Pts',(-10.6525152694905,11.6036352530459,
11.9807061458023));
#122820=CARTESIAN_POINT('Ctrl Pts',(-10.6703731332381,11.6021200593224,
11.9685868483809));
#122821=CARTESIAN_POINT('Ctrl Pts',(-10.735326987072,11.5964423902016,11.9218487286979));
#122822=CARTESIAN_POINT('Ctrl Pts',(-10.7801553403127,11.5921827378486,
11.884232529541));
#122823=CARTESIAN_POINT('Ctrl Pts',(-10.871635127332,11.5828120529406,11.7950788411472));
#122824=CARTESIAN_POINT('Ctrl Pts',(-10.9169056414725,11.5777062882203,
11.7424176065636));
#122825=CARTESIAN_POINT('Ctrl Pts',(-10.963342348769,11.5721128936166,11.6776243170531));
#122826=CARTESIAN_POINT('Ctrl Pts',(-10.9692879906955,11.5713891086367,
11.6690919260951));
#122827=CARTESIAN_POINT('Ctrl Pts',(-10.9776599766469,11.570360057979,11.6567317145132));
#122828=CARTESIAN_POINT('Ctrl Pts',(-10.9801782665281,11.5700491872053,
11.6529671831796));
#122829=CARTESIAN_POINT('Ctrl Pts',(-10.9845582736125,11.5695062670896,
11.6463371749579));
#122830=CARTESIAN_POINT('Ctrl Pts',(-10.9864293288907,11.5692736168557,
11.6434779857766));
#122831=CARTESIAN_POINT('Ctrl Pts',(-10.9903915232622,11.5687794313835,
11.6373653969942));
#122832=CARTESIAN_POINT('Ctrl Pts',(-10.9924791038739,11.568518124435,11.6341098075936));
#122833=CARTESIAN_POINT('Ctrl Pts',(-10.9981922777561,11.5678002278441,
11.6251027609012));
#122834=CARTESIAN_POINT('Ctrl Pts',(-11.0017842334639,11.5673457520091,
11.6193299928529));
#122835=CARTESIAN_POINT('Ctrl Pts',(-11.0223236699117,11.5647266329988,
11.5856740071272));
#122836=CARTESIAN_POINT('Ctrl Pts',(-11.038158195742,11.5626253912577,11.5571245088472));
#122837=CARTESIAN_POINT('Ctrl Pts',(-11.074280868677,11.5575229601613,11.4850922935149));
#122838=CARTESIAN_POINT('Ctrl Pts',(-11.093137695031,11.5545658575668,11.4409584619326));
#122839=CARTESIAN_POINT('Ctrl Pts',(-11.1343591547775,11.5469774721492,
11.325431796728));
#122840=CARTESIAN_POINT('Ctrl Pts',(-11.1527112385436,11.5423407892761,
11.2528469091625));
#122841=CARTESIAN_POINT('Ctrl Pts',(-11.1665110259867,11.5364322625477,
11.1631134822439));
#122842=CARTESIAN_POINT('Ctrl Pts',(-11.1686305574301,11.5353759422225,
11.1471616854395));
#122843=CARTESIAN_POINT('Ctrl Pts',(-11.1712836518244,11.5337971340684,
11.1234886472789));
#122844=CARTESIAN_POINT('Ctrl Pts',(-11.1720690548649,11.5332824315019,
11.1157970850563));
#122845=CARTESIAN_POINT('Ctrl Pts',(-11.1733347591155,11.5323601798707,
11.1020652482584));
#122846=CARTESIAN_POINT('Ctrl Pts',(-11.1738442881375,11.5319535508573,
11.096027895525));
#122847=CARTESIAN_POINT('Ctrl Pts',(-11.1748240914353,11.5310898135671,
11.083241710955));
#122848=CARTESIAN_POINT('Ctrl Pts',(-11.175282843281,11.5306323638384,11.0764922431001));
#122849=CARTESIAN_POINT('Ctrl Pts',(-11.1763560799771,11.5294018839892,
11.0583993417979));
#122850=CARTESIAN_POINT('Ctrl Pts',(-11.1768646212295,11.5286256201298,
11.047050586153));
#122851=CARTESIAN_POINT('Ctrl Pts',(-11.1786985582833,11.5244637888941,
10.9865706553073));
#122852=CARTESIAN_POINT('Ctrl Pts',(-11.1771115125317,11.5209899416152,
10.9374063274741));
#122853=CARTESIAN_POINT('Ctrl Pts',(-11.1677298832601,11.5138452869112,
10.8387639577073));
#122854=CARTESIAN_POINT('Ctrl Pts',(-11.1598420688603,11.5101792909591,
10.7893914178048));
#122855=CARTESIAN_POINT('Ctrl Pts',(-11.1441481672073,11.5049495662789,
10.7198661592634));
#122856=CARTESIAN_POINT('Ctrl Pts',(-11.1388872966125,11.5033861636991,
10.6991914999717));
#122857=CARTESIAN_POINT('Ctrl Pts',(-11.1217262736686,11.4988016062291,
10.638678472675));
#122858=CARTESIAN_POINT('Ctrl Pts',(-11.1082740554659,11.4958071327588,
10.5993100265784));
#122859=CARTESIAN_POINT('Ctrl Pts',(-11.0902436760273,11.4924397732825,
10.5544559066076));
#122860=CARTESIAN_POINT('Ctrl Pts',(-11.0876668533149,11.4919713084939,
10.5482017775917));
#122861=CARTESIAN_POINT('Ctrl Pts',(-11.0833810922463,11.4912129467006,
10.538049154046));
#122862=CARTESIAN_POINT('Ctrl Pts',(-11.0817046920236,11.4909212567509,
10.5341372135572));
#122863=CARTESIAN_POINT('Ctrl Pts',(-11.0786567521532,11.4903998034251,
10.5271298965851));
#122864=CARTESIAN_POINT('Ctrl Pts',(-11.0772930410664,11.4901695934959,
10.5240312739366));
#122865=CARTESIAN_POINT('Ctrl Pts',(-11.0742435335754,11.4896615963059,
10.5171824386257));
#122866=CARTESIAN_POINT('Ctrl Pts',(-11.0725514481381,11.4893841896893,
10.5134351437081));
#122867=CARTESIAN_POINT('Ctrl Pts',(-11.067529607272,11.4885736229485,10.5024672653557));
#122868=CARTESIAN_POINT('Ctrl Pts',(-11.0641462356961,11.4880435618061,
10.4952712788427));
#122869=CARTESIAN_POINT('Ctrl Pts',(-11.0561987926366,11.4868333099497,
10.4788033417617));
#122870=CARTESIAN_POINT('Ctrl Pts',(-11.0515849937768,11.4861557642648,
10.4695559756348));
#122871=CARTESIAN_POINT('Ctrl Pts',(-11.0355099155894,11.4838738785624,
10.4383712746884));
#122872=CARTESIAN_POINT('Ctrl Pts',(-11.023478547636,11.4822956212471,10.4167338254846));
#122873=CARTESIAN_POINT('Ctrl Pts',(-10.9837657092893,11.4774184344919,
10.3503317725675));
#122874=CARTESIAN_POINT('Ctrl Pts',(-10.9537608836166,11.4741862626555,
10.3070321714718));
#122875=CARTESIAN_POINT('Ctrl Pts',(-10.8762133085991,11.466478373831,10.2097476904082));
#122876=CARTESIAN_POINT('Ctrl Pts',(-10.8264344633927,11.4619878827328,
10.1578286485053));
#122877=CARTESIAN_POINT('Ctrl Pts',(-10.7630395090095,11.4564857835986,
10.1027740680207));
#122878=CARTESIAN_POINT('Ctrl Pts',(-10.7537122722784,11.4556815352609,
10.0949246120226));
#122879=CARTESIAN_POINT('Ctrl Pts',(-10.7388282493376,11.4544053144119,
10.0827884140839));
#122880=CARTESIAN_POINT('Ctrl Pts',(-10.7333519480492,11.4539372424099,
10.0784039973656));
#122881=CARTESIAN_POINT('Ctrl Pts',(-10.7230970101861,11.4530632880664,
10.0703430069087));
#122882=CARTESIAN_POINT('Ctrl Pts',(-10.718328655482,11.4526579251219,10.0666536809176));
#122883=CARTESIAN_POINT('Ctrl Pts',(-10.707671741214,11.4517540740552,10.058538353549));
#122884=CARTESIAN_POINT('Ctrl Pts',(-10.7017696004514,11.4512548977326,
10.0541306915479));
#122885=CARTESIAN_POINT('Ctrl Pts',(-10.6843533233893,11.4497857477098,
10.0413771255962));
#122886=CARTESIAN_POINT('Ctrl Pts',(-10.6727292639847,11.4488100336609,
10.0331843023129));
#122887=CARTESIAN_POINT('Ctrl Pts',(-10.6013896376719,11.4428482757219,
9.98481247704116));
#122888=CARTESIAN_POINT('Ctrl Pts',(-10.5382523279102,11.4376683850679,
9.94997315892713));
#122889=CARTESIAN_POINT('Ctrl Pts',(-10.3973679283859,11.4264144039185,
9.88829307529733));
#122890=CARTESIAN_POINT('Ctrl Pts',(-10.3191723352072,11.4203438064807,
9.86337145383154));
#122891=CARTESIAN_POINT('Ctrl Pts',(-10.2296669637638,11.4139425911536,
9.84482062648191));
#122892=CARTESIAN_POINT('Ctrl Pts',(-10.2202903317901,11.4132787433372,
9.84299590170522));
#122893=CARTESIAN_POINT('Ctrl Pts',(-10.2065851413353,11.4123192455857,
9.84050148473441));
#122894=CARTESIAN_POINT('Ctrl Pts',(-10.2022736854918,11.4120189541285,
9.83974158687715));
#122895=CARTESIAN_POINT('Ctrl Pts',(-10.1946076552545,11.4114878916562,
9.83843447270111));
#122896=CARTESIAN_POINT('Ctrl Pts',(-10.1912548237236,11.4112566051693,
9.83787771419009));
#122897=CARTESIAN_POINT('Ctrl Pts',(-10.1839891377179,11.4107575435465,
9.8367034986869));
#122898=CARTESIAN_POINT('Ctrl Pts',(-10.1800755451406,11.4104900571378,
9.8360912613264));
#122899=CARTESIAN_POINT('Ctrl Pts',(-10.1690066092292,11.4097370778158,
9.83441681809528));
#122900=CARTESIAN_POINT('Ctrl Pts',(-10.1618443149665,11.4092540512951,
9.83340074915521));
#122901=CARTESIAN_POINT('Ctrl Pts',(-10.1123660199937,11.4059433222284,
9.82684603568829));
#122902=CARTESIAN_POINT('Ctrl Pts',(-10.069780552609,11.4032248161534,9.82354435486669));
#122903=CARTESIAN_POINT('Ctrl Pts',(-9.95477429478815,11.3960138560923,
9.82089685127928));
#122904=CARTESIAN_POINT('Ctrl Pts',(-9.88248499963884,11.3916117101161,
9.82590104197443));
#122905=CARTESIAN_POINT('Ctrl Pts',(-9.81114930150155,11.3870771460943,
9.83748958018577));
#122906=CARTESIAN_POINT('Ctrl Pts',(-9.81114930150156,11.2872494929995,
9.83748958018577));
#122907=CARTESIAN_POINT('Ctrl Pts',(-9.84737765306304,11.2895573217892,
9.83160425702546));
#122908=CARTESIAN_POINT('Ctrl Pts',(-9.88388323073177,11.2918974625956,
9.82741207842403));
#122909=CARTESIAN_POINT('Ctrl Pts',(-9.93648744901483,11.2953294482307,
9.82385526598519));
#122910=CARTESIAN_POINT('Ctrl Pts',(-9.95244618936399,11.2963783388013,
9.82310201164768));
#122911=CARTESIAN_POINT('Ctrl Pts',(-9.97612035696641,11.2979480795901,
9.82246688166452));
#122912=CARTESIAN_POINT('Ctrl Pts',(-9.9838276837551,11.2984612746864,9.82233581458947));
#122913=CARTESIAN_POINT('Ctrl Pts',(-9.99759026902171,11.2993817573054,
9.8222369012787));
#122914=CARTESIAN_POINT('Ctrl Pts',(-10.0036450934907,11.2997881368981,
9.82224007774416));
#122915=CARTESIAN_POINT('Ctrl Pts',(-10.0164745205632,11.3006523282061,
9.82234573991638));
#122916=CARTESIAN_POINT('Ctrl Pts',(-10.0232487790928,11.3011104886817,
9.82245999767215));
#122917=CARTESIAN_POINT('Ctrl Pts',(-10.0414303567718,11.3023452979655,
9.82292360764631));
#122918=CARTESIAN_POINT('Ctrl Pts',(-10.0528339655797,11.3031252216827,
9.82338032308687));
#122919=CARTESIAN_POINT('Ctrl Pts',(-10.1142520899508,11.3073564423581,
9.82673476292573));
#122920=CARTESIAN_POINT('Ctrl Pts',(-10.1640431863648,11.3108996521448,
9.83265537772922));
#122921=CARTESIAN_POINT('Ctrl Pts',(-10.2617303421977,11.3180671460305,
9.85064484445307));
#122922=CARTESIAN_POINT('Ctrl Pts',(-10.309550676165,11.3216819135494,9.86259157721101));
#122923=CARTESIAN_POINT('Ctrl Pts',(-10.3785054858079,11.3269902754965,
9.88448993357294));
#122924=CARTESIAN_POINT('Ctrl Pts',(-10.4003207728054,11.3286838311987,
9.89213158164503));
#122925=CARTESIAN_POINT('Ctrl Pts',(-10.4588805260113,11.3332499026083,
9.91460015488255));
#122926=CARTESIAN_POINT('Ctrl Pts',(-10.4951283317902,11.3360985983244,
9.93064843363919));
#122927=CARTESIAN_POINT('Ctrl Pts',(-10.5370345252153,11.3393671864089,
9.95179080266278));
#122928=CARTESIAN_POINT('Ctrl Pts',(-10.5435366569285,11.339873580824,9.95514761234966));
#122929=CARTESIAN_POINT('Ctrl Pts',(-10.5535647013223,11.3406529234632,
9.96044366727162));
#122930=CARTESIAN_POINT('Ctrl Pts',(-10.5571125371895,11.3409283238183,
9.96234067749375));
#122931=CARTESIAN_POINT('Ctrl Pts',(-10.5636320683037,11.3414337067903,
9.96586971446952));
#122932=CARTESIAN_POINT('Ctrl Pts',(-10.5666064507902,11.3416639967443,
9.96749639888724));
#122933=CARTESIAN_POINT('Ctrl Pts',(-10.5733913623308,11.3421887127709,
9.97124520410875));
#122934=CARTESIAN_POINT('Ctrl Pts',(-10.5771971655063,11.3424826121209,
9.97337566845887));
#122935=CARTESIAN_POINT('Ctrl Pts',(-10.5890099645021,11.3433937960387,
9.98007485245793));
#122936=CARTESIAN_POINT('Ctrl Pts',(-10.5969754435782,11.3440067080817,
9.98471660235024));
#122937=CARTESIAN_POINT('Ctrl Pts',(-10.6156245664929,11.3454401073032,
9.99587944344701));
#122938=CARTESIAN_POINT('Ctrl Pts',(-10.6262605592423,11.3462563659961,
10.0024783522059));
#122939=CARTESIAN_POINT('Ctrl Pts',(-10.6647318611005,11.3492119686065,
10.0272051036391));
#122940=CARTESIAN_POINT('Ctrl Pts',(-10.6919037488671,11.3513057926237,
10.0463397482413));
#122941=CARTESIAN_POINT('Ctrl Pts',(-10.7793868342499,11.3581939011251,
10.1136560958946));
#122942=CARTESIAN_POINT('Ctrl Pts',(-10.8357674185423,11.3628914289487,
10.166608049354));
#122943=CARTESIAN_POINT('Ctrl Pts',(-10.9110578605448,11.3701295113591,
10.2527028130505));
#122944=CARTESIAN_POINT('Ctrl Pts',(-10.9342085710923,11.3725206633456,
10.2818541695447));
#122945=CARTESIAN_POINT('Ctrl Pts',(-10.9623187454,11.3756835687085,10.3209146080355));
#122946=CARTESIAN_POINT('Ctrl Pts',(-10.968574328312,11.3764057774505,10.3298671066322));
#122947=CARTESIAN_POINT('Ctrl Pts',(-10.9784476832123,11.3775765091303,
10.3444241715335));
#122948=CARTESIAN_POINT('Ctrl Pts',(-10.9821440160531,11.3780220883544,
10.3499748741026));
#122949=CARTESIAN_POINT('Ctrl Pts',(-10.989119077439,11.3788771761367,10.3606444938674));
#122950=CARTESIAN_POINT('Ctrl Pts',(-10.9924057139585,11.379286375225,10.365758004305));
#122951=CARTESIAN_POINT('Ctrl Pts',(-10.9998761760139,11.3802312349034,
10.3775811565477));
#122952=CARTESIAN_POINT('Ctrl Pts',(-11.0040322698802,11.3807678829423,
10.3843078855408));
#122953=CARTESIAN_POINT('Ctrl Pts',(-11.0169328871182,11.3824692034622,
10.4056658370025));
#122954=CARTESIAN_POINT('Ctrl Pts',(-11.025427352653,11.3836427088733,10.4204447514974));
#122955=CARTESIAN_POINT('Ctrl Pts',(-11.0446332872541,11.3864272842217,
10.4556046635634));
#122956=CARTESIAN_POINT('Ctrl Pts',(-11.0550734578732,11.3880469536531,
10.4761251440827));
#122957=CARTESIAN_POINT('Ctrl Pts',(-11.1158941464383,11.3981747865419,
10.6048730140338));
#122958=CARTESIAN_POINT('Ctrl Pts',(-11.1501694862814,11.4071725039487,
10.7199125012477));
#122959=CARTESIAN_POINT('Ctrl Pts',(-11.1685549326109,11.4166392397871,
10.8524113895528));
#122960=CARTESIAN_POINT('Ctrl Pts',(-11.17027458303,11.4176497058772,10.8667315675298));
#122961=CARTESIAN_POINT('Ctrl Pts',(-11.172272172983,11.4190180611896,10.8864141054624));
#122962=CARTESIAN_POINT('Ctrl Pts',(-11.1727770738069,11.4193870614828,
10.8917514854352));
#122963=CARTESIAN_POINT('Ctrl Pts',(-11.173525067366,11.4199731503686,10.9002793186423));
#122964=CARTESIAN_POINT('Ctrl Pts',(-11.1737916281222,11.4201914906954,
10.903467557794));
#122965=CARTESIAN_POINT('Ctrl Pts',(-11.1743238849418,11.4206482720651,
10.9101621448309));
#122966=CARTESIAN_POINT('Ctrl Pts',(-11.1745868751823,11.4208865525349,
10.9136686608159));
#122967=CARTESIAN_POINT('Ctrl Pts',(-11.1751990015863,11.4214742877395,
10.9223515302462));
#122968=CARTESIAN_POINT('Ctrl Pts',(-11.1755296520104,11.4218227402786,
10.9275291926398));
#122969=CARTESIAN_POINT('Ctrl Pts',(-11.1766441184479,11.423126302074,10.947003097274));
#122970=CARTESIAN_POINT('Ctrl Pts',(-11.1772014760199,11.4240699014457,
10.961311721003));
#122971=CARTESIAN_POINT('Ctrl Pts',(-11.1779669827714,11.4264803765638,
10.9982956403654));
#122972=CARTESIAN_POINT('Ctrl Pts',(-11.1777815345476,11.4279308704364,
11.0209738158883));
#122973=CARTESIAN_POINT('Ctrl Pts',(-11.1739088223258,11.4345415591004,
11.1254330503157));
#122974=CARTESIAN_POINT('Ctrl Pts',(-11.1623569097417,11.4394997797624,
11.2066954818918));
#122975=CARTESIAN_POINT('Ctrl Pts',(-11.1310138725775,11.4475945646869,
11.3318534979501));
#122976=CARTESIAN_POINT('Ctrl Pts',(-11.1168213836361,11.450601323583,11.3768664737534));
#122977=CARTESIAN_POINT('Ctrl Pts',(-11.0958245075684,11.4544571393744,
11.4317386765184));
#122978=CARTESIAN_POINT('Ctrl Pts',(-11.0915189657757,11.4552234156293,
11.4425109805742));
#122979=CARTESIAN_POINT('Ctrl Pts',(-11.0844322685834,11.4564482734834,
11.4595086216701));
#122980=CARTESIAN_POINT('Ctrl Pts',(-11.0817548970428,11.456903391947,11.4657766181));
#122981=CARTESIAN_POINT('Ctrl Pts',(-11.0768418599362,11.4577252592851,
11.4770076492949));
#122982=CARTESIAN_POINT('Ctrl Pts',(-11.074625890852,11.4580913354805,11.4819791300507));
#122983=CARTESIAN_POINT('Ctrl Pts',(-11.0693381116814,11.4589542879358,
11.4936243911195));
#122984=CARTESIAN_POINT('Ctrl Pts',(-11.0662381873348,11.4594521073703,
11.500285078974));
#122985=CARTESIAN_POINT('Ctrl Pts',(-11.056994662952,11.4609136362439,11.5196700796031));
#122986=CARTESIAN_POINT('Ctrl Pts',(-11.0506843346093,11.4618829974824,
11.5323129794422));
#122987=CARTESIAN_POINT('Ctrl Pts',(-11.0358012395096,11.4641078965645,
11.5608354666634));
#122988=CARTESIAN_POINT('Ctrl Pts',(-11.0270880674437,11.4653680292247,
11.5766373816398));
#122989=CARTESIAN_POINT('Ctrl Pts',(-10.9962096752762,11.4696962733487,
11.6297156994075));
#122990=CARTESIAN_POINT('Ctrl Pts',(-10.9723521561183,11.4728178054089,
11.6659626106579));
#122991=CARTESIAN_POINT('Ctrl Pts',(-10.9101071357254,11.4804393990128,
11.7500343470243));
#122992=CARTESIAN_POINT('Ctrl Pts',(-10.8698777641322,11.4849685248226,
11.7963410656411));
#122993=CARTESIAN_POINT('Ctrl Pts',(-10.8012883862133,11.4919522840426,
11.8638616262008));
#122994=CARTESIAN_POINT('Ctrl Pts',(-10.7752621139751,11.4944592893511,
11.8872931541492));
#122995=CARTESIAN_POINT('Ctrl Pts',(-10.7427274959838,11.4973913356088,
11.9140578015892));
#122996=CARTESIAN_POINT('Ctrl Pts',(-10.7371856497686,11.4978840667946,
11.9185331360155));
#122997=CARTESIAN_POINT('Ctrl Pts',(-10.7284847002826,11.4986468612334,
11.925430138526));
#122998=CARTESIAN_POINT('Ctrl Pts',(-10.7253534586762,11.4989192205252,
11.9278864483328));
#122999=CARTESIAN_POINT('Ctrl Pts',(-10.7195279406223,11.4994218692902,
11.9324087792665));
#123000=CARTESIAN_POINT('Ctrl Pts',(-10.7168371780232,11.4996524391839,
11.9344790257941));
#123001=CARTESIAN_POINT('Ctrl Pts',(-10.7106213271886,11.5001814461097,
11.93921879393));
#123002=CARTESIAN_POINT('Ctrl Pts',(-10.7070901203066,11.5004793219339,
11.9418801287149));
#123003=CARTESIAN_POINT('Ctrl Pts',(-10.6958939667679,11.5014157359894,
11.9502197857745));
#123004=CARTESIAN_POINT('Ctrl Pts',(-10.6881747505092,11.5020495482404,
11.9558250787929));
#123005=CARTESIAN_POINT('Ctrl Pts',(-10.6474206251142,11.5053395038155,
11.9846689086053));
#123006=CARTESIAN_POINT('Ctrl Pts',(-10.6132712003313,11.5079055495045,
12.006292926449));
#123007=CARTESIAN_POINT('Ctrl Pts',(-10.4948425329033,11.5164166735068,
12.0730107881803));
#123008=CARTESIAN_POINT('Ctrl Pts',(-10.4062185334783,11.5221906341204,
12.1095980781174));
#123009=CARTESIAN_POINT('Ctrl Pts',(-10.2887057980497,11.5300029672657,
12.1421212301156));
#123010=CARTESIAN_POINT('Ctrl Pts',(-10.2630358667609,11.5317160423217,
12.1483047982117));
#123011=CARTESIAN_POINT('Ctrl Pts',(-10.2277561606616,11.534090457461,12.1555582123499));
#123012=CARTESIAN_POINT('Ctrl Pts',(-10.2183078612519,11.5347282606841,
12.157380369424));
#123013=CARTESIAN_POINT('Ctrl Pts',(-10.2031777601195,11.535753128282,12.1601064368247));
#123014=CARTESIAN_POINT('Ctrl Pts',(-10.1975096900724,11.5361378501152,
12.1610848665412));
#123015=CARTESIAN_POINT('Ctrl Pts',(-10.1857971963802,11.5369345662467,
12.1630184478343));
#123016=CARTESIAN_POINT('Ctrl Pts',(-10.179752052067,11.5373467199077,12.1639680861339));
#123017=CARTESIAN_POINT('Ctrl Pts',(-10.1656010048259,11.5383138699707,
12.1660782220364));
#123018=CARTESIAN_POINT('Ctrl Pts',(-10.1574899393363,11.5388700112702,
12.1672013647407));
#123019=CARTESIAN_POINT('Ctrl Pts',(-10.1308804302874,11.5407007349562,
12.1706035848899));
#123020=CARTESIAN_POINT('Ctrl Pts',(-10.1123403324389,11.5419861674889,
12.1725280470613));
#123021=CARTESIAN_POINT('Ctrl Pts',(-10.0463734096412,11.5465973844078,
12.1777965410393));
#123022=CARTESIAN_POINT('Ctrl Pts',(-9.99880352294367,11.5499936547528,
12.1787081006965));
#123023=CARTESIAN_POINT('Ctrl Pts',(-9.87540882230567,11.5589582085281,
12.1736027842035));
#123024=CARTESIAN_POINT('Ctrl Pts',(-9.79998893187672,11.5645986856286,
12.1631258146078));
#123025=CARTESIAN_POINT('Ctrl Pts',(-9.69886376144277,11.5720955987445,
12.1389453515556));
#123026=CARTESIAN_POINT('Ctrl Pts',(-9.67186149244443,11.5740888713974,
12.1314614224299));
#123027=CARTESIAN_POINT('Ctrl Pts',(-9.63875764468439,11.5765019656518,
12.121001319763));
#123028=CARTESIAN_POINT('Ctrl Pts',(-9.6323829091429,11.5769652116153,12.1189270208291));
#123029=CARTESIAN_POINT('Ctrl Pts',(-9.62234252296618,11.5776921852624,
12.1155648714268));
#123030=CARTESIAN_POINT('Ctrl Pts',(-9.61866505518231,11.5779578867409,
12.1143131576352));
#123031=CARTESIAN_POINT('Ctrl Pts',(-9.61176952407692,11.578454945639,12.1119279651843));
#123032=CARTESIAN_POINT('Ctrl Pts',(-9.60855020269497,11.5786865231849,
12.1107987030642));
#123033=CARTESIAN_POINT('Ctrl Pts',(-9.6010260105442,11.5792266930345,12.1081226201327));
#123034=CARTESIAN_POINT('Ctrl Pts',(-9.59672518649246,11.5795346370998,
12.1065646894959));
#123035=CARTESIAN_POINT('Ctrl Pts',(-9.58269378679182,11.5805369654304,
12.1013892834332));
#123036=CARTESIAN_POINT('Ctrl Pts',(-9.57300162682791,11.5812256337594,
12.0976680903849));
#123037=CARTESIAN_POINT('Ctrl Pts',(-9.5184848746513,11.5850851702012,12.0759056065092));
#123038=CARTESIAN_POINT('Ctrl Pts',(-9.47474970872814,11.5881280663859,
12.0552454188835));
#123039=CARTESIAN_POINT('Ctrl Pts',(-9.35756823855235,11.5964521188397,
11.9907931234771));
#123040=CARTESIAN_POINT('Ctrl Pts',(-9.28743670762614,11.6016514627571,
11.941616979577));
#123041=CARTESIAN_POINT('Ctrl Pts',(-9.20286309537365,11.6088539030606,
11.8674114858105));
#123042=CARTESIAN_POINT('Ctrl Pts',(-9.18311095506994,11.610611865583,11.8488356970984));
#123043=CARTESIAN_POINT('Ctrl Pts',(-9.1571719101485,11.613038909656,11.8226969945064));
#123044=CARTESIAN_POINT('Ctrl Pts',(-9.15041133136488,11.6136830442357,
11.8157135640854));
#123045=CARTESIAN_POINT('Ctrl Pts',(-9.13977623696417,11.6147154896804,
11.8044522583644));
#123046=CARTESIAN_POINT('Ctrl Pts',(-9.1358452959118,11.6151013927654,11.8002280949062));
#123047=CARTESIAN_POINT('Ctrl Pts',(-9.12781650904053,11.6158985999246,
11.7914722656048));
#123048=CARTESIAN_POINT('Ctrl Pts',(-9.12372257469971,11.6163100503583,
11.7869372660002));
#123049=CARTESIAN_POINT('Ctrl Pts',(-9.11426674051005,11.6172721449325,
11.7762974124336));
#123050=CARTESIAN_POINT('Ctrl Pts',(-9.10893241836143,11.6178238982919,
11.7701685781332));
#123051=CARTESIAN_POINT('Ctrl Pts',(-9.0918100279115,11.6196248991335,11.7500799050643));
#123052=CARTESIAN_POINT('Ctrl Pts',(-9.08028379731052,11.6208845143538,
11.7359014412764));
#123053=CARTESIAN_POINT('Ctrl Pts',(-9.02120635476934,11.6276006886583,
11.6596733291351));
#123054=CARTESIAN_POINT('Ctrl Pts',(-8.9795984126393,11.6332786326552,11.5932812812547));
#123055=CARTESIAN_POINT('Ctrl Pts',(-8.91464383613043,11.6440048148759,
11.4623069537105));
#123056=CARTESIAN_POINT('Ctrl Pts',(-8.88974766899018,11.6490145302144,
11.3988322295689));
#123057=CARTESIAN_POINT('Ctrl Pts',(-8.86779844645613,11.6544532113663,
11.3245054614217));
#123058=CARTESIAN_POINT('Ctrl Pts',(-8.8652340559233,11.6551107690279,11.3154210173819));
#123059=CARTESIAN_POINT('Ctrl Pts',(-8.86147720265792,11.6561084296883,
11.301472982271));
#123060=CARTESIAN_POINT('Ctrl Pts',(-8.86020614117336,11.6564525594978,
11.2966312201322));
#123061=CARTESIAN_POINT('Ctrl Pts',(-8.85811213037243,11.6570307266812,
11.2884424265208));
#123062=CARTESIAN_POINT('Ctrl Pts',(-8.8572729420207,11.6572656609644,11.2850996534163));
#123063=CARTESIAN_POINT('Ctrl Pts',(-8.85556675661982,11.6577500551445,
11.2781747583257));
#123064=CARTESIAN_POINT('Ctrl Pts',(-8.85470188250704,11.657999396056,11.2745921843961));
#123065=CARTESIAN_POINT('Ctrl Pts',(-8.85247921495593,11.658650478696,11.2651920007702));
#123066=CARTESIAN_POINT('Ctrl Pts',(-8.85114882102701,11.6590507122057,
11.2593679272472));
#123067=CARTESIAN_POINT('Ctrl Pts',(-8.84529792086333,11.6608614141788,
11.2328257569416));
#123068=CARTESIAN_POINT('Ctrl Pts',(-8.84129283448115,11.6622456486791,
11.2119966110721));
#123069=CARTESIAN_POINT('Ctrl Pts',(-8.83120988733393,11.6662443009451,
11.1506686885803));
#123070=CARTESIAN_POINT('Ctrl Pts',(-8.8266783404924,11.6688025740083,11.1099461855073));
#123071=CARTESIAN_POINT('Ctrl Pts',(-8.81858974836313,11.6773615717492,
10.9722559879378));
#123072=CARTESIAN_POINT('Ctrl Pts',(-8.82488134758213,11.6832828811689,
10.8751236524719));
#123073=CARTESIAN_POINT('Ctrl Pts',(-8.84547627315186,11.6904714295353,
10.766880497118));
#123074=CARTESIAN_POINT('Ctrl Pts',(-8.84816488988286,11.6913399246038,
10.7539398548229));
#123075=CARTESIAN_POINT('Ctrl Pts',(-8.85280171489664,11.6927366039603,
10.7333670216105));
#123076=CARTESIAN_POINT('Ctrl Pts',(-8.85460974623558,11.6932603915929,
10.7257041522808));
#123077=CARTESIAN_POINT('Ctrl Pts',(-8.85795291110962,11.6941938282056,
10.7121447796497));
#123078=CARTESIAN_POINT('Ctrl Pts',(-8.85945724162704,11.6946024867538,
10.7062409234189));
#123079=CARTESIAN_POINT('Ctrl Pts',(-8.86269186422105,11.6954583297614,
10.6939459110035));
#123080=CARTESIAN_POINT('Ctrl Pts',(-8.86443037680246,11.6959057640935,
10.6875571590109));
#123081=CARTESIAN_POINT('Ctrl Pts',(-8.86911936164415,11.6970808974177,
10.6708821589855));
#123082=CARTESIAN_POINT('Ctrl Pts',(-8.87215626215684,11.6978113402741,
10.6606210651866));
#123083=CARTESIAN_POINT('Ctrl Pts',(-8.88710455624572,11.7012701546579,
10.6125317967769));
#123084=CARTESIAN_POINT('Ctrl Pts',(-8.90078065262895,11.7040546783059,
10.5752835335413));
#123085=CARTESIAN_POINT('Ctrl Pts',(-8.95068483610588,11.7131663121917,
10.458022696459));
#123086=CARTESIAN_POINT('Ctrl Pts',(-8.99398468694034,11.7196859427481,
10.3813464724914));
#123087=CARTESIAN_POINT('Ctrl Pts',(-9.06664531773832,11.7286966156065,
10.2807914684039));
#123088=CARTESIAN_POINT('Ctrl Pts',(-9.08924909719492,11.7312988749648,
10.2523736130383));
#123089=CARTESIAN_POINT('Ctrl Pts',(-9.11785583177452,11.7343251456023,
10.21963580256));
#123090=CARTESIAN_POINT('Ctrl Pts',(-9.12262971704901,11.7348218905809,
10.2142723072423));
#123091=CARTESIAN_POINT('Ctrl Pts',(-9.13013404744714,11.7355895498571,
10.205994819601));
#123092=CARTESIAN_POINT('Ctrl Pts',(-9.13283066776027,11.7358628056026,
10.2030505961355));
#123093=CARTESIAN_POINT('Ctrl Pts',(-9.13784696551319,11.7363662498549,
10.1976293105576));
#123094=CARTESIAN_POINT('Ctrl Pts',(-9.14016238147055,11.7365967267529,
10.1951485550823));
#123095=CARTESIAN_POINT('Ctrl Pts',(-9.14550698442549,11.7371244220209,
10.1894716918284));
#123096=CARTESIAN_POINT('Ctrl Pts',(-9.14854340469529,11.7374210896485,
10.1862825306759));
#123097=CARTESIAN_POINT('Ctrl Pts',(-9.15814594165178,11.7383497920389,
10.1763095618233));
#123098=CARTESIAN_POINT('Ctrl Pts',(-9.16477597425506,11.7389772103389,
10.1695874313731));
#123099=CARTESIAN_POINT('Ctrl Pts',(-9.19958163621376,11.742204983061,10.1351369088079));
#123100=CARTESIAN_POINT('Ctrl Pts',(-9.22906223050449,11.7447189675293,
10.1087574198106));
#123101=CARTESIAN_POINT('Ctrl Pts',(-9.33126768899329,11.7529528192789,
10.0261775106796));
#123102=CARTESIAN_POINT('Ctrl Pts',(-9.40922467466743,11.7585083363272,
9.97700540371097));
#123103=CARTESIAN_POINT('Ctrl Pts',(-9.51924025581333,11.7662860210077,
9.92442122786862));
#123104=CARTESIAN_POINT('Ctrl Pts',(-9.54686074132296,11.7682311333758,
9.91249634420751));
#123105=CARTESIAN_POINT('Ctrl Pts',(-9.58431589752778,11.7708757963589,
9.89800017810766));
#123106=CARTESIAN_POINT('Ctrl Pts',(-9.59377235482036,11.7715440415593,
9.89447932158377));
#123107=CARTESIAN_POINT('Ctrl Pts',(-9.60938298536954,11.7726486234302,
9.88889445805193));
#123108=CARTESIAN_POINT('Ctrl Pts',(-9.61551117991129,11.7730826059062,
9.88675900100521));
#123109=CARTESIAN_POINT('Ctrl Pts',(-9.62747493976373,11.7739307019252,
9.88270062628271));
#123110=CARTESIAN_POINT('Ctrl Pts',(-9.6333085304097,11.7743446300591,9.88077250985911));
#123111=CARTESIAN_POINT('Ctrl Pts',(-9.64709703031774,11.7753240626958,
9.87633450959071));
#123112=CARTESIAN_POINT('Ctrl Pts',(-9.65506395787159,11.7758907989115,
9.87386334710656));
#123113=CARTESIAN_POINT('Ctrl Pts',(-9.68178563886909,11.7777948077483,
9.86588504009686));
#123114=CARTESIAN_POINT('Ctrl Pts',(-9.70065026233228,11.7791441691292,
9.86076043892263));
#123115=CARTESIAN_POINT('Ctrl Pts',(-9.74989433953818,11.7826819746355,
9.84869074533714));
#123116=CARTESIAN_POINT('Ctrl Pts',(-9.78042408017642,11.7848906446434,
9.84248091566963));
#123117=CARTESIAN_POINT('Ctrl Pts',(-9.81114930150157,11.7871268320303,
9.83748958018577));
#123118=CARTESIAN_POINT('Origin',(-10.,2.67563288526385,11.));
#123119=CARTESIAN_POINT('',(-9.81114930150157,12.3872370429983,9.83748958018577));
#123120=CARTESIAN_POINT('',(-9.81114930148955,12.2889045666398,9.83748958018772));
#123121=CARTESIAN_POINT('',(-9.81114930150157,2.67563288526385,9.83748958018577));
#123122=CARTESIAN_POINT('Ctrl Pts',(-9.81114930150156,12.3872370429983,
9.83748958018577));
#123123=CARTESIAN_POINT('Ctrl Pts',(-9.76160618676258,12.3836299704724,
9.84553789671247));
#123124=CARTESIAN_POINT('Ctrl Pts',(-9.71259593242639,12.3799506740213,
9.85675028810344));
#123125=CARTESIAN_POINT('Ctrl Pts',(-9.60051589314023,12.3713694093543,
9.89006659515214));
#123126=CARTESIAN_POINT('Ctrl Pts',(-9.5383324439195,12.3664776583828,9.91445648855665));
#123127=CARTESIAN_POINT('Ctrl Pts',(-9.47156323397072,12.3612864710941,
9.9474268553019));
#123128=CARTESIAN_POINT('Ctrl Pts',(-9.46461859660247,12.3607474111369,
9.95094213619925));
#123129=CARTESIAN_POINT('Ctrl Pts',(-9.45409035715892,12.3599320821303,
9.95640317032562));
#123130=CARTESIAN_POINT('Ctrl Pts',(-9.45048132415873,12.3596529347779,
9.95829903176879));
#123131=CARTESIAN_POINT('Ctrl Pts',(-9.44389215466269,12.3591440130093,
9.96180416266418));
#123132=CARTESIAN_POINT('Ctrl Pts',(-9.44090909019244,12.3589138987812,
9.96340755961084));
#123133=CARTESIAN_POINT('Ctrl Pts',(-9.43415813589313,12.3583937505195,
9.9670738176633));
#123134=CARTESIAN_POINT('Ctrl Pts',(-9.43039458061039,12.3581042050758,
9.96914444222949));
#123135=CARTESIAN_POINT('Ctrl Pts',(-9.42061782363,12.3573529379019,9.97459328799913));
#123136=CARTESIAN_POINT('Ctrl Pts',(-9.4146227179992,12.3568931521619,9.9780038774287));
#123137=CARTESIAN_POINT('Ctrl Pts',(-9.35929643656635,12.3526549918194,
10.0101253393834));
#123138=CARTESIAN_POINT('Ctrl Pts',(-9.31207660422203,12.3490731043331,
10.0423382167819));
#123139=CARTESIAN_POINT('Ctrl Pts',(-9.21382384177081,12.3412796944708,
10.120397932985));
#123140=CARTESIAN_POINT('Ctrl Pts',(-9.16408324747363,12.3370940171404,
10.1675244238099));
#123141=CARTESIAN_POINT('Ctrl Pts',(-9.09359345634885,12.3303691242148,
10.2470350989005));
#123142=CARTESIAN_POINT('Ctrl Pts',(-9.06985658776819,12.3279348188222,
10.2765625456223));
#123143=CARTESIAN_POINT('Ctrl Pts',(-9.04137712998696,12.3247502769696,
10.3157130677671));
#123144=CARTESIAN_POINT('Ctrl Pts',(-9.03528482380032,12.3240520331408,
10.3243292003439));
#123145=CARTESIAN_POINT('Ctrl Pts',(-9.02557750442845,12.3229106656835,
10.3384568907643));
#123146=CARTESIAN_POINT('Ctrl Pts',(-9.02189144904224,12.3224702177506,
10.3439191019275));
#123147=CARTESIAN_POINT('Ctrl Pts',(-9.01487952046986,12.321618455429,10.3545002208894));
#123148=CARTESIAN_POINT('Ctrl Pts',(-9.01154721912971,12.3212073970195,
10.3596146303947));
#123149=CARTESIAN_POINT('Ctrl Pts',(-9.00396891372762,12.3202578312103,
10.3714458814049));
#123150=CARTESIAN_POINT('Ctrl Pts',(-8.99975086971297,12.3197183242605,
10.3781801894225));
#123151=CARTESIAN_POINT('Ctrl Pts',(-8.98633682708029,12.3179662054654,
10.400086032539));
#123152=CARTESIAN_POINT('Ctrl Pts',(-8.97741576718902,12.3167438485322,
10.4154221830435));
#123153=CARTESIAN_POINT('Ctrl Pts',(-8.90792220272462,12.3067358560587,
10.5413497053976));
#123154=CARTESIAN_POINT('Ctrl Pts',(-8.8651307789173,12.2972936991391,10.6608064093586));
#123155=CARTESIAN_POINT('Ctrl Pts',(-8.83872097472247,12.2868863269254,
10.8028545894888));
#123156=CARTESIAN_POINT('Ctrl Pts',(-8.83577568455388,12.2855693372387,
10.8210667549098));
#123157=CARTESIAN_POINT('Ctrl Pts',(-8.83157646988353,12.2834004419215,
10.8515624724007));
#123158=CARTESIAN_POINT('Ctrl Pts',(-8.8300856969844,12.282539125307,10.8638096958764));
#123159=CARTESIAN_POINT('Ctrl Pts',(-8.82827216159539,12.281349273821,10.8809498861448));
#123160=CARTESIAN_POINT('Ctrl Pts',(-8.82778714093373,12.281012647343,10.8858243805658));
#123161=CARTESIAN_POINT('Ctrl Pts',(-8.82701126419884,12.2804409248086,
10.894148817342));
#123162=CARTESIAN_POINT('Ctrl Pts',(-8.82670518463172,12.2802050107709,
10.8975972427542));
#123163=CARTESIAN_POINT('Ctrl Pts',(-8.8261004356901,12.2797163121981,10.9047695897608));
#123164=CARTESIAN_POINT('Ctrl Pts',(-8.82580427299882,12.2794636643636,
10.9084936407075));
#123165=CARTESIAN_POINT('Ctrl Pts',(-8.82506383113207,12.2787943266036,
10.9184004641199));
#123166=CARTESIAN_POINT('Ctrl Pts',(-8.82465062681548,12.2783793015423,
10.9245855433403));
#123167=CARTESIAN_POINT('Ctrl Pts',(-8.82304265437537,12.2765582970677,
10.9518947740142));
#123168=CARTESIAN_POINT('Ctrl Pts',(-8.82236831893546,12.2751780967448,
10.9730470419396));
#123169=CARTESIAN_POINT('Ctrl Pts',(-8.82176079990173,12.2672352272143,
11.096568239539));
#123170=CARTESIAN_POINT('Ctrl Pts',(-8.83460347680853,12.2611097242201,
11.1985648931698));
#123171=CARTESIAN_POINT('Ctrl Pts',(-8.86748809725854,12.2529048434168,
11.3244716322836));
#123172=CARTESIAN_POINT('Ctrl Pts',(-8.87544655877457,12.2511365022331,
11.3510618857467));
#123173=CARTESIAN_POINT('Ctrl Pts',(-8.89061932964242,12.2480717700565,
11.3959219253569));
#123174=CARTESIAN_POINT('Ctrl Pts',(-8.89736519180978,12.2467895917852,
11.414338087863));
#123175=CARTESIAN_POINT('Ctrl Pts',(-8.907635585877,12.2449398987945,11.4403462653681));
#123176=CARTESIAN_POINT('Ctrl Pts',(-8.9107863294314,12.2443846683976,11.4480830509423));
#123177=CARTESIAN_POINT('Ctrl Pts',(-8.9163981836012,12.243416063109,11.4614541799711));
#123178=CARTESIAN_POINT('Ctrl Pts',(-8.91882163285402,12.2430039581116,
11.4671040491092));
#123179=CARTESIAN_POINT('Ctrl Pts',(-8.92358150785358,12.2422061301025,
11.4779653839331));
#123180=CARTESIAN_POINT('Ctrl Pts',(-8.92591183119203,12.2418206223042,
11.4831793477809));
#123181=CARTESIAN_POINT('Ctrl Pts',(-8.93217599057848,12.2407974642004,
11.4969257729409));
#123182=CARTESIAN_POINT('Ctrl Pts',(-8.93617409987834,12.2401576483642,
11.5054283176445));
#123183=CARTESIAN_POINT('Ctrl Pts',(-8.95107974154006,12.2378185686096,
11.5361667120886));
#123184=CARTESIAN_POINT('Ctrl Pts',(-8.96258555552996,12.2360990675684,
11.5581035419926));
#123185=CARTESIAN_POINT('Ctrl Pts',(-9.02848478904072,12.2266815042326,
11.6746574360618));
#123186=CARTESIAN_POINT('Ctrl Pts',(-9.09513620131377,12.2185489611787,
11.7617206611963));
#123187=CARTESIAN_POINT('Ctrl Pts',(-9.19654843196857,12.2082290057327,
11.8617856141624));
#123188=CARTESIAN_POINT('Ctrl Pts',(-9.22129259980168,12.2058433375341,
11.8842081768844));
#123189=CARTESIAN_POINT('Ctrl Pts',(-9.25221649396252,12.2030473209367,
11.9099239861014));
#123190=CARTESIAN_POINT('Ctrl Pts',(-9.25751291115199,12.2025746835896,
11.9142509288193));
#123191=CARTESIAN_POINT('Ctrl Pts',(-9.26586999042197,12.2018390284918,
11.9209577715589));
#123192=CARTESIAN_POINT('Ctrl Pts',(-9.26890512099231,12.2015739104187,
11.9233690307438));
#123193=CARTESIAN_POINT('Ctrl Pts',(-9.27463657024989,12.2010772123813,
11.9278764034622));
#123194=CARTESIAN_POINT('Ctrl Pts',(-9.27733009134492,12.2008454184038,
11.929975767847));
#123195=CARTESIAN_POINT('Ctrl Pts',(-9.28360515273213,12.2003091217246,
11.9348229037928));
#123196=CARTESIAN_POINT('Ctrl Pts',(-9.28719340575597,12.2000052274908,
11.937561837704));
#123197=CARTESIAN_POINT('Ctrl Pts',(-9.29903021931046,12.1990114978714,
11.9464897080238));
#123198=CARTESIAN_POINT('Ctrl Pts',(-9.30734459172771,12.198327322217,11.9525911525848));
#123199=CARTESIAN_POINT('Ctrl Pts',(-9.37380488351564,12.1929575165845,
12.0000322548688));
#123200=CARTESIAN_POINT('Ctrl Pts',(-9.43552586671782,12.188558202979,12.0361257586735));
#123201=CARTESIAN_POINT('Ctrl Pts',(-9.55181707138373,12.1806135455869,
12.090634733429));
#123202=CARTESIAN_POINT('Ctrl Pts',(-9.60518201256105,12.1770845328358,
12.1110671480051));
#123203=CARTESIAN_POINT('Ctrl Pts',(-9.68019777018182,12.1720942643174,
12.1336996489631));
#123204=CARTESIAN_POINT('Ctrl Pts',(-9.70074309402364,12.1707251744367,
12.1392952137203));
#123205=CARTESIAN_POINT('Ctrl Pts',(-9.73703147357809,12.168294416076,12.1481291374567));
#123206=CARTESIAN_POINT('Ctrl Pts',(-9.75271045092133,12.1672401363712,
12.1516079197754));
#123207=CARTESIAN_POINT('Ctrl Pts',(-9.77602981215884,12.1656637961893,
12.1562837459332));
#123208=CARTESIAN_POINT('Ctrl Pts',(-9.78361916552548,12.1651494849072,
12.1577279800865));
#123209=CARTESIAN_POINT('Ctrl Pts',(-9.79718422374252,12.1642276684945,
12.1601713340948));
#123210=CARTESIAN_POINT('Ctrl Pts',(-9.80315451783919,12.1638210800972,
12.1611992151948));
#123211=CARTESIAN_POINT('Ctrl Pts',(-9.81581135089552,12.1629571487377,
12.1632778755968));
#123212=CARTESIAN_POINT('Ctrl Pts',(-9.82249952755908,12.1624994621919,
12.1643171618146));
#123213=CARTESIAN_POINT('Ctrl Pts',(-9.84045162724924,12.1612676574012,
12.1669484934057));
#123214=CARTESIAN_POINT('Ctrl Pts',(-9.85173003757058,12.1604902932226,
12.1684350525478));
#123215=CARTESIAN_POINT('Ctrl Pts',(-9.90642727011608,12.1567022851152,
12.1748397929032));
#123216=CARTESIAN_POINT('Ctrl Pts',(-9.95007055226927,12.1536231753417,
12.1775018556463));
#123217=CARTESIAN_POINT('Ctrl Pts',(-10.0822327231451,12.1441324235055,
12.1782024956472));
#123218=CARTESIAN_POINT('Ctrl Pts',(-10.1704703770715,12.1375483179575,
12.1687005907656));
#123219=CARTESIAN_POINT('Ctrl Pts',(-10.277284797482,12.1296352259838,12.1448355623733));
#123220=CARTESIAN_POINT('Ctrl Pts',(-10.2976376480873,12.1281316364459,
12.1397136737628));
#123221=CARTESIAN_POINT('Ctrl Pts',(-10.3308884024165,12.1256929074211,
12.1303943795055));
#123222=CARTESIAN_POINT('Ctrl Pts',(-10.3438695621243,12.1247453572993,
12.1265133605033));
#123223=CARTESIAN_POINT('Ctrl Pts',(-10.3616230051352,12.1234583453713,
12.1208700517526));
#123224=CARTESIAN_POINT('Ctrl Pts',(-10.3664545803885,12.1231090014807,
12.1192997425349));
#123225=CARTESIAN_POINT('Ctrl Pts',(-10.3745933695163,12.1225222540686,
12.1165962070587));
#123226=CARTESIAN_POINT('Ctrl Pts',(-10.3779059390047,12.1222839269008,
12.115479441579));
#123227=CARTESIAN_POINT('Ctrl Pts',(-10.3846886416362,12.1217969972243,
12.1131591084982));
#123228=CARTESIAN_POINT('Ctrl Pts',(-10.3881581871568,12.1215484830556,
12.111954034352));
#123229=CARTESIAN_POINT('Ctrl Pts',(-10.3971993600612,12.1209022231358,
12.1087662979927));
#123230=CARTESIAN_POINT('Ctrl Pts',(-10.4027618763469,12.1205059443577,
12.1067578370105));
#123231=CARTESIAN_POINT('Ctrl Pts',(-10.425717156149,12.1188751709447,12.0982733728524));
#123232=CARTESIAN_POINT('Ctrl Pts',(-10.4429718010844,12.1176603032386,
12.091428226678));
#123233=CARTESIAN_POINT('Ctrl Pts',(-10.5654896064493,12.1090637331105,
12.039439178034));
#123234=CARTESIAN_POINT('Ctrl Pts',(-10.6638393220722,12.1022654180125,
11.9795588689531));
#123235=CARTESIAN_POINT('Ctrl Pts',(-10.7695148938815,12.0935422836262,
11.8918854219308));
#123236=CARTESIAN_POINT('Ctrl Pts',(-10.7866006344376,12.0920823108362,
11.8768535360224));
#123237=CARTESIAN_POINT('Ctrl Pts',(-10.8155959013439,12.0895055517145,
11.849814006072));
#123238=CARTESIAN_POINT('Ctrl Pts',(-10.8277023275361,12.0883974962961,
11.838027045896));
#123239=CARTESIAN_POINT('Ctrl Pts',(-10.8450776886567,12.0867562754594,
11.8203663040466));
#123240=CARTESIAN_POINT('Ctrl Pts',(-10.8505481796238,12.0862318369102,
11.814693170332));
#123241=CARTESIAN_POINT('Ctrl Pts',(-10.8601350855913,12.0852986985181,
11.8045493287245));
#123242=CARTESIAN_POINT('Ctrl Pts',(-10.864274647321,12.0848910018274,11.8001008183075));
#123243=CARTESIAN_POINT('Ctrl Pts',(-10.8728952696353,12.0840317411773,
11.7906918455874));
#123244=CARTESIAN_POINT('Ctrl Pts',(-10.8773688806839,12.0835798866288,
11.7857248821697));
#123245=CARTESIAN_POINT('Ctrl Pts',(-10.889084344015,12.0823805230305,11.7724926200048));
#123246=CARTESIAN_POINT('Ctrl Pts',(-10.8962530700152,12.0816300601922,
11.7641637514572));
#123247=CARTESIAN_POINT('Ctrl Pts',(-10.9282116623612,12.0782071396007,
11.7259647996493));
#123248=CARTESIAN_POINT('Ctrl Pts',(-10.9516295951193,12.0754814110671,
11.6949836738548));
#123249=CARTESIAN_POINT('Ctrl Pts',(-11.0158313995291,12.0673279635601,
11.600703713481));
#123250=CARTESIAN_POINT('Ctrl Pts',(-11.0521269596415,12.0617731517375,
11.5345888625871));
#123251=CARTESIAN_POINT('Ctrl Pts',(-11.0950387527641,12.0538329611891,
11.434852144938));
#123252=CARTESIAN_POINT('Ctrl Pts',(-11.1069082669311,12.0514114164991,
11.4036838342042));
#123253=CARTESIAN_POINT('Ctrl Pts',(-11.1214028844627,12.0481433357976,
11.3601499651524));
#123254=CARTESIAN_POINT('Ctrl Pts',(-11.1251754630735,12.047256740384,11.3481847663827));
#123255=CARTESIAN_POINT('Ctrl Pts',(-11.1313923435413,12.0457325955713,
11.3273098237242));
#123256=CARTESIAN_POINT('Ctrl Pts',(-11.1339242811537,12.045091107214,11.3184275325967));
#123257=CARTESIAN_POINT('Ctrl Pts',(-11.1374987802191,12.0441545540402,
11.3053041816845));
#123258=CARTESIAN_POINT('Ctrl Pts',(-11.1386225913124,12.0438552121324,
11.3010858921274));
#123259=CARTESIAN_POINT('Ctrl Pts',(-11.1405699313925,12.0433277893603,
11.2936095802436));
#123260=CARTESIAN_POINT('Ctrl Pts',(-11.1414029999692,12.0430991829534,
11.2903541744859));
#123261=CARTESIAN_POINT('Ctrl Pts',(-11.1431993802867,12.0425996066937,
11.2832071863056));
#123262=CARTESIAN_POINT('Ctrl Pts',(-11.1441567641818,12.0423289708863,
11.2793142202481));
#123263=CARTESIAN_POINT('Ctrl Pts',(-11.1467897791724,12.0415718925514,
11.268366975604));
#123264=CARTESIAN_POINT('Ctrl Pts',(-11.1484202092392,12.0410879022624,
11.2613018574454));
#123265=CARTESIAN_POINT('Ctrl Pts',(-11.1581805386689,12.0380894738549,
11.2171505273887));
#123266=CARTESIAN_POINT('Ctrl Pts',(-11.1645792960949,12.035660472511,11.1797003268119));
#123267=CARTESIAN_POINT('Ctrl Pts',(-11.177616044113,12.0288564643399,11.0723641484136));
#123268=CARTESIAN_POINT('Ctrl Pts',(-11.1798357227347,12.0245834694337,
11.0021078021566));
#123269=CARTESIAN_POINT('Ctrl Pts',(-11.1726904199467,12.0168441277723,
10.8784315146374));
#123270=CARTESIAN_POINT('Ctrl Pts',(-11.1659252744894,12.0134341036479,
10.8250746186215));
#123271=CARTESIAN_POINT('Ctrl Pts',(-11.1532996379893,12.0091470098148,
10.7609817329291));
#123272=CARTESIAN_POINT('Ctrl Pts',(-11.1508881132562,12.0083803117057,
10.7496276331002));
#123273=CARTESIAN_POINT('Ctrl Pts',(-11.1467942107791,12.0071548529186,
10.7316632848213));
#123274=CARTESIAN_POINT('Ctrl Pts',(-11.1452215037937,12.0066995598358,
10.7250286223171));
#123275=CARTESIAN_POINT('Ctrl Pts',(-11.1421448934489,12.0058368513597,
10.7125339983493));
#123276=CARTESIAN_POINT('Ctrl Pts',(-11.1406532704289,12.0054298386628,
10.7066712184983));
#123277=CARTESIAN_POINT('Ctrl Pts',(-11.1371752440153,12.0045053693404,
10.6934287515461));
#123278=CARTESIAN_POINT('Ctrl Pts',(-11.1351620615146,12.0039870723721,
10.6860564456525));
#123279=CARTESIAN_POINT('Ctrl Pts',(-11.1288156789064,12.0024022516808,
10.6636753666599));
#123280=CARTESIAN_POINT('Ctrl Pts',(-11.1242556373257,12.0013285313511,
10.6487332675562));
#123281=CARTESIAN_POINT('Ctrl Pts',(-11.0921914514131,11.9941764058379,
10.550696223028));
#123282=CARTESIAN_POINT('Ctrl Pts',(-11.0557988317536,11.9878047673149,
10.4708124694543));
#123283=CARTESIAN_POINT('Ctrl Pts',(-10.9868933004128,11.9779490414106,
10.3555413842839));
#123284=CARTESIAN_POINT('Ctrl Pts',(-10.9605065471821,11.9745153010447,
10.3168360781675));
#123285=CARTESIAN_POINT('Ctrl Pts',(-10.9178430745701,11.9695162311914,
10.2616325709469));
#123286=CARTESIAN_POINT('Ctrl Pts',(-10.9032714747041,11.9678914882944,
10.2438762132457));
#123287=CARTESIAN_POINT('Ctrl Pts',(-10.8841609560181,11.9658730698953,
10.2219305396354));
#123288=CARTESIAN_POINT('Ctrl Pts',(-10.8800968795151,11.9654499477349,
10.2173364911799));
#123289=CARTESIAN_POINT('Ctrl Pts',(-10.8735096161487,11.9647741656414,
10.2100064170602));
#123290=CARTESIAN_POINT('Ctrl Pts',(-10.871009093925,11.9645199181846,10.207250310715));
#123291=CARTESIAN_POINT('Ctrl Pts',(-10.8661788724575,11.9640332282865,
10.2019768253969));
#123292=CARTESIAN_POINT('Ctrl Pts',(-10.8638511952463,11.9638006523242,
10.1994577218648));
#123293=CARTESIAN_POINT('Ctrl Pts',(-10.8586873093338,11.9632889094237,
10.1939179102763));
#123294=CARTESIAN_POINT('Ctrl Pts',(-10.8558460696825,11.9630101154695,
10.1909018991006));
#123295=CARTESIAN_POINT('Ctrl Pts',(-10.8457366470507,11.9620276252861,
10.1802834593454));
#123296=CARTESIAN_POINT('Ctrl Pts',(-10.8383823525459,11.9613300728391,
10.1727631941769));
#123297=CARTESIAN_POINT('Ctrl Pts',(-10.7842260796503,11.9563073169715,
10.1188489312276));
#123298=CARTESIAN_POINT('Ctrl Pts',(-10.7336978726762,11.95222440841,10.0763509967901));
#123299=CARTESIAN_POINT('Ctrl Pts',(-10.6492435429015,11.945824342893,10.0166460731715));
#123300=CARTESIAN_POINT('Ctrl Pts',(-10.6175972558304,11.9435091201759,
9.99646840346917));
#123301=CARTESIAN_POINT('Ctrl Pts',(-10.538634092459,11.9378242182725,9.95127329475322));
#123302=CARTESIAN_POINT('Ctrl Pts',(-10.490475817117,11.9344296907177,9.92790541937281));
#123303=CARTESIAN_POINT('Ctrl Pts',(-10.4301495466326,11.9301600496171,
9.90355079556771));
#123304=CARTESIAN_POINT('Ctrl Pts',(-10.4193351523102,11.9293941806119,
9.89936949668968));
#123305=CARTESIAN_POINT('Ctrl Pts',(-10.40206841981,11.9281697435367,9.89298486817855));
#123306=CARTESIAN_POINT('Ctrl Pts',(-10.3956554613296,11.9277146330197,
9.89067666168918));
#123307=CARTESIAN_POINT('Ctrl Pts',(-10.3835129428983,11.9268520805812,
9.8864249074562));
#123308=CARTESIAN_POINT('Ctrl Pts',(-10.3777877166424,11.9264450396826,
9.88446958673505));
#123309=CARTESIAN_POINT('Ctrl Pts',(-10.3647928012099,11.9255202463072,
9.88014298057294));
#123310=CARTESIAN_POINT('Ctrl Pts',(-10.3575146327765,11.925001651077,9.87779822921384));
#123311=CARTESIAN_POINT('Ctrl Pts',(-10.335277688365,11.9234149678473,9.87087260369048));
#123312=CARTESIAN_POINT('Ctrl Pts',(-10.320250533029,11.9223396582804,9.86651891909287));
#123313=CARTESIAN_POINT('Ctrl Pts',(-10.2209285725711,11.9152090249127,
9.83987595763394));
#123314=CARTESIAN_POINT('Ctrl Pts',(-10.1344820533132,11.9088630166077,
9.82671127663411));
#123315=CARTESIAN_POINT('Ctrl Pts',(-10.0004037138852,11.8990152681782,
9.82131154142789));
#123316=CARTESIAN_POINT('Ctrl Pts',(-9.9533405998498,11.8955643517526,9.82223515717757));
#123317=CARTESIAN_POINT('Ctrl Pts',(-9.88350163733715,11.8905439357649,
9.82779973108206));
#123318=CARTESIAN_POINT('Ctrl Pts',(-9.86060333633592,11.8889145105641,
9.83030171476413));
#123319=CARTESIAN_POINT('Ctrl Pts',(-9.83171100865946,11.8868911932928,
9.83431927009611));
#123320=CARTESIAN_POINT('Ctrl Pts',(-9.82563714228905,11.8864676858942,
9.83521231693964));
#123321=CARTESIAN_POINT('Ctrl Pts',(-9.81676178105942,11.8858518067123,
9.83658825199385));
#123322=CARTESIAN_POINT('Ctrl Pts',(-9.81395473831848,11.8856574553958,
9.83703383484927));
#123323=CARTESIAN_POINT('Ctrl Pts',(-9.81114930150134,11.8854636688711,
9.83748958018581));
#123324=CARTESIAN_POINT('',(-11.1777499019438,11.9246914705086,10.999519405199));
#123325=CARTESIAN_POINT('Ctrl Pts',(-9.81114930150157,11.7871268320303,
9.83748958018577));
#123326=CARTESIAN_POINT('Ctrl Pts',(-9.84265146749419,11.7894195655962,
9.83237202945201));
#123327=CARTESIAN_POINT('Ctrl Pts',(-9.87435912257571,11.7917412401712,
9.82853536515747));
#123328=CARTESIAN_POINT('Ctrl Pts',(-9.98527968920542,11.7998816896544,
9.81967259576722));
#123329=CARTESIAN_POINT('Ctrl Pts',(-10.0648050142063,11.8057649315899,
9.82136040255806));
#123330=CARTESIAN_POINT('Ctrl Pts',(-10.1550366002715,11.8121633871668,
9.83244168935296));
#123331=CARTESIAN_POINT('Ctrl Pts',(-10.1664921428589,11.8129702070396,
9.83402009134467));
#123332=CARTESIAN_POINT('Ctrl Pts',(-10.1823104429231,11.8140750097516,
9.8364375121008));
#123333=CARTESIAN_POINT('Ctrl Pts',(-10.1866940499209,11.8143801839975,
9.8371328131946));
#123334=CARTESIAN_POINT('Ctrl Pts',(-10.1942212173553,11.8149023794814,
9.83837038784229));
#123335=CARTESIAN_POINT('Ctrl Pts',(-10.1973666585246,11.8151200449309,
9.83890067615568));
#123336=CARTESIAN_POINT('Ctrl Pts',(-10.2039846100336,11.815576798188,9.84004406334225));
#123337=CARTESIAN_POINT('Ctrl Pts',(-10.2074565894794,11.8158157171866,
9.84065998940724));
#123338=CARTESIAN_POINT('Ctrl Pts',(-10.2160776666166,11.816407319433,9.84222932935155));
#123339=CARTESIAN_POINT('Ctrl Pts',(-10.2212233495161,11.8167589708983,
9.84320152316361));
#123340=CARTESIAN_POINT('Ctrl Pts',(-10.2407621989008,11.8180892745941,
9.84702821761173));
#123341=CARTESIAN_POINT('Ctrl Pts',(-10.2551087502112,11.819055798924,9.85011742292053));
#123342=CARTESIAN_POINT('Ctrl Pts',(-10.3756227967875,11.8271166942065,
9.87843412671235));
#123343=CARTESIAN_POINT('Ctrl Pts',(-10.4778785581854,11.8336170388484,
9.9180383766846));
#123344=CARTESIAN_POINT('Ctrl Pts',(-10.6105288401802,11.8431785937721,
9.99194600455481));
#123345=CARTESIAN_POINT('Ctrl Pts',(-10.6466680962014,11.8459105610676,
10.0147395834394));
#123346=CARTESIAN_POINT('Ctrl Pts',(-10.6907264483452,11.8494578862955,
10.0459977160656));
#123347=CARTESIAN_POINT('Ctrl Pts',(-10.6998700224752,11.8502064793528,
10.052685204765));
#123348=CARTESIAN_POINT('Ctrl Pts',(-10.7143112199105,11.8514096152484,
10.0635705047728));
#123349=CARTESIAN_POINT('Ctrl Pts',(-10.7196717830395,11.8518609075647,
10.0676839377596));
#123350=CARTESIAN_POINT('Ctrl Pts',(-10.7295537597395,11.8527017723064,
10.0754028911907));
#123351=CARTESIAN_POINT('Ctrl Pts',(-10.7340846082483,11.8530908519899,
10.0789960435164));
#123352=CARTESIAN_POINT('Ctrl Pts',(-10.7387516881056,11.8534953766363,
10.0827535502482));
#123353=CARTESIAN_POINT('Ctrl Pts',(-10.7389145973676,11.8535095017477,
10.0828847814707));
#123354=CARTESIAN_POINT('Ctrl Pts',(-10.7392304080557,11.8535368934708,
10.0831393208946));
#123355=CARTESIAN_POINT('Ctrl Pts',(-10.7393833136292,11.8535501598788,
10.08326262397));
#123356=CARTESIAN_POINT('Ctrl Pts',(-10.7396804447232,11.853575947763,10.0835023532217));
#123357=CARTESIAN_POINT('Ctrl Pts',(-10.7398246736243,11.853588469072,10.0836187752072));
#123358=CARTESIAN_POINT('Ctrl Pts',(-10.7401055694787,11.85361286249,10.0838456246905));
#123359=CARTESIAN_POINT('Ctrl Pts',(-10.7402422392278,11.8536247344621,
10.0839560487427));
#123360=CARTESIAN_POINT('Ctrl Pts',(-10.7405089669717,11.853647910642,10.0841716534674));
#123361=CARTESIAN_POINT('Ctrl Pts',(-10.7406390272939,11.8536592147363,
10.0842768312819));
#123362=CARTESIAN_POINT('Ctrl Pts',(-10.740893350656,11.8536813250315,10.0844825883626));
#123363=CARTESIAN_POINT('Ctrl Pts',(-10.7410176156344,11.8536921311366,
10.0845831652318));
#123364=CARTESIAN_POINT('Ctrl Pts',(-10.7468050480192,11.8541955373455,
10.0892693144007));
#123365=CARTESIAN_POINT('Ctrl Pts',(-10.7524254437942,11.8546902167318,
10.0939072294525));
#123366=CARTESIAN_POINT('Ctrl Pts',(-10.7645657177112,11.8557716403079,
10.1041161538132));
#123367=CARTESIAN_POINT('Ctrl Pts',(-10.7710684716705,11.8563591590664,
10.1097067854797));
#123368=CARTESIAN_POINT('Ctrl Pts',(-10.7883004863567,11.8579386431096,
10.1248521241998));
#123369=CARTESIAN_POINT('Ctrl Pts',(-10.7989166558257,11.8589356570113,
10.1345327231335));
#123370=CARTESIAN_POINT('Ctrl Pts',(-10.8315936402043,11.8620813772571,
10.1654436068719));
#123371=CARTESIAN_POINT('Ctrl Pts',(-10.8530040435193,11.8642562988166,
10.1873400525553));
#123372=CARTESIAN_POINT('Ctrl Pts',(-10.9086430416007,11.8702228956226,
10.2488658358855));
#123373=CARTESIAN_POINT('Ctrl Pts',(-10.9411211754113,11.8740622688413,
10.2899824195799));
#123374=CARTESIAN_POINT('Ctrl Pts',(-11.004141723145,11.8822292665767,10.3817192587976));
#123375=CARTESIAN_POINT('Ctrl Pts',(-11.0338349729055,11.8865463788711,
10.4327625850547));
#123376=CARTESIAN_POINT('Ctrl Pts',(-11.0641677695136,11.8914240980274,
10.4952700153881));
#123377=CARTESIAN_POINT('Ctrl Pts',(-11.0686272091642,11.8921555920061,
10.5047815574599));
#123378=CARTESIAN_POINT('Ctrl Pts',(-11.0746948828354,11.893170360402,10.5181870764257));
#123379=CARTESIAN_POINT('Ctrl Pts',(-11.0764102427971,11.8934595379611,
10.5220316170766));
#123380=CARTESIAN_POINT('Ctrl Pts',(-11.0794918679213,11.8939831633869,
10.5290390263095));
#123381=CARTESIAN_POINT('Ctrl Pts',(-11.0808649384155,11.8942180087875,
10.5321988480658));
#123382=CARTESIAN_POINT('Ctrl Pts',(-11.0836789956021,11.894702465733,10.5387533240788));
#123383=CARTESIAN_POINT('Ctrl Pts',(-11.0851179316682,11.894951956546,10.5421487830395));
#123384=CARTESIAN_POINT('Ctrl Pts',(-11.0888499908174,11.8956038766535,
10.5510717535225));
#123385=CARTESIAN_POINT('Ctrl Pts',(-11.0911170114148,11.89600479064,10.5566101668512));
#123386=CARTESIAN_POINT('Ctrl Pts',(-11.1012658035289,11.8978234365716,
10.5819533161184));
#123387=CARTESIAN_POINT('Ctrl Pts',(-11.1086517891863,11.8992146525209,
10.6019538392975));
#123388=CARTESIAN_POINT('Ctrl Pts',(-11.1287388301803,11.9032420952576,
10.6612541955722));
#123389=CARTESIAN_POINT('Ctrl Pts',(-11.1399214754789,11.905821219531,10.7010357803265));
#123390=CARTESIAN_POINT('Ctrl Pts',(-11.1680716632431,11.9137731768417,
10.8260744062333));
#123391=CARTESIAN_POINT('Ctrl Pts',(-11.1777144565469,11.9190828918736,
10.912656599808));
#123392=CARTESIAN_POINT('Ctrl Pts',(-11.1777499019438,11.9246914705086,
10.999519405199));
#123393=CARTESIAN_POINT('Ctrl Pts',(-11.1777498978294,11.9246908261691,
10.9995094259802));
#123394=CARTESIAN_POINT('Ctrl Pts',(-11.177755783503,11.9256221251925,11.0139329102706));
#123395=CARTESIAN_POINT('Ctrl Pts',(-11.1774969546123,11.9265603664752,
11.0283547832212));
#123396=CARTESIAN_POINT('Ctrl Pts',(-11.1765976782018,11.9281847721749,
11.05310294073));
#123397=CARTESIAN_POINT('Ctrl Pts',(-11.1760860245079,11.9288670704794,
11.0634324098018));
#123398=CARTESIAN_POINT('Ctrl Pts',(-11.1750659675478,11.9299483060232,
11.0796894479493));
#123399=CARTESIAN_POINT('Ctrl Pts',(-11.1746485629377,11.9303444502281,
11.085622354684));
#123400=CARTESIAN_POINT('Ctrl Pts',(-11.1737358034003,11.9311292975541,
11.0973288444902));
#123401=CARTESIAN_POINT('Ctrl Pts',(-11.1732427391017,11.9315179193461,
11.1031024405907));
#123402=CARTESIAN_POINT('Ctrl Pts',(-11.1721020706597,11.9323483230663,
11.1153890619231));
#123403=CARTESIAN_POINT('Ctrl Pts',(-11.1714427420018,11.9327904558006,
11.1219007747635));
#123404=CARTESIAN_POINT('Ctrl Pts',(-11.169600899152,11.9339360666646,11.138693526422));
#123405=CARTESIAN_POINT('Ctrl Pts',(-11.1683371110564,11.9346420393839,
11.1489648973813));
#123406=CARTESIAN_POINT('Ctrl Pts',(-11.1625629445594,11.9375732936573,
11.1912848306329));
#123407=CARTESIAN_POINT('Ctrl Pts',(-11.1568682277918,11.9398347315364,
11.2231547514224));
#123408=CARTESIAN_POINT('Ctrl Pts',(-11.1309316339241,11.9483475855106,
11.3402264047285));
#123409=CARTESIAN_POINT('Ctrl Pts',(-11.1025228833957,11.9548253680828,
11.4233203497335));
#123410=CARTESIAN_POINT('Ctrl Pts',(-11.0477701047596,11.9641915610551,
11.5393862919074));
#123411=CARTESIAN_POINT('Ctrl Pts',(-11.0284548957363,11.9671388187079,
11.5753615891282));
#123412=CARTESIAN_POINT('Ctrl Pts',(-11.002342464544,11.9706681875444,11.6184630363119));
#123413=CARTESIAN_POINT('Ctrl Pts',(-10.997275546867,11.9713344153117,11.6266007036261));
#123414=CARTESIAN_POINT('Ctrl Pts',(-10.9897222057876,11.9722998795227,
11.6384078989193));
#123415=CARTESIAN_POINT('Ctrl Pts',(-10.9873136822041,11.972603767704,11.6421264552732));
#123416=CARTESIAN_POINT('Ctrl Pts',(-10.9830388154057,11.9731360928222,
11.6486455694762));
#123417=CARTESIAN_POINT('Ctrl Pts',(-10.9811813821827,11.9733650931529,
11.6514518276092));
#123418=CARTESIAN_POINT('Ctrl Pts',(-10.9771114986351,11.9738618776224,
11.6575438170293));
#123419=CARTESIAN_POINT('Ctrl Pts',(-10.974894483174,11.9741293569372,11.6608263765228));
#123420=CARTESIAN_POINT('Ctrl Pts',(-10.9686911439102,11.9748693177498,
11.6699120052822));
#123421=CARTESIAN_POINT('Ctrl Pts',(-10.9646692060127,11.9753395186303,
11.6756907251419));
#123422=CARTESIAN_POINT('Ctrl Pts',(-10.94105563891,11.9780476849214,11.7089780493033));
#123423=CARTESIAN_POINT('Ctrl Pts',(-10.9203379243412,11.9802182581707,
11.7356725906976));
#123424=CARTESIAN_POINT('Ctrl Pts',(-10.8583184335943,11.986281452752,11.8088553959763));
#123425=CARTESIAN_POINT('Ctrl Pts',(-10.814445961821,11.9900833427241,11.8530158829485));
#123426=CARTESIAN_POINT('Ctrl Pts',(-10.734158915249,11.9966541211329,11.9219615217974));
#123427=CARTESIAN_POINT('Ctrl Pts',(-10.699471781803,11.9993877000918,11.9485468609408));
#123428=CARTESIAN_POINT('Ctrl Pts',(-10.6484148802514,12.0033462675896,
11.9833522724646));
#123429=CARTESIAN_POINT('Ctrl Pts',(-10.6332063257463,12.0045175673697,
11.99321359521));
#123430=CARTESIAN_POINT('Ctrl Pts',(-10.6092298225601,12.0063565016424,
12.0079855489864));
#123431=CARTESIAN_POINT('Ctrl Pts',(-10.6006160131888,12.0070156599234,
12.0131417662491));
#123432=CARTESIAN_POINT('Ctrl Pts',(-10.5860439692757,12.0081289233563,
12.0216134310379));
#123433=CARTESIAN_POINT('Ctrl Pts',(-10.5801208579939,12.0085809297365,
12.0249884503267));
#123434=CARTESIAN_POINT('Ctrl Pts',(-10.5684882613395,12.0094678686641,
12.0314836349629));
#123435=CARTESIAN_POINT('Ctrl Pts',(-10.5627815547245,12.0099026242601,
12.0346082888091));
#123436=CARTESIAN_POINT('Ctrl Pts',(-10.5519870830568,12.0107244620246,
12.0404029671566));
#123437=CARTESIAN_POINT('Ctrl Pts',(-10.5469050796694,12.0111111659204,
12.0430833647204));
#123438=CARTESIAN_POINT('Ctrl Pts',(-10.534942891162,12.0120210122996,12.0492811219235));
#123439=CARTESIAN_POINT('Ctrl Pts',(-10.5280473678224,12.012545188239,12.0527681330866));
#123440=CARTESIAN_POINT('Ctrl Pts',(-10.5067032116947,12.0141670816505,
12.0632992491961));
#123441=CARTESIAN_POINT('Ctrl Pts',(-10.4921448112291,12.0152724994744,
12.0701153576629));
#123442=CARTESIAN_POINT('Ctrl Pts',(-10.4156241274805,12.0210811593774,
12.1040498772558));
#123443=CARTESIAN_POINT('Ctrl Pts',(-10.3515591641075,12.0259497534578,
12.1260874852991));
#123444=CARTESIAN_POINT('Ctrl Pts',(-10.2296581922039,12.0351408608072,
12.1565991328903));
#123445=CARTESIAN_POINT('Ctrl Pts',(-10.1723834217287,12.0394281145099,
12.1665113126214));
#123446=CARTESIAN_POINT('Ctrl Pts',(-10.0946230140934,12.0450699135368,
12.1741145026504));
#123447=CARTESIAN_POINT('Ctrl Pts',(-10.0745876484128,12.0465072395938,
12.17555738105));
#123448=CARTESIAN_POINT('Ctrl Pts',(-10.0414134024463,12.0488507038394,
12.1770948355798));
#123449=CARTESIAN_POINT('Ctrl Pts',(-10.0282927796975,12.0497681473157,
12.177483280649));
#123450=CARTESIAN_POINT('Ctrl Pts',(-10.0101505326263,12.0510213198357,
12.1777169463803));
#123451=CARTESIAN_POINT('Ctrl Pts',(-10.0051328431663,12.0513662872969,
12.1777495044828));
#123452=CARTESIAN_POINT('Ctrl Pts',(-9.99663190605569,12.0519478005035,
12.1777503344473));
#123453=CARTESIAN_POINT('Ctrl Pts',(-9.99314876233222,12.0521852336447,
12.1777352232711));
#123454=CARTESIAN_POINT('Ctrl Pts',(-9.98597419991665,12.0526725168494,
12.1776722664624));
#123455=CARTESIAN_POINT('Ctrl Pts',(-9.9822828707635,12.0529222630283,12.1776225178468));
#123456=CARTESIAN_POINT('Ctrl Pts',(-9.97259087563087,12.0535756159525,
12.1774463151537));
#123457=CARTESIAN_POINT('Ctrl Pts',(-9.96659074260276,12.0539776951973,
12.1772913447698));
#123458=CARTESIAN_POINT('Ctrl Pts',(-9.94126799028439,12.0556654757494,
12.1764435581702));
#123459=CARTESIAN_POINT('Ctrl Pts',(-9.92196159372133,12.0569297979229,
12.1753208092634));
#123460=CARTESIAN_POINT('Ctrl Pts',(-9.78940226119842,12.0655095478397,
12.1643307320265));
#123461=CARTESIAN_POINT('Ctrl Pts',(-9.67806281472448,12.0722618928368,
12.1385866300699));
#123462=CARTESIAN_POINT('Ctrl Pts',(-9.55098066558749,12.0809281388331,
12.0890326041522));
#123463=CARTESIAN_POINT('Ctrl Pts',(-9.5300751057532,12.082384837017,12.0801763161222));
#123464=CARTESIAN_POINT('Ctrl Pts',(-9.49410723281759,12.0849563013698,
12.0636973212264));
#123465=CARTESIAN_POINT('Ctrl Pts',(-9.47892836256622,12.0860623861987,
12.0563445391701));
#123466=CARTESIAN_POINT('Ctrl Pts',(-9.45690205494621,12.0877011519974,
12.0450845356525));
#123467=CARTESIAN_POINT('Ctrl Pts',(-9.449927186539,12.0882251422958,12.0414302470411));
#123468=CARTESIAN_POINT('Ctrl Pts',(-9.43763752884214,12.0891576836301,
12.0348335188372));
#123469=CARTESIAN_POINT('Ctrl Pts',(-9.43230782683142,12.0895652347138,
12.0319193548158));
#123470=CARTESIAN_POINT('Ctrl Pts',(-9.42116035067936,12.0904243917137,
12.0257116624776));
#123471=CARTESIAN_POINT('Ctrl Pts',(-9.41534761603547,12.0908762895932,
12.0224095759113));
#123472=CARTESIAN_POINT('Ctrl Pts',(-9.40004830274959,12.0920762416338,
12.0135452401849));
#123473=CARTESIAN_POINT('Ctrl Pts',(-9.39061116625172,12.0928272560223,
12.0078994136458));
#123474=CARTESIAN_POINT('Ctrl Pts',(-9.34887399634329,12.0961984938383,
11.9821294326415));
#123475=CARTESIAN_POINT('Ctrl Pts',(-9.31748475768185,12.0988697118025,
11.9605809100776));
#123476=CARTESIAN_POINT('Ctrl Pts',(-9.22611556104383,12.1070689614915,
11.8911146442338));
#123477=CARTESIAN_POINT('Ctrl Pts',(-9.16972353488591,12.1127345751575,
11.8388213722552));
#123478=CARTESIAN_POINT('Ctrl Pts',(-9.0970389146401,12.1207435873642,11.756858242238));
#123479=CARTESIAN_POINT('Ctrl Pts',(-9.0762893776164,12.1231276652709,11.7313905178527));
#123480=CARTESIAN_POINT('Ctrl Pts',(-9.04919225619578,12.1263505797081,
11.695135993109));
#123481=CARTESIAN_POINT('Ctrl Pts',(-9.04191202747868,12.127228435146,11.6850670612147));
#123482=CARTESIAN_POINT('Ctrl Pts',(-9.02953933581988,12.1287390804252,
11.6673718546581));
#123483=CARTESIAN_POINT('Ctrl Pts',(-9.02437416920066,12.1293757211598,
11.6597979571697));
#123484=CARTESIAN_POINT('Ctrl Pts',(-9.01688813918409,12.1303065389456,
11.6485407217811));
#123485=CARTESIAN_POINT('Ctrl Pts',(-9.01449856289214,12.1306049217407,
11.644903804967));
#123486=CARTESIAN_POINT('Ctrl Pts',(-9.01045939897434,12.1311113430238,
11.6386813495417));
#123487=CARTESIAN_POINT('Ctrl Pts',(-9.0087996868492,12.1313200341171,11.6361025132408));
#123488=CARTESIAN_POINT('Ctrl Pts',(-9.00505360680032,12.1317924158358,
11.6302316450915));
#123489=CARTESIAN_POINT('Ctrl Pts',(-9.00297348896896,12.1320556997121,
11.6269357137844));
#123490=CARTESIAN_POINT('Ctrl Pts',(-8.99733062128461,12.1327728043524,
11.6178955151367));
#123491=CARTESIAN_POINT('Ctrl Pts',(-8.99380083400843,12.1332245660208,
11.6121307003452));
#123492=CARTESIAN_POINT('Ctrl Pts',(-8.97544608101233,12.1355925424366,
11.5815660900498));
#123493=CARTESIAN_POINT('Ctrl Pts',(-8.96148649992685,12.1374597346795,
11.556255218153));
#123494=CARTESIAN_POINT('Ctrl Pts',(-8.91890851729149,12.1434701021332,
11.4718521116726));
#123495=CARTESIAN_POINT('Ctrl Pts',(-8.89429493792555,12.14748307587,11.4108778434292));
#123496=CARTESIAN_POINT('Ctrl Pts',(-8.86160825660064,12.1543435571037,
11.3052499953245));
#123497=CARTESIAN_POINT('Ctrl Pts',(-8.8507947686932,12.1571521037317,11.2616107710267));
#123498=CARTESIAN_POINT('Ctrl Pts',(-8.83742290097849,12.1617886187591,
11.1904358542441));
#123499=CARTESIAN_POINT('Ctrl Pts',(-8.83329369867413,12.1635725750304,
11.1632407606041));
#123500=CARTESIAN_POINT('Ctrl Pts',(-8.82902616172211,12.1660110556969,
11.1265116242625));
#123501=CARTESIAN_POINT('Ctrl Pts',(-8.82804586633937,12.1666395631766,
11.1170829661049));
#123502=CARTESIAN_POINT('Ctrl Pts',(-8.82659813616777,12.1676957145058,
11.1013093795092));
#123503=CARTESIAN_POINT('Ctrl Pts',(-8.82606809443844,12.1681214070262,
11.0949705366784));
#123504=CARTESIAN_POINT('Ctrl Pts',(-8.82512661032692,12.1689618483157,
11.0824948947301));
#123505=CARTESIAN_POINT('Ctrl Pts',(-8.82471183980364,12.1693764799683,
11.0763585453952));
#123506=CARTESIAN_POINT('Ctrl Pts',(-8.82382487876583,12.1703830435992,
11.0615085022981));
#123507=CARTESIAN_POINT('Ctrl Pts',(-8.82340144064217,12.1709764610019,
11.0527923733429));
#123508=CARTESIAN_POINT('Ctrl Pts',(-8.82231164331672,12.1729669918766,
11.0236901311657));
#123509=CARTESIAN_POINT('Ctrl Pts',(-8.82207803410386,12.1743772326128,
11.0032925061872));
#123510=CARTESIAN_POINT('Ctrl Pts',(-8.82370840560998,12.1822275238111,
10.8910127063675));
#123511=CARTESIAN_POINT('Ctrl Pts',(-8.83579272272953,12.1889767011168,
10.7996103708562));
#123512=CARTESIAN_POINT('Ctrl Pts',(-8.86091117947494,12.1964668745766,
10.7005360134776));
#123513=CARTESIAN_POINT('Ctrl Pts',(-8.86358475794481,12.1972237962367,
10.690544959543));
#123514=CARTESIAN_POINT('Ctrl Pts',(-8.87474132814395,12.200227380788,10.6509494028131));
#123515=CARTESIAN_POINT('Ctrl Pts',(-8.88425296051962,12.2024591397807,
10.621645416623));
#123516=CARTESIAN_POINT('Ctrl Pts',(-8.899026458731,12.2054977715023,10.5815570218364));
#123517=CARTESIAN_POINT('Ctrl Pts',(-8.90331982680242,12.2063395101654,
10.5704305803293));
#123518=CARTESIAN_POINT('Ctrl Pts',(-8.91110486377902,12.2077943255239,
10.5511332648474));
#123519=CARTESIAN_POINT('Ctrl Pts',(-8.91452131498735,12.2084108971433,
10.5429332655042));
#123520=CARTESIAN_POINT('Ctrl Pts',(-8.91972768322518,12.2093181147967,
10.5308249285663));
#123521=CARTESIAN_POINT('Ctrl Pts',(-8.92144665149034,12.209612675519,10.5268866922958));
#123522=CARTESIAN_POINT('Ctrl Pts',(-8.92442681533606,12.2101148382218,
10.5201596581452));
#123523=CARTESIAN_POINT('Ctrl Pts',(-8.9256773693948,12.2103230625142,10.5173662720309));
#123524=CARTESIAN_POINT('Ctrl Pts',(-8.92856047477507,12.2107974460069,
10.51099295887));
#123525=CARTESIAN_POINT('Ctrl Pts',(-8.93020008790359,12.2110631754266,
10.5074163099547));
#123526=CARTESIAN_POINT('Ctrl Pts',(-8.93477403859497,12.2117935932234,
10.4975692683727));
#123527=CARTESIAN_POINT('Ctrl Pts',(-8.93774584242191,12.2122560945969,
10.4913163071968));
#123528=CARTESIAN_POINT('Ctrl Pts',(-8.95455813389338,12.2148087940525,
10.4567315665533));
#123529=CARTESIAN_POINT('Ctrl Pts',(-8.96947822564044,12.216840399407,10.4289356016382));
#123530=CARTESIAN_POINT('Ctrl Pts',(-8.98630223687682,12.2189393077875,
10.40040478847));
#123531=CARTESIAN_POINT('Ctrl Pts',(-8.98710975063993,12.2190396205947,
10.3990416691348));
#123532=CARTESIAN_POINT('Ctrl Pts',(-9.02750329276134,12.2240363217316,
10.3311682669105));
#123533=CARTESIAN_POINT('Ctrl Pts',(-9.07354787411905,12.2287349241803,
10.2687180149885));
#123534=CARTESIAN_POINT('Ctrl Pts',(-9.16026673871962,12.2368331695996,
10.1725610416616));
#123535=CARTESIAN_POINT('Ctrl Pts',(-9.19766711655844,12.240142827333,10.1362476522582));
#123536=CARTESIAN_POINT('Ctrl Pts',(-9.24612314151881,12.2443167639677,
10.095070462418));
#123537=CARTESIAN_POINT('Ctrl Pts',(-9.25501076407317,12.2450778502939,
10.0877397253008));
#123538=CARTESIAN_POINT('Ctrl Pts',(-9.26931178707853,12.2462963285017,
10.0762922443746));
#123539=CARTESIAN_POINT('Ctrl Pts',(-9.27465591979757,12.2467503201409,
10.0720898511411));
#123540=CARTESIAN_POINT('Ctrl Pts',(-9.28482447108847,12.2476118122534,
10.0642352671384));
#123541=CARTESIAN_POINT('Ctrl Pts',(-9.28964125269203,12.2480189212337,
10.0605735152744));
#123542=CARTESIAN_POINT('Ctrl Pts',(-9.30062666834373,12.2489453261507,
10.0523551200946));
#123543=CARTESIAN_POINT('Ctrl Pts',(-9.30681197186335,12.2494654779694,
10.0478213254443));
#123544=CARTESIAN_POINT('Ctrl Pts',(-9.32584927449223,12.2510622804511,
10.0341508878961));
#123545=CARTESIAN_POINT('Ctrl Pts',(-9.33884041434342,12.2521462903062,
10.025211987843));
#123546=CARTESIAN_POINT('Ctrl Pts',(-9.42300176961781,12.2591365574972,
9.96975895831474));
#123547=CARTESIAN_POINT('Ctrl Pts',(-9.49884109879698,12.2653174174141,
9.93081418616209));
#123548=CARTESIAN_POINT('Ctrl Pts',(-9.62349310948899,12.2751148750309,
9.88299886779541));
#123549=CARTESIAN_POINT('Ctrl Pts',(-9.66982461076612,12.2786782176714,
9.86843750990203));
#123550=CARTESIAN_POINT('Ctrl Pts',(-9.73218891383256,12.2832844991724,
9.85299538852081));
#123551=CARTESIAN_POINT('Ctrl Pts',(-9.74752847923379,12.2844024382356,
9.8495216047509));
#123552=CARTESIAN_POINT('Ctrl Pts',(-9.77366965658846,12.2862773438221,
9.84414976543403));
#123553=CARTESIAN_POINT('Ctrl Pts',(-9.78443631302591,12.2870409274326,
9.84209348071059));
#123554=CARTESIAN_POINT('Ctrl Pts',(-9.79983367116159,12.2881192014786,
9.8393750165261));
#123555=CARTESIAN_POINT('Ctrl Pts',(-9.80444166314972,12.2884401526046,
9.83858971495161));
#123556=CARTESIAN_POINT('Ctrl Pts',(-9.80975253265642,12.2888079585808,
9.83771713238524));
#123557=CARTESIAN_POINT('Ctrl Pts',(-9.8104508646595,12.2888562800112,9.83760304177997));
#123558=CARTESIAN_POINT('Ctrl Pts',(-9.81114930147754,12.2889045666398,
9.83748958018968));
#123559=CARTESIAN_POINT('Origin',(-10.,2.67563288526385,11.));
#123560=CARTESIAN_POINT('',(-9.81116440461326,12.8870115174245,9.83777311283111));
#123561=CARTESIAN_POINT('',(-9.81114930150157,12.7872971999427,9.83748958018577));
#123562=CARTESIAN_POINT('',(-9.81114930150157,2.67563288526385,9.83748958018577));
#123563=CARTESIAN_POINT('Ctrl Pts',(-9.81110867807875,12.8871739896041,
9.83749618022011));
#123564=CARTESIAN_POINT('Ctrl Pts',(-9.78406883002272,12.8854478804254,
9.84188979386417));
#123565=CARTESIAN_POINT('Ctrl Pts',(-9.75719191255045,12.8837043151253,
9.84722525463141));
#123566=CARTESIAN_POINT('Ctrl Pts',(-9.71464208644478,12.8808807571287,
9.85722610260996));
#123567=CARTESIAN_POINT('Ctrl Pts',(-9.6988375012299,12.8798178659499,9.86128913730254));
#123568=CARTESIAN_POINT('Ctrl Pts',(-9.67541680943465,12.8782188242581,
9.86783179935482));
#123569=CARTESIAN_POINT('Ctrl Pts',(-9.66773291883104,12.8776903284387,
9.87006298236067));
#123570=CARTESIAN_POINT('Ctrl Pts',(-9.65428623069631,12.876758316912,9.8741165354314));
#123571=CARTESIAN_POINT('Ctrl Pts',(-9.64851355604475,12.8763558722712,
9.87590531380619));
#123572=CARTESIAN_POINT('Ctrl Pts',(-9.63724727043895,12.8755657311629,
9.87949166509802));
#123573=CARTESIAN_POINT('Ctrl Pts',(-9.63175261472048,12.8751781670077,
9.88128541056828));
#123574=CARTESIAN_POINT('Ctrl Pts',(-9.62085616364738,12.8744050867876,
9.88493156132713));
#123575=CARTESIAN_POINT('Ctrl Pts',(-9.61545419425648,12.874019612599,9.88678295338018));
#123576=CARTESIAN_POINT('Ctrl Pts',(-9.60272489802426,12.8731059219586,
9.89124931474804));
#123577=CARTESIAN_POINT('Ctrl Pts',(-9.59540967212191,12.8725766283155,
9.89389772160528));
#123578=CARTESIAN_POINT('Ctrl Pts',(-9.56964082096367,12.8706968345156,
9.9035169128794));
#123579=CARTESIAN_POINT('Ctrl Pts',(-9.55133753045879,12.8693336695691,
9.91087829379931));
#123580=CARTESIAN_POINT('Ctrl Pts',(-9.4936394361986,12.8649439694878,9.93578507714946));
#123581=CARTESIAN_POINT('Ctrl Pts',(-9.45502289944056,12.8618642147492,
9.95503413376984));
#123582=CARTESIAN_POINT('Ctrl Pts',(-9.34485753226269,12.8526743579141,
10.0177175693384));
#123583=CARTESIAN_POINT('Ctrl Pts',(-9.2767791651881,12.8464463114501,10.0667039500517));
#123584=CARTESIAN_POINT('Ctrl Pts',(-9.20219053210713,12.8392573586922,
10.133474468202));
#123585=CARTESIAN_POINT('Ctrl Pts',(-9.1901476222388,12.8380845260397,10.1447189776182));
#123586=CARTESIAN_POINT('Ctrl Pts',(-9.17020981209158,12.8361274115923,
10.1641338556926));
#123587=CARTESIAN_POINT('Ctrl Pts',(-9.16219020899813,12.8353357843607,
10.1721722733547));
#123588=CARTESIAN_POINT('Ctrl Pts',(-9.1509859751738,12.8342250376851,10.183732424297));
#123589=CARTESIAN_POINT('Ctrl Pts',(-9.14770474643366,12.8338991545232,
10.187159073256));
#123590=CARTESIAN_POINT('Ctrl Pts',(-9.14208382321269,12.8333400129505,
10.1931005682813));
#123591=CARTESIAN_POINT('Ctrl Pts',(-9.13973427665814,12.8331060221488,
10.195605976045));
#123592=CARTESIAN_POINT('Ctrl Pts',(-9.13482301230796,12.8326163994766,
10.2008891692449));
#123593=CARTESIAN_POINT('Ctrl Pts',(-9.13226365778701,12.8323609417971,
10.2036690504066));
#123594=CARTESIAN_POINT('Ctrl Pts',(-9.12536779798752,12.8316716507882,
10.2112318126023));
#123595=CARTESIAN_POINT('Ctrl Pts',(-9.12105709168175,12.8312396894337,
10.2160381955358));
#123596=CARTESIAN_POINT('Ctrl Pts',(-9.10074877752226,12.8291981061035,
10.2390597908665));
#123597=CARTESIAN_POINT('Ctrl Pts',(-9.08527534714444,12.8276229199306,
10.2577320123707));
#123598=CARTESIAN_POINT('Ctrl Pts',(-9.02801231419209,12.8216561173945,
10.3313458831917));
#123599=CARTESIAN_POINT('Ctrl Pts',(-8.99050366702705,12.8174403691046,
10.3894452878321));
#123600=CARTESIAN_POINT('Ctrl Pts',(-8.93670766792437,12.8102949624782,
10.4914277525041));
#123601=CARTESIAN_POINT('Ctrl Pts',(-8.91755001937229,12.8074072933221,
10.5335904523836));
#123602=CARTESIAN_POINT('Ctrl Pts',(-8.89418093907903,12.8032480696345,
10.5942768435863));
#123603=CARTESIAN_POINT('Ctrl Pts',(-8.88785833374651,12.8020372321317,
10.6119433909258));
#123604=CARTESIAN_POINT('Ctrl Pts',(-8.87873515882337,12.8001440652263,
10.6394927324995));
#123605=CARTESIAN_POINT('Ctrl Pts',(-8.87563717982932,12.7994709482178,
10.6492742209935));
#123606=CARTESIAN_POINT('Ctrl Pts',(-8.87008619871506,12.798205201327,10.6676306429787));
#123607=CARTESIAN_POINT('Ctrl Pts',(-8.86760202206982,12.7976136034216,
10.6761954290991));
#123608=CARTESIAN_POINT('Ctrl Pts',(-8.86356749968488,12.796608228155,10.6907199562875));
#123609=CARTESIAN_POINT('Ctrl Pts',(-8.86196617240306,12.7961961061597,
10.6966652377317));
#123610=CARTESIAN_POINT('Ctrl Pts',(-8.85886229692574,12.7953702763121,
10.7085596919887));
#123611=CARTESIAN_POINT('Ctrl Pts',(-8.85735947691383,12.7949565917973,
10.7145085937411));
#123612=CARTESIAN_POINT('Ctrl Pts',(-8.85381161860218,12.7939450766861,
10.7290296713489));
#123613=CARTESIAN_POINT('Ctrl Pts',(-8.85181620568938,12.7933456838564,
10.7376134687512));
#123614=CARTESIAN_POINT('Ctrl Pts',(-8.84533941918717,12.7912907079505,
10.7669648761172));
#123615=CARTESIAN_POINT('Ctrl Pts',(-8.8413239538762,12.7898205910628,10.7878299165997));
#123616=CARTESIAN_POINT('Ctrl Pts',(-8.82301373584406,12.7819257423038,
10.8991152661796));
#123617=CARTESIAN_POINT('Ctrl Pts',(-8.81873575341719,12.7751952318128,
10.9908513870907));
#123618=CARTESIAN_POINT('Ctrl Pts',(-8.82580218420936,12.7677644904687,
11.0919287317256));
#123619=CARTESIAN_POINT('Ctrl Pts',(-8.82660909190401,12.7670455778776,
11.1017112713051));
#123620=CARTESIAN_POINT('Ctrl Pts',(-8.83150848004004,12.7632630917765,
11.1532380744841));
#123621=CARTESIAN_POINT('Ctrl Pts',(-8.83770694970566,12.7602288019821,
11.1947560578584));
#123622=CARTESIAN_POINT('Ctrl Pts',(-8.84804808504356,12.7566106430386,
11.2453480428075));
#123623=CARTESIAN_POINT('Ctrl Pts',(-8.85010484295941,12.7559372143641,
11.254813695718));
#123624=CARTESIAN_POINT('Ctrl Pts',(-8.85327184897153,12.7549647920798,
11.2685688394817));
#123625=CARTESIAN_POINT('Ctrl Pts',(-8.8542898249666,12.7546609838712,11.2728788565181));
#123626=CARTESIAN_POINT('Ctrl Pts',(-8.85612129444679,12.7541295406617,
11.2804421754318));
#123627=CARTESIAN_POINT('Ctrl Pts',(-8.85692439301217,12.7539013373118,
11.2836978398858));
#123628=CARTESIAN_POINT('Ctrl Pts',(-8.85870130073373,12.7534067577356,
11.2907711520637));
#123629=CARTESIAN_POINT('Ctrl Pts',(-8.85968036633839,12.7531406813628,
11.2945873691117));
#123630=CARTESIAN_POINT('Ctrl Pts',(-8.86243659423793,12.7524088694713,
11.3051109732266));
#123631=CARTESIAN_POINT('Ctrl Pts',(-8.86425394354386,12.7519453314807,
11.3118078079074));
#123632=CARTESIAN_POINT('Ctrl Pts',(-8.87471855740354,12.7493766430976,
11.3490635061735));
#123633=CARTESIAN_POINT('Ctrl Pts',(-8.88454074511231,12.7473309143182,
11.3792818249036));
#123634=CARTESIAN_POINT('Ctrl Pts',(-8.91767946752626,12.7412864379041,
11.4687515602554));
#123635=CARTESIAN_POINT('Ctrl Pts',(-8.94458787843713,12.7373941136138,
11.5265471321714));
#123636=CARTESIAN_POINT('Ctrl Pts',(-8.9978922417656,12.7306973327199,11.6203483006338));
#123637=CARTESIAN_POINT('Ctrl Pts',(-9.02189624531239,12.7279298144736,
11.6575443469777));
#123638=CARTESIAN_POINT('Ctrl Pts',(-9.05869900724826,12.723925665021,11.7080832733436));
#123639=CARTESIAN_POINT('Ctrl Pts',(-9.06980637550736,12.722744078595,11.7226127930195));
#123640=CARTESIAN_POINT('Ctrl Pts',(-9.09018631039357,12.720617358585,11.7480228922402));
#123641=CARTESIAN_POINT('Ctrl Pts',(-9.09932729003125,12.7196772092936,
11.7590045046177));
#123642=CARTESIAN_POINT('Ctrl Pts',(-9.11349677523994,12.7182386241192,
11.7754106839105));
#123643=CARTESIAN_POINT('Ctrl Pts',(-9.11838054170768,12.7177460313308,
11.7809589123828));
#123644=CARTESIAN_POINT('Ctrl Pts',(-9.12735292660507,12.7168466530045,
11.790960613971));
#123645=CARTESIAN_POINT('Ctrl Pts',(-9.13142425685647,12.716440590624,11.7954293077699));
#123646=CARTESIAN_POINT('Ctrl Pts',(-9.14030393536213,12.7155592116851,
11.8050261829889));
#123647=CARTESIAN_POINT('Ctrl Pts',(-9.14512413407912,12.7150834056182,
11.8101430299815));
#123648=CARTESIAN_POINT('Ctrl Pts',(-9.15843832488758,12.7137760899345,
11.8240254782902));
#123649=CARTESIAN_POINT('Ctrl Pts',(-9.16702303214714,12.7129407275305,
11.8327024640066));
#123650=CARTESIAN_POINT('Ctrl Pts',(-9.22597026455609,12.7072531220207,
11.8904595349904));
#123651=CARTESIAN_POINT('Ctrl Pts',(-9.28049775176035,12.7022133226105,
11.9350687661089));
#123652=CARTESIAN_POINT('Ctrl Pts',(-9.38079887512987,12.6933626049321,
12.0031338172257));
#123653=CARTESIAN_POINT('Ctrl Pts',(-9.42473919570574,12.6896086474711,
12.0289618565023));
#123654=CARTESIAN_POINT('Ctrl Pts',(-9.50503869840875,12.6830707848471,
12.0694058510048));
#123655=CARTESIAN_POINT('Ctrl Pts',(-9.54071801921699,12.680270311077,12.0852079431273));
#123656=CARTESIAN_POINT('Ctrl Pts',(-9.58376087460311,12.6770619886137,
12.1017670779487));
#123657=CARTESIAN_POINT('Ctrl Pts',(-9.5904258092782,12.6765699163905,12.1042620576965));
#123658=CARTESIAN_POINT('Ctrl Pts',(-9.60082143276683,12.6758101553457,
12.1080465277982));
#123659=CARTESIAN_POINT('Ctrl Pts',(-9.604536545226,12.6755401650494,12.109377885747));
#123660=CARTESIAN_POINT('Ctrl Pts',(-9.61147665969136,12.6750387372548,
12.111825670925));
#123661=CARTESIAN_POINT('Ctrl Pts',(-9.6146998235921,12.6748070472628,12.1129467565907));
#123662=CARTESIAN_POINT('Ctrl Pts',(-9.62212289018574,12.6742761320691,
12.1154925458112));
#123663=CARTESIAN_POINT('Ctrl Pts',(-9.62632601298613,12.6739774660465,
12.116907553424));
#123664=CARTESIAN_POINT('Ctrl Pts',(-9.63988607793801,12.6730198803475,
12.1213875195001));
#123665=CARTESIAN_POINT('Ctrl Pts',(-9.64927378385512,12.6723660543991,
12.1243589918728));
#123666=CARTESIAN_POINT('Ctrl Pts',(-9.73424009222725,12.6665209525267,
12.1500854356494));
#123667=CARTESIAN_POINT('Ctrl Pts',(-9.81190144202986,12.6616844429891,
12.165309992578));
#123668=CARTESIAN_POINT('Ctrl Pts',(-9.9645067388448,12.6521978194249,12.1795585383324));
#123669=CARTESIAN_POINT('Ctrl Pts',(-10.0389803970292,12.6475715806278,
12.1794476349033));
#123670=CARTESIAN_POINT('Ctrl Pts',(-10.1271022677888,12.641790889398,12.1709579166111));
#123671=CARTESIAN_POINT('Ctrl Pts',(-10.1412358629588,12.6408547584067,
12.1693373472622));
#123672=CARTESIAN_POINT('Ctrl Pts',(-10.1626409511236,12.6394217093175,
12.1664893004826));
#123673=CARTESIAN_POINT('Ctrl Pts',(-10.1699363157317,12.6389305858136,
12.1654488455468));
#123674=CARTESIAN_POINT('Ctrl Pts',(-10.1831841245349,12.6380335948936,
12.163432429501));
#123675=CARTESIAN_POINT('Ctrl Pts',(-10.1891397928994,12.6376284453887,
12.162479065587));
#123676=CARTESIAN_POINT('Ctrl Pts',(-10.2020092138304,12.636748731592,12.160317455604));
#123677=CARTESIAN_POINT('Ctrl Pts',(-10.2089199825487,12.636273676327,12.1590930754097));
#123678=CARTESIAN_POINT('Ctrl Pts',(-10.227809217088,12.6349677139771,12.1555720561977));
#123679=CARTESIAN_POINT('Ctrl Pts',(-10.2397633177152,12.6341329463958,
12.1531510519288));
#123680=CARTESIAN_POINT('Ctrl Pts',(-10.3221350377745,12.6283214193523,
12.1351325542028));
#123681=CARTESIAN_POINT('Ctrl Pts',(-10.3910154701715,12.6231459202771,
12.1132836192644));
#123682=CARTESIAN_POINT('Ctrl Pts',(-10.5061844216218,12.6140092080635,
12.0647388694548));
#123683=CARTESIAN_POINT('Ctrl Pts',(-10.5534752999921,12.6101061246871,
12.0409402916311));
#123684=CARTESIAN_POINT('Ctrl Pts',(-10.6302833635469,12.6036283621981,
11.9955689279957));
#123685=CARTESIAN_POINT('Ctrl Pts',(-10.6606916634473,12.6010246604386,
11.9756544928696));
#123686=CARTESIAN_POINT('Ctrl Pts',(-10.6957915137623,12.5980119533303,
11.9502725849841));
#123687=CARTESIAN_POINT('Ctrl Pts',(-10.7014132249043,12.5975292135131,
11.9461307046283));
#123688=CARTESIAN_POINT('Ctrl Pts',(-10.7101222787125,12.5967814411074,
11.9395938870652));
#123689=CARTESIAN_POINT('Ctrl Pts',(-10.7132349926306,12.5965141949876,
11.9372332525772));
#123690=CARTESIAN_POINT('Ctrl Pts',(-10.7190391881619,12.5960159873988,
11.932785777303));
#123691=CARTESIAN_POINT('Ctrl Pts',(-10.7217333587641,12.595784790828,11.9307027558118));
#123692=CARTESIAN_POINT('Ctrl Pts',(-10.7279316691233,12.5952529723598,
11.9258673773861));
#123693=CARTESIAN_POINT('Ctrl Pts',(-10.7314292676585,12.5949529278357,
11.9231067887536));
#123694=CARTESIAN_POINT('Ctrl Pts',(-10.7427215690399,12.5939840636808,
11.9140895108106));
#123695=CARTESIAN_POINT('Ctrl Pts',(-10.7504525608679,12.5933205298584,
11.9077532335629));
#123696=CARTESIAN_POINT('Ctrl Pts',(-10.8168158042945,12.5876133517544,
11.8519349026337));
#123697=CARTESIAN_POINT('Ctrl Pts',(-10.8705721164581,12.5829043980112,
11.7969245231313));
#123698=CARTESIAN_POINT('Ctrl Pts',(-10.9614769897654,12.5739180649251,
11.6836307962055));
#123699=CARTESIAN_POINT('Ctrl Pts',(-10.999605153357,12.569664397412,11.6265598352636));
#123700=CARTESIAN_POINT('Ctrl Pts',(-11.0418984916495,12.5639727647234,
11.549472389243));
#123701=CARTESIAN_POINT('Ctrl Pts',(-11.0508185486628,12.5627025572245,
11.5322148829592));
#123702=CARTESIAN_POINT('Ctrl Pts',(-11.0629427979673,12.5608674400674,
11.5072640907305));
#123703=CARTESIAN_POINT('Ctrl Pts',(-11.0664987555512,12.5603145655806,
11.4997445827643));
#123704=CARTESIAN_POINT('Ctrl Pts',(-11.0725393309801,12.5593490475729,
11.486612892755));
#123705=CARTESIAN_POINT('Ctrl Pts',(-11.0750603120424,12.5589376568278,
11.4810177199848));
#123706=CARTESIAN_POINT('Ctrl Pts',(-11.0801576758564,12.5580880373549,
11.4694641580304));
#123707=CARTESIAN_POINT('Ctrl Pts',(-11.082728749645,12.557649646572,11.4635036700718));
#123708=CARTESIAN_POINT('Ctrl Pts',(-11.0891786994473,12.5565240398669,
11.4482042848302));
#123709=CARTESIAN_POINT('Ctrl Pts',(-11.0929867425828,12.5558344881168,
11.4388362903701));
#123710=CARTESIAN_POINT('Ctrl Pts',(-11.1077171039995,12.553063412293,11.401217238985));
#123711=CARTESIAN_POINT('Ctrl Pts',(-11.1176676039105,12.550950501749,11.3726007195488));
#123712=CARTESIAN_POINT('Ctrl Pts',(-11.1532770691595,12.542306526373,11.2558657283896));
#123713=CARTESIAN_POINT('Ctrl Pts',(-11.1696986535704,12.5355104722746,
11.1652758018376));
#123714=CARTESIAN_POINT('Ctrl Pts',(-11.1779106478584,12.5259419186797,
11.0343331401563));
#123715=CARTESIAN_POINT('Ctrl Pts',(-11.178399895203,12.5230946327988,10.9948458127129));
#123716=CARTESIAN_POINT('Ctrl Pts',(-11.1765483314593,12.5196711373701,
10.9459813142326));
#123717=CARTESIAN_POINT('Ctrl Pts',(-11.1760780678809,12.5190158608483,
10.9365619442179));
#123718=CARTESIAN_POINT('Ctrl Pts',(-11.1752225608884,12.5180633386396,
10.9227578478658));
#123719=CARTESIAN_POINT('Ctrl Pts',(-11.1749258202402,12.5177616029668,
10.9183682893257));
#123720=CARTESIAN_POINT('Ctrl Pts',(-11.1743567166375,12.5172295871915,
10.9105971335661));
#123721=CARTESIAN_POINT('Ctrl Pts',(-11.1740943331922,12.5169987760645,
10.9072149354266));
#123722=CARTESIAN_POINT('Ctrl Pts',(-11.1734911804317,12.5164979759127,
10.899852774744));
#123723=CARTESIAN_POINT('Ctrl Pts',(-11.1731447760542,12.5162282974416,
10.8958733805657));
#123724=CARTESIAN_POINT('Ctrl Pts',(-11.1721187025306,12.5154765790728,
10.8847419346606));
#123725=CARTESIAN_POINT('Ctrl Pts',(-11.1713938158466,12.5149969360654,
10.8775940811916));
#123726=CARTESIAN_POINT('Ctrl Pts',(-11.1666061885918,12.5121100609931,
10.8343324279586));
#123727=CARTESIAN_POINT('Ctrl Pts',(-11.1609386913637,12.5097809823345,
10.7984121461238));
#123728=CARTESIAN_POINT('Ctrl Pts',(-11.1310742290487,12.5004343553015,
10.6531619437831));
#123729=CARTESIAN_POINT('Ctrl Pts',(-11.0930159292454,12.4937306902847,
10.5472936672179));
#123730=CARTESIAN_POINT('Ctrl Pts',(-11.0310283513882,12.4851755731495,
10.4303580711809));
#123731=CARTESIAN_POINT('Ctrl Pts',(-11.0210054743986,12.4838426494338,
10.4125826614298));
#123732=CARTESIAN_POINT('Ctrl Pts',(-11.006168568574,12.4819325386807,10.387797532695));
#123733=CARTESIAN_POINT('Ctrl Pts',(-11.0017322669786,12.4813687827273,
10.3805651701695));
#123734=CARTESIAN_POINT('Ctrl Pts',(-10.9939346381446,12.4803900522237,
10.3681558038375));
#123735=CARTESIAN_POINT('Ctrl Pts',(-10.9906099994122,12.4799764218833,
10.3629560613829));
#123736=CARTESIAN_POINT('Ctrl Pts',(-10.9841457227841,12.4791790094774,
10.3530188897202));
#123737=CARTESIAN_POINT('Ctrl Pts',(-10.9810123533457,12.4787954666535,
10.348277573373));
#123738=CARTESIAN_POINT('Ctrl Pts',(-10.9726973661277,12.4777852850294,
10.3358914340319));
#123739=CARTESIAN_POINT('Ctrl Pts',(-10.9674600139073,12.4771565854204,
10.3282846834106));
#123740=CARTESIAN_POINT('Ctrl Pts',(-10.948474968276,12.4749036274125,10.3013934064281));
#123741=CARTESIAN_POINT('Ctrl Pts',(-10.9342365296448,12.4732610391562,
10.2824640038576));
#123742=CARTESIAN_POINT('Ctrl Pts',(-10.8640759169286,12.4653762176606,
10.1948194565096));
#123743=CARTESIAN_POINT('Ctrl Pts',(-10.801094551065,12.4588622807454,10.1321372571497));
#123744=CARTESIAN_POINT('Ctrl Pts',(-10.7261162005275,12.4518530284067,
10.0726914949289));
#123745=CARTESIAN_POINT('Ctrl Pts',(-10.7204945253284,12.4513317459406,
10.0683168776095));
#123746=CARTESIAN_POINT('Ctrl Pts',(-10.6795848309468,12.4475702872252,
10.0370739118507));
#123747=CARTESIAN_POINT('Ctrl Pts',(-10.6428397950433,12.444360791642,10.0121639728208));
#123748=CARTESIAN_POINT('Ctrl Pts',(-10.5969669140284,12.440621295372,9.984712684578));
#123749=CARTESIAN_POINT('Ctrl Pts',(-10.5891061618307,12.4399895537027,
9.98013149278667));
#123750=CARTESIAN_POINT('Ctrl Pts',(-10.5774174254342,12.4390643231345,
9.9734996243037));
#123751=CARTESIAN_POINT('Ctrl Pts',(-10.5736301422479,12.4387667046716,
9.97137841461988));
#123752=CARTESIAN_POINT('Ctrl Pts',(-10.5668634667379,12.4382389180998,
9.96763748059245));
#123753=CARTESIAN_POINT('Ctrl Pts',(-10.5638887156563,12.438008254587,9.96600963315684));
#123754=CARTESIAN_POINT('Ctrl Pts',(-10.5573507053667,12.4375042816974,
9.96246850181343));
#123755=CARTESIAN_POINT('Ctrl Pts',(-10.5537845939901,12.4372313115131,
9.96056070731184));
#123756=CARTESIAN_POINT('Ctrl Pts',(-10.5436588932818,12.4364614474871,
9.9552105732648));
#123757=CARTESIAN_POINT('Ctrl Pts',(-10.5370764158648,12.4359671375187,
9.95181162528969));
#123758=CARTESIAN_POINT('Ctrl Pts',(-10.4920233428744,12.4326226419558,
9.92908373425419));
#123759=CARTESIAN_POINT('Ctrl Pts',(-10.452545484898,12.4298827672595,9.91181248020323));
#123760=CARTESIAN_POINT('Ctrl Pts',(-10.3955466647752,12.426071048336,9.89051625698182));
#123761=CARTESIAN_POINT('Ctrl Pts',(-10.3787481094242,12.4249647734204,
9.88466989890805));
#123762=CARTESIAN_POINT('Ctrl Pts',(-10.317283313217,12.4209588483814,9.86482736107988));
#123763=CARTESIAN_POINT('Ctrl Pts',(-10.2719264923229,12.4180803149453,
9.8531165990746));
#123764=CARTESIAN_POINT('Ctrl Pts',(-10.1731205530919,12.4117912305726,
9.83379814898562));
#123765=CARTESIAN_POINT('Ctrl Pts',(-10.1196068466762,12.4083722814087,
9.8271016259962));
#123766=CARTESIAN_POINT('Ctrl Pts',(-10.0542309563397,12.4040751518198,
9.82344190264234));
#123767=CARTESIAN_POINT('Ctrl Pts',(-10.0426262548855,12.4033079871435,
9.82296434216628));
#123768=CARTESIAN_POINT('Ctrl Pts',(-10.0241990088803,12.4020819532691,
9.82247888177279));
#123769=CARTESIAN_POINT('Ctrl Pts',(-10.0173799932372,12.4016265572039,
9.82235849748672));
#123770=CARTESIAN_POINT('Ctrl Pts',(-10.0045113276275,12.4007637601384,
9.82224310442615));
#123771=CARTESIAN_POINT('Ctrl Pts',(-9.99846199040873,12.4003567627693,
9.82223546948614));
#123772=CARTESIAN_POINT('Ctrl Pts',(-9.98477333157773,12.3994324743206,
9.82232365338146));
#123773=CARTESIAN_POINT('Ctrl Pts',(-9.97713452480975,12.3989143442458,
9.82244720113989));
#123774=CARTESIAN_POINT('Ctrl Pts',(-9.95389411097235,12.3973305713491,
9.82304930340815));
#123775=CARTESIAN_POINT('Ctrl Pts',(-9.9383008709507,12.3962577457753,9.82376368351143));
#123776=CARTESIAN_POINT('Ctrl Pts',(-9.88532245655986,12.3925764129702,
9.82724713746238));
#123777=CARTESIAN_POINT('Ctrl Pts',(-9.84808779705843,12.3899264143302,
9.83148889359536));
#123778=CARTESIAN_POINT('Ctrl Pts',(-9.81114930150156,12.3872370429983,
9.83748958018577));
#123779=CARTESIAN_POINT('Ctrl Pts',(-9.81114930147754,12.2889045666398,
9.83748958018968));
#123780=CARTESIAN_POINT('Ctrl Pts',(-9.81383173227387,12.2890900172582,
9.83705381727436));
#123781=CARTESIAN_POINT('Ctrl Pts',(-9.81651570929456,12.2892749519145,
9.83662733246075));
#123782=CARTESIAN_POINT('Ctrl Pts',(-9.82298737303286,12.2897193534125,
9.83562193711081));
#123783=CARTESIAN_POINT('Ctrl Pts',(-9.82677644394306,12.2899783050531,
9.83505221399412));
#123784=CARTESIAN_POINT('Ctrl Pts',(-9.83713737611941,12.2906831715642,
9.83354601761439));
#123785=CARTESIAN_POINT('Ctrl Pts',(-9.84371460154284,12.2911270965891,
9.83264658026892));
#123786=CARTESIAN_POINT('Ctrl Pts',(-9.87610734113437,12.2932976282326,
9.82849555443918));
#123787=CARTESIAN_POINT('Ctrl Pts',(-9.90202018048166,12.2949847476504,
9.82604419001744));
#123788=CARTESIAN_POINT('Ctrl Pts',(-10.0093483690408,12.3018478843484,
9.81947009334006));
#123789=CARTESIAN_POINT('Ctrl Pts',(-10.0910041442942,12.3067875563781,
9.82294501328452));
#123790=CARTESIAN_POINT('Ctrl Pts',(-10.2264940354,12.3153341786876,9.84290514455523));
#123791=CARTESIAN_POINT('Ctrl Pts',(-10.2806912153051,12.3188477973632,
9.85484528147258));
#123792=CARTESIAN_POINT('Ctrl Pts',(-10.3450495814925,12.3232513836494,
9.87386837710154));
#123793=CARTESIAN_POINT('Ctrl Pts',(-10.3562068552719,12.3240232546126,
9.87734764682795));
#123794=CARTESIAN_POINT('Ctrl Pts',(-10.3738037736563,12.325254983368,9.88312377085827));
#123795=CARTESIAN_POINT('Ctrl Pts',(-10.3802785640701,12.3257113095331,
9.8853117104703));
#123796=CARTESIAN_POINT('Ctrl Pts',(-10.3924436753499,12.3265747313485,
9.88954083070421));
#123797=CARTESIAN_POINT('Ctrl Pts',(-10.3981380585138,12.3269814135963,
9.8915697184646));
#123798=CARTESIAN_POINT('Ctrl Pts',(-10.4109664978768,12.3279034355693,
9.89625205161689));
#123799=CARTESIAN_POINT('Ctrl Pts',(-10.4180908991964,12.3284195994309,
9.89893097798448));
#123800=CARTESIAN_POINT('Ctrl Pts',(-10.4396139290726,12.3299917305461,
9.9072631018026));
#123801=CARTESIAN_POINT('Ctrl Pts',(-10.4539271228197,12.3310547287337,
9.91313088961841));
#123802=CARTESIAN_POINT('Ctrl Pts',(-10.5502698728734,12.3383328789426,
9.95486224856121));
#123803=CARTESIAN_POINT('Ctrl Pts',(-10.6280801335751,12.3448567434955,
9.99969034442004));
#123804=CARTESIAN_POINT('Ctrl Pts',(-10.7366301626911,12.354762618692,10.0799236801379));
#123805=CARTESIAN_POINT('Ctrl Pts',(-10.7716170726544,12.358097575809,10.1090611746994));
#123806=CARTESIAN_POINT('Ctrl Pts',(-10.8213211854691,12.3629733663097,
10.1555850179048));
#123807=CARTESIAN_POINT('Ctrl Pts',(-10.8373640777366,12.3645707057991,
10.171491271185));
#123808=CARTESIAN_POINT('Ctrl Pts',(-10.8571467901598,12.366560312435,10.1922675900918));
#123809=CARTESIAN_POINT('Ctrl Pts',(-10.8613185742236,12.3669810534016,
10.1967176190142));
#123810=CARTESIAN_POINT('Ctrl Pts',(-10.8679741308999,12.3676539068072,
10.203928547089));
#123811=CARTESIAN_POINT('Ctrl Pts',(-10.8704796794235,12.367907583808,10.2066690610299));
#123812=CARTESIAN_POINT('Ctrl Pts',(-10.8752763759233,12.3683938770941,
10.2119656667887));
#123813=CARTESIAN_POINT('Ctrl Pts',(-10.8775693565291,12.3686266217461,
10.2145199751907));
#123814=CARTESIAN_POINT('Ctrl Pts',(-10.8826144134907,12.3691394202105,
10.2201896778483));
#123815=CARTESIAN_POINT('Ctrl Pts',(-10.8853612569619,12.3694190947035,
10.2233097223448));
#123816=CARTESIAN_POINT('Ctrl Pts',(-10.8950573742619,12.3704082953551,
10.2344414871539));
#123817=CARTESIAN_POINT('Ctrl Pts',(-10.9019151334402,12.3711115665998,
10.2425327392474));
#123818=CARTESIAN_POINT('Ctrl Pts',(-10.9487048044757,12.3759445115104,
10.2992749527889));
#123819=CARTESIAN_POINT('Ctrl Pts',(-10.9847951520627,12.3798541930568,
10.3509722981556));
#123820=CARTESIAN_POINT('Ctrl Pts',(-11.0365092950994,12.3861946413552,
10.4393746423769));
#123821=CARTESIAN_POINT('Ctrl Pts',(-11.0547102834317,12.3886280209249,
10.4744160904239));
#123822=CARTESIAN_POINT('Ctrl Pts',(-11.0936826949566,12.394481730254,10.5596609437193));
#123823=CARTESIAN_POINT('Ctrl Pts',(-11.1128066182164,12.3979247438835,
10.6105123319528));
#123824=CARTESIAN_POINT('Ctrl Pts',(-11.1316890345852,12.4022488582423,
10.6736408508139));
#123825=CARTESIAN_POINT('Ctrl Pts',(-11.1348569835265,12.4030171710055,
10.6848334147411));
#123826=CARTESIAN_POINT('Ctrl Pts',(-11.1396192647359,12.4042445492705,
10.7026625717775));
#123827=CARTESIAN_POINT('Ctrl Pts',(-11.1413226362922,12.4047001272313,
10.7092694522982));
#123828=CARTESIAN_POINT('Ctrl Pts',(-11.1444272645068,12.4055629617689,
10.7217593338015));
#123829=CARTESIAN_POINT('Ctrl Pts',(-11.1458408076143,12.4059698122316,
10.7276390752276));
#123830=CARTESIAN_POINT('Ctrl Pts',(-11.1489355190148,12.4068933463511,
10.7409624213983));
#123831=CARTESIAN_POINT('Ctrl Pts',(-11.1505897351065,12.4074108646688,
10.7484119424355));
#123832=CARTESIAN_POINT('Ctrl Pts',(-11.155291028379,12.4089559472228,10.7706003174318));
#123833=CARTESIAN_POINT('Ctrl Pts',(-11.1581280060205,12.4099900338806,
10.7853815944423));
#123834=CARTESIAN_POINT('Ctrl Pts',(-11.1762906896256,12.4174091955278,
10.890899156526));
#123835=CARTESIAN_POINT('Ctrl Pts',(-11.1812156698372,12.4241232825722,
10.9830866878563));
#123836=CARTESIAN_POINT('Ctrl Pts',(-11.1725744385655,12.4340953702116,
11.1187130782638));
#123837=CARTESIAN_POINT('Ctrl Pts',(-11.1673328681741,12.4373115991175,
11.1623515743318));
#123838=CARTESIAN_POINT('Ctrl Pts',(-11.155804320499,12.4420384271522,11.2273779522965));
#123839=CARTESIAN_POINT('Ctrl Pts',(-11.1513297072006,12.4436020800488,
11.2490470190653));
#123840=CARTESIAN_POINT('Ctrl Pts',(-11.1448551867644,12.4455562824911,
11.2764748909272));
#123841=CARTESIAN_POINT('Ctrl Pts',(-11.1434178589975,12.4459741282282,
11.2823603506691));
#123842=CARTESIAN_POINT('Ctrl Pts',(-11.1410286320628,12.4466434761926,
11.2918260500629));
#123843=CARTESIAN_POINT('Ctrl Pts',(-11.1401051675985,12.4468965148387,
11.2954132536908));
#123844=CARTESIAN_POINT('Ctrl Pts',(-11.1382923925061,12.4473824207276,
11.3023198638966));
#123845=CARTESIAN_POINT('Ctrl Pts',(-11.1374054609663,12.4476154100539,
11.3056398021211));
#123846=CARTESIAN_POINT('Ctrl Pts',(-11.1354089212677,12.4481296270556,
11.3129841375192));
#123847=CARTESIAN_POINT('Ctrl Pts',(-11.1342924100443,12.448410467045,11.3170066539719));
#123848=CARTESIAN_POINT('Ctrl Pts',(-11.1303481425142,12.4493800003188,
11.3309292122626));
#123849=CARTESIAN_POINT('Ctrl Pts',(-11.1274118783254,12.4500628765946,
11.340798387688));
#123850=CARTESIAN_POINT('Ctrl Pts',(-11.1038793784072,12.4552594719201,
11.416259184072));
#123851=CARTESIAN_POINT('Ctrl Pts',(-11.0777021179619,12.4595082351514,
11.4799813422831));
#123852=CARTESIAN_POINT('Ctrl Pts',(-11.0190893860017,12.4674010076476,
11.5933054904039));
#123853=CARTESIAN_POINT('Ctrl Pts',(-10.9881945566757,12.4710326836439,
11.6434481234495));
#123854=CARTESIAN_POINT('Ctrl Pts',(-10.9409783680066,12.4761541728011,
11.7086068849954));
#123855=CARTESIAN_POINT('Ctrl Pts',(-10.9277911490262,12.4775459195896,
11.7257875075303));
#123856=CARTESIAN_POINT('Ctrl Pts',(-10.9038809566076,12.4800131027819,
11.7552211165978));
#123857=CARTESIAN_POINT('Ctrl Pts',(-10.893363413515,12.4810808247063,11.7676336941122));
#123858=CARTESIAN_POINT('Ctrl Pts',(-10.8774524296126,12.4826732857733,
11.7856414962697));
#123859=CARTESIAN_POINT('Ctrl Pts',(-10.8722550154339,12.4831900344556,
11.7914079290279));
#123860=CARTESIAN_POINT('Ctrl Pts',(-10.8628993845384,12.4841144160741,
11.8015837082938));
#123861=CARTESIAN_POINT('Ctrl Pts',(-10.8587633859077,12.4845211103968,
11.806013172301));
#123862=CARTESIAN_POINT('Ctrl Pts',(-10.8499538023294,12.4853833745067,
11.8153030481195));
#123863=CARTESIAN_POINT('Ctrl Pts',(-10.8452723087885,12.4858392732942,
11.8201556237085));
#123864=CARTESIAN_POINT('Ctrl Pts',(-10.832659036157,12.4870616482828,11.8330071335704));
#123865=CARTESIAN_POINT('Ctrl Pts',(-10.8246538960569,12.4878312867054,
11.8409327508884));
#123866=CARTESIAN_POINT('Ctrl Pts',(-10.7863150082217,12.4914897826344,
11.8778168680624));
#123867=CARTESIAN_POINT('Ctrl Pts',(-10.7545657022235,12.4944413852421,
11.9052533422834));
#123868=CARTESIAN_POINT('Ctrl Pts',(-10.634773938621,12.5053073404985,11.9980853860355));
#123869=CARTESIAN_POINT('Ctrl Pts',(-10.5391842613604,12.5135454495557,
12.0528008253265));
#123870=CARTESIAN_POINT('Ctrl Pts',(-10.4279657758124,12.5220272348384,
12.097289356547));
#123871=CARTESIAN_POINT('Ctrl Pts',(-10.4184675869722,12.5227428703444,
12.1009466524536));
#123872=CARTESIAN_POINT('Ctrl Pts',(-10.4015548069343,12.5240003686634,
12.1072084397259));
#123873=CARTESIAN_POINT('Ctrl Pts',(-10.3941594166615,12.5245446123103,
12.1098626737236));
#123874=CARTESIAN_POINT('Ctrl Pts',(-10.3828735705865,12.5253660735851,
12.1137861680705));
#123875=CARTESIAN_POINT('Ctrl Pts',(-10.379002319948,12.525646234837,12.1151094304975));
#123876=CARTESIAN_POINT('Ctrl Pts',(-10.3719155598545,12.5261560559811,
12.1174906426592));
#123877=CARTESIAN_POINT('Ctrl Pts',(-10.3687023545423,12.5263860649456,
12.1185549134768));
#123878=CARTESIAN_POINT('Ctrl Pts',(-10.3614199813835,12.5269047844032,
12.1209321746096));
#123879=CARTESIAN_POINT('Ctrl Pts',(-10.3573482163626,12.5271930173748,
12.1222368719274));
#123880=CARTESIAN_POINT('Ctrl Pts',(-10.3467516696572,12.5279386886658,
12.1255687549981));
#123881=CARTESIAN_POINT('Ctrl Pts',(-10.3402160848432,12.5283942375078,
12.1275614234385));
#123882=CARTESIAN_POINT('Ctrl Pts',(-10.2879317211156,12.5320067027754,
12.1430066818791));
#123883=CARTESIAN_POINT('Ctrl Pts',(-10.2414158378224,12.5350271686034,
12.1537280799974));
#123884=CARTESIAN_POINT('Ctrl Pts',(-10.1189054147635,12.5427815828107,
12.1742279749265));
#123885=CARTESIAN_POINT('Ctrl Pts',(-10.0423889904386,12.5474393654137,
12.1794715062008));
#123886=CARTESIAN_POINT('Ctrl Pts',(-9.92748329316009,12.5547059698119,
12.176143617985));
#123887=CARTESIAN_POINT('Ctrl Pts',(-9.88914318632026,12.5571737880781,
12.173150795251));
#123888=CARTESIAN_POINT('Ctrl Pts',(-9.84011850951595,12.5604215082524,
12.1668992078778));
#123889=CARTESIAN_POINT('Ctrl Pts',(-9.8292366569593,12.5611482064698,12.1653564775146));
#123890=CARTESIAN_POINT('Ctrl Pts',(-9.81177436318909,12.5623244558508,
12.162631001767));
#123891=CARTESIAN_POINT('Ctrl Pts',(-9.80517945702542,12.5627710119694,
12.1615440971186));
#123892=CARTESIAN_POINT('Ctrl Pts',(-9.79260891427126,12.5636268060776,
12.159362283235));
#123893=CARTESIAN_POINT('Ctrl Pts',(-9.78663178150155,12.564035724877,12.1582771547397));
#123894=CARTESIAN_POINT('Ctrl Pts',(-9.77292413074451,12.5649782453653,
12.1556788742987));
#123895=CARTESIAN_POINT('Ctrl Pts',(-9.76519993516243,12.5655128178143,
12.1541343228734));
#123896=CARTESIAN_POINT('Ctrl Pts',(-9.74097322673439,12.5672007182818,
12.1490366154183));
#123897=CARTESIAN_POINT('Ctrl Pts',(-9.72453190157307,12.5683626817358,
12.1452062209552));
#123898=CARTESIAN_POINT('Ctrl Pts',(-9.68615936799015,12.5711148316239,
12.1353923165588));
#123899=CARTESIAN_POINT('Ctrl Pts',(-9.66430842761712,12.5727133462199,
12.1291247523341));
#123900=CARTESIAN_POINT('Ctrl Pts',(-9.53385442457937,12.582446407804,12.08758488285));
#123901=CARTESIAN_POINT('Ctrl Pts',(-9.430691227497,12.5910250083356,12.0373110505005));
#123902=CARTESIAN_POINT('Ctrl Pts',(-9.32077732291851,12.6005096726938,
11.962345260387));
#123903=CARTESIAN_POINT('Ctrl Pts',(-9.30542978302708,12.6018408142823,
11.9513275760085));
#123904=CARTESIAN_POINT('Ctrl Pts',(-9.28560293330061,12.6035628564676,
11.9363585407384));
#123905=CARTESIAN_POINT('Ctrl Pts',(-9.28088006361357,12.6039732378647,
11.9327363006486));
#123906=CARTESIAN_POINT('Ctrl Pts',(-9.27328101219053,12.6046335635537,
11.9268161222098));
#123907=CARTESIAN_POINT('Ctrl Pts',(-9.27038786150642,12.6048849723301,
11.9245402857287));
#123908=CARTESIAN_POINT('Ctrl Pts',(-9.26477103355307,12.6053729973934,
11.9200791392653));
#123909=CARTESIAN_POINT('Ctrl Pts',(-9.26204634421165,12.6056096979167,
11.917895232544));
#123910=CARTESIAN_POINT('Ctrl Pts',(-9.25540042905378,12.6061870592657,
11.9125196455374));
#123911=CARTESIAN_POINT('Ctrl Pts',(-9.25148990493053,12.6065267986259,
11.9093147224343));
#123912=CARTESIAN_POINT('Ctrl Pts',(-9.23731268332321,12.6077590530955,
11.897542156968));
#123913=CARTESIAN_POINT('Ctrl Pts',(-9.22717100683596,12.6086416336667,
11.8888246457526));
#123914=CARTESIAN_POINT('Ctrl Pts',(-9.15098072007739,12.6153002315115,
11.8210432057346));
#123915=CARTESIAN_POINT('Ctrl Pts',(-9.09163063385042,12.6206679816203,
11.7548608605004));
#123916=CARTESIAN_POINT('Ctrl Pts',(-9.00370540351625,12.6300950971517,
11.6312447052773));
#123917=CARTESIAN_POINT('Ctrl Pts',(-8.97134151426516,12.634066809928,11.577003457373));
#123918=CARTESIAN_POINT('Ctrl Pts',(-8.93812220494041,12.6389938285286,
11.5095659544643));
#123919=CARTESIAN_POINT('Ctrl Pts',(-8.9329355465158,12.6397934233851,11.4986134254098));
#123920=CARTESIAN_POINT('Ctrl Pts',(-8.92502114557952,12.6410639236338,
11.4812115127273));
#123921=CARTESIAN_POINT('Ctrl Pts',(-8.92218024081496,12.6415309902298,
11.474814301163));
#123922=CARTESIAN_POINT('Ctrl Pts',(-8.91699808661008,12.6424040822049,
11.4628588227457));
#123923=CARTESIAN_POINT('Ctrl Pts',(-8.91464217084767,12.6428095978943,
11.4573071337555));
#123924=CARTESIAN_POINT('Ctrl Pts',(-8.90949529707561,12.6437150930461,
11.4449147534415));
#123925=CARTESIAN_POINT('Ctrl Pts',(-8.90672587948089,12.6442157719862,
11.4380654494884));
#123926=CARTESIAN_POINT('Ctrl Pts',(-8.89877656886888,12.6456936182524,
11.4178602899702));
#123927=CARTESIAN_POINT('Ctrl Pts',(-8.89377585113021,12.6466766265054,
11.404435864322));
#123928=CARTESIAN_POINT('Ctrl Pts',(-8.87217991296978,12.651177705311,11.3430617331618));
#123929=CARTESIAN_POINT('Ctrl Pts',(-8.85845116710635,12.6547858854001,
11.2941675333026));
#123930=CARTESIAN_POINT('Ctrl Pts',(-8.83140579959324,12.6642207392366,
11.1667541177985));
#123931=CARTESIAN_POINT('Ctrl Pts',(-8.82281541907372,12.6701307758134,
11.0874937278619));
#123932=CARTESIAN_POINT('Ctrl Pts',(-8.82208805224753,12.6778756390834,
10.9800691998945));
#123933=CARTESIAN_POINT('Ctrl Pts',(-8.82289093543136,12.6798613753455,
10.9521635765681));
#123934=CARTESIAN_POINT('Ctrl Pts',(-8.82511505088381,12.6822668131692,
10.9176272494007));
#123935=CARTESIAN_POINT('Ctrl Pts',(-8.82560245808805,12.6827296136136,
10.9109475857441));
#123936=CARTESIAN_POINT('Ctrl Pts',(-8.82646247863124,12.6834560664612,
10.9004016588598));
#123937=CARTESIAN_POINT('Ctrl Pts',(-8.82679727333158,12.6837216875961,
10.8965325807228));
#123938=CARTESIAN_POINT('Ctrl Pts',(-8.82746194930453,12.6842185268924,
10.8892696602143));
#123939=CARTESIAN_POINT('Ctrl Pts',(-8.82778742918393,12.6844499655391,
10.8858756044523));
#123940=CARTESIAN_POINT('Ctrl Pts',(-8.82858384972127,12.6849898415465,
10.8779337556712));
#123941=CARTESIAN_POINT('Ctrl Pts',(-8.82906653734369,12.6852976306464,
10.873387232452));
#123942=CARTESIAN_POINT('Ctrl Pts',(-8.83073208749951,12.6862999909181,
10.8585240652326));
#123943=CARTESIAN_POINT('Ctrl Pts',(-8.83202495304457,12.6869888344812,
10.8482198987244));
#123944=CARTESIAN_POINT('Ctrl Pts',(-8.8401121556615,12.6908528267042,10.7900085556355));
#123945=CARTESIAN_POINT('Ctrl Pts',(-8.84971818265734,12.6938994901274,
10.7425334265172));
#123946=CARTESIAN_POINT('Ctrl Pts',(-8.88432411217041,12.7022368463267,
10.6131078186209));
#123947=CARTESIAN_POINT('Ctrl Pts',(-8.91537150895569,12.7074455303491,
10.5330967194049));
#123948=CARTESIAN_POINT('Ctrl Pts',(-8.96724838437296,12.7146511125664,
10.4332133857361));
#123949=CARTESIAN_POINT('Ctrl Pts',(-8.98050195524227,12.7164008428838,
10.4097064064854));
#123950=CARTESIAN_POINT('Ctrl Pts',(-8.99960050817822,12.7188179952596,
10.3783972557602));
#123951=CARTESIAN_POINT('Ctrl Pts',(-9.00475279765119,12.7194607006416,
10.3701808895838));
#123952=CARTESIAN_POINT('Ctrl Pts',(-9.01312728376249,12.7204911812416,
10.3571854775149));
#123953=CARTESIAN_POINT('Ctrl Pts',(-9.01628418375284,12.7208765591536,
10.3523647174228));
#123954=CARTESIAN_POINT('Ctrl Pts',(-9.02285815988468,12.721672919849,10.3424848625733));
#123955=CARTESIAN_POINT('Ctrl Pts',(-9.02627944355355,12.7220840504695,
10.3374287908513));
#123956=CARTESIAN_POINT('Ctrl Pts',(-9.03434531225376,12.7230458007598,
10.3257062222593));
#123957=CARTESIAN_POINT('Ctrl Pts',(-9.03901983408079,12.7235975328591,
10.3190608032694));
#123958=CARTESIAN_POINT('Ctrl Pts',(-9.05444292695788,12.7254001848041,
10.2976100767621));
#123959=CARTESIAN_POINT('Ctrl Pts',(-9.06546733670553,12.7266615174542,
10.2830073787407));
#123960=CARTESIAN_POINT('Ctrl Pts',(-9.12791011315197,12.7336648027364,
10.2041847677976));
#123961=CARTESIAN_POINT('Ctrl Pts',(-9.1856006621458,12.7396550354643,10.1452415614109));
#123962=CARTESIAN_POINT('Ctrl Pts',(-9.29805742075508,12.7503698574778,
10.0521411516742));
#123963=CARTESIAN_POINT('Ctrl Pts',(-9.35039191603067,12.7550519855471,
10.0155353481846));
#123964=CARTESIAN_POINT('Ctrl Pts',(-9.41368114100117,12.7601988112945,
9.97852240813713));
#123965=CARTESIAN_POINT('Ctrl Pts',(-9.42198400478981,12.7608643245444,
9.97380128700313));
#123966=CARTESIAN_POINT('Ctrl Pts',(-9.43474843910004,12.7618717227801,
9.96674733856949));
#123967=CARTESIAN_POINT('Ctrl Pts',(-9.4391688396424,12.7622177496953,9.96434136834038));
#123968=CARTESIAN_POINT('Ctrl Pts',(-9.44664485640826,12.7627980265347,
9.96033416613209));
#123969=CARTESIAN_POINT('Ctrl Pts',(-9.44969229957226,12.7630331905975,
9.95871790705176));
#123970=CARTESIAN_POINT('Ctrl Pts',(-9.45599999319334,12.7635170484619,
9.95540794953687));
#123971=CARTESIAN_POINT('Ctrl Pts',(-9.45926112821108,12.7637656306932,
9.9537160840547));
#123972=CARTESIAN_POINT('Ctrl Pts',(-9.46780137686993,12.7644126480962,
9.94933602795103));
#123973=CARTESIAN_POINT('Ctrl Pts',(-9.4730930301969,12.764809608459,9.94667231810796));
#123974=CARTESIAN_POINT('Ctrl Pts',(-9.49695672178769,12.7665831506817,
9.93488466453105));
#123975=CARTESIAN_POINT('Ctrl Pts',(-9.51574840485089,12.7679347877326,
9.92621057213089));
#123976=CARTESIAN_POINT('Ctrl Pts',(-9.57089692878683,12.7718003172363,
9.9024969585786));
#123977=CARTESIAN_POINT('Ctrl Pts',(-9.60779219707913,12.7742623584784,
9.88877730847137));
#123978=CARTESIAN_POINT('Ctrl Pts',(-9.69961543009393,12.7802429163818,
9.85977733714761));
#123979=CARTESIAN_POINT('Ctrl Pts',(-9.75504250514998,12.7837322841863,
9.84660417176354));
#123980=CARTESIAN_POINT('Ctrl Pts',(-9.81114930150157,12.7872971999427,
9.83748958018577));
#123981=CARTESIAN_POINT('Origin',(-10.,2.67563288526385,11.));
#123982=CARTESIAN_POINT('',(-8.88725970493355,13.15,11.3858809379011));
#123983=CARTESIAN_POINT('Ctrl Pts',(-9.81114930150157,12.7872971999427,
9.83748958018577));
#123984=CARTESIAN_POINT('Ctrl Pts',(-9.85064840761449,12.7898068956463,
9.83107292047043));
#123985=CARTESIAN_POINT('Ctrl Pts',(-9.89048444922047,12.7923530522079,
9.82666770785197));
#123986=CARTESIAN_POINT('Ctrl Pts',(-9.94663828774431,12.7960136030827,
9.82334849075221));
#123987=CARTESIAN_POINT('Ctrl Pts',(-9.96278856564973,12.7970744726786,
9.82272708569078));
#123988=CARTESIAN_POINT('Ctrl Pts',(-9.98669013886237,12.7986588315724,
9.82229973999947));
#123989=CARTESIAN_POINT('Ctrl Pts',(-9.99443538998884,12.799174457132,9.82223767884118));
#123990=CARTESIAN_POINT('Ctrl Pts',(-10.0082416296171,12.8000977904741,
9.82226324036451));
#123991=CARTESIAN_POINT('Ctrl Pts',(-10.0143024454134,12.800504571097,9.82232125043788));
#123992=CARTESIAN_POINT('Ctrl Pts',(-10.027120084049,12.8013680283292,9.82254289129614));
#123993=CARTESIAN_POINT('Ctrl Pts',(-10.0338764643338,12.8018250417664,
9.82271790819828));
#123994=CARTESIAN_POINT('Ctrl Pts',(-10.0519517448613,12.8030528792592,
9.82334185329487));
#123995=CARTESIAN_POINT('Ctrl Pts',(-10.0632660616117,12.803826910191,9.82389593660675));
#123996=CARTESIAN_POINT('Ctrl Pts',(-10.1230689540906,12.8079482890019,
9.82769002283007));
#123997=CARTESIAN_POINT('Ctrl Pts',(-10.1713241722421,12.8113817712899,
9.83376522166938));
#123998=CARTESIAN_POINT('Ctrl Pts',(-10.2684680361244,12.8185071586902,
9.85215484172937));
#123999=CARTESIAN_POINT('Ctrl Pts',(-10.3172227257137,12.8221968221134,
9.86466182323661));
#124000=CARTESIAN_POINT('Ctrl Pts',(-10.3833145208831,12.8272968664482,
9.88620690359202));
#124001=CARTESIAN_POINT('Ctrl Pts',(-10.401454686601,12.8287068810652,9.89261603818782));
#124002=CARTESIAN_POINT('Ctrl Pts',(-10.4603959511511,12.8333092993468,
9.91507944917733));
#124003=CARTESIAN_POINT('Ctrl Pts',(-10.5004630618422,12.8364724544636,
9.93296925254057));
#124004=CARTESIAN_POINT('Ctrl Pts',(-10.5460305082256,12.840042841253,9.95644805498468));
#124005=CARTESIAN_POINT('Ctrl Pts',(-10.5525860006101,12.8405557785544,
9.95990447708994));
#124006=CARTESIAN_POINT('Ctrl Pts',(-10.5626705435065,12.8413432513868,
9.96534387343638));
#124007=CARTESIAN_POINT('Ctrl Pts',(-10.566222591352,12.8416203109166,9.96728347595301));
#124008=CARTESIAN_POINT('Ctrl Pts',(-10.5727400850639,12.8421280067585,
9.97088610161777));
#124009=CARTESIAN_POINT('Ctrl Pts',(-10.5757083385015,12.8423589581212,
9.97254366013215));
#124010=CARTESIAN_POINT('Ctrl Pts',(-10.5824661353693,12.8428841936287,
9.97635588931542));
#124011=CARTESIAN_POINT('Ctrl Pts',(-10.5862509334626,12.8431779586374,
9.97851876732213));
#124012=CARTESIAN_POINT('Ctrl Pts',(-10.5979409157031,12.8440843346478,
9.98528555300132));
#124013=CARTESIAN_POINT('Ctrl Pts',(-10.605804754991,12.8446926752615,9.98996071412177));
#124014=CARTESIAN_POINT('Ctrl Pts',(-10.6241804707968,12.8461128936734,
10.0011771614478));
#124015=CARTESIAN_POINT('Ctrl Pts',(-10.6346454260007,12.8469206797104,
10.007793604037));
#124016=CARTESIAN_POINT('Ctrl Pts',(-10.6722966265972,12.8498305976039,
10.0324379689147));
#124017=CARTESIAN_POINT('Ctrl Pts',(-10.6988368009481,12.8518890116896,
10.0514292516681));
#124018=CARTESIAN_POINT('Ctrl Pts',(-10.7849522050021,12.8587123786858,
10.1186294379401));
#124019=CARTESIAN_POINT('Ctrl Pts',(-10.840604564399,12.8633793432393,10.1715387674165));
#124020=CARTESIAN_POINT('Ctrl Pts',(-10.9154652957684,12.8706186466293,
10.2580778984159));
#124021=CARTESIAN_POINT('Ctrl Pts',(-10.9388117405499,12.8730480455368,
10.2878503040314));
#124022=CARTESIAN_POINT('Ctrl Pts',(-10.9670423297474,12.8762553360454,
10.327657085576));
#124023=CARTESIAN_POINT('Ctrl Pts',(-10.9732743790793,12.8769821251904,
10.3367105972208));
#124024=CARTESIAN_POINT('Ctrl Pts',(-10.9830972662635,12.8781592268787,
10.3514171971944));
#124025=CARTESIAN_POINT('Ctrl Pts',(-10.9867682829658,12.878606559447,10.3570161435543));
#124026=CARTESIAN_POINT('Ctrl Pts',(-10.9936883970188,12.8794643442666,
10.3677693837309));
#124027=CARTESIAN_POINT('Ctrl Pts',(-10.9969456342904,12.8798744806926,
10.3729182011871));
#124028=CARTESIAN_POINT('Ctrl Pts',(-11.0043403187278,12.8808205698479,
10.3848104544928));
#124029=CARTESIAN_POINT('Ctrl Pts',(-11.0084500209594,12.881357503299,10.3915707085629));
#124030=CARTESIAN_POINT('Ctrl Pts',(-11.0211759631318,12.8830560975778,
10.4129874288123));
#124031=CARTESIAN_POINT('Ctrl Pts',(-11.0295427999917,12.884226510488,10.4277887825921));
#124032=CARTESIAN_POINT('Ctrl Pts',(-11.048431563209,12.887000988222,10.46296017347));
#124033=CARTESIAN_POINT('Ctrl Pts',(-11.0586845926314,12.8886135322086,
10.4834660399043));
#124034=CARTESIAN_POINT('Ctrl Pts',(-11.1175969135865,12.8985663482114,
10.6104227826123));
#124035=CARTESIAN_POINT('Ctrl Pts',(-11.1507538847801,12.9073748326706,
10.7233184485896));
#124036=CARTESIAN_POINT('Ctrl Pts',(-11.1689763819234,12.91685604592,10.855566575958));
#124037=CARTESIAN_POINT('Ctrl Pts',(-11.1708835505594,12.9180142777831,
10.8719430840064));
#124038=CARTESIAN_POINT('Ctrl Pts',(-11.1729825308593,12.9195474635182,
10.8939856869771));
#124039=CARTESIAN_POINT('Ctrl Pts',(-11.1734781339901,12.9199371118442,
10.8996200989351));
#124040=CARTESIAN_POINT('Ctrl Pts',(-11.1741951881055,12.9205477696985,
10.9085050033524));
#124041=CARTESIAN_POINT('Ctrl Pts',(-11.1744437680385,12.9207702178147,
10.9117531272488));
#124042=CARTESIAN_POINT('Ctrl Pts',(-11.1749276113275,12.9212264701463,
10.918439901416));
#124043=CARTESIAN_POINT('Ctrl Pts',(-11.1751612545557,12.9214601623584,
10.9218785071881));
#124044=CARTESIAN_POINT('Ctrl Pts',(-11.1756904856625,12.9220240582894,
10.9302078146349));
#124045=CARTESIAN_POINT('Ctrl Pts',(-11.1759706558401,12.9223534136191,
10.9350994148766));
#124046=CARTESIAN_POINT('Ctrl Pts',(-11.1768570537891,12.9235172961872,
10.952473963759));
#124047=CARTESIAN_POINT('Ctrl Pts',(-11.1772951372886,12.9243431390457,
10.9649651632963));
#124048=CARTESIAN_POINT('Ctrl Pts',(-11.1778942756681,12.9263906475012,
10.9962675311418));
#124049=CARTESIAN_POINT('Ctrl Pts',(-11.1778036825287,12.9276013322428,
11.0150804885096));
#124050=CARTESIAN_POINT('Ctrl Pts',(-11.175292968582,12.9331557136721,11.1023119296313));
#124051=CARTESIAN_POINT('Ctrl Pts',(-11.1673611679931,12.9373310189597,
11.1704419972551));
#124052=CARTESIAN_POINT('Ctrl Pts',(-11.1401835166149,12.9456867082197,
11.3024453450685));
#124053=CARTESIAN_POINT('Ctrl Pts',(-11.1213537969094,12.9498491887249,
11.3661360153631));
#124054=CARTESIAN_POINT('Ctrl Pts',(-11.0928648193882,12.95498645553,11.4391906493396));
#124055=CARTESIAN_POINT('Ctrl Pts',(-11.0882877621961,12.9557858698275,
11.450412775935));
#124056=CARTESIAN_POINT('Ctrl Pts',(-11.0808075126212,12.9570540509385,
11.4679730154782));
#124057=CARTESIAN_POINT('Ctrl Pts',(-11.0780197508826,12.9575189298154,
11.4743596059181));
#124058=CARTESIAN_POINT('Ctrl Pts',(-11.0727329168234,12.9583866217539,
11.4861840841294));
#124059=CARTESIAN_POINT('Ctrl Pts',(-11.0702487432218,12.9587889165432,
11.4916284164401));
#124060=CARTESIAN_POINT('Ctrl Pts',(-11.0646402360107,12.9596854728129,
11.5036760802582));
#124061=CARTESIAN_POINT('Ctrl Pts',(-11.0614957605435,12.9601804136823,
11.5102697052732));
#124062=CARTESIAN_POINT('Ctrl Pts',(-11.0521130655825,12.9616353298062,
11.5294821088002));
#124063=CARTESIAN_POINT('Ctrl Pts',(-11.0457099006386,12.9626009636563,
11.5420184314903));
#124064=CARTESIAN_POINT('Ctrl Pts',(-11.0306161470636,12.9648181883696,
11.5703060253895));
#124065=CARTESIAN_POINT('Ctrl Pts',(-11.0217864437812,12.9660743908674,
11.5859786756873));
#124066=CARTESIAN_POINT('Ctrl Pts',(-10.9905093442848,12.9703915323975,
11.6386375013316));
#124067=CARTESIAN_POINT('Ctrl Pts',(-10.9663865323899,12.9735060763644,
11.6745835921664));
#124068=CARTESIAN_POINT('Ctrl Pts',(-10.9036696872257,12.9810974977375,
11.757750775982));
#124069=CARTESIAN_POINT('Ctrl Pts',(-10.8632791638431,12.9856033701052,
11.8034638172549));
#124070=CARTESIAN_POINT('Ctrl Pts',(-10.7940019939752,12.9926084524547,
11.8705858955302));
#124071=CARTESIAN_POINT('Ctrl Pts',(-10.7673595116995,12.9951571567793,
11.8941581907598));
#124072=CARTESIAN_POINT('Ctrl Pts',(-10.7341460224141,12.9981284485604,
11.920964392835));
#124073=CARTESIAN_POINT('Ctrl Pts',(-10.7285627175034,12.9986212835788,
11.9253875772014));
#124074=CARTESIAN_POINT('Ctrl Pts',(-10.7198087418057,12.9993832693491,
11.9321942742457));
#124075=CARTESIAN_POINT('Ctrl Pts',(-10.7166656921114,12.9996547347482,
11.934612795031));
#124076=CARTESIAN_POINT('Ctrl Pts',(-10.7108398683953,13.0001539198479,
11.9390489929892));
#124077=CARTESIAN_POINT('Ctrl Pts',(-10.7081606885353,13.0003819319455,
11.9410710755734));
#124078=CARTESIAN_POINT('Ctrl Pts',(-10.7019566247551,13.0009064149162,
11.9457120287394));
#124079=CARTESIAN_POINT('Ctrl Pts',(-10.6984256969912,13.0012023246584,
11.9483226727575));
#124080=CARTESIAN_POINT('Ctrl Pts',(-10.6873221083331,13.0021250698465,
11.9564366212971));
#124081=CARTESIAN_POINT('Ctrl Pts',(-10.6796981660609,13.002747384879,11.9618695897508));
#124082=CARTESIAN_POINT('Ctrl Pts',(-10.661529779794,13.0042061095415,11.97449282608));
#124083=CARTESIAN_POINT('Ctrl Pts',(-10.6509314775494,13.0050380960689,
11.9816038699702));
#124084=CARTESIAN_POINT('Ctrl Pts',(-10.6115063934171,13.0080722588288,
12.0071371389317));
#124085=CARTESIAN_POINT('Ctrl Pts',(-10.5819948410109,13.0102263456181,
12.024474318512));
#124086=CARTESIAN_POINT('Ctrl Pts',(-10.4827129035858,13.017232897787,12.0771225347248));
#124087=CARTESIAN_POINT('Ctrl Pts',(-10.410185886626,13.0219916803197,12.1067755462806));
#124088=CARTESIAN_POINT('Ctrl Pts',(-10.3006818366798,13.0292317291624,
12.1392920116502));
#124089=CARTESIAN_POINT('Ctrl Pts',(-10.2656570909294,13.0315527336887,
12.1479641872666));
#124090=CARTESIAN_POINT('Ctrl Pts',(-10.219712919835,13.034633686254,12.1571247398477));
#124091=CARTESIAN_POINT('Ctrl Pts',(-10.2091055608103,13.0353474104155,
12.159088556825));
#124092=CARTESIAN_POINT('Ctrl Pts',(-10.1919068403152,13.0365092172225,
12.1620289160807));
#124093=CARTESIAN_POINT('Ctrl Pts',(-10.1853313881247,13.0369544768231,
12.1630957444161));
#124094=CARTESIAN_POINT('Ctrl Pts',(-10.1726969820333,13.0378122427771,
12.1650357440693));
#124095=CARTESIAN_POINT('Ctrl Pts',(-10.1666395613961,13.0382244650599,
12.1659175728696));
#124096=CARTESIAN_POINT('Ctrl Pts',(-10.1526157983865,13.0391812008066,
12.167847609798));
#124097=CARTESIAN_POINT('Ctrl Pts',(-10.1446451314917,13.0397267549422,
12.1688615837893));
#124098=CARTESIAN_POINT('Ctrl Pts',(-10.119159634303,13.0414771061904,12.1718390077806));
#124099=CARTESIAN_POINT('Ctrl Pts',(-10.1016115513385,13.0426913701659,
12.1734908238236));
#124100=CARTESIAN_POINT('Ctrl Pts',(-10.0600501209667,13.0455901138855,
12.1764638564938));
#124101=CARTESIAN_POINT('Ctrl Pts',(-10.0360210437332,13.0472840853127,
12.1774445089455));
#124102=CARTESIAN_POINT('Ctrl Pts',(-9.94017878671836,13.0541112457052,
12.1784194724864));
#124103=CARTESIAN_POINT('Ctrl Pts',(-9.86846703037902,13.0593894184681,
12.1725818323701));
#124104=CARTESIAN_POINT('Ctrl Pts',(-9.74362477992669,13.0686674466244,
12.1508190538728));
#124105=CARTESIAN_POINT('Ctrl Pts',(-9.69022725301103,13.0726615020068,
12.1376093253964));
#124106=CARTESIAN_POINT('Ctrl Pts',(-9.63072331134241,13.0770173006316,
12.1183860409223));
#124107=CARTESIAN_POINT('Ctrl Pts',(-9.62352716063983,13.0775423898841,
12.1159842373226));
#124108=CARTESIAN_POINT('Ctrl Pts',(-9.61247056675385,13.0783460466103,
12.1121748407477));
#124109=CARTESIAN_POINT('Ctrl Pts',(-9.60859359596864,13.0786272512412,
12.1108163512405));
#124110=CARTESIAN_POINT('Ctrl Pts',(-9.60154494387888,13.079137317803,12.1083050203729));
#124111=CARTESIAN_POINT('Ctrl Pts',(-9.59837109712932,13.0793665390039,
12.1071588298828));
#124112=CARTESIAN_POINT('Ctrl Pts',(-9.59516341493462,13.0795977803896,
12.1059848116457));
#124113=CARTESIAN_POINT('Ctrl Pts',(-9.59512471554921,13.0796005701611,
12.1059706452882));
#124114=CARTESIAN_POINT('Ctrl Pts',(-9.5950477604444,13.0796061175977,12.1059424704019));
#124115=CARTESIAN_POINT('Ctrl Pts',(-9.59500950473514,13.0796088752635,
12.1059284619291));
#124116=CARTESIAN_POINT('Ctrl Pts',(-9.59493342020972,13.079614359702,12.105900596826));
#124117=CARTESIAN_POINT('Ctrl Pts',(-9.59489559137832,13.0796170864772,
12.1058867402398));
#124118=CARTESIAN_POINT('Ctrl Pts',(-9.59482034430635,13.0796225103139,
12.1058591730867));
#124119=CARTESIAN_POINT('Ctrl Pts',(-9.59478292608478,13.0796252073753,
12.1058454625741));
#124120=CARTESIAN_POINT('Ctrl Pts',(-9.59470848485319,13.0796305728967,
12.1058181820737));
#124121=CARTESIAN_POINT('Ctrl Pts',(-9.59467146172201,13.0796332413666,
12.1058046120867));
#124122=CARTESIAN_POINT('Ctrl Pts',(-9.59459779528503,13.079638550818,12.1057776071324));
#124123=CARTESIAN_POINT('Ctrl Pts',(-9.59456115205745,13.0796411917948,
12.1057641722367));
#124124=CARTESIAN_POINT('Ctrl Pts',(-9.59448823099611,13.0796464473036,
12.1057374323014));
#124125=CARTESIAN_POINT('Ctrl Pts',(-9.59445195313516,13.0796490618386,
12.1057241272927));
#124126=CARTESIAN_POINT('Ctrl Pts',(-9.59437974878,13.0796542654778,12.1056976421087));
#124127=CARTESIAN_POINT('Ctrl Pts',(-9.59434382223773,13.0796568545867,
12.1056844619546));
#124128=CARTESIAN_POINT('Ctrl Pts',(-9.59427230686273,13.0796620083611,
12.1056582215851));
#124129=CARTESIAN_POINT('Ctrl Pts',(-9.59423671803249,13.0796645730275,
12.1056451614076));
#124130=CARTESIAN_POINT('Ctrl Pts',(-9.59416586484047,13.0796696788744,
12.1056191562425));
#124131=CARTESIAN_POINT('Ctrl Pts',(-9.59413060052028,13.0796722200528,
12.1056062113054));
#124132=CARTESIAN_POINT('Ctrl Pts',(-9.59406038375695,13.079677279834,12.1055804321038));
#124133=CARTESIAN_POINT('Ctrl Pts',(-9.59402543126224,13.0796797984413,
12.105567597854));
#124134=CARTESIAN_POINT('Ctrl Pts',(-9.59395582574197,13.0796848139772,
12.1055420355708));
#124135=CARTESIAN_POINT('Ctrl Pts',(-9.59392117272207,13.0796873109062,
12.1055293075715));
#124136=CARTESIAN_POINT('Ctrl Pts',(-9.59385215419259,13.0796922839496,
12.105503953492));
#124137=CARTESIAN_POINT('Ctrl Pts',(-9.59381778869325,13.0796947600642,
12.105491327446));
#124138=CARTESIAN_POINT('Ctrl Pts',(-9.59374933359598,13.0796996923178,
12.1054661730986));
#124139=CARTESIAN_POINT('Ctrl Pts',(-9.59371524400376,13.0797021484572,
12.1054536448283));
#124140=CARTESIAN_POINT('Ctrl Pts',(-9.5936473296044,13.0797070415638,12.105428682033));
#124141=CARTESIAN_POINT('Ctrl Pts',(-9.59361350472327,13.079709478537,12.1054162475083));
#124142=CARTESIAN_POINT('Ctrl Pts',(-9.59354610876972,13.0797143341044,
12.1053914682515));
#124143=CARTESIAN_POINT('Ctrl Pts',(-9.59351253768661,13.0797167527,12.1053791235415));
#124144=CARTESIAN_POINT('Ctrl Pts',(-9.59344563858582,13.0797215722883,
12.1053545200415));
#124145=CARTESIAN_POINT('Ctrl Pts',(-9.59341231062789,13.0797239732773,
12.1053422612983));
#124146=CARTESIAN_POINT('Ctrl Pts',(-9.58921791840261,13.0800261370001,
12.1037992578247));
#124147=CARTESIAN_POINT('Ctrl Pts',(-9.58506544934563,13.0803245754349,
12.1022450001442));
#124148=CARTESIAN_POINT('Ctrl Pts',(-9.57608135998949,13.080968935501,12.098824315061));
#124149=CARTESIAN_POINT('Ctrl Pts',(-9.57125305169878,13.0813143959228,
12.0969493813793));
#124150=CARTESIAN_POINT('Ctrl Pts',(-9.55813539709362,13.082251073329,12.0917556771422));
#124151=CARTESIAN_POINT('Ctrl Pts',(-9.54987100242236,13.0828391468118,
12.0883743297964));
#124152=CARTESIAN_POINT('Ctrl Pts',(-9.52344263340581,13.0847155577068,
12.0772087218396));
#124153=CARTESIAN_POINT('Ctrl Pts',(-9.5054350839105,13.0859877329996,12.0690608886513));
#124154=CARTESIAN_POINT('Ctrl Pts',(-9.43704259549868,13.090825989417,12.0360172524376));
#124155=CARTESIAN_POINT('Ctrl Pts',(-9.3882567168026,13.0942940031834,12.0079799832356));
#124156=CARTESIAN_POINT('Ctrl Pts',(-9.28734593884398,13.1018644397697,
11.9399518461945));
#124157=CARTESIAN_POINT('Ctrl Pts',(-9.23618980821173,13.1059669657346,
11.8988759157088));
#124158=CARTESIAN_POINT('Ctrl Pts',(-9.17721209272348,13.1112682655371,
11.8428326955974));
#124159=CARTESIAN_POINT('Ctrl Pts',(-9.1659309224605,13.1123109135151,11.8316703849429));
#124160=CARTESIAN_POINT('Ctrl Pts',(-9.14947191171068,13.113877940139,11.8147130211893));
#124161=CARTESIAN_POINT('Ctrl Pts',(-9.14412001994672,13.1143949943733,
11.809088864643));
#124162=CARTESIAN_POINT('Ctrl Pts',(-9.13462853193339,13.115325853258,11.7989149609325));
#124163=CARTESIAN_POINT('Ctrl Pts',(-9.13046820053756,13.1157387788329,
11.7943848814441));
#124164=CARTESIAN_POINT('Ctrl Pts',(-9.12168918886093,13.1166207972181,
11.7846740416978));
#124165=CARTESIAN_POINT('Ctrl Pts',(-9.11708045681241,13.1170902739214,
11.7794846434893));
#124166=CARTESIAN_POINT('Ctrl Pts',(-9.10473320934241,13.1183658661476,
11.765331732753));
#124167=CARTESIAN_POINT('Ctrl Pts',(-9.09708374848399,13.1191754995966,
11.7562919494934));
#124168=CARTESIAN_POINT('Ctrl Pts',(-9.05413802577621,13.1238352859139,
11.7039603190058));
#124169=CARTESIAN_POINT('Ctrl Pts',(-9.02182575853436,13.1277995076865,
11.6583224945081));
#124170=CARTESIAN_POINT('Ctrl Pts',(-8.94984959361929,13.1378578414956,
11.5395993327016));
#124171=CARTESIAN_POINT('Ctrl Pts',(-8.91445128966916,13.1440331934835,
11.4642915797605));
#124172=CARTESIAN_POINT('Ctrl Pts',(-8.88725970493321,13.1500000000001,
11.3858809379001));
#124173=CARTESIAN_POINT('',(-9.99063336962942,13.15,12.1777127530665));
#124174=CARTESIAN_POINT('Origin',(-10.,13.15,11.));
#124175=CARTESIAN_POINT('',(-11.1772954272628,13.0251562212751,10.9995934172276));
#124176=CARTESIAN_POINT('Ctrl Pts',(-11.1777499234177,13.0254177721281,
10.999575277046));
#124177=CARTESIAN_POINT('Ctrl Pts',(-11.1777577176107,13.0269365486979,
11.0211884488591));
#124178=CARTESIAN_POINT('Ctrl Pts',(-11.1771705716744,13.0284370553205,
11.0427989728332));
#124179=CARTESIAN_POINT('Ctrl Pts',(-11.1755995648328,13.0304066396755,
11.0714944569654));
#124180=CARTESIAN_POINT('Ctrl Pts',(-11.1751456864787,13.0308926866991,
11.0786028869611));
#124181=CARTESIAN_POINT('Ctrl Pts',(-11.174225909971,13.0317514363242,11.0912085761244));
#124182=CARTESIAN_POINT('Ctrl Pts',(-11.1737858258318,13.0321249660324,
11.0967074400733));
#124183=CARTESIAN_POINT('Ctrl Pts',(-11.1728329683863,13.0328659682834,
11.107646388824));
#124184=CARTESIAN_POINT('Ctrl Pts',(-11.1723209395147,13.0332334553756,
11.1130863977106));
#124185=CARTESIAN_POINT('Ctrl Pts',(-11.1711460135807,13.0340160535254,
11.1247022642352));
#124186=CARTESIAN_POINT('Ctrl Pts',(-11.1704720799956,13.034430794186,11.130876859675));
#124187=CARTESIAN_POINT('Ctrl Pts',(-11.1685775147471,13.0355138608371,
11.1470478341186));
#124188=CARTESIAN_POINT('Ctrl Pts',(-11.1672774464124,13.0361795957087,
11.1570345419591));
#124189=CARTESIAN_POINT('Ctrl Pts',(-11.1611175719878,13.0390342259051,
11.2000365202171));
#124190=CARTESIAN_POINT('Ctrl Pts',(-11.1549836689483,13.0411817482987,
11.2328554899879));
#124191=CARTESIAN_POINT('Ctrl Pts',(-11.1334691257893,13.0472321972448,
11.3258838813155));
#124192=CARTESIAN_POINT('Ctrl Pts',(-11.1147099243551,13.0510399841972,
11.3851946694449));
#124193=CARTESIAN_POINT('Ctrl Pts',(-11.0656545921376,13.0590870149611,
11.5061133897456));
#124194=CARTESIAN_POINT('Ctrl Pts',(-11.0344844859888,13.0633170379455,
11.5671061022227));
#124195=CARTESIAN_POINT('Ctrl Pts',(-10.9942855312569,13.0683399983489,
11.6313049735448));
#124196=CARTESIAN_POINT('Ctrl Pts',(-10.990304398483,13.0688335867455,11.637531864601));
#124197=CARTESIAN_POINT('Ctrl Pts',(-10.984152320596,13.06959123457,11.6469576602496));
#124198=CARTESIAN_POINT('Ctrl Pts',(-10.9820236867026,13.0698524824746,
11.6501841912838));
#124199=CARTESIAN_POINT('Ctrl Pts',(-10.9780246286169,13.0703417300501,
11.6561814254742));
#124200=CARTESIAN_POINT('Ctrl Pts',(-10.9761582423722,13.0705694354109,
11.6589547195682));
#124201=CARTESIAN_POINT('Ctrl Pts',(-10.9718988496437,13.0710876144093,
11.6652260151153));
#124202=CARTESIAN_POINT('Ctrl Pts',(-10.9694987328802,13.0713785587402,
11.6687190969701));
#124203=CARTESIAN_POINT('Ctrl Pts',(-10.9632425751771,13.0721341151097,
11.6777197105089));
#124204=CARTESIAN_POINT('Ctrl Pts',(-10.9593581969249,13.0726005079692,
11.6832072228588));
#124205=CARTESIAN_POINT('Ctrl Pts',(-10.9322789708401,13.0758318407849,
11.7207761103104));
#124206=CARTESIAN_POINT('Ctrl Pts',(-10.9075287698814,13.0786849341472,
11.7517001383513));
#124207=CARTESIAN_POINT('Ctrl Pts',(-10.8647875565658,13.0833933198988,
11.7999093719809));
#124208=CARTESIAN_POINT('Ctrl Pts',(-10.8477190946205,13.0852238242874,
11.8179760349368));
#124209=CARTESIAN_POINT('Ctrl Pts',(-10.7858840212843,13.0916585834664,
11.8794117228298));
#124210=CARTESIAN_POINT('Ctrl Pts',(-10.7382556912384,13.0962672086525,
11.9197599180347));
#124211=CARTESIAN_POINT('Ctrl Pts',(-10.6468884894268,13.104398508784,11.9854703978618));
#124212=CARTESIAN_POINT('Ctrl Pts',(-10.6042839821358,13.1079515380481,
12.0121554677843));
#124213=CARTESIAN_POINT('Ctrl Pts',(-10.5489750712035,13.1122853104622,
12.0420563217255));
#124214=CARTESIAN_POINT('Ctrl Pts',(-10.5377533754489,13.1131511732929,
12.0478913749513));
#124215=CARTESIAN_POINT('Ctrl Pts',(-10.5197333915153,13.1145211530228,
12.056895673695));
#124216=CARTESIAN_POINT('Ctrl Pts',(-10.5129953123566,13.1150289509163,
12.0601825677283));
#124217=CARTESIAN_POINT('Ctrl Pts',(-10.5007775373901,13.1159419089311,
12.0659987504876));
#124218=CARTESIAN_POINT('Ctrl Pts',(-10.4953089596567,13.1163477538018,
12.0685506607345));
#124219=CARTESIAN_POINT('Ctrl Pts',(-10.4823365812577,13.1173040935237,
12.0744832319354));
#124220=CARTESIAN_POINT('Ctrl Pts',(-10.4748164242994,13.1178534762734,
12.0778275194227));
#124221=CARTESIAN_POINT('Ctrl Pts',(-10.4523443503552,13.1194809504437,
12.0875402281599));
#124222=CARTESIAN_POINT('Ctrl Pts',(-10.4372946874503,13.1205523055852,
12.0936784496696));
#124223=CARTESIAN_POINT('Ctrl Pts',(-10.3584839054224,13.1260769780107,
12.1239355510394));
#124224=CARTESIAN_POINT('Ctrl Pts',(-10.292842380685,13.1303824394693,12.142797549714));
#124225=CARTESIAN_POINT('Ctrl Pts',(-10.1648024768581,13.1386305765498,
12.1678248973038));
#124226=CARTESIAN_POINT('Ctrl Pts',(-10.1028253210713,13.1425625675842,
12.1749044100269));
#124227=CARTESIAN_POINT('Ctrl Pts',(-10.0311209417352,13.1472915530833,
12.1773768473046));
#124228=CARTESIAN_POINT('Ctrl Pts',(-10.0216527151898,13.1479196453913,
12.1775890212404));
#124229=CARTESIAN_POINT('Ctrl Pts',(-10.0082480130816,13.1488151762712,
12.1777276936811));
#124230=CARTESIAN_POINT('Ctrl Pts',(-10.0043126586523,13.1490788555009,
12.1777486787568));
#124231=CARTESIAN_POINT('Ctrl Pts',(-9.9971259392377,13.1495618946493,12.1777509812338));
#124232=CARTESIAN_POINT('Ctrl Pts',(-9.99388457723913,13.1497803175007,
12.1777386106959));
#124233=CARTESIAN_POINT('Ctrl Pts',(-9.99063336962942,13.15,12.1777127530665));
#124234=CARTESIAN_POINT('Ctrl Pts',(-9.81116440461326,12.8870115174245,
9.83777311283111));
#124235=CARTESIAN_POINT('Ctrl Pts',(-9.85764179083828,12.8900321853929,
9.83013029488514));
#124236=CARTESIAN_POINT('Ctrl Pts',(-9.90455116173817,12.8930103398809,
9.82526020590206));
#124237=CARTESIAN_POINT('Ctrl Pts',(-9.9515353357889,12.8959892278449,9.82321108761683));
#124238=CARTESIAN_POINT('Ctrl Pts',(-9.99860896525469,12.8989737874562,
9.82115806791735));
#124239=CARTESIAN_POINT('Ctrl Pts',(-10.045757547291,12.9019596135139,9.82193735631773));
#124240=CARTESIAN_POINT('Ctrl Pts',(-10.092609471857,12.9050053361438,9.8255527815257));
#124241=CARTESIAN_POINT('Ctrl Pts',(-10.1291483434982,12.9073806338346,
9.82837237877439));
#124242=CARTESIAN_POINT('Ctrl Pts',(-10.1655064318549,12.9097928264916,
9.83291619779872));
#124243=CARTESIAN_POINT('Ctrl Pts',(-10.2015038000959,12.912272145452,9.83916325637052));
#124244=CARTESIAN_POINT('Ctrl Pts',(-10.2015210427633,12.9122733330409,
9.83916624869909));
#124245=CARTESIAN_POINT('Ctrl Pts',(-10.2015382853485,12.9122745206451,
9.83916924141816));
#124246=CARTESIAN_POINT('Ctrl Pts',(-10.2015555278514,12.9122757082647,
9.83917223452772));
#124247=CARTESIAN_POINT('Ctrl Pts',(-10.2442282194276,12.9152148944474,
9.84657974618454));
#124248=CARTESIAN_POINT('Ctrl Pts',(-10.2865568592501,12.9182562844301,
9.85641454158234));
#124249=CARTESIAN_POINT('Ctrl Pts',(-10.3282607259639,12.9213410703907,
9.86859966612906));
#124250=CARTESIAN_POINT('Ctrl Pts',(-10.3332038360598,12.9217067064295,
9.87004395455871));
#124251=CARTESIAN_POINT('Ctrl Pts',(-10.3381381277854,12.9220729521418,
9.87152121879118));
#124252=CARTESIAN_POINT('Ctrl Pts',(-10.3430631019052,12.9224397095998,
9.87303129417658));
#124253=CARTESIAN_POINT('Ctrl Pts',(-10.3879237399555,12.925780432449,9.88678627920702));
#124254=CARTESIAN_POINT('Ctrl Pts',(-10.4320158733059,12.9291630655903,
9.90326743373218));
#124255=CARTESIAN_POINT('Ctrl Pts',(-10.4750087718731,12.9325288967133,
9.92233712650969));
#124256=CARTESIAN_POINT('Ctrl Pts',(-10.5179599024573,12.9358914579015,
9.9413882929112));
#124257=CARTESIAN_POINT('Ctrl Pts',(-10.5598141289736,12.9392369577166,
9.96302272516638));
#124258=CARTESIAN_POINT('Ctrl Pts',(-10.6002628671917,12.9425285565809,
9.98707213673965));
#124259=CARTESIAN_POINT('Ctrl Pts',(-10.6406899655252,12.9458183944553,
10.011108681991));
#124260=CARTESIAN_POINT('Ctrl Pts',(-10.6797131310047,12.9490542995934,
10.0375575726317));
#124261=CARTESIAN_POINT('Ctrl Pts',(-10.7170435689573,12.9522239589476,
10.0662218540858));
#124262=CARTESIAN_POINT('Ctrl Pts',(-10.7543703291871,12.955393306033,10.09488331159));
#124263=CARTESIAN_POINT('Ctrl Pts',(-10.7900046053942,12.9584964779604,
10.1257597863454));
#124264=CARTESIAN_POINT('Ctrl Pts',(-10.8236772833654,12.9615458522909,
10.1586253022285));
#124265=CARTESIAN_POINT('Ctrl Pts',(-10.8573843173583,12.9645983378788,
10.1915243505907));
#124266=CARTESIAN_POINT('Ctrl Pts',(-10.8891255088694,12.967597123764,10.2264166559677));
#124267=CARTESIAN_POINT('Ctrl Pts',(-10.9186530064052,12.970577413428,10.2630447536762));
#124268=CARTESIAN_POINT('Ctrl Pts',(-10.9481986928991,12.9735595389524,
10.2996954143172));
#124269=CARTESIAN_POINT('Ctrl Pts',(-10.9755275164772,12.9765235663849,
10.3380842168579));
#124270=CARTESIAN_POINT('Ctrl Pts',(-11.0004182904618,12.9795229212538,
10.3779196065224));
#124271=CARTESIAN_POINT('Ctrl Pts',(-11.0233446274457,12.9822855601536,
10.4146110958227));
#124272=CARTESIAN_POINT('Ctrl Pts',(-11.0442026173884,12.9850787708026,
10.4525303703702));
#124273=CARTESIAN_POINT('Ctrl Pts',(-11.0628454756567,12.987951913143,10.4914199788974));
#124274=CARTESIAN_POINT('Ctrl Pts',(-11.0644790954582,12.9882036783043,
10.4948277629212));
#124275=CARTESIAN_POINT('Ctrl Pts',(-11.0660957352143,12.988456057222,10.498243013967));
#124276=CARTESIAN_POINT('Ctrl Pts',(-11.067695312561,12.9887090831076,10.5016655686762));
#124277=CARTESIAN_POINT('Ctrl Pts',(-11.0727371756071,12.9895066199477,
10.5124534509552));
#124278=CARTESIAN_POINT('Ctrl Pts',(-11.0776094005779,12.9903106007719,
10.5233135115653));
#124279=CARTESIAN_POINT('Ctrl Pts',(-11.0823094096359,12.9911220678411,
10.5342399661854));
#124280=CARTESIAN_POINT('Ctrl Pts',(-11.0823175711111,12.991123476938,10.5342589397633));
#124281=CARTESIAN_POINT('Ctrl Pts',(-11.082325732067,12.9911248860575,10.5342779135414));
#124282=CARTESIAN_POINT('Ctrl Pts',(-11.0823338925038,12.9911262951996,
10.5342968875198));
#124283=CARTESIAN_POINT('Ctrl Pts',(-11.0999253299888,12.9941639800148,
10.5751990553205));
#124284=CARTESIAN_POINT('Ctrl Pts',(-11.1151555993952,12.9973132986395,
10.6171683939075));
#124285=CARTESIAN_POINT('Ctrl Pts',(-11.1279453099112,13.0005094500513,
10.6599293048586));
#124286=CARTESIAN_POINT('Ctrl Pts',(-11.1298768953495,13.0009921536683,
10.666387336322));
#124287=CARTESIAN_POINT('Ctrl Pts',(-11.1317528145371,13.0014759254947,
10.6728633258445));
#124288=CARTESIAN_POINT('Ctrl Pts',(-11.1335727985327,13.0019605423062,
10.6793562208813));
#124289=CARTESIAN_POINT('Ctrl Pts',(-11.1465529134116,13.0054168264831,
10.7256635091205));
#124290=CARTESIAN_POINT('Ctrl Pts',(-11.1566880602086,13.008915125034,10.7728364981445));
#124291=CARTESIAN_POINT('Ctrl Pts',(-11.1639147879019,13.0123938753952,
10.8205348651852));
#124292=CARTESIAN_POINT('Ctrl Pts',(-11.1647785754975,13.0128096792746,
10.8262360980981));
#124293=CARTESIAN_POINT('Ctrl Pts',(-11.1656007929283,13.0132252038757,
10.8319447785655));
#124294=CARTESIAN_POINT('Ctrl Pts',(-11.1663813188882,13.0136403440721,
10.837660277284));
#124295=CARTESIAN_POINT('Ctrl Pts',(-11.1732971651245,13.0173186916377,
10.8883024241616));
#124296=CARTESIAN_POINT('Ctrl Pts',(-11.1769423028602,13.020966755683,10.9394862387593));
#124297=CARTESIAN_POINT('Ctrl Pts',(-11.1772703118677,13.0245435525335,
10.9908036332495));
#124298=CARTESIAN_POINT('Ctrl Pts',(-11.1772890367999,13.0247477398476,
10.9937331708732));
#124299=CARTESIAN_POINT('Ctrl Pts',(-11.1772969587745,13.024951704152,10.9966631424074));
#124300=CARTESIAN_POINT('Ctrl Pts',(-11.1772940717528,13.0251554412139,
10.9995934713297));
#124301=CARTESIAN_POINT('Origin',(-10.,3.5,11.));
#124302=CARTESIAN_POINT('',(-11.288874705773,13.1492342550778,10.3059746432093));
#124303=CARTESIAN_POINT('Ctrl Pts',(-11.463991763927,12.6884918210949,10.9993887619195));
#124304=CARTESIAN_POINT('Ctrl Pts',(-11.4639306072661,12.6916694228865,
11.0548606201258));
#124305=CARTESIAN_POINT('Ctrl Pts',(-11.4606650012394,12.6949287056907,
11.1104413929884));
#124306=CARTESIAN_POINT('Ctrl Pts',(-11.4542247554779,12.6981982648876,
11.1657358244845));
#124307=CARTESIAN_POINT('Ctrl Pts',(-11.4479113119717,12.7014034496033,
11.2199415617167));
#124308=CARTESIAN_POINT('Ctrl Pts',(-11.4385475454018,12.70461814771,11.273872221106));
#124309=CARTESIAN_POINT('Ctrl Pts',(-11.4262011123443,12.7077927824406,
11.3271678981243));
#124310=CARTESIAN_POINT('Ctrl Pts',(-11.4138654318444,12.7109646523692,
11.3804171597257));
#124311=CARTESIAN_POINT('Ctrl Pts',(-11.3985524523269,12.7140963374362,
11.4330325782745));
#124312=CARTESIAN_POINT('Ctrl Pts',(-11.3803645690148,12.7171603245914,
11.4846667322799));
#124313=CARTESIAN_POINT('Ctrl Pts',(-11.3621849539508,12.720222918852,11.536277413296));
#124314=CARTESIAN_POINT('Ctrl Pts',(-11.3411330761592,12.7232178336545,
11.5869076790711));
#124315=CARTESIAN_POINT('Ctrl Pts',(-11.3173446373055,12.7261412311667,
11.6362221723392));
#124316=CARTESIAN_POINT('Ctrl Pts',(-11.2926743352398,12.7291730021933,
11.6873648073233));
#124317=CARTESIAN_POINT('Ctrl Pts',(-11.2650604962163,12.7321277902365,
11.7370920766566));
#124318=CARTESIAN_POINT('Ctrl Pts',(-11.2346929672173,12.7350278368395,
11.7850445538785));
#124319=CARTESIAN_POINT('Ctrl Pts',(-11.2053818388839,12.7378269990023,
11.8313288996941));
#124320=CARTESIAN_POINT('Ctrl Pts',(-11.1735053054335,12.7405755318138,
11.8759596398189));
#124321=CARTESIAN_POINT('Ctrl Pts',(-11.1392707220035,12.7433149314186,
11.9186294430486));
#124322=CARTESIAN_POINT('Ctrl Pts',(-11.1050138117042,12.7460561175857,
11.9613270743697));
#124323=CARTESIAN_POINT('Ctrl Pts',(-11.0683955094785,12.7487885838883,
12.002060812035));
#124324=CARTESIAN_POINT('Ctrl Pts',(-11.0296630300884,12.7515701670991,
12.0405429981061));
#124325=CARTESIAN_POINT('Ctrl Pts',(-10.994277032835,12.7541114218137,12.0757003273569));
#124326=CARTESIAN_POINT('Ctrl Pts',(-10.9571259891997,12.7566942402975,
12.1089786558575));
#124327=CARTESIAN_POINT('Ctrl Pts',(-10.9184321226944,12.7593688259845,
12.1401776686378));
#124328=CARTESIAN_POINT('Ctrl Pts',(-10.9147017991821,12.7596266722732,
12.1431854427748));
#124329=CARTESIAN_POINT('Ctrl Pts',(-10.9109571274964,12.7598853714582,
12.1461739305206));
#124330=CARTESIAN_POINT('Ctrl Pts',(-10.9071983003763,12.7601449685223,
12.1491429772846));
#124331=CARTESIAN_POINT('Ctrl Pts',(-10.9027286881088,12.7604536547654,
12.1526734636345));
#124332=CARTESIAN_POINT('Ctrl Pts',(-10.8982391177638,12.7607636118325,
12.1561764266014));
#124333=CARTESIAN_POINT('Ctrl Pts',(-10.8937299523839,12.7610749150924,
12.1596515912169));
#124334=CARTESIAN_POINT('Ctrl Pts',(-10.8937152925033,12.7610759271796,
12.1596628894271));
#124335=CARTESIAN_POINT('Ctrl Pts',(-10.8937006324156,12.7610769392811,
12.1596741873435));
#124336=CARTESIAN_POINT('Ctrl Pts',(-10.8936859721208,12.7610779513968,
12.1596854849661));
#124337=CARTESIAN_POINT('Ctrl Pts',(-10.8537499481008,12.763835049828,12.1904612730685));
#124338=CARTESIAN_POINT('Ctrl Pts',(-10.8121129634155,12.7667055672991,
12.219173400463));
#124339=CARTESIAN_POINT('Ctrl Pts',(-10.7690278434298,12.7696293657161,
12.2456599611385));
#124340=CARTESIAN_POINT('Ctrl Pts',(-10.7650618919684,12.7698984990644,
12.2480980282497));
#124341=CARTESIAN_POINT('Ctrl Pts',(-10.761083706844,12.7701680838652,12.2505172388233));
#124342=CARTESIAN_POINT('Ctrl Pts',(-10.7570935073437,12.7704380732146,
12.2529174676517));
#124343=CARTESIAN_POINT('Ctrl Pts',(-10.7098389494908,12.7736354640544,
12.2813425506649));
#124344=CARTESIAN_POINT('Ctrl Pts',(-10.6608936219115,12.7768889670954,
12.3071058356523));
#124345=CARTESIAN_POINT('Ctrl Pts',(-10.6105997122338,12.7801339179107,
12.3300427880688));
#124346=CARTESIAN_POINT('Ctrl Pts',(-10.5603556027551,12.7833756556294,
12.3529570286937));
#124347=CARTESIAN_POINT('Ctrl Pts',(-10.5087656730358,12.7866085236495,
12.3730508776882));
#124348=CARTESIAN_POINT('Ctrl Pts',(-10.4561797286586,12.7897883683785,
12.3901984627458));
#124349=CARTESIAN_POINT('Ctrl Pts',(-10.4036251100483,12.7929663188546,
12.4073358328828));
#124350=CARTESIAN_POINT('Ctrl Pts',(-10.3500756848916,12.7960911734393,
12.4215305799771));
#124351=CARTESIAN_POINT('Ctrl Pts',(-10.2958885096565,12.7991426090625,
12.4326916658829));
#124352=CARTESIAN_POINT('Ctrl Pts',(-10.2417122397385,12.802193430576,12.4438505055896));
#124353=CARTESIAN_POINT('Ctrl Pts',(-10.1868984941038,12.8051708661675,
12.4519768687009));
#124354=CARTESIAN_POINT('Ctrl Pts',(-10.1318117243294,12.8080793134399,
12.4570137059567));
#124355=CARTESIAN_POINT('Ctrl Pts',(-10.0766746164422,12.8109904184421,
12.4620551458582));
#124356=CARTESIAN_POINT('Ctrl Pts',(-10.0212640174713,12.8138325374196,
12.4640012238705));
#124357=CARTESIAN_POINT('Ctrl Pts',(-9.96595264511685,12.8166338655913,
12.462830420146));
#124358=CARTESIAN_POINT('Ctrl Pts',(-9.91061622684647,12.8194364622514,
12.461659086262));
#124359=CARTESIAN_POINT('Ctrl Pts',(-9.85537920337594,12.8221985245844,
12.4573677032184));
#124360=CARTESIAN_POINT('Ctrl Pts',(-9.80062128797522,12.8249689650342,
12.4499743785991));
#124361=CARTESIAN_POINT('Ctrl Pts',(-9.74576049243588,12.8277446106364,
12.4425671632709));
#124362=CARTESIAN_POINT('Ctrl Pts',(-9.69138082321311,12.8305291858514,
12.4320458028768));
#124363=CARTESIAN_POINT('Ctrl Pts',(-9.63786857487717,12.8333866006413,
12.4184749302969));
#124364=CARTESIAN_POINT('Ctrl Pts',(-9.59715191586502,12.8355607642632,
12.4081490589587));
#124365=CARTESIAN_POINT('Ctrl Pts',(-9.55693763547138,12.8377775238315,
12.3960585411452));
#124366=CARTESIAN_POINT('Ctrl Pts',(-9.5173957676152,12.8400672357347,12.3822530440279));
#124367=CARTESIAN_POINT('Ctrl Pts',(-9.51737844909782,12.840068238581,12.3822469975067));
#124368=CARTESIAN_POINT('Ctrl Pts',(-9.51736113070901,12.8400692414413,
12.3822409506567));
#124369=CARTESIAN_POINT('Ctrl Pts',(-9.51734381244877,12.8400702443156,
12.3822349034779));
#124370=CARTESIAN_POINT('Ctrl Pts',(-9.46970834541888,12.8428287422249,
12.3656015821447));
#124371=CARTESIAN_POINT('Ctrl Pts',(-9.42287266454677,12.8457003959102,
12.3464124368936));
#124372=CARTESIAN_POINT('Ctrl Pts',(-9.37711103475015,12.8486249916029,
12.3247909965804));
#124373=CARTESIAN_POINT('Ctrl Pts',(-9.3729300008179,12.8488921987343,12.322815542996));
#124374=CARTESIAN_POINT('Ctrl Pts',(-9.36875795172639,12.8491598478073,
12.3208198159464));
#124375=CARTESIAN_POINT('Ctrl Pts',(-9.36459510762443,12.8494278928976,
12.3188039282783));
#124376=CARTESIAN_POINT('Ctrl Pts',(-9.31495778950907,12.852624034547,12.2947666943536));
#124377=CARTESIAN_POINT('Ctrl Pts',(-9.26662576689027,12.8558758586289,
12.2678584206617));
#124378=CARTESIAN_POINT('Ctrl Pts',(-9.21992386854803,12.8591188273359,
12.2382757540587));
#124379=CARTESIAN_POINT('Ctrl Pts',(-9.17326800766399,12.8623585992128,
12.2087222492419));
#124380=CARTESIAN_POINT('Ctrl Pts',(-9.12823881971626,12.8655892004004,
12.1764998869579));
#124381=CARTESIAN_POINT('Ctrl Pts',(-9.08513296385328,12.8687666544394,
12.1418328127599));
#124382=CARTESIAN_POINT('Ctrl Pts',(-9.04205260528417,12.8719422290011,
12.1071862442812));
#124383=CARTESIAN_POINT('Ctrl Pts',(-9.00089320646608,12.8750645846866,
12.0700979443509));
#124384=CARTESIAN_POINT('Ctrl Pts',(-8.96192625110391,12.8781136056907,
12.0308171767114));
#124385=CARTESIAN_POINT('Ctrl Pts',(-8.92296698235448,12.8811620252457,
11.9915441575871));
#124386=CARTESIAN_POINT('Ctrl Pts',(-8.88619933293799,12.8841371435309,
11.9500795295694));
#124387=CARTESIAN_POINT('Ctrl Pts',(-8.85187038717562,12.8870435803164,
11.9066973488058));
#124388=CARTESIAN_POINT('Ctrl Pts',(-8.81750988950394,12.8899526884228,
11.8632752952583));
#124389=CARTESIAN_POINT('Ctrl Pts',(-8.78559275552825,12.8927931183539,
11.8179320859967));
#124390=CARTESIAN_POINT('Ctrl Pts',(-8.75634084620763,12.8955932876637,
11.7709681597297));
#124391=CARTESIAN_POINT('Ctrl Pts',(-8.72707560095911,12.8983947335689,
11.7239828226369));
#124392=CARTESIAN_POINT('Ctrl Pts',(-8.70047834350937,12.9011561774023,
11.6753751666226));
#124393=CARTESIAN_POINT('Ctrl Pts',(-8.67674156563753,12.9039267316423,
11.6254732072825));
#124394=CARTESIAN_POINT('Ctrl Pts',(-8.65296010294484,12.9067025014898,
11.5754773067965));
#124395=CARTESIAN_POINT('Ctrl Pts',(-8.63205046998966,12.9094879388544,
11.524182112466));
#124396=CARTESIAN_POINT('Ctrl Pts',(-8.61416975518133,12.9123470979137,
11.4719466581655));
#124397=CARTESIAN_POINT('Ctrl Pts',(-8.6005777153295,12.9145204899896,11.4322398352481));
#124398=CARTESIAN_POINT('Ctrl Pts',(-8.5887352577041,12.9167369048377,11.3919903307576));
#124399=CARTESIAN_POINT('Ctrl Pts',(-8.57869358592355,12.9190266353551,
11.3513673085708));
#124400=CARTESIAN_POINT('Ctrl Pts',(-8.57868907329069,12.9190276643385,
11.3513490529667));
#124401=CARTESIAN_POINT('Ctrl Pts',(-8.57868456102113,12.9190286933367,
11.3513307972868));
#124402=CARTESIAN_POINT('Ctrl Pts',(-8.57868004911485,12.9190297223496,
11.3513125415313));
#124403=CARTESIAN_POINT('Ctrl Pts',(-8.56660070253902,12.9217846121045,
11.3024379451385));
#124404=CARTESIAN_POINT('Ctrl Pts',(-8.55708741400778,12.924652975869,11.2528372813682));
#124405=CARTESIAN_POINT('Ctrl Pts',(-8.55018686238138,12.9275746380525,
11.2028063462097));
#124406=CARTESIAN_POINT('Ctrl Pts',(-8.54955230728425,12.9278433057955,
11.1982056437386));
#124407=CARTESIAN_POINT('Ctrl Pts',(-8.54893983039631,12.9281124242362,
11.193601335831));
#124408=CARTESIAN_POINT('Ctrl Pts',(-8.54834945817009,12.9283819465821,
11.1889936722351));
#124409=CARTESIAN_POINT('Ctrl Pts',(-8.54135148776675,12.9315767266135,
11.1343767847181));
#124410=CARTESIAN_POINT('Ctrl Pts',(-8.53746133071862,12.9348276337055,
11.0792829802226));
#124411=CARTESIAN_POINT('Ctrl Pts',(-8.53669217238271,12.9380699468489,
11.0240906774086));
#124412=CARTESIAN_POINT('Ctrl Pts',(-8.53592377559064,12.9413090497774,
10.9689530205062));
#124413=CARTESIAN_POINT('Ctrl Pts',(-8.53826984716269,12.944539241719,10.9137170085431));
#124414=CARTESIAN_POINT('Ctrl Pts',(-8.54370509600633,12.9477162716722,
10.8587525388433));
#124415=CARTESIAN_POINT('Ctrl Pts',(-8.54913712565265,12.9508914199293,
10.8038206235819));
#124416=CARTESIAN_POINT('Ctrl Pts',(-8.55765454448063,12.9540133329836,
10.7491598992555));
#124417=CARTESIAN_POINT('Ctrl Pts',(-8.5691972312881,12.9570615499469,10.6951329001681));
#124418=CARTESIAN_POINT('Ctrl Pts',(-8.5807376732402,12.9601091740841,10.641116408409));
#124419=CARTESIAN_POINT('Ctrl Pts',(-8.5953022305721,12.963083133139,10.5877334291422));
#124420=CARTESIAN_POINT('Ctrl Pts',(-8.61279668643374,12.9659876583311,
10.5353395611747));
#124421=CARTESIAN_POINT('Ctrl Pts',(-8.63030756142934,12.9688949095176,
10.4828965198037));
#124422=CARTESIAN_POINT('Ctrl Pts',(-8.65075399173112,12.9717327226785,
10.4314445539024));
#124423=CARTESIAN_POINT('Ctrl Pts',(-8.67400594107476,12.9745291241955,
10.3813324828995));
#124424=CARTESIAN_POINT('Ctrl Pts',(-8.69726867948781,12.9773268232626,
10.3311971595401));
#124425=CARTESIAN_POINT('Ctrl Pts',(-8.72333981954434,12.9800833620599,
10.2824031845639));
#124426=CARTESIAN_POINT('Ctrl Pts',(-8.7520503332962,12.9828475259031,10.235289759722));
#124427=CARTESIAN_POINT('Ctrl Pts',(-8.78081591254253,12.9856169912902,
10.1880859734167));
#124428=CARTESIAN_POINT('Ctrl Pts',(-8.81223139921618,12.9883946255454,
10.1425695998377));
#124429=CARTESIAN_POINT('Ctrl Pts',(-8.84608268313027,12.99124432723,10.0990671209387));
#124430=CARTESIAN_POINT('Ctrl Pts',(-8.87230015811641,12.9934513921916,
10.0653748936287));
#124431=CARTESIAN_POINT('Ctrl Pts',(-8.89997787675521,12.9957021291343,
10.0328905194451));
#124432=CARTESIAN_POINT('Ctrl Pts',(-8.92899589006904,12.9980286231998,
10.0017564676114));
#124433=CARTESIAN_POINT('Ctrl Pts',(-8.9290084654359,12.9980296314189,10.0017429752293));
#124434=CARTESIAN_POINT('Ctrl Pts',(-8.92902104105451,12.9980306396523,
10.0017294831003));
#124435=CARTESIAN_POINT('Ctrl Pts',(-8.92903361692483,12.9980316478999,
10.0017159912244));
#124436=CARTESIAN_POINT('Ctrl Pts',(-8.96342523601557,13.0007889335873,
9.96481934371385));
#124437=CARTESIAN_POINT('Ctrl Pts',(-8.99983258448837,13.0036599961189,
9.92968370963538));
#124438=CARTESIAN_POINT('Ctrl Pts',(-9.03803252860992,13.0065848607624,
9.89650983373753));
#124439=CARTESIAN_POINT('Ctrl Pts',(-9.04159484639477,13.0068576176362,
9.89341621957601));
#124440=CARTESIAN_POINT('Ctrl Pts',(-9.04517271624349,13.0071308423951,
9.89033967081621));
#124441=CARTESIAN_POINT('Ctrl Pts',(-9.04876593431357,13.0074044864008,
9.88728035283533));
#124442=CARTESIAN_POINT('Ctrl Pts',(-9.09081513479617,13.0106067723269,
9.85147905366303));
#124443=CARTESIAN_POINT('Ctrl Pts',(-9.13497186781783,13.0138658422133,
9.81803614812968));
#124444=CARTESIAN_POINT('Ctrl Pts',(-9.18092427701071,13.0171168896996,
9.78717016845008));
#124445=CARTESIAN_POINT('Ctrl Pts',(-9.22683084803429,13.0203646942206,
9.75633497801586));
#124446=CARTESIAN_POINT('Ctrl Pts',(-9.27452936708117,13.0236041548999,
9.72807124327942));
#124447=CARTESIAN_POINT('Ctrl Pts',(-9.3236942342042,13.0267909395546,9.70256050116778));
#124448=CARTESIAN_POINT('Ctrl Pts',(-9.37282928121454,13.0299757913194,
9.67706523216223));
#124449=CARTESIAN_POINT('Ctrl Pts',(-9.42342885733123,13.033107893756,9.65431948756656));
#124450=CARTESIAN_POINT('Ctrl Pts',(-9.47515458758201,13.0361667410128,
9.63447158781853));
#124451=CARTESIAN_POINT('Ctrl Pts',(-9.52686916668666,13.0392249288365,
9.61462796692417));
#124452=CARTESIAN_POINT('Ctrl Pts',(-9.5797094058222,13.0422098962276,9.59768097893714));
#124453=CARTESIAN_POINT('Ctrl Pts',(-9.63332411368873,13.0451258651884,
9.58374662065141));
#124454=CARTESIAN_POINT('Ctrl Pts',(-9.68698584714255,13.0480443917525,
9.56980004050702));
#124455=CARTESIAN_POINT('Ctrl Pts',(-9.74142340983765,13.0508939277508,
9.55887156717953));
#124456=CARTESIAN_POINT('Ctrl Pts',(-9.79627166289408,13.0537024946183,
9.55104350129771));
#124457=CARTESIAN_POINT('Ctrl Pts',(-9.85114376646174,13.0565122827782,
9.54321203141736));
#124458=CARTESIAN_POINT('Ctrl Pts',(-9.90642689820126,13.0592813606473,
9.5384840198725));
#124459=CARTESIAN_POINT('Ctrl Pts',(-9.96174250575976,13.062058455779,9.53690381441628));
#124460=CARTESIAN_POINT('Ctrl Pts',(-10.0171592713773,13.0648406295054,
9.53532071916956));
#124461=CARTESIAN_POINT('Ctrl Pts',(-10.0726085057825,13.0676313713475,
9.53689752043782));
#124462=CARTESIAN_POINT('Ctrl Pts',(-10.1276975482097,13.0704943671667,
9.54163371294026));
#124463=CARTESIAN_POINT('Ctrl Pts',(-10.1688531780977,13.0726332389116,
9.54517200253689));
#124464=CARTESIAN_POINT('Ctrl Pts',(-10.209807456237,13.0748128461259,9.55047277122835));
#124465=CARTESIAN_POINT('Ctrl Pts',(-10.2503935023658,13.0770618128499,
9.55751614721885));
#124466=CARTESIAN_POINT('Ctrl Pts',(-10.2504107598799,13.0770627691287,
9.55751914211912));
#124467=CARTESIAN_POINT('Ctrl Pts',(-10.2504280173278,13.07706372542,9.55752213733427));
#124468=CARTESIAN_POINT('Ctrl Pts',(-10.2504452747094,13.0770646817239,
9.55752513286428));
#124469=CARTESIAN_POINT('Ctrl Pts',(-10.2999283478705,13.0798067462746,
9.5661143866647));
#124470=CARTESIAN_POINT('Ctrl Pts',(-10.3490540963103,13.0826594087948,
9.57733250151461));
#124471=CARTESIAN_POINT('Ctrl Pts',(-10.3975314251549,13.0855635331345,
9.59110550936363));
#124472=CARTESIAN_POINT('Ctrl Pts',(-10.4020023090948,13.0858313697331,
9.59237574270909));
#124473=CARTESIAN_POINT('Ctrl Pts',(-10.4064676540746,13.0860996440499,
9.5936676792684));
#124474=CARTESIAN_POINT('Ctrl Pts',(-10.4109272177777,13.0863683096957,
9.59498124369684));
#124475=CARTESIAN_POINT('Ctrl Pts',(-10.4632663881832,13.0895214739851,
9.61039774563183));
#124476=CARTESIAN_POINT('Ctrl Pts',(-10.5148132490296,13.0927279572486,
9.62879731176444));
#124477=CARTESIAN_POINT('Ctrl Pts',(-10.5652209584256,13.0959256301729,
9.65004411605881));
#124478=CARTESIAN_POINT('Ctrl Pts',(-10.6155809302256,13.099120274806,9.67127079899927));
#124479=CARTESIAN_POINT('Ctrl Pts',(-10.6648040502312,13.1023058064021,
9.69533903076452));
#124480=CARTESIAN_POINT('Ctrl Pts',(-10.7125662975263,13.105439842644,9.72208043911381));
#124481=CARTESIAN_POINT('Ctrl Pts',(-10.7603032011951,13.108572215902,9.74880765792428));
#124482=CARTESIAN_POINT('Ctrl Pts',(-10.8065808261548,13.1116530190775,
9.77820509768527));
#124483=CARTESIAN_POINT('Ctrl Pts',(-10.8510960532976,13.114662790778,9.81007477960554));
#124484=CARTESIAN_POINT('Ctrl Pts',(-10.8964121546961,13.1177267113356,
9.84251782954903));
#124485=CARTESIAN_POINT('Ctrl Pts',(-10.9399017374015,13.120716954681,9.87752295521772));
#124486=CARTESIAN_POINT('Ctrl Pts',(-10.9812669267779,13.1236382711485,
9.91485049741996));
#124487=CARTESIAN_POINT('Ctrl Pts',(-11.0219325646473,13.1265101834826,
9.95154677118628));
#124488=CARTESIAN_POINT('Ctrl Pts',(-11.0605449414042,13.1293156851876,
9.99048755399651));
#124489=CARTESIAN_POINT('Ctrl Pts',(-11.0968436896816,13.1320822444629,
10.031415469163));
#124490=CARTESIAN_POINT('Ctrl Pts',(-11.1340790829517,13.134920191431,10.0733994793363));
#124491=CARTESIAN_POINT('Ctrl Pts',(-11.1688794471558,13.1377173925956,
10.1174747759693));
#124492=CARTESIAN_POINT('Ctrl Pts',(-11.2009922628842,13.1405248625602,
10.1633297738821));
#124493=CARTESIAN_POINT('Ctrl Pts',(-11.2313042754948,13.1431748969169,
10.2066133428706));
#124494=CARTESIAN_POINT('Ctrl Pts',(-11.2592216391798,13.1458345968796,
10.2514830235118));
#124495=CARTESIAN_POINT('Ctrl Pts',(-11.2845607691875,13.148559395597,10.2976452467453));
#124496=CARTESIAN_POINT('Ctrl Pts',(-11.2860661388544,13.1487212728728,
10.3003876933326));
#124497=CARTESIAN_POINT('Ctrl Pts',(-11.2875624218902,13.1488833799093,
10.3031347098596));
#124498=CARTESIAN_POINT('Ctrl Pts',(-11.2890495846627,13.1490457283295,
10.3058862379435));
#124499=CARTESIAN_POINT('',(-10.2623899083091,13.15,9.56021397908664));
#124500=CARTESIAN_POINT('Origin',(-10.,13.15,11.));
#124501=CARTESIAN_POINT('Ctrl Pts',(-10.2623899083091,13.15,9.56021397908663));
#124502=CARTESIAN_POINT('Ctrl Pts',(-10.2066727834959,13.1469204952333,
9.55005996240732));
#124503=CARTESIAN_POINT('Ctrl Pts',(-10.1503209963368,13.1438409904666,
9.54313634185553));
#124504=CARTESIAN_POINT('Ctrl Pts',(-10.093728771318,13.1407614856999,9.53950447880618));
#124505=CARTESIAN_POINT('Ctrl Pts',(-10.0371641637688,13.1376834837567,
9.53587438813576));
#124506=CARTESIAN_POINT('Ctrl Pts',(-9.98035984204682,13.1346054818135,
9.53553290138471));
#124507=CARTESIAN_POINT('Ctrl Pts',(-9.92371509738344,13.1315274798704,
9.53848952667701));
#124508=CARTESIAN_POINT('Ctrl Pts',(-9.8670840125995,13.1284502201874,9.54144543897916));
#124509=CARTESIAN_POINT('Ctrl Pts',(-9.8106129204972,13.1253729605043,9.54769785837776));
#124510=CARTESIAN_POINT('Ctrl Pts',(-9.75469909499313,13.1222957008213,
9.55720420155768));
#124511=CARTESIAN_POINT('Ctrl Pts',(-9.69878134951582,13.1192182253996,
9.56671121120266));
#124512=CARTESIAN_POINT('Ctrl Pts',(-9.64342143405366,13.1161407499779,
9.57947251435366));
#124513=CARTESIAN_POINT('Ctrl Pts',(-9.58900763170072,13.1130632745562,
9.595394175151));
#124514=CARTESIAN_POINT('Ctrl Pts',(-9.53457307596047,13.1099846253874,
9.61132190845896));
#124515=CARTESIAN_POINT('Ctrl Pts',(-9.48108582259361,13.1069059762186,
9.63041225381241));
#124516=CARTESIAN_POINT('Ctrl Pts',(-9.42891835822367,13.1038273270499,
9.65252161114693));
#124517=CARTESIAN_POINT('Ctrl Pts',(-9.37667202481571,13.1007440234456,
9.67466439436798));
#124518=CARTESIAN_POINT('Ctrl Pts',(-9.32574991787845,13.0976607198414,
9.69983510710552));
#124519=CARTESIAN_POINT('Ctrl Pts',(-9.27650306928019,13.0945774162371,
9.72784260359065));
#124520=CARTESIAN_POINT('Ctrl Pts',(-9.22721636945145,13.091491617581,9.755872764129));
#124521=CARTESIAN_POINT('Ctrl Pts',(-9.17960804257342,13.0884058189248,
9.78674401331004));
#124522=CARTESIAN_POINT('Ctrl Pts',(-9.13400044645138,13.0853200202687,
9.82022162112811));
#124523=CARTESIAN_POINT('Ctrl Pts',(-9.08829907787532,13.0822278769915,
9.85376806128348));
#124524=CARTESIAN_POINT('Ctrl Pts',(-9.04460703761997,13.0791357337144,
9.88993125001151));
#124525=CARTESIAN_POINT('Ctrl Pts',(-9.00321327857189,13.0760435904372,
9.92843643119757));
#124526=CARTESIAN_POINT('Ctrl Pts',(-8.98078087256881,13.0743678737348,
9.94930343814382));
#124527=CARTESIAN_POINT('Ctrl Pts',(-8.95902279238694,13.0726921570323,
9.97085761632403));
#124528=CARTESIAN_POINT('Ctrl Pts',(-8.93798015951895,13.0710164403299,
9.9930510894665));
#124529=CARTESIAN_POINT('Ctrl Pts',(-8.90055520974898,13.0680361282269,
10.0325228429675));
#124530=CARTESIAN_POINT('Ctrl Pts',(-8.86523868247035,13.0650558161238,
10.0741844535331));
#124531=CARTESIAN_POINT('Ctrl Pts',(-8.83230144086544,13.0620755040207,
10.1177798885793));
#124532=CARTESIAN_POINT('Ctrl Pts',(-8.7994307085445,13.0591012099815,10.1612872925389));
#124533=CARTESIAN_POINT('Ctrl Pts',(-8.76893005595056,13.0561269159423,
10.2067203504602));
#124534=CARTESIAN_POINT('Ctrl Pts',(-8.74103264624124,13.0531526219032,
10.2537872607831));
#124535=CARTESIAN_POINT('Ctrl Pts',(-8.71316679315608,13.0501816922867,
10.3008009305787));
#124536=CARTESIAN_POINT('Ctrl Pts',(-8.68789862887806,13.0472107626702,
10.3494443336317));
#124537=CARTESIAN_POINT('Ctrl Pts',(-8.6654190612364,13.0442398330538,10.399395331446));
#124538=CARTESIAN_POINT('Ctrl Pts',(-8.64295558404035,13.041271029972,10.4493105752891));
#124539=CARTESIAN_POINT('Ctrl Pts',(-8.62327697216056,13.0383022268903,
10.5005310693765));
#124540=CARTESIAN_POINT('Ctrl Pts',(-8.60652785182188,13.0353334238085,
10.5527108069136));
#124541=CARTESIAN_POINT('Ctrl Pts',(-8.58978376392874,13.0323655127342,
10.6048748665117));
#124542=CARTESIAN_POINT('Ctrl Pts',(-8.57596758709121,13.0293976016599,
10.6579970840582));
#124543=CARTESIAN_POINT('Ctrl Pts',(-8.56517465496131,13.0264296905856,
10.7117145871977));
#124544=CARTESIAN_POINT('Ctrl Pts',(-8.55437249422687,13.0234592417693,
10.7654780220253));
#124545=CARTESIAN_POINT('Ctrl Pts',(-8.54659885225552,13.020488792953,10.8198372291036));
#124546=CARTESIAN_POINT('Ctrl Pts',(-8.54189792310134,13.0175183441366,
10.8744190167907));
#124547=CARTESIAN_POINT('Ctrl Pts',(-8.53719511151245,13.0145467058371,
10.9290226611465));
#124548=CARTESIAN_POINT('Ctrl Pts',(-8.53556748112019,13.0115750675376,
10.9838485227374));
#124549=CARTESIAN_POINT('Ctrl Pts',(-8.53700706325901,13.0086034292382,
11.0385216438637));
#124550=CARTESIAN_POINT('Ctrl Pts',(-8.53844943988335,13.0056260224591,
11.0933008952632));
#124551=CARTESIAN_POINT('Ctrl Pts',(-8.54297087756189,13.00264861568,11.1479262741279));
#124552=CARTESIAN_POINT('Ctrl Pts',(-8.5505114136092,12.9996712089009,11.2020274434893));
#124553=CARTESIAN_POINT('Ctrl Pts',(-8.55695965237494,12.9971250994872,
11.2482916951762));
#124554=CARTESIAN_POINT('Ctrl Pts',(-8.5656147458921,12.9945789900735,11.294172543667));
#124555=CARTESIAN_POINT('Ctrl Pts',(-8.57641011449673,12.9920328806598,
11.3394467379322));
#124556=CARTESIAN_POINT('Ctrl Pts',(-8.58919170728616,12.9890183162744,
11.3930508654206));
#124557=CARTESIAN_POINT('Ctrl Pts',(-8.60503150897651,12.986003751889,11.4460427091708));
#124558=CARTESIAN_POINT('Ctrl Pts',(-8.62385347287675,12.9829891875036,
11.4980491801887));
#124559=CARTESIAN_POINT('Ctrl Pts',(-8.64264201665942,12.9799799757528,
11.5499633089629));
#124560=CARTESIAN_POINT('Ctrl Pts',(-8.6644020355962,12.976970764002,11.6008950465764));
#124561=CARTESIAN_POINT('Ctrl Pts',(-8.68900719273,12.9739615522512,11.6504845188675));
#124562=CARTESIAN_POINT('Ctrl Pts',(-8.71358799874196,12.9709553186437,
11.7000249136715));
#124563=CARTESIAN_POINT('Ctrl Pts',(-8.7410081315262,12.9679490850361,11.7482252058589));
#124564=CARTESIAN_POINT('Ctrl Pts',(-8.77109314757686,12.9649428514286,
11.7947453668109));
#124565=CARTESIAN_POINT('Ctrl Pts',(-8.80116016980837,12.9619384158465,
11.8412377040995));
#124566=CARTESIAN_POINT('Ctrl Pts',(-8.83388863052887,12.9589339802644,
11.8860514611139));
#124567=CARTESIAN_POINT('Ctrl Pts',(-8.86905925543878,12.9559295446822,
11.9288731249699));
#124568=CARTESIAN_POINT('Ctrl Pts',(-8.90422261581189,12.9529257296701,
11.9716859439573));
#124569=CARTESIAN_POINT('Ctrl Pts',(-8.94182680470588,12.9499219146579,
12.0125070805286));
#124570=CARTESIAN_POINT('Ctrl Pts',(-8.98161193394522,12.9469180996457,
12.0510556583346));
#124571=CARTESIAN_POINT('Ctrl Pts',(-9.02143262164391,12.9439115999361,
12.0896386894166));
#124572=CARTESIAN_POINT('Ctrl Pts',(-9.0634377654752,12.9409051002265,12.1259447365983));
#124573=CARTESIAN_POINT('Ctrl Pts',(-9.10733128966854,12.9378986005169,
12.1597304961047));
#124574=CARTESIAN_POINT('Ctrl Pts',(-9.15124428261898,12.9348907672892,
12.1935312411187));
#124575=CARTESIAN_POINT('Ctrl Pts',(-9.19704689074182,12.9318829340614,
12.22480917203));
#124576=CARTESIAN_POINT('Ctrl Pts',(-9.2444133471966,12.9288751008336,12.253363897719));
#124577=CARTESIAN_POINT('Ctrl Pts',(-9.29186728686476,12.925861712305,12.2819713623998));
#124578=CARTESIAN_POINT('Ctrl Pts',(-9.34089037852705,12.9228483237763,
12.3078453275584));
#124579=CARTESIAN_POINT('Ctrl Pts',(-9.39113255506277,12.9198349352477,
12.3308315763069));
#124580=CARTESIAN_POINT('Ctrl Pts',(-9.42884469940513,12.9175730638284,
12.3480852223562));
#124581=CARTESIAN_POINT('Ctrl Pts',(-9.46724317756633,12.915311192409,12.3637128649905));
#124582=CARTESIAN_POINT('Ctrl Pts',(-9.50617417360824,12.9130493209897,
12.3776677041974));
#124583=CARTESIAN_POINT('Ctrl Pts',(-9.55807203035402,12.910034081442,12.3962705225094));
#124584=CARTESIAN_POINT('Ctrl Pts',(-9.61112726852308,12.9070188418942,
12.4119742732251));
#124585=CARTESIAN_POINT('Ctrl Pts',(-9.66498535908375,12.9040036023465,
12.4246394071384));
#124586=CARTESIAN_POINT('Ctrl Pts',(-9.71875086406413,12.9009935461928,
12.4372827688582));
#124587=CARTESIAN_POINT('Ctrl Pts',(-9.77331597410781,12.8979834900391,
12.4468977615394));
#124588=CARTESIAN_POINT('Ctrl Pts',(-9.82830984692722,12.8949734338853,
12.4533942140169));
#124589=CARTESIAN_POINT('Ctrl Pts',(-9.8832511933067,12.8919662527343,12.459884461521));
#124590=CARTESIAN_POINT('Ctrl Pts',(-9.93861997111454,12.8889590715833,
12.4632620088642));
#124591=CARTESIAN_POINT('Ctrl Pts',(-9.99403579492368,12.8859518904323,
12.4634878469799));
#124592=CARTESIAN_POINT('Ctrl Pts',(-10.0494203555223,12.8829464058028,
12.4637135576875));
#124593=CARTESIAN_POINT('Ctrl Pts',(-10.1048513844888,12.8799409211733,
12.4607910818566));
#124594=CARTESIAN_POINT('Ctrl Pts',(-10.1599463280466,12.8769354365438,
12.4547334539854));
#124595=CARTESIAN_POINT('Ctrl Pts',(-10.2150317286662,12.8739304724911,
12.4486768753497));
#124596=CARTESIAN_POINT('Ctrl Pts',(-10.2697806369713,12.8709255084385,
12.4394862810262));
#124597=CARTESIAN_POINT('Ctrl Pts',(-10.3238157568095,12.8679205443859,
12.4272265432095));
#124598=CARTESIAN_POINT('Ctrl Pts',(-10.3779017934463,12.8649127487832,
12.4149552531542));
#124599=CARTESIAN_POINT('Ctrl Pts',(-10.4312721839688,12.8619049531805,
12.3996091590201));
#124600=CARTESIAN_POINT('Ctrl Pts',(-10.4835614183549,12.8588971575778,
12.3813039508662));
#124601=CARTESIAN_POINT('Ctrl Pts',(-10.5358752893579,12.8558879448208,
12.362990118023));
#124602=CARTESIAN_POINT('Ctrl Pts',(-10.5871065022511,12.8528787320639,
12.3417145941067));
#124603=CARTESIAN_POINT('Ctrl Pts',(-10.6369093691016,12.849869519307,12.3176413417735));
#124604=CARTESIAN_POINT('Ctrl Pts',(-10.6868061775791,12.8468546303639,
12.2935226807994));
#124605=CARTESIAN_POINT('Ctrl Pts',(-10.7352687970077,12.8438397414209,
12.2665960053905));
#124606=CARTESIAN_POINT('Ctrl Pts',(-10.781977016144,12.8408248524778,12.2370708129378));
#124607=CARTESIAN_POINT('Ctrl Pts',(-10.8168821283986,12.8385718220917,
12.2150065986312));
#124608=CARTESIAN_POINT('Ctrl Pts',(-10.8508080173204,12.8363187917057,
12.1914921758089));
#124609=CARTESIAN_POINT('Ctrl Pts',(-10.8836331703264,12.8340657613196,
12.1666296200161));
#124610=CARTESIAN_POINT('Ctrl Pts',(-10.9281971894432,12.8310070066757,
12.1328757663345));
#124611=CARTESIAN_POINT('Ctrl Pts',(-10.9709323801074,12.8279482520317,
12.0964827451277));
#124612=CARTESIAN_POINT('Ctrl Pts',(-11.0115060496337,12.8248894973878,
12.0576803683318));
#124613=CARTESIAN_POINT('Ctrl Pts',(-11.0509173035851,12.8219183745523,
12.0199896604496));
#124614=CARTESIAN_POINT('Ctrl Pts',(-11.0882887948641,12.8189472517169,
11.9800261918535));
#124615=CARTESIAN_POINT('Ctrl Pts',(-11.1233463040231,12.8159761288814,
11.9380433525363));
#124616=CARTESIAN_POINT('Ctrl Pts',(-11.1583695041737,12.8130079137334,
11.8961015996974));
#124617=CARTESIAN_POINT('Ctrl Pts',(-11.1910828596685,12.8100396985854,
11.8521448013385));
#124618=CARTESIAN_POINT('Ctrl Pts',(-11.2212495020353,12.8070714834374,
11.8064625867196));
#124619=CARTESIAN_POINT('Ctrl Pts',(-11.2513991981548,12.8041049356976,
11.7608060342907));
#124620=CARTESIAN_POINT('Ctrl Pts',(-11.2790047175845,12.8011383879578,
11.7134264364987));
#124621=CARTESIAN_POINT('Ctrl Pts',(-11.3038714750513,12.798171840218,11.6646438343561));
#124622=CARTESIAN_POINT('Ctrl Pts',(-11.3287346289191,12.7952057223794,
11.6158683016086));
#124623=CARTESIAN_POINT('Ctrl Pts',(-11.3508595646768,12.7922396045408,
11.5656906508641));
#124624=CARTESIAN_POINT('Ctrl Pts',(-11.370097980956,12.7892734867022,11.5144548304568));
#124625=CARTESIAN_POINT('Ctrl Pts',(-11.3893533958098,12.7863047480774,
11.4631737393838));
#124626=CARTESIAN_POINT('Ctrl Pts',(-11.4057170135729,12.7833360094526,
11.4108331211167));
#124627=CARTESIAN_POINT('Ctrl Pts',(-11.4190896270524,12.7803672708279,
11.3577944666878));
#124628=CARTESIAN_POINT('Ctrl Pts',(-11.4324695517042,12.7773969091127,
11.3047268145804));
#124629=CARTESIAN_POINT('Ctrl Pts',(-11.4428551179191,12.7744265473976,
11.2509608986462));
#124630=CARTESIAN_POINT('Ctrl Pts',(-11.4501984059751,12.7714561856825,
11.1968675527031));
#124631=CARTESIAN_POINT('Ctrl Pts',(-11.4575535382614,12.7684810329734,
11.1426869578266));
#124632=CARTESIAN_POINT('Ctrl Pts',(-11.4618565698593,12.7655058802644,
11.0881784184255));
#124633=CARTESIAN_POINT('Ctrl Pts',(-11.4631115929678,12.7625307275554,
11.0337152268741));
#124634=CARTESIAN_POINT('Ctrl Pts',(-11.4633752506757,12.7619057016585,
11.0222734931305));
#124635=CARTESIAN_POINT('Ctrl Pts',(-11.463504569122,12.7612806757617,11.0108337466015));
#124636=CARTESIAN_POINT('Ctrl Pts',(-11.4634998767682,12.7606556498649,
10.9993994174008));
#124637=CARTESIAN_POINT('Origin',(-10.,13.15,11.));
#124638=CARTESIAN_POINT('',(-11.3001231424463,13.15,10.3280535255874));
#124639=CARTESIAN_POINT('',(-11.4635,13.15,11.));
#124640=CARTESIAN_POINT('Origin',(-10.,13.15,11.));
#124641=CARTESIAN_POINT('Ctrl Pts',(-11.3001231424463,13.15,10.3280535255874));
#124642=CARTESIAN_POINT('Ctrl Pts',(-11.3131761773218,13.1500001384125,
10.3600202599267));
#124643=CARTESIAN_POINT('Ctrl Pts',(-11.3249989234091,13.15,10.3924378242408));
#124644=CARTESIAN_POINT('Ctrl Pts',(-11.3355332824938,13.15,10.425267838127));
#124645=CARTESIAN_POINT('Ctrl Pts',(-11.3530400634154,13.15,10.4798271953819));
#124646=CARTESIAN_POINT('Ctrl Pts',(-11.3669904096394,13.15,10.5355261957002));
#124647=CARTESIAN_POINT('Ctrl Pts',(-11.3774433906746,13.15,10.5920302374161));
#124648=CARTESIAN_POINT('Ctrl Pts',(-11.3819168595279,13.15,10.6162117670538));
#124649=CARTESIAN_POINT('Ctrl Pts',(-11.3857491615815,13.15,10.6405407123288));
#124650=CARTESIAN_POINT('Ctrl Pts',(-11.3889422263824,13.15,10.6649903831658));
#124651=CARTESIAN_POINT('Ctrl Pts',(-11.3905331695892,13.15,10.6771724214745));
#124652=CARTESIAN_POINT('Ctrl Pts',(-11.3919652511976,13.15,10.6893842554283));
#124653=CARTESIAN_POINT('Ctrl Pts',(-11.3932374922766,13.15,10.7016085237643));
#124654=CARTESIAN_POINT('Ctrl Pts',(-11.3991939351861,13.15,10.7588407242136));
#124655=CARTESIAN_POINT('Ctrl Pts',(-11.4016617168143,13.15,10.81642392022));
#124656=CARTESIAN_POINT('Ctrl Pts',(-11.4007057393064,13.15,10.8740172395586));
#124657=CARTESIAN_POINT('Ctrl Pts',(-11.4000640964045,13.15,10.9126733211552));
#124658=CARTESIAN_POINT('Ctrl Pts',(-11.397878941981,13.15,10.9513339579117));
#124659=CARTESIAN_POINT('Ctrl Pts',(-11.3941573214885,13.15,10.9898921947642));
#124660=CARTESIAN_POINT('Ctrl Pts',(-11.3925406285891,13.15,11.0066421099846));
#124661=CARTESIAN_POINT('Ctrl Pts',(-11.3906338685773,13.15,11.0233726427463));
#124662=CARTESIAN_POINT('Ctrl Pts',(-11.3884370658247,13.15,11.0400747034851));
#124663=CARTESIAN_POINT('Ctrl Pts',(-11.3869501481743,13.15,11.0513795823056));
#124664=CARTESIAN_POINT('Ctrl Pts',(-11.3853299562707,13.15,11.0626733277691));
#124665=CARTESIAN_POINT('Ctrl Pts',(-11.3835793602485,13.15,11.0739358722133));
#124666=CARTESIAN_POINT('Ctrl Pts',(-11.3749382707088,13.15,11.1295287410149));
#124667=CARTESIAN_POINT('Ctrl Pts',(-11.3631134776978,13.15,11.1844512590875));
#124668=CARTESIAN_POINT('Ctrl Pts',(-11.3481619217541,13.15,11.2383858660144));
#124669=CARTESIAN_POINT('Ctrl Pts',(-11.3335747203039,13.15,11.2910061404084));
#124670=CARTESIAN_POINT('Ctrl Pts',(-11.3160107755577,13.15,11.3426869861088));
#124671=CARTESIAN_POINT('Ctrl Pts',(-11.2954804801254,13.15,11.3931098408422));
#124672=CARTESIAN_POINT('Ctrl Pts',(-11.2831410946931,13.15,11.423415641419));
#124673=CARTESIAN_POINT('Ctrl Pts',(-11.2697293596248,13.15,11.4532664844744));
#124674=CARTESIAN_POINT('Ctrl Pts',(-11.2552409779441,13.15,11.4825868996509));
#124675=CARTESIAN_POINT('Ctrl Pts',(-11.2449747067262,13.15,11.5033629491129));
#124676=CARTESIAN_POINT('Ctrl Pts',(-11.2341677552456,13.15,11.5238725721958));
#124677=CARTESIAN_POINT('Ctrl Pts',(-11.2228172228053,13.15,11.5440871005847));
#124678=CARTESIAN_POINT('Ctrl Pts',(-11.2179779990594,13.15,11.5527054298398));
#124679=CARTESIAN_POINT('Ctrl Pts',(-11.2130398598468,13.15,11.5612700459744));
#124680=CARTESIAN_POINT('Ctrl Pts',(-11.2080101180467,13.15,11.5697664482042));
#124681=CARTESIAN_POINT('Ctrl Pts',(-11.1811395839106,13.15,11.6151570219604));
#124682=CARTESIAN_POINT('Ctrl Pts',(-11.1516077646003,13.15,11.6586941060695));
#124683=CARTESIAN_POINT('Ctrl Pts',(-11.1194321742994,13.15,11.7000869398436));
#124684=CARTESIAN_POINT('Ctrl Pts',(-11.1119483238485,13.15,11.7097146661668));
#124685=CARTESIAN_POINT('Ctrl Pts',(-11.1043212841036,13.15,11.7192262371259));
#124686=CARTESIAN_POINT('Ctrl Pts',(-11.0965509899046,13.15,11.7286176981156));
#124687=CARTESIAN_POINT('Ctrl Pts',(-11.0623201142441,13.15,11.7699903830067));
#124688=CARTESIAN_POINT('Ctrl Pts',(-11.0253109874935,13.15,11.809035775708));
#124689=CARTESIAN_POINT('Ctrl Pts',(-10.9858215050894,13.15,11.8456181550914));
#124690=CARTESIAN_POINT('Ctrl Pts',(-10.9676656385286,13.15,11.8624374385594));
#124691=CARTESIAN_POINT('Ctrl Pts',(-10.948985131905,13.15,11.8787354281648));
#124692=CARTESIAN_POINT('Ctrl Pts',(-10.9298077378061,13.15,11.8944954447994));
#124693=CARTESIAN_POINT('Ctrl Pts',(-10.9162290702529,13.15,11.9056544179847));
#124694=CARTESIAN_POINT('Ctrl Pts',(-10.9024012778973,13.15,11.9165436356749));
#124695=CARTESIAN_POINT('Ctrl Pts',(-10.8883341250136,13.15,11.9271564682047));
#124696=CARTESIAN_POINT('Ctrl Pts',(-10.8801543039317,13.15,11.9333276580669));
#124697=CARTESIAN_POINT('Ctrl Pts',(-10.8719002307745,13.15,11.9394002908066));
#124698=CARTESIAN_POINT('Ctrl Pts',(-10.8635785576173,13.15,11.9453704723774));
#124699=CARTESIAN_POINT('Ctrl Pts',(-10.8209146516277,13.15,11.9759786518223));
#124700=CARTESIAN_POINT('Ctrl Pts',(-10.7764391517408,13.15,12.0039254571033));
#124701=CARTESIAN_POINT('Ctrl Pts',(-10.7304434962769,13.15,12.0291037016939));
#124702=CARTESIAN_POINT('Ctrl Pts',(-10.6846701427477,13.15,12.0541602571286));
#124703=CARTESIAN_POINT('Ctrl Pts',(-10.637390123747,13.15,12.076475205012));
#124704=CARTESIAN_POINT('Ctrl Pts',(-10.5888782659809,13.15,12.0958933837174));
#124705=CARTESIAN_POINT('Ctrl Pts',(-10.5645820655954,13.15,12.1056185928244));
#124706=CARTESIAN_POINT('Ctrl Pts',(-10.5399767966041,13.15,12.114616401565));
#124707=CARTESIAN_POINT('Ctrl Pts',(-10.5150971825505,13.15,12.1228623097433));
#124708=CARTESIAN_POINT('Ctrl Pts',(-10.4967682426672,13.15,12.1289371127911));
#124709=CARTESIAN_POINT('Ctrl Pts',(-10.478290409887,13.15,12.1346037641086));
#124710=CARTESIAN_POINT('Ctrl Pts',(-10.4596778365068,13.15,12.1398512498179));
#124711=CARTESIAN_POINT('Ctrl Pts',(-10.4506803455549,13.15,12.1423879331784));
#124712=CARTESIAN_POINT('Ctrl Pts',(-10.4416523204638,13.15,12.1448262828857));
#124713=CARTESIAN_POINT('Ctrl Pts',(-10.4326078634624,13.15,12.1471621057536));
#124714=CARTESIAN_POINT('Ctrl Pts',(-10.3837777132245,13.15,12.1597729879272));
#124715=CARTESIAN_POINT('Ctrl Pts',(-10.3343722745856,13.15,12.1694272995591));
#124716=CARTESIAN_POINT('Ctrl Pts',(-10.2846451915519,13.15,12.1759981133649));
#124717=CARTESIAN_POINT('Ctrl Pts',(-10.2359330315984,13.15,12.1824348177442));
#124718=CARTESIAN_POINT('Ctrl Pts',(-10.186911278204,13.15,12.1859126350798));
#124719=CARTESIAN_POINT('Ctrl Pts',(-10.1378247727926,13.15,12.1862630676831));
#124720=CARTESIAN_POINT('Ctrl Pts',(-10.0887382673813,13.15,12.1866135002864));
#124721=CARTESIAN_POINT('Ctrl Pts',(-10.0395861028003,13.15,12.18383673007));
#124722=CARTESIAN_POINT('Ctrl Pts',(-9.99063336962942,13.15,12.1777127530665));
#124723=CARTESIAN_POINT('Ctrl Pts',(-8.88725970493454,13.15,11.3858809379032));
#124724=CARTESIAN_POINT('Ctrl Pts',(-8.82376602848846,13.15,11.257038925907));
#124725=CARTESIAN_POINT('Ctrl Pts',(-8.78447134070238,13.15,11.1152741740962));
#124726=CARTESIAN_POINT('Ctrl Pts',(-8.76392545979419,13.15,10.799130945112));
#124727=CARTESIAN_POINT('Ctrl Pts',(-8.78332170790095,13.15,10.6406721133509));
#124728=CARTESIAN_POINT('Ctrl Pts',(-8.87404255296001,13.15,10.3431797244535));
#124729=CARTESIAN_POINT('Ctrl Pts',(-8.94502385990684,13.15,10.2027828893632));
#124730=CARTESIAN_POINT('Ctrl Pts',(-9.13810939903446,13.15,9.95383959518158));
#124731=CARTESIAN_POINT('Ctrl Pts',(-9.26076129175572,13.15,9.84753666691401));
#124732=CARTESIAN_POINT('Ctrl Pts',(-9.52446957852726,13.15,9.68764328331985));
#124733=CARTESIAN_POINT('Ctrl Pts',(-9.66358225430457,13.15,9.63064099380393));
#124734=CARTESIAN_POINT('Ctrl Pts',(-9.95615051730649,13.15,9.55970692742898));
#124735=CARTESIAN_POINT('Ctrl Pts',(-10.110190526121,13.15,9.54703709299416));
#124736=CARTESIAN_POINT('Ctrl Pts',(-10.2623899083091,13.15,9.5602139790866));
#124737=CARTESIAN_POINT('Origin',(-10.,13.15,11.));
#124738=CARTESIAN_POINT('Ctrl Pts',(-10.5090242870262,3.43381032135065,
9.9402163861523));
#124739=CARTESIAN_POINT('Ctrl Pts',(-10.8597543436467,3.46014567915783,
10.1086659006971));
#124740=CARTESIAN_POINT('Ctrl Pts',(-11.3748996206351,3.51280889018836,
10.8179605421406));
#124741=CARTESIAN_POINT('Ctrl Pts',(-10.9029747057089,3.59179995444226,
12.0542997660115));
#124742=CARTESIAN_POINT('Ctrl Pts',(-9.61102705413118,3.67078351411235,
12.3312080230099));
#124743=CARTESIAN_POINT('Ctrl Pts',(-8.67243540897439,3.74976707378244,
11.4024835440384));
#124744=CARTESIAN_POINT('Ctrl Pts',(-8.93744951993946,3.82875063345253,
10.1079392171469));
#124745=CARTESIAN_POINT('Ctrl Pts',(-10.1662184072312,3.90773419312261,
9.62280065437638));
#124746=CARTESIAN_POINT('Ctrl Pts',(-11.244163884115,3.98671775279271,10.3863742247578));
#124747=CARTESIAN_POINT('Ctrl Pts',(-11.1938649654809,4.06570131246279,
11.7065393375666));
#124748=CARTESIAN_POINT('Ctrl Pts',(-10.0608681388599,4.14468487213289,
12.3859082577524));
#124749=CARTESIAN_POINT('Ctrl Pts',(-8.87268420671462,4.22366843180297,
11.8084764549642));
#124750=CARTESIAN_POINT('Ctrl Pts',(-8.70681751959354,4.30265199147307,
10.49784911305));
#124751=CARTESIAN_POINT('Ctrl Pts',(-9.71369639202666,4.38163555114315,
9.64261346806346));
#124752=CARTESIAN_POINT('Ctrl Pts',(-10.9802123564701,4.46061911081324,
10.0183401047257));
#124753=CARTESIAN_POINT('Ctrl Pts',(-11.3578086652279,4.53960267048333,
11.2843023117032));
#124754=CARTESIAN_POINT('Ctrl Pts',(-10.504054987852,4.61858623015341,12.292439426545));
#124755=CARTESIAN_POINT('Ctrl Pts',(-9.19319158814925,4.69756978982351,
12.1285087346752));
#124756=CARTESIAN_POINT('Ctrl Pts',(-8.61399459221431,4.77655334949359,
10.9411723380592));
#124757=CARTESIAN_POINT('Ctrl Pts',(-9.29171783157003,4.85553690916369,
9.80718487427643));
#124758=CARTESIAN_POINT('Ctrl Pts',(-10.6117575376679,4.93452046883377,
9.75491993483644));
#124759=CARTESIAN_POINT('Ctrl Pts',(-11.3770155961763,5.01350402850386,
10.8317749122026));
#124760=CARTESIAN_POINT('Ctrl Pts',(-10.8935060234263,5.09248758817395,
12.0611873555489));
#124761=CARTESIAN_POINT('Ctrl Pts',(-9.59970687324196,5.17147114784404,
12.3282458523706));
#124762=CARTESIAN_POINT('Ctrl Pts',(-8.66891965550706,5.25045470751413,
11.3907643076178));
#124763=CARTESIAN_POINT('Ctrl Pts',(-8.94524297664017,5.32943826718422,
10.0989121864417));
#124764=CARTESIAN_POINT('Ctrl Pts',(-10.1780888111114,5.40842182685431,
9.62422530790764));
#124765=CARTESIAN_POINT('Ctrl Pts',(-11.249432087953,5.48740538652439,10.3971807195104));
#124766=CARTESIAN_POINT('Ctrl Pts',(-11.1877087953521,5.5663889461945,11.7168120009095));
#124767=CARTESIAN_POINT('Ctrl Pts',(-10.0488936440701,5.64537250586456,
12.3863913729684));
#124768=CARTESIAN_POINT('Ctrl Pts',(-8.86573854494997,5.72435606553468,
11.7987005564936));
#124769=CARTESIAN_POINT('Ctrl Pts',(-8.71120576787552,5.80333962520474,
10.4866959433319));
#124770=CARTESIAN_POINT('Ctrl Pts',(-9.72543572159486,5.88232318487485,
9.640188952682));
#124771=CARTESIAN_POINT('Ctrl Pts',(-10.9886584841126,5.96130674454492,
10.026847376226));
#124772=CARTESIAN_POINT('Ctrl Pts',(-11.3553012023303,6.04029030421503,
11.2960241178163));
#124773=CARTESIAN_POINT('Ctrl Pts',(-10.4928683281718,6.1192738638851,12.296746867533));
#124774=CARTESIAN_POINT('Ctrl Pts',(-9.18347028393007,6.1982574235552,12.1214949175736));
#124775=CARTESIAN_POINT('Ctrl Pts',(-8.61455468207693,6.27724098322528,
10.9291981750663));
#124776=CARTESIAN_POINT('Ctrl Pts',(-9.30205132416306,6.35622454289538,
9.80110914872666));
#124777=CARTESIAN_POINT('Ctrl Pts',(-10.62249338143,6.43520810256546,9.76025259933933));
#124778=CARTESIAN_POINT('Ctrl Pts',(-11.3784178095403,6.51419166223555,
10.8436799126432));
#124779=CARTESIAN_POINT('Ctrl Pts',(-10.8843029970064,6.59317522190564,
12.0688684843584));
#124780=CARTESIAN_POINT('Ctrl Pts',(-9.58824450728937,6.67215878157573,
12.3247373481531));
#124781=CARTESIAN_POINT('Ctrl Pts',(-8.66559277412816,6.75114234124581,
11.3792479174763));
#124782=CARTESIAN_POINT('Ctrl Pts',(-8.95306861171804,6.83012590091592,
10.0898317212739));
#124783=CARTESIAN_POINT('Ctrl Pts',(-10.1899701666462,6.90910946058599,
9.62581552797539));
#124784=CARTESIAN_POINT('Ctrl Pts',(-11.2545943748831,6.98809302025609,
10.407999508547));
#124785=CARTESIAN_POINT('Ctrl Pts',(-11.1814705151243,7.06707657992617,
11.7270481753372));
#124786=CARTESIAN_POINT('Ctrl Pts',(-10.0369120762793,7.14606013959627,
12.3867621014413));
#124787=CARTESIAN_POINT('Ctrl Pts',(-8.85887935736957,7.22504369926635,
11.7888696383636));
#124788=CARTESIAN_POINT('Ctrl Pts',(-8.71568931948482,7.30402725893644,
10.4755786967677));
#124789=CARTESIAN_POINT('Ctrl Pts',(-9.73719603516132,7.38301081860653,
9.6378672225388));
#124790=CARTESIAN_POINT('Ctrl Pts',(-10.9970305396777,7.46199437827663,
10.0354266589216));
#124791=CARTESIAN_POINT('Ctrl Pts',(-11.3526926734573,7.5409779379467,11.3077241598318));
#124792=CARTESIAN_POINT('Ctrl Pts',(-10.4816447991026,7.6199614976168,12.3009573070883));
#124793=CARTESIAN_POINT('Ctrl Pts',(-9.17380998339862,7.69894505728688,
12.1143974532622));
#124794=CARTESIAN_POINT('Ctrl Pts',(-8.61521820114381,7.77792861695698,
10.9172292507842));
#124795=CARTESIAN_POINT('Ctrl Pts',(-9.31243694043001,7.85691217662706,
9.79512296623934));
#124796=CARTESIAN_POINT('Ctrl Pts',(-10.6331827401846,7.93589573629716,
9.76567781965101));
#124797=CARTESIAN_POINT('Ctrl Pts',(-11.3797171025569,8.01487929596723,
10.8555965918649));
#124798=CARTESIAN_POINT('Ctrl Pts',(-10.8750339405711,8.09386285563734,
12.0764697999562));
#124799=CARTESIAN_POINT('Ctrl Pts',(-9.57681288677996,8.17284641530742,
12.321129930996));
#124800=CARTESIAN_POINT('Ctrl Pts',(-8.66236552917783,8.2518299749775,11.3677032089028));
#124801=CARTESIAN_POINT('Ctrl Pts',(-8.96097241869386,8.3308135346476,10.0808192165551));
#124802=CARTESIAN_POINT('Ctrl Pts',(-10.2018373374917,8.40979709431769,
9.62750835464715));
#124803=CARTESIAN_POINT('Ctrl Pts',(-11.2596629844915,8.48878065398777,
10.4188625008905));
#124804=CARTESIAN_POINT('Ctrl Pts',(-11.1751440174684,8.56776421365786,
11.7372300628551));
#124805=CARTESIAN_POINT('Ctrl Pts',(-10.0249277523716,8.64674777332795,
12.3870292839486));
#124806=CARTESIAN_POINT('Ctrl Pts',(-8.85210537436044,8.72573133299805,
11.7789798173233));
#124807=CARTESIAN_POINT('Ctrl Pts',(-8.72026876731281,8.80471489266813,
10.4645006074195));
#124808=CARTESIAN_POINT('Ctrl Pts',(-9.74897597163002,8.88369845233822,
9.63564719938351));
#124809=CARTESIAN_POINT('Ctrl Pts',(-11.005328149507,8.96268201200831,10.04407796386));
#124810=CARTESIAN_POINT('Ctrl Pts',(-11.3499831424592,9.0416655716784,11.3194012248648));
#124811=CARTESIAN_POINT('Ctrl Pts',(-10.4703853068404,9.12064913134849,
12.3050706074684));
#124812=CARTESIAN_POINT('Ctrl Pts',(-9.16421137237607,9.19963269101857,
12.1072167797246));
#124813=CARTESIAN_POINT('Ctrl Pts',(-8.61598511834872,9.27861625068866,
10.9052665067839));
#124814=CARTESIAN_POINT('Ctrl Pts',(-9.32287389528337,9.35759981035876,
9.7892267488582));
#124815=CARTESIAN_POINT('Ctrl Pts',(-10.6438248207931,9.43658337002884,
9.77119520366337));
#124816=CARTESIAN_POINT('Ctrl Pts',(-11.3809133756036,9.51556692969893,
10.8675240533223));
#124817=CARTESIAN_POINT('Ctrl Pts',(-10.8656995475751,9.59455048936902,
12.0839907382895));
#124818=CARTESIAN_POINT('Ctrl Pts',(-9.56541286457688,9.67353404903911,
12.3174238684243));
#124819=CARTESIAN_POINT('Ctrl Pts',(-8.6592381619943,9.7525176087092,11.3561310448651));
#124820=CARTESIAN_POINT('Ctrl Pts',(-8.96895380721882,9.83150116837929,
10.0718753447297));
#124821=CARTESIAN_POINT('Ctrl Pts',(-10.2136894376561,9.91048472804938,
9.62930366178233));
#124822=CARTESIAN_POINT('Ctrl Pts',(-11.2646375382657,9.98946828771946,
10.4297688852943));
#124823=CARTESIAN_POINT('Ctrl Pts',(-11.168729774795,10.0684518473895,11.7473569032777));
#124824=CARTESIAN_POINT('Ctrl Pts',(-10.012941567172,10.1474354070596,12.3871929005038));
#124825=CARTESIAN_POINT('Ctrl Pts',(-8.84541710172598,10.2264189667297,
11.7690318318396));
#124826=CARTESIAN_POINT('Ctrl Pts',(-8.72494376942007,10.3054025263998,
10.45346250245));
#124827=CARTESIAN_POINT('Ctrl Pts',(-9.76077465142473,10.3843860860699,
9.6335290489851));
#124828=CARTESIAN_POINT('Ctrl Pts',(-11.0135506940386,10.46336964574,10.0528006450672));
#124829=CARTESIAN_POINT('Ctrl Pts',(-11.3471728116493,10.5423532054101,
11.3310544410212));
#124830=CARTESIAN_POINT('Ctrl Pts',(-10.4590906921049,10.6213367650801,
12.3090864615405));
#124831=CARTESIAN_POINT('Ctrl Pts',(-9.15467516756241,10.7003203247502,
12.0999534331274));
#124832=CARTESIAN_POINT('Ctrl Pts',(-8.61685537643562,10.7793038844203,
10.8933108362856));
#124833=CARTESIAN_POINT('Ctrl Pts',(-9.33336140940735,10.8582874440904,
9.78342093685283));
#124834=CARTESIAN_POINT('Ctrl Pts',(-10.6544188286669,10.9372710037605,
9.77680433938067));
#124835=CARTESIAN_POINT('Ctrl Pts',(-11.3820065393025,11.0162545634306,
10.8794614064728));
#124836=CARTESIAN_POINT('Ctrl Pts',(-10.8563005150997,11.0952381231007,
12.0914307376909));
#124837=CARTESIAN_POINT('Ctrl Pts',(-9.55404529168748,11.1742216827708,
12.3136194373482));
#124838=CARTESIAN_POINT('Ctrl Pts',(-8.65621090648078,11.2532052424409,
11.3445322890657));
#124839=CARTESIAN_POINT('Ctrl Pts',(-8.97701218059255,11.3321888021109,
10.0630007743079));
#124840=CARTESIAN_POINT('Ctrl Pts',(-10.2255255836145,11.4111723617811,
9.63120131399661));
#124841=CARTESIAN_POINT('Ctrl Pts',(-11.2695176620004,11.4901559214511,
10.4407178499673));
#124842=CARTESIAN_POINT('Ctrl Pts',(-11.1622282713562,11.5691394811212,
11.7574279355407));
#124843=CARTESIAN_POINT('Ctrl Pts',(-10.0009544054462,11.6481230407913,
12.3872529483376));
#124844=CARTESIAN_POINT('Ctrl Pts',(-8.83881505847741,11.7271066004614,
11.7590264065578));
#124845=CARTESIAN_POINT('Ctrl Pts',(-8.72971393906159,11.8060901601315,
10.4424652408987));
#124846=CARTESIAN_POINT('Ctrl Pts',(-9.77259126592953,11.8850737198016,
9.63151286255959));
#124847=CARTESIAN_POINT('Ctrl Pts',(-11.0216974203312,11.9640572794716,
10.0615941798161));
#124848=CARTESIAN_POINT('Ctrl Pts',(-11.3442621578162,12.0430408391418,
11.3426826912335));
#124849=CARTESIAN_POINT('Ctrl Pts',(-10.4477612855078,12.1220243988118,
12.3130050437705));
#124850=CARTESIAN_POINT('Ctrl Pts',(-9.14520306579991,12.2010079584819,
12.0926070447803));
#124851=CARTESIAN_POINT('Ctrl Pts',(-8.61782701892134,12.279991518152,10.8813648817977));
#124852=CARTESIAN_POINT('Ctrl Pts',(-9.34390233273922,12.3589750778221,
9.77770260286736));
#124853=CARTESIAN_POINT('Ctrl Pts',(-10.6649569948427,12.4379586374922,
9.78251126319615));
#124854=CARTESIAN_POINT('Ctrl Pts',(-11.3830099145748,12.5169421971623,
10.8913953614281));
#124855=CARTESIAN_POINT('Ctrl Pts',(-10.8468118025409,12.5959257568324,
12.0988130567366));
#124856=CARTESIAN_POINT('Ctrl Pts',(-9.54276046145547,12.6749093165025,
12.3096711804419));
#124857=CARTESIAN_POINT('Ctrl Pts',(-8.65318901050312,12.7538928761726,
11.3329956779777));
#124858=CARTESIAN_POINT('Ctrl Pts',(-8.98532945352617,12.8328764358426,
10.0540272579587));
#124859=CARTESIAN_POINT('Ctrl Pts',(-10.2369934859239,12.9118599955128,
9.6335268605737));
#124860=CARTESIAN_POINT('Ctrl Pts',(-11.2749857449341,12.9908435551828,
10.451071347098));
#124861=CARTESIAN_POINT('Ctrl Pts',(-11.1542469424753,13.0698334244205,
11.7688789796044));
#124862=CARTESIAN_POINT('Ctrl Pts',(-10.3794236209914,13.1224954404349,
12.1788445786523));
#124863=CARTESIAN_POINT('Ctrl Pts',(-9.99037010550519,13.1488296032259,
12.17565058611));
#124864=CARTESIAN_POINT('Ctrl Pts',(-10.5513377582739,3.49023542398123,
9.85212015063649));
#124865=CARTESIAN_POINT('Ctrl Pts',(-10.9312228209415,3.5165707817884,10.0345723048824));
#124866=CARTESIAN_POINT('Ctrl Pts',(-11.4891903864173,3.56923399281895,
10.8028282163118));
#124867=CARTESIAN_POINT('Ctrl Pts',(-10.9780359458523,3.64822505707284,
12.1419401477623));
#124868=CARTESIAN_POINT('Ctrl Pts',(-9.57869304575365,3.72720861674294,
12.4418668537216));
#124869=CARTESIAN_POINT('Ctrl Pts',(-8.56207944446872,3.80619217641302,
11.4359406428495));
#124870=CARTESIAN_POINT('Ctrl Pts',(-8.84912328417233,3.88517573608311,
10.0337852145809));
#124871=CARTESIAN_POINT('Ctrl Pts',(-10.1800355825104,3.9641592957532,9.50831872021641));
#124872=CARTESIAN_POINT('Ctrl Pts',(-11.3475870292958,4.04314285542329,
10.3353655847789));
#124873=CARTESIAN_POINT('Ctrl Pts',(-11.2931069312924,4.12212641509338,
11.7652715684391));
#124874=CARTESIAN_POINT('Ctrl Pts',(-10.0659279018402,4.20110997476347,
12.5011141343889));
#124875=CARTESIAN_POINT('Ctrl Pts',(-8.77897424901355,4.28009353443356,
11.8756823744131));
#124876=CARTESIAN_POINT('Ctrl Pts',(-8.59931962391916,4.35907709410364,
10.4561070043562));
#124877=CARTESIAN_POINT('Ctrl Pts',(-9.68989693924451,4.43806065377374,
9.52977850624579));
#124878=CARTESIAN_POINT('Ctrl Pts',(-11.061694101878,4.51704421344381,9.9367380303017));
#124879=CARTESIAN_POINT('Ctrl Pts',(-11.4706787175616,4.59602777311392,
11.3079354034798));
#124880=CARTESIAN_POINT('Ctrl Pts',(-10.5459553780284,4.67501133278399,
12.3998755546594));
#124881=CARTESIAN_POINT('Ctrl Pts',(-9.12612432749545,4.75399489245409,
12.2223178575684));
#124882=CARTESIAN_POINT('Ctrl Pts',(-8.49878063982344,4.83297845212418,
10.9362821930396));
#124883=CARTESIAN_POINT('Ctrl Pts',(-9.23284072504908,4.91196201179426,
9.70803017810119));
#124884=CARTESIAN_POINT('Ctrl Pts',(-10.6626108773617,4.99094557146436,
9.65142063061672));
#124885=CARTESIAN_POINT('Ctrl Pts',(-11.4914822558648,5.06992913113444,
10.8177909283396));
#124886=CARTESIAN_POINT('Ctrl Pts',(-10.9677801639641,5.14891269080454,
12.1494002793753));
#124887=CARTESIAN_POINT('Ctrl Pts',(-9.56643185642774,5.22789625047462,
12.4386584478327));
#124888=CARTESIAN_POINT('Ctrl Pts',(-8.55827143827977,5.30687981014471,
11.4232472258526));
#124889=CARTESIAN_POINT('Ctrl Pts',(-8.85756458462907,5.3858633698148,10.0240077972755));
#124890=CARTESIAN_POINT('Ctrl Pts',(-10.1928927330077,5.46484692948489,
9.50986180038816));
#124891=CARTESIAN_POINT('Ctrl Pts',(-11.3532931611411,5.54383048915498,
10.3470703869731));
#124892=CARTESIAN_POINT('Ctrl Pts',(-11.2864390195152,5.62281404882507,
11.77639816362));
#124893=CARTESIAN_POINT('Ctrl Pts',(-10.0529580077071,5.70179760849516,
12.5016374093425));
#124894=CARTESIAN_POINT('Ctrl Pts',(-8.77145121782494,5.78078116816525,
11.865093838492));
#124895=CARTESIAN_POINT('Ctrl Pts',(-8.60407265247242,5.85976472783534,
10.4440267092764));
#124896=CARTESIAN_POINT('Ctrl Pts',(-9.70261211966464,5.93874828750542,
9.52715244908236));
#124897=CARTESIAN_POINT('Ctrl Pts',(-11.0708423276095,6.01773184717552,
9.94595248257362));
#124898=CARTESIAN_POINT('Ctrl Pts',(-11.4679628177349,6.0967154068456,11.3206316037791));
#124899=CARTESIAN_POINT('Ctrl Pts',(-10.533838809079,6.17569896651569,12.4045410586809));
#124900=CARTESIAN_POINT('Ctrl Pts',(-9.11559492406168,6.25468252618578,
12.2147210055197));
#124901=CARTESIAN_POINT('Ctrl Pts',(-8.49938728806626,6.33366608585587,
10.9233126582846));
#124902=CARTESIAN_POINT('Ctrl Pts',(-9.24403320601036,6.41264964552595,
9.70144939798937));
#124903=CARTESIAN_POINT('Ctrl Pts',(-10.6742391555871,6.49163320519605,
9.65719658152432));
#124904=CARTESIAN_POINT('Ctrl Pts',(-11.4930010304939,6.57061676486612,
10.8306855512928));
#124905=CARTESIAN_POINT('Ctrl Pts',(-10.9578121210141,6.64960032453624,
12.1577199145024));
#124906=CARTESIAN_POINT('Ctrl Pts',(-9.55401666267395,6.72858388420629,
12.4348582934994));
#124907=CARTESIAN_POINT('Ctrl Pts',(-8.55466800447861,6.80756744387642,
11.4107735170613));
#124908=CARTESIAN_POINT('Ctrl Pts',(-8.86604073834288,6.88655100354648,
10.0141725036809));
#124909=CARTESIAN_POINT('Ctrl Pts',(-10.2057617455338,6.96553456321659,
9.51158421008386));
#124910=CARTESIAN_POINT('Ctrl Pts',(-11.3588845715633,7.04451812288666,
10.3587885054337));
#124911=CARTESIAN_POINT('Ctrl Pts',(-11.2796821721034,7.12350168255676,
11.7874852366852));
#124912=CARTESIAN_POINT('Ctrl Pts',(-10.0399804526184,7.20248524222684,
12.5020389552223));
#124913=CARTESIAN_POINT('Ctrl Pts',(-8.76402184912772,7.28146880189694,
11.8544457093129));
#124914=CARTESIAN_POINT('Ctrl Pts',(-8.60892890659698,7.36045236156703,
10.4319853235212));
#124915=CARTESIAN_POINT('Ctrl Pts',(-9.71535002841199,7.43943592123711,
9.52463772134717));
#124916=CARTESIAN_POINT('Ctrl Pts',(-11.0799103239017,7.51841948090721,
9.9552449320883));
#124917=CARTESIAN_POINT('Ctrl Pts',(-11.4651374506592,7.59740304057729,
11.333304230805));
#124918=CARTESIAN_POINT('Ctrl Pts',(-10.5216823059128,7.67638660024737,
12.4091014978681));
#124919=CARTESIAN_POINT('Ctrl Pts',(-9.1051315953463,7.75537015991747,12.2070335529509));
#124920=CARTESIAN_POINT('Ctrl Pts',(-8.50010596323409,7.83435371958756,
10.9103487977168));
#124921=CARTESIAN_POINT('Ctrl Pts',(-9.25528214351071,7.91333727925765,
9.6949656043526));
#124922=CARTESIAN_POINT('Ctrl Pts',(-10.685817084663,7.99232083892774,9.66307278209282));
#124923=CARTESIAN_POINT('Ctrl Pts',(-11.4944083293544,8.07130439859782,
10.8435928238447));
#124924=CARTESIAN_POINT('Ctrl Pts',(-10.9477725591963,8.15028795826791,
12.1659531018147));
#124925=CARTESIAN_POINT('Ctrl Pts',(-9.54163477012829,8.229271517938,12.4309510039276));
#124926=CARTESIAN_POINT('Ctrl Pts',(-8.55117248954609,8.30825507760809,
11.3982691358224));
#124927=CARTESIAN_POINT('Ctrl Pts',(-8.87460156212072,8.38723863727818,
10.0044108198581));
#124928=CARTESIAN_POINT('Ctrl Pts',(-10.2186153942451,8.46622219694826,
9.51341775572429));
#124929=CARTESIAN_POINT('Ctrl Pts',(-11.3643745175839,8.54520575661836,
10.3705545016729));
#124930=CARTESIAN_POINT('Ctrl Pts',(-11.2728297740467,8.62418931628843,
11.7985135101531));
#124931=CARTESIAN_POINT('Ctrl Pts',(-10.0269999123061,8.70317287595854,
12.5023283477097));
#124932=CARTESIAN_POINT('Ctrl Pts',(-8.75668476777029,8.78215643562862,
11.8437337808233));
#124933=CARTESIAN_POINT('Ctrl Pts',(-8.61388902846928,8.86113999529871,
10.4199863499891));
#124934=CARTESIAN_POINT('Ctrl Pts',(-9.72810919124724,8.94012355496881,
9.5222331551586));
#124935=CARTESIAN_POINT('Ctrl Pts',(-11.0888976860354,9.01910711463889,
9.9646153908119));
#124936=CARTESIAN_POINT('Ctrl Pts',(-11.4622026854927,9.09809067430898,
11.3459519708493));
#124937=CARTESIAN_POINT('Ctrl Pts',(-10.5094868500547,9.17707423397907,
12.4135567230282));
#124938=CARTESIAN_POINT('Ctrl Pts',(-9.09473508418051,9.25605779364916,
12.1992559742537));
#124939=CARTESIAN_POINT('Ctrl Pts',(-8.50093663167824,9.33504135331924,
10.8973916311767));
#124940=CARTESIAN_POINT('Ctrl Pts',(-9.26658668720091,9.41402491298935,
9.68857925431773));
#124941=CARTESIAN_POINT('Ctrl Pts',(-10.6973438055201,9.49300847265941,
9.66904880761934));
#124942=CARTESIAN_POINT('Ctrl Pts',(-11.4957040445425,9.57199203232953,
10.8565117749229));
#124943=CARTESIAN_POINT('Ctrl Pts',(-10.9376622296101,9.6509755919996,12.1740992303717));
#124944=CARTESIAN_POINT('Ctrl Pts',(-9.52928710254954,9.7299591516697,12.4269368688805));
#124945=CARTESIAN_POINT('Ctrl Pts',(-8.54778515488208,9.80894271133978,
11.3857350168392));
#124946=CARTESIAN_POINT('Ctrl Pts',(-8.8832464165401,9.88792627100986,9.9947234741494));
#124947=CARTESIAN_POINT('Ctrl Pts',(-10.2314527195007,9.96690983067997,
9.51536230068326));
#124948=CARTESIAN_POINT('Ctrl Pts',(-11.3697625892266,10.04589339035,10.382367497008));
#124949=CARTESIAN_POINT('Ctrl Pts',(-11.265882337025,10.1248769500202,11.8094821606464));
#124950=CARTESIAN_POINT('Ctrl Pts',(-10.014017355979,10.2038605096902,12.5025055651571));
#124951=CARTESIAN_POINT('Ctrl Pts',(-8.74944052160167,10.2828440693603,
11.8329588528764));
#124952=CARTESIAN_POINT('Ctrl Pts',(-8.61895264772564,10.3618276290304,
10.4080306846023));
#124953=CARTESIAN_POINT('Ctrl Pts',(-9.74088865547793,10.4408111887005,
9.51993893006537));
#124954=CARTESIAN_POINT('Ctrl Pts',(-11.0978037429465,10.5197947483706,
9.97406315907262));
#124955=CARTESIAN_POINT('Ctrl Pts',(-11.4591587413663,10.5987783080407,
11.3585738795403));
#124956=CARTESIAN_POINT('Ctrl Pts',(-10.4972533521105,10.6777618677108,
12.4179064014977));
#124957=CARTESIAN_POINT('Ctrl Pts',(-9.08440616684122,10.7567454273809,
12.1913888501644));
#124958=CARTESIAN_POINT('Ctrl Pts',(-8.50187923138316,10.8357289870509,
10.8844421261351));
#124959=CARTESIAN_POINT('Ctrl Pts',(-9.27794599298326,10.914712546721,9.68229082475239));
#124960=CARTESIAN_POINT('Ctrl Pts',(-10.7088184575185,10.9936961063911,
9.6751242118605));
#124961=CARTESIAN_POINT('Ctrl Pts',(-11.4968880792509,11.0726796660612,
10.8694414399576));
#124962=CARTESIAN_POINT('Ctrl Pts',(-10.9274818872825,11.1516632257313,
12.1821576918168));
#124963=CARTESIAN_POINT('Ctrl Pts',(-9.51697458168635,11.2306467854014,
12.4228161882874));
#124964=CARTESIAN_POINT('Ctrl Pts',(-8.54450625383342,11.3096303450715,
11.373172095611));
#124965=CARTESIAN_POINT('Ctrl Pts',(-8.89197465529891,11.3886139047415,
9.98511119063623));
#124966=CARTESIAN_POINT('Ctrl Pts',(-10.2442727643307,11.4675974644117,
9.51741769832237));
#124967=CARTESIAN_POINT('Ctrl Pts',(-11.375048381179,11.5465810240817,10.3942266121662));
#124968=CARTESIAN_POINT('Ctrl Pts',(-11.2588403855452,11.6255645837519,
11.8203903638361));
#124969=CARTESIAN_POINT('Ctrl Pts',(-10.0010337419502,11.7045481434219,
12.5025706045647));
#124970=CARTESIAN_POINT('Ctrl Pts',(-8.74228967277683,11.783531703092,11.8221217103547));
#124971=CARTESIAN_POINT('Ctrl Pts',(-8.62411934547226,11.8625152627621,
10.3961192578091));
#124972=CARTESIAN_POINT('Ctrl Pts',(-9.7536875452706,11.9414988224322,9.51775514486607));
#124973=CARTESIAN_POINT('Ctrl Pts',(-11.1066276791042,12.0204823821023,
9.98358767069083));
#124974=CARTESIAN_POINT('Ctrl Pts',(-11.4560061347023,12.0994659417724,
11.3711687469525));
#124975=CARTESIAN_POINT('Ctrl Pts',(-10.4849821701748,12.1784495014425,
12.422150722245));
#124976=CARTESIAN_POINT('Ctrl Pts',(-9.07414668122336,12.2574330611125,
12.1834317813448));
#124977=CARTESIAN_POINT('Ctrl Pts',(-8.50293164322984,12.3364166207826,
10.8715031447629));
#124978=CARTESIAN_POINT('Ctrl Pts',(-9.28936314770077,12.4154001804527,
9.67609714495959));
#124979=CARTESIAN_POINT('Ctrl Pts',(-10.7202326258867,12.4943837401228,
9.68130553299437));
#124980=CARTESIAN_POINT('Ctrl Pts',(-11.4979748617236,12.5733672997929,
10.8823674243165));
#124981=CARTESIAN_POINT('Ctrl Pts',(-10.9172044100689,12.652350859463,12.1901536781328));
#124982=CARTESIAN_POINT('Ctrl Pts',(-9.50475168159853,12.7313344191331,
12.4185397261082));
#124983=CARTESIAN_POINT('Ctrl Pts',(-8.54123315784066,12.8103179788032,
11.3606764849742));
#124984=CARTESIAN_POINT('Ctrl Pts',(-8.90098331506439,12.8893015384733,
9.9753917361545));
#124985=CARTESIAN_POINT('Ctrl Pts',(-10.2566939546601,12.9682850981434,
9.51993655973871));
#124986=CARTESIAN_POINT('Ctrl Pts',(-11.3809710073947,13.0472686578134,
10.4054407605748));
#124987=CARTESIAN_POINT('Ctrl Pts',(-11.2501955957278,13.1262585270511,
11.8327932945507));
#124988=CARTESIAN_POINT('Ctrl Pts',(-10.4109638262168,13.1789205430655,
12.276837950394));
#124989=CARTESIAN_POINT('Ctrl Pts',(-9.9895696048725,13.2052547058564,12.2733784520301));
#124990=CARTESIAN_POINT('Ctrl Pts',(-10.5936512295213,3.54666052661181,
9.76402391512065));
#124991=CARTESIAN_POINT('Ctrl Pts',(-11.0026912982362,3.57299588441898,
9.96047870906769));
#124992=CARTESIAN_POINT('Ctrl Pts',(-11.6034811521994,3.62565909544952,
10.787695890483));
#124993=CARTESIAN_POINT('Ctrl Pts',(-11.0530971859957,3.70465015970341,
12.229580529513));
#124994=CARTESIAN_POINT('Ctrl Pts',(-9.54635903737612,3.78363371937351,
12.5525256844331));
#124995=CARTESIAN_POINT('Ctrl Pts',(-8.45172347996309,3.86261727904359,
11.4693977416606));
#124996=CARTESIAN_POINT('Ctrl Pts',(-8.76079704840517,3.94160083871369,
9.95963121201489));
#124997=CARTESIAN_POINT('Ctrl Pts',(-10.1938527577895,4.02058439838376,
9.39383678605651));
#124998=CARTESIAN_POINT('Ctrl Pts',(-11.4510101744767,4.09956795805386,
10.2843569447999));
#124999=CARTESIAN_POINT('Ctrl Pts',(-11.3923488971039,4.17855151772395,
11.8240037993117));
#125000=CARTESIAN_POINT('Ctrl Pts',(-10.0709876648205,4.25753507739404,
12.6163200110253));
#125001=CARTESIAN_POINT('Ctrl Pts',(-8.68526429131249,4.33651863706412,
11.9428882938621));
#125002=CARTESIAN_POINT('Ctrl Pts',(-8.49182172824476,4.41550219673422,
10.4143648956623));
#125003=CARTESIAN_POINT('Ctrl Pts',(-9.66609748646237,4.49448575640431,
9.41694354442816));
#125004=CARTESIAN_POINT('Ctrl Pts',(-11.143175847286,4.57346931607439,9.8551359558777));
#125005=CARTESIAN_POINT('Ctrl Pts',(-11.5835487698954,4.65245287574449,
11.3315684952565));
#125006=CARTESIAN_POINT('Ctrl Pts',(-10.5878557682048,4.73143643541457,
12.5073116827738));
#125007=CARTESIAN_POINT('Ctrl Pts',(-9.05905706684169,4.81041999508466,
12.3161269804615));
#125008=CARTESIAN_POINT('Ctrl Pts',(-8.38356668743254,4.88940355475475,
10.9313920480199));
#125009=CARTESIAN_POINT('Ctrl Pts',(-9.17396361852812,4.96838711442483,
9.60887548192595));
#125010=CARTESIAN_POINT('Ctrl Pts',(-10.7134642170556,5.04737067409493,
9.54792132639699));
#125011=CARTESIAN_POINT('Ctrl Pts',(-11.6059489155532,5.126354233765,10.8038069444767));
#125012=CARTESIAN_POINT('Ctrl Pts',(-11.042054304502,5.20533779343511,12.2376132032017));
#125013=CARTESIAN_POINT('Ctrl Pts',(-9.5331568396135,5.28432135310519,12.5490710432952));
#125014=CARTESIAN_POINT('Ctrl Pts',(-8.44762322105251,5.36330491277529,
11.4557301440873));
#125015=CARTESIAN_POINT('Ctrl Pts',(-8.76988619261797,5.44228847244537,
9.94910340810924));
#125016=CARTESIAN_POINT('Ctrl Pts',(-10.207696654904,5.52127203211547,9.3954982928687));
#125017=CARTESIAN_POINT('Ctrl Pts',(-11.4571542343291,5.60025559178554,
10.2969600544358));
#125018=CARTESIAN_POINT('Ctrl Pts',(-11.3851692436782,5.67923915145565,
11.8359843263305));
#125019=CARTESIAN_POINT('Ctrl Pts',(-10.0570223713442,5.75822271112572,
12.6168834457166));
#125020=CARTESIAN_POINT('Ctrl Pts',(-8.67716389069992,5.83720627079582,
11.9314871204905));
#125021=CARTESIAN_POINT('Ctrl Pts',(-8.49693953706932,5.9161898304659,10.401357475221));
#125022=CARTESIAN_POINT('Ctrl Pts',(-9.6797885177344,5.995173390136,9.41411594548272));
#125023=CARTESIAN_POINT('Ctrl Pts',(-11.1530261711066,6.07415694980609,
9.86505758892115));
#125024=CARTESIAN_POINT('Ctrl Pts',(-11.5806244331394,6.15314050947617,
11.3452390897421));
#125025=CARTESIAN_POINT('Ctrl Pts',(-10.5748092899862,6.23212406914626,
12.5123352498288));
#125026=CARTESIAN_POINT('Ctrl Pts',(-9.04771956419327,6.31110762881636,
12.3079470934657));
#125027=CARTESIAN_POINT('Ctrl Pts',(-8.38421989405561,6.39009118848643,
10.9174271415028));
#125028=CARTESIAN_POINT('Ctrl Pts',(-9.18601508785768,6.46907474815653,
9.60178964725208));
#125029=CARTESIAN_POINT('Ctrl Pts',(-10.725984929744,6.54805830782661,9.55414056370933));
#125030=CARTESIAN_POINT('Ctrl Pts',(-11.6075842514474,6.62704186749671,
10.8176911899423));
#125031=CARTESIAN_POINT('Ctrl Pts',(-11.0313212450217,6.70602542716679,
12.2465713446463));
#125032=CARTESIAN_POINT('Ctrl Pts',(-9.51978881805855,6.78500898683688,
12.5449792388459));
#125033=CARTESIAN_POINT('Ctrl Pts',(-8.44374323482906,6.86399254650697,
11.4422991166463));
#125034=CARTESIAN_POINT('Ctrl Pts',(-8.77901286496774,6.94297610617706,
9.93851328608784));
#125035=CARTESIAN_POINT('Ctrl Pts',(-10.2215533244214,7.02195966584715,
9.39735289219234));
#125036=CARTESIAN_POINT('Ctrl Pts',(-11.4631747682434,7.10094322551724,
10.3095775023202));
#125037=CARTESIAN_POINT('Ctrl Pts',(-11.3778938290828,7.17992678518733,
11.8479222980334));
#125038=CARTESIAN_POINT('Ctrl Pts',(-10.0430488289575,7.25891034485742,
12.6173158090032));
#125039=CARTESIAN_POINT('Ctrl Pts',(-8.66916434088588,7.3378939045275,11.9200217802622));
#125040=CARTESIAN_POINT('Ctrl Pts',(-8.50216849370914,7.41687746419759,
10.3883919502746));
#125041=CARTESIAN_POINT('Ctrl Pts',(-9.69350402166268,7.49586102386769,
9.41140822015553));
#125042=CARTESIAN_POINT('Ctrl Pts',(-11.1627901081258,7.57484458353777,
9.875063205255));
#125043=CARTESIAN_POINT('Ctrl Pts',(-11.5775822278612,7.65382814320786,
11.3588843017781));
#125044=CARTESIAN_POINT('Ctrl Pts',(-10.5617198127228,7.73281170287795,
12.517245688648));
#125045=CARTESIAN_POINT('Ctrl Pts',(-9.03645320729398,7.81179526254804,
12.2996696526396));
#125046=CARTESIAN_POINT('Ctrl Pts',(-8.38499372532438,7.89077882221813,
10.9034683446493));
#125047=CARTESIAN_POINT('Ctrl Pts',(-9.19812734659141,7.96976238188822,
9.59480824246587));
#125048=CARTESIAN_POINT('Ctrl Pts',(-10.7384514291415,8.04874594155832,
9.56046774453458));
#125049=CARTESIAN_POINT('Ctrl Pts',(-11.6090995561519,8.12772950122838,
10.8315890558243));
#125050=CARTESIAN_POINT('Ctrl Pts',(-11.0205111778215,8.20671306089849,
12.2554364036731));
#125051=CARTESIAN_POINT('Ctrl Pts',(-9.50645665347662,8.28569662056857,
12.5407720768592));
#125052=CARTESIAN_POINT('Ctrl Pts',(-8.43997944991436,8.36468018023866,
11.428835062742));
#125053=CARTESIAN_POINT('Ctrl Pts',(-8.78823070554761,8.44366373990875,
9.92800242316098));
#125054=CARTESIAN_POINT('Ctrl Pts',(-10.2353934509987,8.52264729957884,
9.39932715680145));
#125055=CARTESIAN_POINT('Ctrl Pts',(-11.4690860506765,8.60163085924892,
10.3222465024552));
#125056=CARTESIAN_POINT('Ctrl Pts',(-11.3705155306249,8.68061441891903,
11.8597969574513));
#125057=CARTESIAN_POINT('Ctrl Pts',(-10.0290720722405,8.7595979785891,12.6176274114709));
#125058=CARTESIAN_POINT('Ctrl Pts',(-8.6612641611801,8.83858153825921,11.9084877443233));
#125059=CARTESIAN_POINT('Ctrl Pts',(-8.50750928962575,8.91756509792929,
10.3754720925586));
#125060=CARTESIAN_POINT('Ctrl Pts',(-9.70724241086445,8.99654865759937,
9.40881911093368));
#125061=CARTESIAN_POINT('Ctrl Pts',(-11.1724672225638,9.07553221726946,
9.88515281776378));
#125062=CARTESIAN_POINT('Ctrl Pts',(-11.5744222285264,9.15451577693955,
11.3725027168337));
#125063=CARTESIAN_POINT('Ctrl Pts',(-10.548588393269,9.23349933660964,12.5220428385881));
#125064=CARTESIAN_POINT('Ctrl Pts',(-9.02525879598499,9.31248289627973,
12.2912951687828));
#125065=CARTESIAN_POINT('Ctrl Pts',(-8.38588814500775,9.39146645594982,
10.8895167555695));
#125066=CARTESIAN_POINT('Ctrl Pts',(-9.21029947911844,9.47045001561991,
9.58793175977726));
#125067=CARTESIAN_POINT('Ctrl Pts',(-10.7508627902472,9.54943357529,9.56690241157533));
#125068=CARTESIAN_POINT('Ctrl Pts',(-11.6104947134815,9.62841713496008,
10.8454994965235));
#125069=CARTESIAN_POINT('Ctrl Pts',(-11.009624911645,9.70740069463019,12.264207722454));
#125070=CARTESIAN_POINT('Ctrl Pts',(-9.49316134052218,9.78638425430025,
12.5364498693368));
#125071=CARTESIAN_POINT('Ctrl Pts',(-8.43633214776987,9.86536781397036,
11.4153389888133));
#125072=CARTESIAN_POINT('Ctrl Pts',(-8.79753902586138,9.94435137364043,
9.91757160356907));
#125073=CARTESIAN_POINT('Ctrl Pts',(-10.2492160013451,10.0233349333105,
9.4014209395842));
#125074=CARTESIAN_POINT('Ctrl Pts',(-11.4748876401873,10.1023184929806,
10.3349661087214));
#125075=CARTESIAN_POINT('Ctrl Pts',(-11.363034899255,10.1813020526507,11.8716074180152));
#125076=CARTESIAN_POINT('Ctrl Pts',(-10.0150931447859,10.2602856123208,
12.6178182298103));
#125077=CARTESIAN_POINT('Ctrl Pts',(-8.65346394147736,10.3392691719908,
11.8968858739132));
#125078=CARTESIAN_POINT('Ctrl Pts',(-8.51296152603122,10.4182527316609,
10.3625988667544));
#125079=CARTESIAN_POINT('Ctrl Pts',(-9.72100265953115,10.497236291331,9.40634881114567));
#125080=CARTESIAN_POINT('Ctrl Pts',(-11.1820567918543,10.5762198510011,
9.89532567307804));
#125081=CARTESIAN_POINT('Ctrl Pts',(-11.5711446710833,10.6552034106712,
11.3860933180592));
#125082=CARTESIAN_POINT('Ctrl Pts',(-10.5354160121161,10.7341869703413,
12.5267263414547));
#125083=CARTESIAN_POINT('Ctrl Pts',(-9.01413716612003,10.8131705300114,
12.2828242672015));
#125084=CARTESIAN_POINT('Ctrl Pts',(-8.3869030863307,10.8921540896815,10.8755734159845));
#125085=CARTESIAN_POINT('Ctrl Pts',(-9.22253057655917,10.9711376493516,
9.58116071265196));
#125086=CARTESIAN_POINT('Ctrl Pts',(-10.7632180863699,11.0501212090216,
9.5734440843403));
#125087=CARTESIAN_POINT('Ctrl Pts',(-11.6117696191991,11.1291047686917,
10.8594214734424));
#125088=CARTESIAN_POINT('Ctrl Pts',(-10.9986632594654,11.2080883283618,
12.2728846459425));
#125089=CARTESIAN_POINT('Ctrl Pts',(-9.47990387168526,11.2870718880319,
12.5320129392265));
#125090=CARTESIAN_POINT('Ctrl Pts',(-8.43280160118601,11.366055447702,11.4018119021562));
#125091=CARTESIAN_POINT('Ctrl Pts',(-8.80693713000531,11.4450390073721,
9.90722160696449));
#125092=CARTESIAN_POINT('Ctrl Pts',(-10.2630199450469,11.5240225670421,
9.40363408264815));
#125093=CARTESIAN_POINT('Ctrl Pts',(-11.4805791003575,11.6030061267123,
10.3477353743652));
#125094=CARTESIAN_POINT('Ctrl Pts',(-11.3554524997339,11.6819896863823,
11.8833527921317));
#125095=CARTESIAN_POINT('Ctrl Pts',(-10.0011130784543,11.7609732460524,
12.6178882607918));
#125096=CARTESIAN_POINT('Ctrl Pts',(-8.64576428707628,11.8399568057225,
11.885217014152));
#125097=CARTESIAN_POINT('Ctrl Pts',(-8.51852475188289,11.9189403653926,
10.3497732747195));
#125098=CARTESIAN_POINT('Ctrl Pts',(-9.73478382461175,11.9979239250627,
9.40399742717256));
#125099=CARTESIAN_POINT('Ctrl Pts',(-11.1915579378771,12.0769074847328,
9.90558116156562));
#125100=CARTESIAN_POINT('Ctrl Pts',(-11.5677501115883,12.1558910444029,
11.3996548026714));
#125101=CARTESIAN_POINT('Ctrl Pts',(-10.5222030548419,12.234874604073,12.5312964007194));
#125102=CARTESIAN_POINT('Ctrl Pts',(-9.00309029664685,12.313858163743,12.2742565179095));
#125103=CARTESIAN_POINT('Ctrl Pts',(-8.38803626753834,12.3928417234132,
10.861641407728));
#125104=CARTESIAN_POINT('Ctrl Pts',(-9.23482396266229,12.4718252830832,
9.5744916870518));
#125105=CARTESIAN_POINT('Ctrl Pts',(-10.7755082569308,12.5508088427533,
9.58009980279261));
#125106=CARTESIAN_POINT('Ctrl Pts',(-11.6129398088724,12.6297924024234,
10.8733394872047));
#125107=CARTESIAN_POINT('Ctrl Pts',(-10.987597017597,12.7087759620935,12.2814942995286));
#125108=CARTESIAN_POINT('Ctrl Pts',(-9.46674290174155,12.7877595217636,
12.5274082717744));
#125109=CARTESIAN_POINT('Ctrl Pts',(-8.42927730517822,12.8667430814337,
11.3883572919707));
#125110=CARTESIAN_POINT('Ctrl Pts',(-8.8166371766026,12.9457266411038,9.89675621435035));
#125111=CARTESIAN_POINT('Ctrl Pts',(-10.2763944233962,13.0247102007739,
9.40634625890373));
#125112=CARTESIAN_POINT('Ctrl Pts',(-11.4869562698552,13.1036937604439,
10.3598101740517));
#125113=CARTESIAN_POINT('Ctrl Pts',(-11.3461442489803,13.1826836296816,
11.896707609497));
#125114=CARTESIAN_POINT('Ctrl Pts',(-10.442504031442,13.2353456456961,12.3748313221357));
#125115=CARTESIAN_POINT('Ctrl Pts',(-9.98876910423983,13.261679808487,12.3711063179499));
#125116=CARTESIAN_POINT('Ctrl Pts',(-10.6359647007688,3.60308562924238,
9.67592767960482));
#125117=CARTESIAN_POINT('Ctrl Pts',(-11.074159775531,3.62942098704956,9.88638511325299));
#125118=CARTESIAN_POINT('Ctrl Pts',(-11.7177719179817,3.6820841980801,10.7725635646542));
#125119=CARTESIAN_POINT('Ctrl Pts',(-11.1281584261389,3.76107526233399,
12.3172209112638));
#125120=CARTESIAN_POINT('Ctrl Pts',(-9.51402502899859,3.84005882200409,
12.6631845151446));
#125121=CARTESIAN_POINT('Ctrl Pts',(-8.34136751545742,3.91904238167417,
11.5028548404716));
#125122=CARTESIAN_POINT('Ctrl Pts',(-8.67247081263803,3.99802594134427,
9.88547720944895));
#125123=CARTESIAN_POINT('Ctrl Pts',(-10.2076699330686,4.07700950101435,
9.27935485189655));
#125124=CARTESIAN_POINT('Ctrl Pts',(-11.5544333196575,4.15599306068445,
10.233348304821));
#125125=CARTESIAN_POINT('Ctrl Pts',(-11.4915908629155,4.23497662035453,
11.8827360301843));
#125126=CARTESIAN_POINT('Ctrl Pts',(-10.0760474278007,4.31396018002462,
12.7315258876618));
#125127=CARTESIAN_POINT('Ctrl Pts',(-8.59155433361139,4.39294373969471,
12.010094213311));
#125128=CARTESIAN_POINT('Ctrl Pts',(-8.38432383257039,4.47192729936479,
10.3726227869686));
#125129=CARTESIAN_POINT('Ctrl Pts',(-9.64229803368022,4.5509108590349,9.3041085826105));
#125130=CARTESIAN_POINT('Ctrl Pts',(-11.224657592694,4.62989441870496,9.77353388145369));
#125131=CARTESIAN_POINT('Ctrl Pts',(-11.696418822229,4.70887797837507,11.3552015870332));
#125132=CARTESIAN_POINT('Ctrl Pts',(-10.6297561583812,4.78786153804515,
12.6147478108881));
#125133=CARTESIAN_POINT('Ctrl Pts',(-8.99198980618788,4.86684509771525,
12.4099361033547));
#125134=CARTESIAN_POINT('Ctrl Pts',(-8.26835273504166,4.94582865738532,
10.9265019030003));
#125135=CARTESIAN_POINT('Ctrl Pts',(-9.11508651200717,5.02481221705542,
9.50972078575068));
#125136=CARTESIAN_POINT('Ctrl Pts',(-10.7643175567494,5.10379577672551,
9.44442202217728));
#125137=CARTESIAN_POINT('Ctrl Pts',(-11.7204155752416,5.1827793363956,10.7898229606137));
#125138=CARTESIAN_POINT('Ctrl Pts',(-11.1163284450397,5.26176289606569,
12.3258261270282));
#125139=CARTESIAN_POINT('Ctrl Pts',(-9.4998818227993,5.34074645573578,12.6594836387575));
#125140=CARTESIAN_POINT('Ctrl Pts',(-8.33697500382525,5.41973001540587,
11.488213062322));
#125141=CARTESIAN_POINT('Ctrl Pts',(-8.68220780060687,5.49871357507595,
9.87419901894299));
#125142=CARTESIAN_POINT('Ctrl Pts',(-10.2225005768003,5.57769713474605,
9.28113478534924));
#125143=CARTESIAN_POINT('Ctrl Pts',(-11.5610153075171,5.65668069441612,
10.2468497218984));
#125144=CARTESIAN_POINT('Ctrl Pts',(-11.4838994678413,5.73566425408623,
11.8955704890411));
#125145=CARTESIAN_POINT('Ctrl Pts',(-10.0610867349812,5.8146478137563,12.7321294820906));
#125146=CARTESIAN_POINT('Ctrl Pts',(-8.58287656357489,5.89363137342641,
11.9978804024888));
#125147=CARTESIAN_POINT('Ctrl Pts',(-8.3898064216662,5.97261493309648,10.3586882411655));
#125148=CARTESIAN_POINT('Ctrl Pts',(-9.65696491580419,6.05159849276657,
9.30107944188306));
#125149=CARTESIAN_POINT('Ctrl Pts',(-11.2352100146035,6.13058205243667,
9.78416269526869));
#125150=CARTESIAN_POINT('Ctrl Pts',(-11.693286048544,6.20956561210675,11.369846575705));
#125151=CARTESIAN_POINT('Ctrl Pts',(-10.6157797708933,6.28854917177684,
12.6201294409768));
#125152=CARTESIAN_POINT('Ctrl Pts',(-8.97984420432487,6.36753273144694,
12.4011731814118));
#125153=CARTESIAN_POINT('Ctrl Pts',(-8.26905250004494,6.44651629111701,
10.9115416247212));
#125154=CARTESIAN_POINT('Ctrl Pts',(-9.12799696970499,6.52549985078712,
9.5021298965148));
#125155=CARTESIAN_POINT('Ctrl Pts',(-10.7777307039011,6.60448341045719,
9.4510845458943));
#125156=CARTESIAN_POINT('Ctrl Pts',(-11.7221674724009,6.68346697012729,
10.8046968285918));
#125157=CARTESIAN_POINT('Ctrl Pts',(-11.1048303690294,6.76245052979738,
12.3354227747902));
#125158=CARTESIAN_POINT('Ctrl Pts',(-9.48556097344312,6.84143408946747,
12.6551001841922));
#125159=CARTESIAN_POINT('Ctrl Pts',(-8.33281846517953,6.92041764913755,
11.4738247162312));
#125160=CARTESIAN_POINT('Ctrl Pts',(-8.69198499159258,6.99940120880765,
9.86285406849477));
#125161=CARTESIAN_POINT('Ctrl Pts',(-10.2373449033089,7.07838476847773,
9.28312157430081));
#125162=CARTESIAN_POINT('Ctrl Pts',(-11.5674649649235,7.15736832814783,
10.260366499207));
#125163=CARTESIAN_POINT('Ctrl Pts',(-11.4761054860619,7.2363518878179,11.9083593593815));
#125164=CARTESIAN_POINT('Ctrl Pts',(-10.0461172052965,7.31533544748801,
12.7325926627842));
#125165=CARTESIAN_POINT('Ctrl Pts',(-8.57430683264404,7.39431900715809,
11.9855978512114));
#125166=CARTESIAN_POINT('Ctrl Pts',(-8.39540808082131,7.47330256682818,
10.3447985770281));
#125167=CARTESIAN_POINT('Ctrl Pts',(-9.67165801491334,7.55228612649826,
9.2981787189639));
#125168=CARTESIAN_POINT('Ctrl Pts',(-11.2456698923498,7.63126968616836,
9.7948814784217));
#125169=CARTESIAN_POINT('Ctrl Pts',(-11.6900270050633,7.71025324583844,
11.3844643727514));
#125170=CARTESIAN_POINT('Ctrl Pts',(-10.601757319533,7.78923680550853,12.6253898794279));
#125171=CARTESIAN_POINT('Ctrl Pts',(-8.96777481924168,7.86822036517862,
12.3923057523283));
#125172=CARTESIAN_POINT('Ctrl Pts',(-8.26988148741464,7.94720392484871,
10.896587891582));
#125173=CARTESIAN_POINT('Ctrl Pts',(-9.14097254967212,8.0261874845188,9.49465088057913));
#125174=CARTESIAN_POINT('Ctrl Pts',(-10.7910857736198,8.10517104418889,
9.45786270697637));
#125175=CARTESIAN_POINT('Ctrl Pts',(-11.7237907829494,8.18415460385897,
10.8195852878039));
#125176=CARTESIAN_POINT('Ctrl Pts',(-11.0932497964466,8.26313816352907,
12.3449197055317));
#125177=CARTESIAN_POINT('Ctrl Pts',(-9.47127853682493,8.34212172319915,
12.6505931497907));
#125178=CARTESIAN_POINT('Ctrl Pts',(-8.32878641028264,8.42110528286925,
11.4594009896616));
#125179=CARTESIAN_POINT('Ctrl Pts',(-8.70185984897448,8.50008884253932,
9.85159402646389));
#125180=CARTESIAN_POINT('Ctrl Pts',(-10.2521715077521,8.57907240220943,
9.2852365578786));
#125181=CARTESIAN_POINT('Ctrl Pts',(-11.573797583769,8.65805596187951,10.2739385032375));
#125182=CARTESIAN_POINT('Ctrl Pts',(-11.4682012872031,8.7370395215496,11.9210804047493));
#125183=CARTESIAN_POINT('Ctrl Pts',(-10.031144232175,8.81602308121969,12.732926475232));
#125184=CARTESIAN_POINT('Ctrl Pts',(-8.56584355458991,8.89500664088978,
11.9732417078233));
#125185=CARTESIAN_POINT('Ctrl Pts',(-8.40112955078225,8.97399020055985,
10.3309578351283));
#125186=CARTESIAN_POINT('Ctrl Pts',(-9.68637563048165,9.05297376022996,
9.29540506670874));
#125187=CARTESIAN_POINT('Ctrl Pts',(-11.2560367590921,9.13195731990004,
9.80569024471567));
#125188=CARTESIAN_POINT('Ctrl Pts',(-11.68664177156,9.21094087957014,11.3990534628182));
#125189=CARTESIAN_POINT('Ctrl Pts',(-10.5876899364831,9.28992443924022,
12.6305289541479));
#125190=CARTESIAN_POINT('Ctrl Pts',(-8.95578250778944,9.3689079989103,12.3833343633119));
#125191=CARTESIAN_POINT('Ctrl Pts',(-8.27083965833728,9.44789155858041,
10.8816418799623));
#125192=CARTESIAN_POINT('Ctrl Pts',(-9.15401227103596,9.52687511825048,
9.48728426523676));
#125193=CARTESIAN_POINT('Ctrl Pts',(-10.8043817749742,9.60585867792059,
9.46475601553131));
#125194=CARTESIAN_POINT('Ctrl Pts',(-11.7252853824205,9.68484223759066,
10.8344872181243));
#125195=CARTESIAN_POINT('Ctrl Pts',(-11.0815875936799,9.76382579726076,
12.3543162145363));
#125196=CARTESIAN_POINT('Ctrl Pts',(-9.45703557849479,9.84280935693084,
12.6459628697931));
#125197=CARTESIAN_POINT('Ctrl Pts',(-8.32487914065766,9.92179291660094,
11.4449429607874));
#125198=CARTESIAN_POINT('Ctrl Pts',(-8.71183163518266,10.000776476271,9.84041973298876));
#125199=CARTESIAN_POINT('Ctrl Pts',(-10.2669792831896,10.0797600359411,
9.28747957848513));
#125200=CARTESIAN_POINT('Ctrl Pts',(-11.5800126911482,10.1587435956113,
10.2875647204351));
#125201=CARTESIAN_POINT('Ctrl Pts',(-11.4601874614852,10.2377271552814,
11.933732675384));
#125202=CARTESIAN_POINT('Ctrl Pts',(-10.0161689335928,10.3167107149515,
12.7331308944637));
#125203=CARTESIAN_POINT('Ctrl Pts',(-8.55748736135308,10.3956942746215,
11.9608128949501));
#125204=CARTESIAN_POINT('Ctrl Pts',(-8.4069704043368,10.4746778342916,10.3171670489067));
#125205=CARTESIAN_POINT('Ctrl Pts',(-9.70111666358434,10.5536613939617,
9.29275869222594));
#125206=CARTESIAN_POINT('Ctrl Pts',(-11.266309840762,10.6326449536318,9.81658818708347));
#125207=CARTESIAN_POINT('Ctrl Pts',(-11.6831306008003,10.7116285133019,
11.4136127565782));
#125208=CARTESIAN_POINT('Ctrl Pts',(-10.5735786721218,10.7906120729719,
12.6355462814118));
#125209=CARTESIAN_POINT('Ctrl Pts',(-8.94386816539882,10.8695956326421,
12.3742596842385));
#125210=CARTESIAN_POINT('Ctrl Pts',(-8.27192694127825,10.9485791923122,
10.8667047058338));
#125211=CARTESIAN_POINT('Ctrl Pts',(-9.16711516013507,11.0275627519822,
9.48003060055151));
#125212=CARTESIAN_POINT('Ctrl Pts',(-10.8176177152214,11.1065463116523,
9.4717639568201));
#125213=CARTESIAN_POINT('Ctrl Pts',(-11.7266511591474,11.1855298713225,
10.8494015069271));
#125214=CARTESIAN_POINT('Ctrl Pts',(-11.0698446316482,11.2645134309925,
12.3636116000683));
#125215=CARTESIAN_POINT('Ctrl Pts',(-9.44283316168417,11.3434969906625,
12.6412096901657));
#125216=CARTESIAN_POINT('Ctrl Pts',(-8.3210969485386,11.4224805503327,11.4304517087014));
#125217=CARTESIAN_POINT('Ctrl Pts',(-8.72189960471168,11.5014641100028,
9.82933202329279));
#125218=CARTESIAN_POINT('Ctrl Pts',(-10.2817671257633,11.5804476696729,
9.28985046697391));
#125219=CARTESIAN_POINT('Ctrl Pts',(-11.5861098195362,11.659431229343,10.301244136564));
#125220=CARTESIAN_POINT('Ctrl Pts',(-11.4520646139229,11.7384147890131,
11.9463152204272));
#125221=CARTESIAN_POINT('Ctrl Pts',(-10.0011924149583,11.8173983486832,
12.7332059170188));
#125222=CARTESIAN_POINT('Ctrl Pts',(-8.54923890137574,11.8963819083532,
11.9483123179489));
#125223=CARTESIAN_POINT('Ctrl Pts',(-8.41293015829353,11.9753654680233,
10.3034272916299));
#125224=CARTESIAN_POINT('Ctrl Pts',(-9.71588010395286,12.0543490276934,
9.29023970947901));
#125225=CARTESIAN_POINT('Ctrl Pts',(-11.27648819665,12.1333325873634,9.82757465244043));
#125226=CARTESIAN_POINT('Ctrl Pts',(-11.6794940884743,12.2123161470336,
11.4281408583904));
#125227=CARTESIAN_POINT('Ctrl Pts',(-10.5594239395087,12.2912997067037,
12.6404420791938));
#125228=CARTESIAN_POINT('Ctrl Pts',(-8.9320339120703,12.3702832663738,12.365081254474));
#125229=CARTESIAN_POINT('Ctrl Pts',(-8.27314089184689,12.4492668260438,
10.8517796706932));
#125230=CARTESIAN_POINT('Ctrl Pts',(-9.18028477762376,12.5282503857139,
9.47288622914401));
#125231=CARTESIAN_POINT('Ctrl Pts',(-10.8307838879748,12.607233945384,9.47889407259081));
#125232=CARTESIAN_POINT('Ctrl Pts',(-11.7279047560209,12.6862175050541,
10.8643115500932));
#125233=CARTESIAN_POINT('Ctrl Pts',(-11.057989625125,12.7652010647242,12.3728349209246));
#125234=CARTESIAN_POINT('Ctrl Pts',(-9.42873412188459,12.8441846243943,
12.6362768174407));
#125235=CARTESIAN_POINT('Ctrl Pts',(-8.31732145251579,12.9231681840643,
11.4160380989671));
#125236=CARTESIAN_POINT('Ctrl Pts',(-8.7322910381408,13.0021517437345,9.81812069254618));
#125237=CARTESIAN_POINT('Ctrl Pts',(-10.2960948921322,13.0811353034045,
9.29275595806876));
#125238=CARTESIAN_POINT('Ctrl Pts',(-11.5929415323158,13.1601188630747,
10.3141795875286));
#125239=CARTESIAN_POINT('Ctrl Pts',(-11.4420929022327,13.2391087323122,
11.9606219244432));
#125240=CARTESIAN_POINT('Ctrl Pts',(-10.4740442366673,13.2917707483266,
12.4728246938774));
#125241=CARTESIAN_POINT('Ctrl Pts',(-9.98796860360714,13.3181049111175,
12.4688341838699));
#125242=CARTESIAN_POINT('Ctrl Pts',(-11.2892917767063,13.1491947132283,
10.3057978051142));
#125243=CARTESIAN_POINT('Ctrl Pts',(-11.2911267665574,13.1493279265878,
10.3094867913697));
#125244=CARTESIAN_POINT('Ctrl Pts',(-11.2929458237144,13.149461539121,10.3131836711958));
#125245=CARTESIAN_POINT('Ctrl Pts',(-11.2965564276256,13.1497299497203,
10.320602301492));
#125246=CARTESIAN_POINT('Ctrl Pts',(-11.2983478787435,13.1498647487794,
10.3243240595053));
#125247=CARTESIAN_POINT('Ctrl Pts',(-11.3001231424463,13.15,10.3280535255874));
#125248=CARTESIAN_POINT('',(-10.685566134506,3.59949089696024,11.9587436199823));
#125249=CARTESIAN_POINT('Ctrl Pts',(-10.6861228805008,3.60000000000003,
11.9594385981141));
#125250=CARTESIAN_POINT('Ctrl Pts',(-10.7168289554558,3.60000000000002,
11.9427622376919));
#125251=CARTESIAN_POINT('Ctrl Pts',(-10.7466758757264,3.6,11.9246812723241));
#125252=CARTESIAN_POINT('Ctrl Pts',(-10.7755540070869,3.60000000000001,
11.9052191306961));
#125253=CARTESIAN_POINT('Ctrl Pts',(-10.815638348132,3.60000000000003,11.8782046707663));
#125254=CARTESIAN_POINT('Ctrl Pts',(-10.8538575727216,3.6,11.8485313428333));
#125255=CARTESIAN_POINT('Ctrl Pts',(-10.8901406100634,3.6,11.8164948795181));
#125256=CARTESIAN_POINT('Ctrl Pts',(-10.9070437155787,3.60000000000001,
11.80157011689));
#125257=CARTESIAN_POINT('Ctrl Pts',(-10.9235263388988,3.60000000000003,
11.7861317763512));
#125258=CARTESIAN_POINT('Ctrl Pts',(-10.939579659689,3.60000000000001,11.770206417048));
#125259=CARTESIAN_POINT('Ctrl Pts',(-10.9477051990523,3.6,11.7621456465954));
#125260=CARTESIAN_POINT('Ctrl Pts',(-10.955713805174,3.60000000000001,11.7539669214989));
#125261=CARTESIAN_POINT('Ctrl Pts',(-10.9636034932934,3.60000000000001,
11.7456755575237));
#125262=CARTESIAN_POINT('Ctrl Pts',(-10.9985464304682,3.60000000000002,
11.7089536230065));
#125263=CARTESIAN_POINT('Ctrl Pts',(-11.0311665020199,3.60000000000001,
11.6700183235567));
#125264=CARTESIAN_POINT('Ctrl Pts',(-11.0613843951033,3.59999999999998,
11.6291938939893));
#125265=CARTESIAN_POINT('Ctrl Pts',(-11.0826276826682,3.59999999999997,
11.6004941731127));
#125266=CARTESIAN_POINT('Ctrl Pts',(-11.1026833822258,3.59999999999997,
11.5708596481404));
#125267=CARTESIAN_POINT('Ctrl Pts',(-11.1215156636168,3.6,11.5403900792165));
#125268=CARTESIAN_POINT('Ctrl Pts',(-11.1273432021012,3.60000000000001,
11.5309614506919));
#125269=CARTESIAN_POINT('Ctrl Pts',(-11.1330535344873,3.6,11.5214527959592));
#125270=CARTESIAN_POINT('Ctrl Pts',(-11.1386454384173,3.59999999999999,
11.511866904403));
#125271=CARTESIAN_POINT('Ctrl Pts',(-11.1442677649375,3.59999999999998,
11.5022288610837));
#125272=CARTESIAN_POINT('Ctrl Pts',(-11.1497665524814,3.60000000000002,
11.4925191719262));
#125273=CARTESIAN_POINT('Ctrl Pts',(-11.1551378824765,3.60000000000002,
11.4827468583259));
#125274=CARTESIAN_POINT('Ctrl Pts',(-11.1807420222877,3.60000000000001,
11.4361640410485));
#125275=CARTESIAN_POINT('Ctrl Pts',(-11.2034758957147,3.59999999999998,
11.3881218423073));
#125276=CARTESIAN_POINT('Ctrl Pts',(-11.2232531113551,3.59999999999999,
11.3389605141168));
#125277=CARTESIAN_POINT('Ctrl Pts',(-11.2429220523829,3.6,11.2900683301712));
#125278=CARTESIAN_POINT('Ctrl Pts',(-11.2596672308722,3.59999999999998,
11.2400682143317));
#125279=CARTESIAN_POINT('Ctrl Pts',(-11.2733682251147,3.6,11.18925800081));
#125280=CARTESIAN_POINT('Ctrl Pts',(-11.2813293082148,3.60000000000002,
11.159734279756));
#125281=CARTESIAN_POINT('Ctrl Pts',(-11.2882618783691,3.6,11.1299364359319));
#125282=CARTESIAN_POINT('Ctrl Pts',(-11.2941355108101,3.6,11.0999192215127));
#125283=CARTESIAN_POINT('Ctrl Pts',(-11.297245546931,3.6,11.0840253735351));
#125284=CARTESIAN_POINT('Ctrl Pts',(-11.3000586080087,3.60000000000002,
11.0680699868974));
#125285=CARTESIAN_POINT('Ctrl Pts',(-11.3025695287904,3.60000000000002,
11.0520610063241));
#125286=CARTESIAN_POINT('Ctrl Pts',(-11.3040622829494,3.60000000000001,
11.0425435924308));
#125287=CARTESIAN_POINT('Ctrl Pts',(-11.3054480305648,3.60000000000003,
11.0330079228566));
#125288=CARTESIAN_POINT('Ctrl Pts',(-11.3067241767973,3.60000000000002,
11.0234689901208));
#125289=CARTESIAN_POINT('Ctrl Pts',(-11.3139927404417,3.60000000000001,
10.9691379597692));
#125290=CARTESIAN_POINT('Ctrl Pts',(-11.3177273076128,3.60000000000001,
10.9145922890096));
#125291=CARTESIAN_POINT('Ctrl Pts',(-11.3178159451722,3.60000000000002,
10.8601622391978));
#125292=CARTESIAN_POINT('Ctrl Pts',(-11.3178338810166,3.60000000000002,
10.8491482975715));
#125293=CARTESIAN_POINT('Ctrl Pts',(-11.3177023864676,3.60000000000002,
10.8381390007859));
#125294=CARTESIAN_POINT('Ctrl Pts',(-11.3174203038176,3.60000000000002,
10.8271369643882));
#125295=CARTESIAN_POINT('Ctrl Pts',(-11.3160738601558,3.60000000000002,
10.7746217807255));
#125296=CARTESIAN_POINT('Ctrl Pts',(-11.3113006782232,3.60000000000003,
10.7222726280919));
#125297=CARTESIAN_POINT('Ctrl Pts',(-11.3033023704179,3.60000000000001,
10.6703071156347));
#125298=CARTESIAN_POINT('Ctrl Pts',(-11.2993868268145,3.6,10.6448675808169));
#125299=CARTESIAN_POINT('Ctrl Pts',(-11.2946975676707,3.60000000000001,
10.6195198671649));
#125300=CARTESIAN_POINT('Ctrl Pts',(-11.2892538466151,3.60000000000002,
10.5942892822886));
#125301=CARTESIAN_POINT('Ctrl Pts',(-11.2858213458543,3.60000000000003,
10.5783803110358));
#125302=CARTESIAN_POINT('Ctrl Pts',(-11.2820888261831,3.60000000000004,
10.5625179087665));
#125303=CARTESIAN_POINT('Ctrl Pts',(-11.2780605557296,3.60000000000003,
10.5467084764853));
#125304=CARTESIAN_POINT('Ctrl Pts',(-11.2754395971204,3.60000000000003,
10.5364222089364));
#125305=CARTESIAN_POINT('Ctrl Pts',(-11.2726929981706,3.59999999999998,
10.5261572437755));
#125306=CARTESIAN_POINT('Ctrl Pts',(-11.2698269341424,3.59999999999998,
10.5159323008787));
#125307=CARTESIAN_POINT('Ctrl Pts',(-11.2548712899696,3.59999999999998,
10.4625766862987));
#125308=CARTESIAN_POINT('Ctrl Pts',(-11.2366414727183,3.60000000000002,
10.4102056220908));
#125309=CARTESIAN_POINT('Ctrl Pts',(-11.2153854207654,3.60000000000002,
10.359061853025));
#125310=CARTESIAN_POINT('Ctrl Pts',(-11.1941293688125,3.60000000000001,
10.3079180839592));
#125311=CARTESIAN_POINT('Ctrl Pts',(-11.1698466762124,3.59999999999999,
10.2580006758086));
#125312=CARTESIAN_POINT('Ctrl Pts',(-11.1427321020229,3.59999999999999,
10.2095520946345));
#125313=CARTESIAN_POINT('Ctrl Pts',(-11.1273228069325,3.59999999999999,
10.1820186184011));
#125314=CARTESIAN_POINT('Ctrl Pts',(-11.1109979678583,3.59999999999999,
10.1549595972699));
#125315=CARTESIAN_POINT('Ctrl Pts',(-11.0937864439126,3.60000000000001,
10.1284212693692));
#125316=CARTESIAN_POINT('Ctrl Pts',(-11.082565870655,3.60000000000002,10.111120346262));
#125317=CARTESIAN_POINT('Ctrl Pts',(-11.0709683549836,3.6,10.0940407503956));
#125318=CARTESIAN_POINT('Ctrl Pts',(-11.0590008447151,3.60000000000001,
10.077195802441));
#125319=CARTESIAN_POINT('Ctrl Pts',(-11.0529621175772,3.60000000000001,
10.0686959522577));
#125320=CARTESIAN_POINT('Ctrl Pts',(-11.0468278086681,3.59999999999998,
10.0602540260021));
#125321=CARTESIAN_POINT('Ctrl Pts',(-11.0406031296959,3.59999999999998,
10.0518776796523));
#125322=CARTESIAN_POINT('Ctrl Pts',(-11.0058073901279,3.60000000000001,
10.0050541940683));
#125323=CARTESIAN_POINT('Ctrl Pts',(-10.9683118154454,3.59999999999999,
9.96043766150485));
#125324=CARTESIAN_POINT('Ctrl Pts',(-10.9283466012212,3.59999999999999,
9.91828742617033));
#125325=CARTESIAN_POINT('Ctrl Pts',(-10.8887131736399,3.6,9.87648711727444));
#125326=CARTESIAN_POINT('Ctrl Pts',(-10.8466503825228,3.59999999999998,
9.83711131627027));
#125327=CARTESIAN_POINT('Ctrl Pts',(-10.802335053032,3.59999999999999,9.80042995952269));
#125328=CARTESIAN_POINT('Ctrl Pts',(-10.7583691871941,3.6,9.76403786613083));
#125329=CARTESIAN_POINT('Ctrl Pts',(-10.7121856401227,3.6,9.73029690432086));
#125330=CARTESIAN_POINT('Ctrl Pts',(-10.6639180216976,3.59999999999999,
9.6995022572823));
#125331=CARTESIAN_POINT('Ctrl Pts',(-10.6540348801927,3.59999999999999,
9.69319683215035));
#125332=CARTESIAN_POINT('Ctrl Pts',(-10.6440642465189,3.59999999999999,
9.68701506792451));
#125333=CARTESIAN_POINT('Ctrl Pts',(-10.6340070945752,3.6,9.68095972236314));
#125334=CARTESIAN_POINT('Ctrl Pts',(-10.6850489504522,3.59949089696024,
11.9580203536378));
#125335=CARTESIAN_POINT('Ctrl Pts',(-10.6811863241073,3.5996605979735,11.960782391118));
#125336=CARTESIAN_POINT('Ctrl Pts',(-10.6773069932407,3.59983029898676,
11.963521067824));
#125337=CARTESIAN_POINT('Ctrl Pts',(-10.6734112416282,3.60000000000002,
11.9662361834193));
#125338=CARTESIAN_POINT('Origin',(-10.,3.6,11.));
#125339=CARTESIAN_POINT('',(-9.34313799844363,3.6,9.69219093101808));
#125340=CARTESIAN_POINT('',(-10.,3.6,12.4635));
#125341=CARTESIAN_POINT('Origin',(-10.,3.6,11.));
#125342=CARTESIAN_POINT('Ctrl Pts',(-9.34313799844362,3.6,9.69219093101808));
#125343=CARTESIAN_POINT('Ctrl Pts',(-9.31378869772595,3.6,9.71038023888623));
#125344=CARTESIAN_POINT('Ctrl Pts',(-9.28516938078342,3.6,9.72965705355884));
#125345=CARTESIAN_POINT('Ctrl Pts',(-9.25735011406641,3.6,9.75002500446162));
#125346=CARTESIAN_POINT('Ctrl Pts',(-9.21111763578621,3.59999999999999,
9.78387423770362));
#125347=CARTESIAN_POINT('Ctrl Pts',(-9.16709250398103,3.6,9.82073588839211));
#125348=CARTESIAN_POINT('Ctrl Pts',(-9.12542360544964,3.6,9.86030453606564));
#125349=CARTESIAN_POINT('Ctrl Pts',(-9.10759094978497,3.6,9.87723836666707));
#125350=CARTESIAN_POINT('Ctrl Pts',(-9.09019035914315,3.6,9.89466832777773));
#125351=CARTESIAN_POINT('Ctrl Pts',(-9.07323596058201,3.6,9.91257169240983));
#125352=CARTESIAN_POINT('Ctrl Pts',(-9.06478843089223,3.6,9.92149204447843));
#125353=CARTESIAN_POINT('Ctrl Pts',(-9.05645190942788,3.6,9.93052987853001));
#125354=CARTESIAN_POINT('Ctrl Pts',(-9.04823739289588,3.6,9.93967172435648));
#125355=CARTESIAN_POINT('Ctrl Pts',(-9.00977558014081,3.6,9.98247545614571));
#125356=CARTESIAN_POINT('Ctrl Pts',(-8.9739302059633,3.6,10.0276140624936));
#125357=CARTESIAN_POINT('Ctrl Pts',(-8.94084915684911,3.6,10.0747735565802));
#125358=CARTESIAN_POINT('Ctrl Pts',(-8.91864933328807,3.60000000000001,
10.1064210549512));
#125359=CARTESIAN_POINT('Ctrl Pts',(-8.89769530525791,3.60000000000001,
10.1389792938016));
#125360=CARTESIAN_POINT('Ctrl Pts',(-8.87804422253735,3.6,10.1723576312641));
#125361=CARTESIAN_POINT('Ctrl Pts',(-8.8695068037653,3.6,10.1868588599691));
#125362=CARTESIAN_POINT('Ctrl Pts',(-8.86121544633237,3.59999999999999,
10.2015149048055));
#125363=CARTESIAN_POINT('Ctrl Pts',(-8.8531754732434,3.6,10.2163183978135));
#125364=CARTESIAN_POINT('Ctrl Pts',(-8.84773355435015,3.6,10.2263382582527));
#125365=CARTESIAN_POINT('Ctrl Pts',(-8.8424060011833,3.60000000000001,10.2364274486439));
#125366=CARTESIAN_POINT('Ctrl Pts',(-8.83720228730787,3.60000000000001,
10.2465680467474));
#125367=CARTESIAN_POINT('Ctrl Pts',(-8.8115274595799,3.6,10.2966011799283));
#125368=CARTESIAN_POINT('Ctrl Pts',(-8.78881976750809,3.6,10.3479621763596));
#125369=CARTESIAN_POINT('Ctrl Pts',(-8.7692196109522,3.6,10.4003610263812));
#125370=CARTESIAN_POINT('Ctrl Pts',(-8.75005907739917,3.6,10.4515845929438));
#125371=CARTESIAN_POINT('Ctrl Pts',(-8.7338681007161,3.59999999999999,10.5038010286998));
#125372=CARTESIAN_POINT('Ctrl Pts',(-8.72082637361428,3.6,10.5567452659834));
#125373=CARTESIAN_POINT('Ctrl Pts',(-8.71301454821891,3.6,10.5884581774805));
#125374=CARTESIAN_POINT('Ctrl Pts',(-8.70633357038008,3.6,10.6204322521276));
#125375=CARTESIAN_POINT('Ctrl Pts',(-8.70083101793325,3.6,10.6526092818269));
#125376=CARTESIAN_POINT('Ctrl Pts',(-8.69692474994577,3.6,10.6754517903284));
#125377=CARTESIAN_POINT('Ctrl Pts',(-8.69361250137296,3.6,10.6983965579859));
#125378=CARTESIAN_POINT('Ctrl Pts',(-8.69091346972229,3.6,10.7214220966029));
#125379=CARTESIAN_POINT('Ctrl Pts',(-8.68976274983282,3.6,10.7312389304463));
#125380=CARTESIAN_POINT('Ctrl Pts',(-8.68872362682811,3.6,10.7410704505316));
#125381=CARTESIAN_POINT('Ctrl Pts',(-8.68779870785736,3.6,10.7509006268472));
#125382=CARTESIAN_POINT('Ctrl Pts',(-8.68285750441264,3.6,10.8034164715958));
#125383=CARTESIAN_POINT('Ctrl Pts',(-8.68115878076703,3.6,10.8559970701011));
#125384=CARTESIAN_POINT('Ctrl Pts',(-8.68285927325483,3.6,10.9083968961105));
#125385=CARTESIAN_POINT('Ctrl Pts',(-8.68325479933144,3.6,10.9205848344548));
#125386=CARTESIAN_POINT('Ctrl Pts',(-8.68383444403342,3.6,10.9327629652221));
#125387=CARTESIAN_POINT('Ctrl Pts',(-8.68460058457489,3.6,10.9449281273122));
#125388=CARTESIAN_POINT('Ctrl Pts',(-8.68796860980452,3.6,10.9984073137331));
#125389=CARTESIAN_POINT('Ctrl Pts',(-8.69493710285313,3.6,11.0516377258003));
#125390=CARTESIAN_POINT('Ctrl Pts',(-8.70534580022722,3.6,11.1043362828418));
#125391=CARTESIAN_POINT('Ctrl Pts',(-8.71016328866203,3.6,11.1287269130959));
#125392=CARTESIAN_POINT('Ctrl Pts',(-8.71571837394256,3.6,11.153003280269));
#125393=CARTESIAN_POINT('Ctrl Pts',(-8.72199822947561,3.6,11.1771351721407));
#125394=CARTESIAN_POINT('Ctrl Pts',(-8.72642452861774,3.6,11.1941443169733));
#125395=CARTESIAN_POINT('Ctrl Pts',(-8.73121093312169,3.59999999999999,
11.2110816562522));
#125396=CARTESIAN_POINT('Ctrl Pts',(-8.73635344029319,3.6,11.2279360872153));
#125397=CARTESIAN_POINT('Ctrl Pts',(-8.73934372359225,3.6,11.2377366614767));
#125398=CARTESIAN_POINT('Ctrl Pts',(-8.74245200868552,3.6,11.2475011454469));
#125399=CARTESIAN_POINT('Ctrl Pts',(-8.74567520277798,3.6,11.257222478785));
#125400=CARTESIAN_POINT('Ctrl Pts',(-8.76221595659062,3.60000000000001,
11.3071103157765));
#125401=CARTESIAN_POINT('Ctrl Pts',(-8.78179248474627,3.60000000000001,
11.3559077825822));
#125402=CARTESIAN_POINT('Ctrl Pts',(-8.80423153088837,3.60000000000001,
11.4033561009679));
#125403=CARTESIAN_POINT('Ctrl Pts',(-8.82651895693268,3.60000000000001,
11.4504838122017));
#125404=CARTESIAN_POINT('Ctrl Pts',(-8.85163115351329,3.6,11.49628142762));
#125405=CARTESIAN_POINT('Ctrl Pts',(-8.87943737957251,3.6,11.5404626975772));
#125406=CARTESIAN_POINT('Ctrl Pts',(-8.89337708954315,3.6,11.5626114813793));
#125407=CARTESIAN_POINT('Ctrl Pts',(-8.90799439605087,3.6,11.584353452149));
#125408=CARTESIAN_POINT('Ctrl Pts',(-8.92327560787848,3.60000000000001,
11.6056483791132));
#125409=CARTESIAN_POINT('Ctrl Pts',(-8.9345333635161,3.60000000000001,11.6213364728841));
#125410=CARTESIAN_POINT('Ctrl Pts',(-8.94615148182247,3.60000000000001,
11.6367818819636));
#125411=CARTESIAN_POINT('Ctrl Pts',(-8.95812498707744,3.60000000000001,
11.6519673775081));
#125412=CARTESIAN_POINT('Ctrl Pts',(-8.96391308794098,3.60000000000001,
11.659308183563));
#125413=CARTESIAN_POINT('Ctrl Pts',(-8.96978369044831,3.60000000000002,
11.666587383583));
#125414=CARTESIAN_POINT('Ctrl Pts',(-8.9757278503594,3.60000000000002,11.6737932961742));
#125415=CARTESIAN_POINT('Ctrl Pts',(-9.00764475977342,3.60000000000001,
11.7124851320027));
#125416=CARTESIAN_POINT('Ctrl Pts',(-9.04174097252213,3.59999999999999,
11.7491455050258));
#125417=CARTESIAN_POINT('Ctrl Pts',(-9.07788793671881,3.6,11.7835268528966));
#125418=CARTESIAN_POINT('Ctrl Pts',(-9.11359045273366,3.60000000000001,
11.8174854618767));
#125419=CARTESIAN_POINT('Ctrl Pts',(-9.15129431594974,3.60000000000002,
11.8492213840825));
#125420=CARTESIAN_POINT('Ctrl Pts',(-9.19089957566146,3.60000000000002,
11.8784522451599));
#125421=CARTESIAN_POINT('Ctrl Pts',(-9.23050483537317,3.60000000000001,
11.9076831062372));
#125422=CARTESIAN_POINT('Ctrl Pts',(-9.2720121273675,3.60000000000001,11.9344095961519));
#125423=CARTESIAN_POINT('Ctrl Pts',(-9.31533557546052,3.59999999999998,
11.9582951989184));
#125424=CARTESIAN_POINT('Origin',(-10.,3.6,11.));
#125425=CARTESIAN_POINT('Ctrl Pts',(-9.14642233544205,3.43194259932811,
12.1953167142801));
#125426=CARTESIAN_POINT('Ctrl Pts',(-8.75085549718757,3.45827676171174,
11.9128528384984));
#125427=CARTESIAN_POINT('Ctrl Pts',(-8.26877923968405,3.51093877731875,
10.9295236576293));
#125428=CARTESIAN_POINT('Ctrl Pts',(-9.11444842119196,3.58992864614909,
9.50893498064554));
#125429=CARTESIAN_POINT('Ctrl Pts',(-10.7639040357623,3.66891220581921,
9.44485799761825));
#125430=CARTESIAN_POINT('Ctrl Pts',(-11.7201929573756,3.74789576548928,
10.7889917392604));
#125431=CARTESIAN_POINT('Ctrl Pts',(-11.1167118195198,3.82687932515938,
12.3255613683884));
#125432=CARTESIAN_POINT('Ctrl Pts',(-9.50041245587606,3.90586288482946,
12.6594642560973));
#125433=CARTESIAN_POINT('Ctrl Pts',(-8.33722952194777,3.98484644449956,
11.488748736956));
#125434=CARTESIAN_POINT('Ctrl Pts',(-8.68192527117523,4.06383000416964,
9.87465187282243));
#125435=CARTESIAN_POINT('Ctrl Pts',(-10.2219528997697,4.14281356383973,
9.28117333877804));
#125436=CARTESIAN_POINT('Ctrl Pts',(-11.5606909851596,4.22179712350982,
10.2463977718065));
#125437=CARTESIAN_POINT('Ctrl Pts',(-11.4840968696261,4.3007806831799,11.8950593682192));
#125438=CARTESIAN_POINT('Ctrl Pts',(-10.0616246295418,4.37976424284999,
12.7320115256649));
#125439=CARTESIAN_POINT('Ctrl Pts',(-8.5832683061886,4.45874780252009,11.9982684041319));
#125440=CARTESIAN_POINT('Ctrl Pts',(-8.38969615407199,4.53773136219018,
10.3592273034201));
#125441=CARTESIAN_POINT('Ctrl Pts',(-9.65645294854522,4.61671492186027,
9.30128228688353));
#125442=CARTESIAN_POINT('Ctrl Pts',(-11.2347604701799,4.69569848153035,
9.78384454771434));
#125443=CARTESIAN_POINT('Ctrl Pts',(-11.6933066879699,4.77468204120044,
11.3692963807137));
#125444=CARTESIAN_POINT('Ctrl Pts',(-10.6162518328385,4.85366560087053,
12.6198459283292));
#125445=CARTESIAN_POINT('Ctrl Pts',(-8.9803396151964,4.93264916054061,12.4014135749777));
#125446=CARTESIAN_POINT('Ctrl Pts',(-8.26912197695644,5.01163272021071,
10.9120878594701));
#125447=CARTESIAN_POINT('Ctrl Pts',(-9.12757751269249,5.0906162798808,9.50248664260314));
#125448=CARTESIAN_POINT('Ctrl Pts',(-10.7772027007156,5.16959983955088,
9.45092826629134));
#125449=CARTESIAN_POINT('Ctrl Pts',(-11.7220097524849,5.24858339922098,
10.8041692563782));
#125450=CARTESIAN_POINT('Ctrl Pts',(-11.105185962217,5.32756695889107,12.3350023424395));
#125451=CARTESIAN_POINT('Ctrl Pts',(-9.48610740508019,5.40655051856115,
12.6551681695168));
#125452=CARTESIAN_POINT('Ctrl Pts',(-8.33306019515262,5.48553407823123,
11.4743194644961));
#125453=CARTESIAN_POINT('Ctrl Pts',(-8.69170280350843,5.56451763790132,
9.86332691030806));
#125454=CARTESIAN_POINT('Ctrl Pts',(-10.2367947036762,5.64350119757142,
9.28314370551658));
#125455=CARTESIAN_POINT('Ctrl Pts',(-11.567145710715,5.72248475724152,10.2599178499643));
#125456=CARTESIAN_POINT('Ctrl Pts',(-11.4763066978144,5.80146831691158,
11.9078467940089));
#125457=CARTESIAN_POINT('Ctrl Pts',(-10.0466564110688,5.8804518765817,12.7324810090635));
#125458=CARTESIAN_POINT('Ctrl Pts',(-8.57469504544221,5.95943543625176,
11.9859883640002));
#125459=CARTESIAN_POINT('Ctrl Pts',(-8.39529324394348,6.03841899592188,
10.3453371138528));
#125460=CARTESIAN_POINT('Ctrl Pts',(-9.67114426993458,6.11740255559194,
9.29837689947444));
#125461=CARTESIAN_POINT('Ctrl Pts',(-11.2452231367503,6.19638611526205,
9.79455957959906));
#125462=CARTESIAN_POINT('Ctrl Pts',(-11.6900523859804,6.27536967493214,
11.3839143134568));
#125463=CARTESIAN_POINT('Ctrl Pts',(-10.6022318198948,6.35435323460221,
12.6251104893337));
#125464=CARTESIAN_POINT('Ctrl Pts',(-8.96826813114866,6.43333679427231,
12.3925504006075));
#125465=CARTESIAN_POINT('Ctrl Pts',(-8.26994624343055,6.5123203539424,10.8971347152067));
#125466=CARTESIAN_POINT('Ctrl Pts',(-9.14055002481499,6.59130391361249,
9.49500398419459));
#125467=CARTESIAN_POINT('Ctrl Pts',(-10.7905591410088,6.67028747328258,
9.45770187317659));
#125468=CARTESIAN_POINT('Ctrl Pts',(-11.7236376274101,6.74927103295267,
10.8190563711763));
#125469=CARTESIAN_POINT('Ctrl Pts',(-11.0936090094188,6.82825459262274,
12.3445023621971));
#125470=CARTESIAN_POINT('Ctrl Pts',(-9.47182436053907,6.90723815229285,
12.6506658539255));
#125471=CARTESIAN_POINT('Ctrl Pts',(-8.32902385616829,6.98622171196293,
11.4598978084107));
#125472=CARTESIAN_POINT('Ctrl Pts',(-8.70157358560417,7.06520527163302,
9.8520644121577));
#125473=CARTESIAN_POINT('Ctrl Pts',(-10.2516211374348,7.14418883130311,
9.2852539340673));
#125474=CARTESIAN_POINT('Ctrl Pts',(-11.5734822182317,7.2231723909732,10.273487112059));
#125475=CARTESIAN_POINT('Ctrl Pts',(-11.4684069204993,7.3021559506433,11.9205695971871));
#125476=CARTESIAN_POINT('Ctrl Pts',(-10.0316843826099,7.38113951031337,
12.7328194849246));
#125477=CARTESIAN_POINT('Ctrl Pts',(-8.56622837849275,7.46012306998348,
11.9736355605647));
#125478=CARTESIAN_POINT('Ctrl Pts',(-8.40101006472008,7.53910662965354,
10.3314953595456));
#125479=CARTESIAN_POINT('Ctrl Pts',(-9.68586019221467,7.61809018932364,
9.29559880057533));
#125480=CARTESIAN_POINT('Ctrl Pts',(-11.2555928016841,7.69707374899373,
9.80536449751617));
#125481=CARTESIAN_POINT('Ctrl Pts',(-11.686671904566,7.77605730866382,11.398503643375));
#125482=CARTESIAN_POINT('Ctrl Pts',(-10.5881668333267,7.8550408683339,12.6302536746195));
#125483=CARTESIAN_POINT('Ctrl Pts',(-8.95627368728507,7.93402442800401,
12.3835832651425));
#125484=CARTESIAN_POINT('Ctrl Pts',(-8.27089968685849,8.01300798767408,
10.8821892427257));
#125485=CARTESIAN_POINT('Ctrl Pts',(-9.1535867108016,8.09199154734418,9.4876337046522));
#125486=CARTESIAN_POINT('Ctrl Pts',(-10.8038565517817,8.17097510701427,
9.46459063712853));
#125487=CARTESIAN_POINT('Ctrl Pts',(-11.7251368029427,8.24995866668436,
10.8339569978334));
#125488=CARTESIAN_POINT('Ctrl Pts',(-11.0819503994852,8.32894222635443,
12.3539019907251));
#125489=CARTESIAN_POINT('Ctrl Pts',(-9.45758075359829,8.40792578602454,
12.6460402876506));
#125490=CARTESIAN_POINT('Ctrl Pts',(-8.32511228469123,8.48690934569461,
11.4454418127471));
#125491=CARTESIAN_POINT('Ctrl Pts',(-8.71154131791904,8.56589290536471,
9.8408876275331));
#125492=CARTESIAN_POINT('Ctrl Pts',(-10.2664287832729,8.64487646503479,
9.28749219830115));
#125493=CARTESIAN_POINT('Ctrl Pts',(-11.5797012378345,8.7238600247049,10.28711062105));
#125494=CARTESIAN_POINT('Ctrl Pts',(-11.4603975009684,8.80284358437497,
11.9332236637597));
#125495=CARTESIAN_POINT('Ctrl Pts',(-10.0167099883599,8.88182714404506,
12.7330285755649));
#125496=CARTESIAN_POINT('Ctrl Pts',(-8.55786876762613,8.96081070371516,
11.9612100582326));
#125497=CARTESIAN_POINT('Ctrl Pts',(-8.40684627801222,9.03979426338524,
10.3177035207829));
#125498=CARTESIAN_POINT('Ctrl Pts',(-9.70059957051577,9.11877782305534,
9.29294796498165));
#125499=CARTESIAN_POINT('Ctrl Pts',(-11.2658687146942,9.19776138272542,
9.81625861583101));
#125500=CARTESIAN_POINT('Ctrl Pts',(-11.6831654836466,9.27674494239552,
11.4130632180386));
#125501=CARTESIAN_POINT('Ctrl Pts',(-10.5740579298357,9.3557285020656,12.6352751330062));
#125502=CARTESIAN_POINT('Ctrl Pts',(-8.94435717581294,9.43471206173569,
12.3745128210308));
#125503=CARTESIAN_POINT('Ctrl Pts',(-8.27198223781284,9.51369562140577,
10.8672525668748));
#125504=CARTESIAN_POINT('Ctrl Pts',(-9.16668659631767,9.59267918107587,
9.48037634965791));
#125505=CARTESIAN_POINT('Ctrl Pts',(-10.8170939406285,9.67166274074595,
9.47159404619589));
#125506=CARTESIAN_POINT('Ctrl Pts',(-11.7265071668941,9.75064630041605,
10.8488700224994));
#125507=CARTESIAN_POINT('Ctrl Pts',(-11.0702110030647,9.82962986008613,
12.363200526832));
#125508=CARTESIAN_POINT('Ctrl Pts',(-9.44337764772432,9.90861341975623,
12.64129181573));
#125509=CARTESIAN_POINT('Ctrl Pts',(-8.32132577282368,9.98759697942632,
11.4309525570752));
#125510=CARTESIAN_POINT('Ctrl Pts',(-8.72160525616959,10.0665805390964,
9.82979739088376));
#125511=CARTESIAN_POINT('Ctrl Pts',(-10.2812165355508,10.1455640987665,
9.28985833114085));
#125512=CARTESIAN_POINT('Ctrl Pts',(-11.5858023051603,10.2245476584366,
10.3007873596792));
#125513=CARTESIAN_POINT('Ctrl Pts',(-11.4522790372668,10.3035312181067,
11.945808048893));
#125514=CARTESIAN_POINT('Ctrl Pts',(-10.0017343464181,10.3825147777768,
12.7331082653652));
#125515=CARTESIAN_POINT('Ctrl Pts',(-8.54961683703311,10.4614983374469,
11.9487127847886));
#125516=CARTESIAN_POINT('Ctrl Pts',(-8.41280144804587,10.540481897117,10.3039626273635));
#125517=CARTESIAN_POINT('Ctrl Pts',(-9.71536130428307,10.6194654567871,
9.29042459062748));
#125518=CARTESIAN_POINT('Ctrl Pts',(-11.2760501085098,10.6984490164571,
9.82724112110314));
#125519=CARTESIAN_POINT('Ctrl Pts',(-11.6795333850265,10.7774325761272,
11.4275919503285));
#125520=CARTESIAN_POINT('Ctrl Pts',(-10.5599061629194,10.8564161357973,
12.6401744895403));
#125521=CARTESIAN_POINT('Ctrl Pts',(-8.93251948646677,10.9353996954674,
12.3653397455663));
#125522=CARTESIAN_POINT('Ctrl Pts',(-8.27319381554146,11.0143832551375,
10.8523258028859));
#125523=CARTESIAN_POINT('Ctrl Pts',(-9.17984870307604,11.0933668148076,
9.47323246119838));
#125524=CARTESIAN_POINT('Ctrl Pts',(-10.8302703194389,11.1723503744777,
9.47871157726292));
#125525=CARTESIAN_POINT('Ctrl Pts',(-11.7277486163822,11.2513339341478,
10.8637943320196));
#125526=CARTESIAN_POINT('Ctrl Pts',(-11.0583916977844,11.3303174938179,
12.3723972755227));
#125527=CARTESIAN_POINT('Ctrl Pts',(-9.42921610136029,11.4093010534879,
12.6364207940589));
#125528=CARTESIAN_POINT('Ctrl Pts',(-8.31766460726359,11.488284613158,11.4164311207011));
#125529=CARTESIAN_POINT('Ctrl Pts',(-8.73176464128558,11.5672681728281,
9.81879453522508));
#125530=CARTESIAN_POINT('Ctrl Pts',(-10.2959833047406,11.6462517324982,
9.29235214643519));
#125531=CARTESIAN_POINT('Ctrl Pts',(-11.5917849365506,11.7252352921683,
10.314516324941));
#125532=CARTESIAN_POINT('Ctrl Pts',(-11.444052189557,11.8042188518384,11.9583217779886));
#125533=CARTESIAN_POINT('Ctrl Pts',(-9.98675847132022,11.8832024115085,
12.7330586155007));
#125534=CARTESIAN_POINT('Ctrl Pts',(-8.5414734019267,11.9621859711786,11.936144544465));
#125535=CARTESIAN_POINT('Ctrl Pts',(-8.41887474788645,12.0411695308487,
10.2902739528369));
#125536=CARTESIAN_POINT('Ctrl Pts',(-9.7301450254167,12.1201530905188,9.28802839053024));
#125537=CARTESIAN_POINT('Ctrl Pts',(-11.2861348131133,12.1991366501888,
9.83831210624346));
#125538=CARTESIAN_POINT('Ctrl Pts',(-11.6757785872691,12.2781202098589,
11.4420870022078));
#125539=CARTESIAN_POINT('Ctrl Pts',(-10.5457073900601,12.357103769529,12.6449547452531));
#125540=CARTESIAN_POINT('Ctrl Pts',(-8.92077148761818,12.4360873291991,
12.3560582580058));
#125541=CARTESIAN_POINT('Ctrl Pts',(-8.27451515546233,12.5150708888692,
10.8374224819375));
#125542=CARTESIAN_POINT('Ctrl Pts',(-9.19310887025665,12.5940544485393,
9.46617872771973));
#125543=CARTESIAN_POINT('Ctrl Pts',(-10.8433139901639,12.6730380082094,
9.48598849228214));
#125544=CARTESIAN_POINT('Ctrl Pts',(-11.7289968730589,12.7520215678794,
10.8786408546047));
#125545=CARTESIAN_POINT('Ctrl Pts',(-11.0462324066889,12.8310051275496,
12.381660612415));
#125546=CARTESIAN_POINT('Ctrl Pts',(-9.41559963367022,12.9099886872196,
12.6311015404504));
#125547=CARTESIAN_POINT('Ctrl Pts',(-8.31315199305088,12.9889722468897,
11.4025174432538));
#125548=CARTESIAN_POINT('Ctrl Pts',(-8.74406409137945,13.0679662885069,
9.80632444093873));
#125549=CARTESIAN_POINT('Ctrl Pts',(-9.78568267619791,13.1206324769007,
9.46773891403626));
#125550=CARTESIAN_POINT('Ctrl Pts',(-10.263911338604,13.1469708120712,9.55510288757666));
#125551=CARTESIAN_POINT('Ctrl Pts',(-9.20320175027983,3.48835183995636,
12.1158050466245));
#125552=CARTESIAN_POINT('Ctrl Pts',(-8.83394775330262,3.51468600234,11.8521304787705));
#125553=CARTESIAN_POINT('Ctrl Pts',(-8.38393888573301,3.567348017947,10.934211696745));
#125554=CARTESIAN_POINT('Ctrl Pts',(-9.17335471940146,3.64633788677736,
9.60811962757268));
#125555=CARTESIAN_POINT('Ctrl Pts',(-10.7130896506819,3.72532144644745,
9.54830500256142));
#125556=CARTESIAN_POINT('Ctrl Pts',(-11.6057668733959,3.80430500611754,
10.8030278675101));
#125557=CARTESIAN_POINT('Ctrl Pts',(-11.0424288968432,3.88328856578762,
12.2373859135307));
#125558=CARTESIAN_POINT('Ctrl Pts',(-9.5336446848734,3.96227212545772,12.5490778046731));
#125559=CARTESIAN_POINT('Ctrl Pts',(-8.44783590104305,4.0412556851278,11.4562374981555));
#125560=CARTESIAN_POINT('Ctrl Pts',(-8.76960271978085,4.1202392447979,9.949509276903));
#125561=CARTESIAN_POINT('Ctrl Pts',(-10.2071887414586,4.19922280446798,
9.39550853765221));
#125562=CARTESIAN_POINT('Ctrl Pts',(-11.4568748655967,4.27820636413808,
10.2965268875437));
#125563=CARTESIAN_POINT('Ctrl Pts',(-11.3853757393542,4.35718992380815,
11.8355206182229));
#125564=CARTESIAN_POINT('Ctrl Pts',(-10.0575254004378,4.43617348347826,
12.6167992784344));
#125565=CARTESIAN_POINT('Ctrl Pts',(-8.67750835006137,4.51515704314833,
11.9318642581576));
#125566=CARTESIAN_POINT('Ctrl Pts',(-8.49681248792099,4.59414060281844,
10.4018510742455));
#125567=CARTESIAN_POINT('Ctrl Pts',(-9.67930546842809,4.67312416248851,
9.41427985199122));
#125568=CARTESIAN_POINT('Ctrl Pts',(-11.1526250302863,4.75210772215862,
9.86474239427214));
#125569=CARTESIAN_POINT('Ctrl Pts',(-11.5806690606327,4.83109128182869,
11.3447310326858));
#125570=CARTESIAN_POINT('Ctrl Pts',(-10.5752591734542,4.91007484149879,
12.5120948615465));
#125571=CARTESIAN_POINT('Ctrl Pts',(-9.04816674140454,4.98905840116887,
12.3081924821154));
#125572=CARTESIAN_POINT('Ctrl Pts',(-8.38425882435147,5.06804196083896,
10.9179357162072));
#125573=CARTESIAN_POINT('Ctrl Pts',(-9.18561047252433,5.14702552050905,
9.60210022866015));
#125574=CARTESIAN_POINT('Ctrl Pts',(-10.7255036973451,5.22600908017914,
9.55397148102599));
#125575=CARTESIAN_POINT('Ctrl Pts',(-11.6074628165108,5.30499263984923,
10.8171957863493));
#125576=CARTESIAN_POINT('Ctrl Pts',(-11.0316697318524,5.38397619951932,
12.2461988803081));
#125577=CARTESIAN_POINT('Ctrl Pts',(-9.52029119648024,5.46295975918941,
12.545067490896));
#125578=CARTESIAN_POINT('Ctrl Pts',(-8.44394391507526,5.54194331885949,
11.4427680512404));
#125579=CARTESIAN_POINT('Ctrl Pts',(-8.77872985720856,5.62092687852959,
9.93893764331382));
#125580=CARTESIAN_POINT('Ctrl Pts',(-10.2210432785046,5.69991043819968,
9.39734783691432));
#125581=CARTESIAN_POINT('Ctrl Pts',(-11.4629002271292,5.77889399786976,
10.3091476191532));
#125582=CARTESIAN_POINT('Ctrl Pts',(-11.3781037645566,5.85787755753985,
11.8474574330094));
#125583=CARTESIAN_POINT('Ctrl Pts',(-10.0435528578375,5.93686111720994,
12.6172375321114));
#125584=CARTESIAN_POINT('Ctrl Pts',(-8.66950537688066,6.01584467688004,
11.9204010780749));
#125585=CARTESIAN_POINT('Ctrl Pts',(-8.50203726312108,6.09482823655011,
10.3888848507898));
#125586=CARTESIAN_POINT('Ctrl Pts',(-9.69301953295339,6.17381179622021,
9.41156772900764));
#125587=CARTESIAN_POINT('Ctrl Pts',(-11.1623917272807,6.25279535589029,
9.87474466940886));
#125588=CARTESIAN_POINT('Ctrl Pts',(-11.577631232633,6.33177891556039,11.3583765903286));
#125589=CARTESIAN_POINT('Ctrl Pts',(-10.5621717623862,6.41076247523047,
12.5170092274773));
#125590=CARTESIAN_POINT('Ctrl Pts',(-9.03689824439466,6.48974603490056,
12.2999188801709));
#125591=CARTESIAN_POINT('Ctrl Pts',(-8.38502826117153,6.56872959457065,
10.9039772450903));
#125592=CARTESIAN_POINT('Ctrl Pts',(-9.1977200618246,6.64771315424074,9.59511531167981));
#125593=CARTESIAN_POINT('Ctrl Pts',(-10.7379716761712,6.72669671391083,
9.56029451211568));
#125594=CARTESIAN_POINT('Ctrl Pts',(-11.6089824062857,6.80568027358092,
10.8310926202371));
#125595=CARTESIAN_POINT('Ctrl Pts',(-11.0208628702045,6.88466383325101,
12.2550669651111));
#125596=CARTESIAN_POINT('Ctrl Pts',(-9.50695825050053,6.96364739292109,
12.5408646663239));
#125597=CARTESIAN_POINT('Ctrl Pts',(-8.44017607065814,7.04263095259119,
11.4293057140636));
#125598=CARTESIAN_POINT('Ctrl Pts',(-8.78794404148706,7.12161451226127,
9.92842431900101));
#125599=CARTESIAN_POINT('Ctrl Pts',(-10.2348834678149,7.20059807193137,
9.39931769447449));
#125600=CARTESIAN_POINT('Ctrl Pts',(-11.4688152344077,7.27958163160145,
10.321814263017));
#125601=CARTESIAN_POINT('Ctrl Pts',(-11.3707294751401,7.35856519127155,
11.8593339238371));
#125602=CARTESIAN_POINT('Ctrl Pts',(-10.029576758689,7.43754875094163,12.6175534927849));
#125603=CARTESIAN_POINT('Ctrl Pts',(-8.66160190694888,7.51653231061172,
11.9088699748546));
#125604=CARTESIAN_POINT('Ctrl Pts',(-8.50737380480662,7.59551587028181,
10.375963840713));
#125605=CARTESIAN_POINT('Ctrl Pts',(-9.70675656193467,7.67449942995189,
9.40897442738754));
#125606=CARTESIAN_POINT('Ctrl Pts',(-11.1720716090448,7.75348298962199,
9.88483085141924));
#125607=CARTESIAN_POINT('Ctrl Pts',(-11.5744756185794,7.83246654929207,
11.3719954477872));
#125608=CARTESIAN_POINT('Ctrl Pts',(-10.549042369309,7.91145010896217,12.5218102915208));
#125609=CARTESIAN_POINT('Ctrl Pts',(-9.02570166290748,7.99043366863225,
12.2915482325542));
#125610=CARTESIAN_POINT('Ctrl Pts',(-8.38591828218086,8.06941722830234,
10.8900259354338));
#125611=CARTESIAN_POINT('Ctrl Pts',(-9.20988955618653,8.14840078797243,
9.58823529819872));
#125612=CARTESIAN_POINT('Ctrl Pts',(-10.7503845520812,8.22738434764252,
9.56672504010109));
#125613=CARTESIAN_POINT('Ctrl Pts',(-11.6103818576654,8.30636790731261,
10.8450020671837));
#125614=CARTESIAN_POINT('Ctrl Pts',(-11.0099797831991,8.38535146698271,
12.2638413366418));
#125615=CARTESIAN_POINT('Ctrl Pts',(-9.49366211875843,8.46433502665278,
12.5365467896212));
#125616=CARTESIAN_POINT('Ctrl Pts',(-8.43652469429721,8.54331858632288,
11.4158113215543));
#125617=CARTESIAN_POINT('Ctrl Pts',(-8.79724872692107,8.62230214599295,
9.91799100660755));
#125618=CARTESIAN_POINT('Ctrl Pts',(-10.2487061189644,8.70128570566306,
9.40140707086987));
#125619=CARTESIAN_POINT('Ctrl Pts',(-11.4746205689897,8.78026926533314,
10.3345315453099));
#125620=CARTESIAN_POINT('Ctrl Pts',(-11.3632528368346,8.85925282500323,
11.8711462503722));
#125621=CARTESIAN_POINT('Ctrl Pts',(-10.0155984511203,8.93823638467332,
12.6177486748559));
#125622=CARTESIAN_POINT('Ctrl Pts',(-8.65379837180093,9.01721994434341,
11.8972710086197));
#125623=CARTESIAN_POINT('Ctrl Pts',(-8.51282179709749,9.0962035040135,10.3630894258321));
#125624=CARTESIAN_POINT('Ctrl Pts',(-9.72051548665811,9.17518706368359,
9.40649992360301));
#125625=CARTESIAN_POINT('Ctrl Pts',(-11.1816639752003,9.25417062335368,
9.89500030027658));
#125626=CARTESIAN_POINT('Ctrl Pts',(-11.5712024424322,9.33315418302377,
11.3855865292906));
#125627=CARTESIAN_POINT('Ctrl Pts',(-10.5358719806333,9.41213774269386,
12.5264977258571));
#125628=CARTESIAN_POINT('Ctrl Pts',(-9.01457782980123,9.49112130236393,
12.2830811483128));
#125629=CARTESIAN_POINT('Ctrl Pts',(-8.38692882257045,9.57010486203404,
10.8760828372614));
#125630=CARTESIAN_POINT('Ctrl Pts',(-9.22211804608748,9.64908842170412,
9.58146069760038));
#125631=CARTESIAN_POINT('Ctrl Pts',(-10.7627413986833,9.72807198137422,
9.57326258708555));
#125632=CARTESIAN_POINT('Ctrl Pts',(-11.611661065924,9.80705554104429,10.8589230874321));
#125633=CARTESIAN_POINT('Ctrl Pts',(-10.9990212835699,9.8860391007144,12.2725213403514));
#125634=CARTESIAN_POINT('Ctrl Pts',(-9.4804037939792,9.96502266038446,12.5321141828741));
#125635=CARTESIAN_POINT('Ctrl Pts',(-8.43299005866429,10.0440062200546,
11.4022858814703));
#125636=CARTESIAN_POINT('Ctrl Pts',(-8.80664321873624,10.1229897797246,
9.90763848507602));
#125637=CARTESIAN_POINT('Ctrl Pts',(-10.2625101998601,10.2019733393947,
9.40361581013704));
#125638=CARTESIAN_POINT('Ctrl Pts',(-11.4803157974012,10.2809568990648,
10.3472985164411));
#125639=CARTESIAN_POINT('Ctrl Pts',(-11.3556744079037,10.3599404587349,
11.8828935306307));
#125640=CARTESIAN_POINT('Ctrl Pts',(-10.0016189788554,10.438924018405,12.6178230637439));
#125641=CARTESIAN_POINT('Ctrl Pts',(-8.64609535410689,10.5179075780751,
11.885605045439));
#125642=CARTESIAN_POINT('Ctrl Pts',(-8.51838083320707,10.5968911377452,
10.3502625674444));
#125643=CARTESIAN_POINT('Ctrl Pts',(-9.73429527977711,10.6758746974153,
9.40414440242168));
#125644=CARTESIAN_POINT('Ctrl Pts',(-11.1911681095151,10.7548582570854,
9.90525225664998));
#125645=CARTESIAN_POINT('Ctrl Pts',(-11.5678119485809,10.8338418167554,
11.3991488200345));
#125646=CARTESIAN_POINT('Ctrl Pts',(-10.5226615797786,10.9128253764255,
12.5310711804745));
#125647=CARTESIAN_POINT('Ctrl Pts',(-9.00352757562587,10.9918089360956,
12.2745182596877));
#125648=CARTESIAN_POINT('Ctrl Pts',(-8.38805980695961,11.0707924957657,
10.8621489916208));
#125649=CARTESIAN_POINT('Ctrl Pts',(-9.23440461831537,11.1497760554358,
9.57479201581885));
#125650=CARTESIAN_POINT('Ctrl Pts',(-10.7750412935959,11.2287596151059,
9.57990666475067));
#125651=CARTESIAN_POINT('Ctrl Pts',(-11.6128199350233,11.307743174776,10.8728546418738));
#125652=CARTESIAN_POINT('Ctrl Pts',(-10.9879881905645,11.3867267344461,
12.2811063274758));
#125653=CARTESIAN_POINT('Ctrl Pts',(-9.46718426419918,11.4657102941162,
12.5275671783037));
#125654=CARTESIAN_POINT('Ctrl Pts',(-8.42957243138638,11.5446938537862,
11.3887304013226));
#125655=CARTESIAN_POINT('Ctrl Pts',(-8.81612680835525,11.6236774134563,
9.89736753201015));
#125656=CARTESIAN_POINT('Ctrl Pts',(-10.2762946934488,11.7026609731264,
9.40594373850743));
#125657=CARTESIAN_POINT('Ctrl Pts',(-11.4859004681562,11.7816445327965,
10.3601142401241));
#125658=CARTESIAN_POINT('Ctrl Pts',(-11.3479948045963,11.8606280924666,
11.8945748548441));
#125659=CARTESIAN_POINT('Ctrl Pts',(-9.98763928894373,11.9396116521367,
12.6177767165552));
#125660=CARTESIAN_POINT('Ctrl Pts',(-8.63849361485231,12.0185952118068,
11.8738728360483));
#125661=CARTESIAN_POINT('Ctrl Pts',(-8.52405014120789,12.0975787714769,
10.3374844543838));
#125662=CARTESIAN_POINT('Ctrl Pts',(-9.74809559767757,12.176562331147,9.40190759595083));
#125663=CARTESIAN_POINT('Ctrl Pts',(-11.2005819863195,12.2555458908171,
9.91558680727001));
#125664=CARTESIAN_POINT('Ctrl Pts',(-11.5643069174567,12.3345294504871,
11.4126796707663));
#125665=CARTESIAN_POINT('Ctrl Pts',(-10.509407299785,12.4135130101572,12.5355334567773));
#125666=CARTESIAN_POINT('Ctrl Pts',(-8.99256104579626,12.4924965698273,
12.2658541704664));
#125667=CARTESIAN_POINT('Ctrl Pts',(-8.38929325223351,12.5714801294974,
10.8482370296052));
#125668=CARTESIAN_POINT('Ctrl Pts',(-9.24678272805185,12.6504636891675,
9.56820749196923));
#125669=CARTESIAN_POINT('Ctrl Pts',(-10.7872173080761,12.7294472488376,
9.58669952425418));
#125670=CARTESIAN_POINT('Ctrl Pts',(-11.6139851585015,12.8084308085077,
10.8867135837151));
#125671=CARTESIAN_POINT('Ctrl Pts',(-10.9766377273729,12.8874143681777,
12.2897534733992));
#125672=CARTESIAN_POINT('Ctrl Pts',(-9.45447355482463,12.9663979278479,
12.5226017578842));
#125673=CARTESIAN_POINT('Ctrl Pts',(-8.42535999325021,13.0453814875179,
11.375742252385));
#125674=CARTESIAN_POINT('Ctrl Pts',(-8.82760810726251,13.1243755291351,
9.8857269400479));
#125675=CARTESIAN_POINT('Ctrl Pts',(-9.79993892110727,13.177041717529,9.56966389573644));
#125676=CARTESIAN_POINT('Ctrl Pts',(-10.2463561330297,13.2033800526994,
9.65121647624079));
#125677=CARTESIAN_POINT('Ctrl Pts',(-9.25998116511762,3.54476108058462,
12.0362933789687));
#125678=CARTESIAN_POINT('Ctrl Pts',(-8.91704000941767,3.57109524296825,
11.7914081190427));
#125679=CARTESIAN_POINT('Ctrl Pts',(-8.49909853178196,3.62375725857524,
10.9388997358606));
#125680=CARTESIAN_POINT('Ctrl Pts',(-9.23226101761095,3.7027471274056,9.70730427449976));
#125681=CARTESIAN_POINT('Ctrl Pts',(-10.6622752656016,3.7817306870757,9.65175200750462));
#125682=CARTESIAN_POINT('Ctrl Pts',(-11.4913407894162,3.86071424674578,
10.8170639957596));
#125683=CARTESIAN_POINT('Ctrl Pts',(-10.9681459741666,3.93969780641587,
12.1492104586732));
#125684=CARTESIAN_POINT('Ctrl Pts',(-9.56687691387072,4.01868136608596,
12.4386913532491));
#125685=CARTESIAN_POINT('Ctrl Pts',(-8.55844228013835,4.09766492575605,
11.4237262593553));
#125686=CARTESIAN_POINT('Ctrl Pts',(-8.85728016838641,4.17664848542614,
10.0243666809836));
#125687=CARTESIAN_POINT('Ctrl Pts',(-10.1924245831472,4.25563204509622,
9.50984373652637));
#125688=CARTESIAN_POINT('Ctrl Pts',(-11.3530587460338,4.33461560476632,
10.3466560032809));
#125689=CARTESIAN_POINT('Ctrl Pts',(-11.2866546090824,4.4135991644364,11.7759818682266));
#125690=CARTESIAN_POINT('Ctrl Pts',(-10.053426171334,4.49258272410649,12.5015870312037));
#125691=CARTESIAN_POINT('Ctrl Pts',(-8.77174839393416,4.57156628377659,
11.8654601121833));
#125692=CARTESIAN_POINT('Ctrl Pts',(-8.60392882177002,4.65054984344667,
10.4444748450709));
#125693=CARTESIAN_POINT('Ctrl Pts',(-9.70215798831091,4.72953340311676,
9.52727741709888));
#125694=CARTESIAN_POINT('Ctrl Pts',(-11.070489590393,4.80851696278685,9.94564024082997));
#125695=CARTESIAN_POINT('Ctrl Pts',(-11.4680314332955,4.88750052245693,
11.3201656846581));
#125696=CARTESIAN_POINT('Ctrl Pts',(-10.5342665140699,4.96648408212703,
12.4043437947639));
#125697=CARTESIAN_POINT('Ctrl Pts',(-9.11599386761268,5.04546764179711,
12.214971389253));
#125698=CARTESIAN_POINT('Ctrl Pts',(-8.49939567174651,5.12445120146722,
10.9237835729444));
#125699=CARTESIAN_POINT('Ctrl Pts',(-9.2436434323562,5.20343476113729,9.70171381471713));
#125700=CARTESIAN_POINT('Ctrl Pts',(-10.6738046939746,5.28241832080739,
9.65701469576066));
#125701=CARTESIAN_POINT('Ctrl Pts',(-11.4929158805367,5.36140188047747,
10.8302223163206));
#125702=CARTESIAN_POINT('Ctrl Pts',(-10.958153501488,5.44038544014756,12.1573954181767));
#125703=CARTESIAN_POINT('Ctrl Pts',(-9.55447498788032,5.51936899981765,
12.4349668122754));
#125704=CARTESIAN_POINT('Ctrl Pts',(-8.5548276349979,5.59835255948773,11.4112166379848));
#125705=CARTESIAN_POINT('Ctrl Pts',(-8.86575691090871,5.67733611915783,
10.0145483763196));
#125706=CARTESIAN_POINT('Ctrl Pts',(-10.2052918533331,5.75631967882791,
9.51155196831206));
#125707=CARTESIAN_POINT('Ctrl Pts',(-11.3586547435432,5.83530323849801,
10.3583773883419));
#125708=CARTESIAN_POINT('Ctrl Pts',(-11.2799008312987,5.91428679816809,
11.7870680720098));
#125709=CARTESIAN_POINT('Ctrl Pts',(-10.0404493046063,5.99327035783819,
12.5019940551594));
#125710=CARTESIAN_POINT('Ctrl Pts',(-8.76431570831911,6.07225391750827,
11.8548137921496));
#125711=CARTESIAN_POINT('Ctrl Pts',(-8.60878128229869,6.15123747717835,
10.4324325877267));
#125712=CARTESIAN_POINT('Ctrl Pts',(-9.71489479597219,6.23022103684846,
9.52475855854082));
#125713=CARTESIAN_POINT('Ctrl Pts',(-11.079560317811,6.30920459651853,9.95492975921862));
#125714=CARTESIAN_POINT('Ctrl Pts',(-11.4652100792857,6.38818815618863,
11.3328388672004));
#125715=CARTESIAN_POINT('Ctrl Pts',(-10.5221117048774,6.46717171585871,
12.408907965621));
#125716=CARTESIAN_POINT('Ctrl Pts',(-9.10552835764069,6.54615527552881,
12.2072873597345));
#125717=CARTESIAN_POINT('Ctrl Pts',(-8.50011027891247,6.6251388351989,10.9108197749738));
#125718=CARTESIAN_POINT('Ctrl Pts',(-9.25489009883425,6.70412239486898,
9.69522663916505));
#125719=CARTESIAN_POINT('Ctrl Pts',(-10.6853842113335,6.78310595453907,
9.66288715105476));
#125720=CARTESIAN_POINT('Ctrl Pts',(-11.4943271851612,6.86208951420916,
10.8431288692977));
#125721=CARTESIAN_POINT('Ctrl Pts',(-10.9481167309902,6.94107307387926,
12.1656315680248));
#125722=CARTESIAN_POINT('Ctrl Pts',(-9.54209214046203,7.02005663354933,
12.4310634787225));
#125723=CARTESIAN_POINT('Ctrl Pts',(-8.55132828514797,7.09904019321943,
11.3987136197164));
#125724=CARTESIAN_POINT('Ctrl Pts',(-8.87431449736998,7.17802375288952,
10.0047842258442));
#125725=CARTESIAN_POINT('Ctrl Pts',(-10.2181457981948,7.2570073125596,9.51338145488168));
#125726=CARTESIAN_POINT('Ctrl Pts',(-11.3641482505836,7.3359908722297,10.3701414139749));
#125727=CARTESIAN_POINT('Ctrl Pts',(-11.2730520297809,7.41497443189978,
11.798098250487));
#125728=CARTESIAN_POINT('Ctrl Pts',(-10.0274691347682,7.49395799156988,
12.5022875006452));
#125729=CARTESIAN_POINT('Ctrl Pts',(-8.75697543540498,7.57294155123996,
11.8441043891445));
#125730=CARTESIAN_POINT('Ctrl Pts',(-8.61373754489317,7.65192511091005,
10.4204323218805));
#125731=CARTESIAN_POINT('Ctrl Pts',(-9.72765293165465,7.73090867058014,
9.52235005419975));
#125732=CARTESIAN_POINT('Ctrl Pts',(-11.0885504164055,7.80989223025023,
9.96429720532229));
#125733=CARTESIAN_POINT('Ctrl Pts',(-11.4622793325926,7.88887578992031,
11.3454872521992));
#125734=CARTESIAN_POINT('Ctrl Pts',(-10.5099179052913,7.96785934959041,
12.4133669084223));
#125735=CARTESIAN_POINT('Ctrl Pts',(-9.09512963852988,8.04684290926049,
12.199513199966));
#125736=CARTESIAN_POINT('Ctrl Pts',(-8.50093687750326,8.12582646893058,
10.8978626281419));
#125737=CARTESIAN_POINT('Ctrl Pts',(-9.26619240157147,8.20481002860068,
9.68883689174524));
#125738=CARTESIAN_POINT('Ctrl Pts',(-10.6969125523805,8.28379358827076,
9.66885944307361));
#125739=CARTESIAN_POINT('Ctrl Pts',(-11.4956269123882,8.36277714794085,
10.856047136534));
#125740=CARTESIAN_POINT('Ctrl Pts',(-10.938009166913,8.44176070761094,12.1737806825583));
#125741=CARTESIAN_POINT('Ctrl Pts',(-9.52974348391854,8.52074426728103,
12.4270532915916));
#125742=CARTESIAN_POINT('Ctrl Pts',(-8.54793710390317,8.59972782695112,
11.3861808303615));
#125743=CARTESIAN_POINT('Ctrl Pts',(-8.88295613592307,8.67871138662121,
9.99509438568203));
#125744=CARTESIAN_POINT('Ctrl Pts',(-10.2309834546559,8.7576949462913,9.51532194343859));
#125745=CARTESIAN_POINT('Ctrl Pts',(-11.3695399001448,8.83667850596138,
10.3819524695695));
#125746=CARTESIAN_POINT('Ctrl Pts',(-11.2661081727008,8.91566206563147,
11.8090688369849));
#125747=CARTESIAN_POINT('Ctrl Pts',(-10.0144869138808,8.99464562530156,
12.5024687741467));
#125748=CARTESIAN_POINT('Ctrl Pts',(-8.74972797597572,9.07362918497165,
11.8333319590067));
#125749=CARTESIAN_POINT('Ctrl Pts',(-8.61879731618278,9.15261274464173,
10.4084753308814));
#125750=CARTESIAN_POINT('Ctrl Pts',(-9.74043140280046,9.23159630431184,
9.52005188222438));
#125751=CARTESIAN_POINT('Ctrl Pts',(-11.0974592357066,9.31057986398191,
9.97374198472214));
#125752=CARTESIAN_POINT('Ctrl Pts',(-11.4592394012177,9.38956342365202,
11.3581098405426));
#125753=CARTESIAN_POINT('Ctrl Pts',(-10.4976860314311,9.46854698332209,
12.4177203187083));
#125754=CARTESIAN_POINT('Ctrl Pts',(-9.08479848378951,9.5475305429922,12.191649475595));
#125755=CARTESIAN_POINT('Ctrl Pts',(-8.50187540732805,9.62651410266227,
10.8849131076482));
#125756=CARTESIAN_POINT('Ctrl Pts',(-9.27754949585731,9.70549766233236,
9.68254504554283));
#125757=CARTESIAN_POINT('Ctrl Pts',(-10.708388856738,9.78448122200245,9.67493112797522));
#125758=CARTESIAN_POINT('Ctrl Pts',(-11.4968149649541,9.86346478167254,
10.8689761523649));
#125759=CARTESIAN_POINT('Ctrl Pts',(-10.9278315640749,9.94244834134262,
12.1818421538707));
#125760=CARTESIAN_POINT('Ctrl Pts',(-9.51742994023411,10.0214319010127,
12.422936550018));
#125761=CARTESIAN_POINT('Ctrl Pts',(-8.54465434450489,10.1004154606828,
11.3736192058652));
#125762=CARTESIAN_POINT('Ctrl Pts',(-8.89168118130291,10.1793990203529,
9.98547957926833));
#125763=CARTESIAN_POINT('Ctrl Pts',(-10.2438038641694,10.2583825800229,
9.5173732891332));
#125764=CARTESIAN_POINT('Ctrl Pts',(-11.374829289642,10.337366139693,10.3938096732028));
#125765=CARTESIAN_POINT('Ctrl Pts',(-11.2590697785407,10.4163496993631,
11.8199790123686));
#125766=CARTESIAN_POINT('Ctrl Pts',(-10.0015036112926,10.4953332590332,
12.5025378621227));
#125767=CARTESIAN_POINT('Ctrl Pts',(-8.74257387118066,10.5743168187033,
11.8224973060896));
#125768=CARTESIAN_POINT('Ctrl Pts',(-8.62396021836827,10.6533003783734,
10.3965625075255));
#125769=CARTESIAN_POINT('Ctrl Pts',(-9.75322925527118,10.7322839380435,
9.51786421421587));
#125770=CARTESIAN_POINT('Ctrl Pts',(-11.1062861105205,10.8112674977136,
9.98326339219686));
#125771=CARTESIAN_POINT('Ctrl Pts',(-11.4560905121352,10.8902510573837,
11.3707056897407));
#125772=CARTESIAN_POINT('Ctrl Pts',(-10.4854169966381,10.9692346170537,
12.4219678714086));
#125773=CARTESIAN_POINT('Ctrl Pts',(-9.07453566478498,11.0482181767238,
12.183696773809));
#125774=CARTESIAN_POINT('Ctrl Pts',(-8.50292579837776,11.1272017363939,
10.8719721803556));
#125775=CARTESIAN_POINT('Ctrl Pts',(-9.28896053355473,11.206185296064,9.67635157043933));
#125776=CARTESIAN_POINT('Ctrl Pts',(-10.7198122677529,11.2851688557341,
9.68110175223841));
#125777=CARTESIAN_POINT('Ctrl Pts',(-11.4978912536645,11.3641524154042,
10.881914951728));
#125778=CARTESIAN_POINT('Ctrl Pts',(-10.9175846833448,11.4431359750743,
12.1898153794288));
#125779=CARTESIAN_POINT('Ctrl Pts',(-9.50515242703808,11.5221195347444,
12.4187135625483));
#125780=CARTESIAN_POINT('Ctrl Pts',(-8.54148025550917,11.6011030944145,
11.3610296819441));
#125781=CARTESIAN_POINT('Ctrl Pts',(-8.900488975425,11.6800866540846,9.97594052879524));
#125782=CARTESIAN_POINT('Ctrl Pts',(-10.2566060821569,11.7590702137546,
9.51953533057963));
#125783=CARTESIAN_POINT('Ctrl Pts',(-11.3800159997619,11.8380537734247,
10.4057121553073));
#125784=CARTESIAN_POINT('Ctrl Pts',(-11.2519374196356,11.9170373330948,
11.8308279316994));
#125785=CARTESIAN_POINT('Ctrl Pts',(-9.98852010656727,11.9960208927649,
12.5024948176097));
#125786=CARTESIAN_POINT('Ctrl Pts',(-8.73551382777791,12.075004452435,11.8116011276316));
#125787=CARTESIAN_POINT('Ctrl Pts',(-8.62922553452934,12.1539880121051,
10.3846949559309));
#125788=CARTESIAN_POINT('Ctrl Pts',(-9.76604616993845,12.2329715717752,
9.51578680137141));
#125789=CARTESIAN_POINT('Ctrl Pts',(-11.1150291595255,12.3119551314453,
9.99286150829657));
#125790=CARTESIAN_POINT('Ctrl Pts',(-11.4528352476442,12.3909386911153,
11.3832723393248));
#125791=CARTESIAN_POINT('Ctrl Pts',(-10.4731072095099,12.4699222507854,
12.4261121683014));
#125792=CARTESIAN_POINT('Ctrl Pts',(-9.06435060397434,12.5489058104555,
12.1756500829267));
#125793=CARTESIAN_POINT('Ctrl Pts',(-8.50407134900466,12.6278893701256,
10.8590515772727));
#125794=CARTESIAN_POINT('Ctrl Pts',(-9.30045658584705,12.7068729297957,
9.67023625621872));
#125795=CARTESIAN_POINT('Ctrl Pts',(-10.7311206259883,12.7858564894658,
9.68741055622625));
#125796=CARTESIAN_POINT('Ctrl Pts',(-11.4989734439442,12.8648400491359,
10.8947863128256));
#125797=CARTESIAN_POINT('Ctrl Pts',(-10.907043048057,12.943823608806,12.1978463343832));
#125798=CARTESIAN_POINT('Ctrl Pts',(-9.49334747597901,13.022807168476,12.4141019753182));
#125799=CARTESIAN_POINT('Ctrl Pts',(-8.53756799344957,13.1017907281462,
11.3489670615161));
#125800=CARTESIAN_POINT('Ctrl Pts',(-8.91115212314558,13.1807847697633,
9.96512943915707));
#125801=CARTESIAN_POINT('Ctrl Pts',(-9.81419516601662,13.2334509581573,
9.67158887743661));
#125802=CARTESIAN_POINT('Ctrl Pts',(-10.2288009274554,13.2597892933277,
9.74733006490493));
#125803=CARTESIAN_POINT('Ctrl Pts',(-9.31676057995541,3.60117032121287,
11.956781711313));
#125804=CARTESIAN_POINT('Ctrl Pts',(-9.00013226553272,3.6275044835965,11.7306857593148));
#125805=CARTESIAN_POINT('Ctrl Pts',(-8.61425817783089,3.6801664992035,10.9435877749763));
#125806=CARTESIAN_POINT('Ctrl Pts',(-9.29116731582048,3.75915636803385,
9.80648892142689));
#125807=CARTESIAN_POINT('Ctrl Pts',(-10.6114608805213,3.83813992770395,
9.75519901244778));
#125808=CARTESIAN_POINT('Ctrl Pts',(-11.3769147054366,3.91712348737403,
10.8311001240093));
#125809=CARTESIAN_POINT('Ctrl Pts',(-10.8938630514901,3.99610704704413,
12.0610350038155));
#125810=CARTESIAN_POINT('Ctrl Pts',(-9.60010914286806,4.07509060671421,
12.3283049018249));
#125811=CARTESIAN_POINT('Ctrl Pts',(-8.66904865923364,4.1540741663843,11.3912150205549));
#125812=CARTESIAN_POINT('Ctrl Pts',(-8.94495761699203,4.23305772605439,
10.0992240850642));
#125813=CARTESIAN_POINT('Ctrl Pts',(-10.1776604248361,4.31204128572447,
9.62417893540055));
#125814=CARTESIAN_POINT('Ctrl Pts',(-11.2492426264709,4.39102484539457,
10.3967851190181));
#125815=CARTESIAN_POINT('Ctrl Pts',(-11.1879334788104,4.47000840506465,
11.7164431182301));
#125816=CARTESIAN_POINT('Ctrl Pts',(-10.0493269422301,4.54899196473475,
12.3863747839732));
#125817=CARTESIAN_POINT('Ctrl Pts',(-8.86598843780693,4.62797552440483,
11.7990559662091));
#125818=CARTESIAN_POINT('Ctrl Pts',(-8.71104515561903,4.70695908407493,
10.4870986158965));
#125819=CARTESIAN_POINT('Ctrl Pts',(-9.72501050819376,4.78594264374501,
9.64027498220657));
#125820=CARTESIAN_POINT('Ctrl Pts',(-10.9883541504996,4.8649262034151,10.0265380873878));
#125821=CARTESIAN_POINT('Ctrl Pts',(-11.3553938059582,4.94390976308519,
11.2956003366303));
#125822=CARTESIAN_POINT('Ctrl Pts',(-10.4932738546855,5.02289332275529,
12.2965927279814));
#125823=CARTESIAN_POINT('Ctrl Pts',(-9.18382099382081,5.10187688242537,
12.1217502963907));
#125824=CARTESIAN_POINT('Ctrl Pts',(-8.61453251914156,5.18086044209545,
10.9296314296816));
#125825=CARTESIAN_POINT('Ctrl Pts',(-9.30167639218805,5.25984400176556,
9.80132740077414));
#125826=CARTESIAN_POINT('Ctrl Pts',(-10.6221056906041,5.33882756143563,
9.7600579104953));
#125827=CARTESIAN_POINT('Ctrl Pts',(-11.3783689445625,5.41781112110573,
10.8432488462917));
#125828=CARTESIAN_POINT('Ctrl Pts',(-10.8846372711235,5.49679468077581,
12.0685919560453));
#125829=CARTESIAN_POINT('Ctrl Pts',(-9.5886587792804,5.5757782404459,12.3248661336547));
#125830=CARTESIAN_POINT('Ctrl Pts',(-8.66571135492052,5.65476180011599,
11.3796652247291));
#125831=CARTESIAN_POINT('Ctrl Pts',(-8.95278396460887,5.73374535978609,
10.0901591093253));
#125832=CARTESIAN_POINT('Ctrl Pts',(-10.1895404281615,5.81272891945616,
9.6257560997098));
#125833=CARTESIAN_POINT('Ctrl Pts',(-11.2544092599574,5.89171247912627,
10.4076071575309));
#125834=CARTESIAN_POINT('Ctrl Pts',(-11.1816978980407,5.97069603879634,
11.7266787110101));
#125835=CARTESIAN_POINT('Ctrl Pts',(-10.0373457513751,6.04967959846644,
12.3867505782075));
#125836=CARTESIAN_POINT('Ctrl Pts',(-8.85912603975755,6.12866315813652,
11.7892265062243));
#125837=CARTESIAN_POINT('Ctrl Pts',(-8.71552530147632,6.20764671780661,
10.4759803246637));
#125838=CARTESIAN_POINT('Ctrl Pts',(-9.73677005899099,6.28663027747671,
9.63794938807401));
#125839=CARTESIAN_POINT('Ctrl Pts',(-10.9967289083413,6.36561383714679,
10.0351148490284));
#125840=CARTESIAN_POINT('Ctrl Pts',(-11.3527889259383,6.44459739681688,
11.3073011440721));
#125841=CARTESIAN_POINT('Ctrl Pts',(-10.4820516473687,6.52358095648697,
12.3008067037646));
#125842=CARTESIAN_POINT('Ctrl Pts',(-9.17415847088668,6.60256451615705,
12.114655839298));
#125843=CARTESIAN_POINT('Ctrl Pts',(-8.61519229665345,6.68154807582715,
10.9176623048574));
#125844=CARTESIAN_POINT('Ctrl Pts',(-9.31206013584387,6.76053163549724,
9.79533796665029));
#125845=CARTESIAN_POINT('Ctrl Pts',(-10.6327967464959,6.83951519516732,
9.76547978999385));
#125846=CARTESIAN_POINT('Ctrl Pts',(-11.3796719640369,6.91849875483742,
10.8551651183584));
#125847=CARTESIAN_POINT('Ctrl Pts',(-10.8753705917758,6.99748231450749,
12.0761961709388));
#125848=CARTESIAN_POINT('Ctrl Pts',(-9.5772260304235,7.0764658741776,12.3212622911209));
#125849=CARTESIAN_POINT('Ctrl Pts',(-8.66248049963781,7.15544943384768,
11.3681215253693));
#125850=CARTESIAN_POINT('Ctrl Pts',(-8.96068495325288,7.23443299351777,
10.0811441326875));
#125851=CARTESIAN_POINT('Ctrl Pts',(-10.2014081285749,7.31341655318785,
9.6274452152889));
#125852=CARTESIAN_POINT('Ctrl Pts',(-11.2594812667594,7.39240011285795,
10.4184685649329));
#125853=CARTESIAN_POINT('Ctrl Pts',(-11.1753745844216,7.47138367252803,
11.7368625771371));
#125854=CARTESIAN_POINT('Ctrl Pts',(-10.0253615108474,7.55036723219812,
12.3870215085055));
#125855=CARTESIAN_POINT('Ctrl Pts',(-8.85234896386109,7.62935079186821,
11.7793388034344));
#125856=CARTESIAN_POINT('Ctrl Pts',(-8.72010128497971,7.70833435153831,
10.4649008030479));
#125857=CARTESIAN_POINT('Ctrl Pts',(-9.74854930137463,7.78731791120839,
9.63572568101198));
#125858=CARTESIAN_POINT('Ctrl Pts',(-11.0050292237662,7.86630147087847,
10.0437635592253));
#125859=CARTESIAN_POINT('Ctrl Pts',(-11.3500830466059,7.94528503054858,
11.3189790566114));
#125860=CARTESIAN_POINT('Ctrl Pts',(-10.4707934412737,8.02426859021864,
12.3049235253236));
#125861=CARTESIAN_POINT('Ctrl Pts',(-9.16455761415227,8.10325214988876,
12.1074781673778));
#125862=CARTESIAN_POINT('Ctrl Pts',(-8.61595547282566,8.18223570955883,
10.90569932085));
#125863=CARTESIAN_POINT('Ctrl Pts',(-9.32249524695637,8.26121926922893,
9.78943848529178));
#125864=CARTESIAN_POINT('Ctrl Pts',(-10.6434405526799,8.34020282889902,
9.77099384604614));
#125865=CARTESIAN_POINT('Ctrl Pts',(-11.3808719671109,8.4191863885691,10.8670922058844));
#125866=CARTESIAN_POINT('Ctrl Pts',(-10.8660385506269,8.49816994823921,
12.0837200284748));
#125867=CARTESIAN_POINT('Ctrl Pts',(-9.56582484907866,8.57715350790928,
12.3175597935623));
#125868=CARTESIAN_POINT('Ctrl Pts',(-8.65934951350916,8.65613706757937,
11.3565503391687));
#125869=CARTESIAN_POINT('Ctrl Pts',(-8.96866354492507,8.73512062724947,
10.0721977647565));
#125870=CARTESIAN_POINT('Ctrl Pts',(-10.2132607903475,8.81410418691954,
9.62923681600733));
#125871=CARTESIAN_POINT('Ctrl Pts',(-11.2644592313,8.89308774658964,10.4293733938294));
#125872=CARTESIAN_POINT('Ctrl Pts',(-11.168963508567,8.97207130625972,11.7469914235974));
#125873=CARTESIAN_POINT('Ctrl Pts',(-10.0133753766411,9.05105486592982,
12.3871888734376));
#125874=CARTESIAN_POINT('Ctrl Pts',(-8.84565758015053,9.1300384255999,11.7693929093938));
#125875=CARTESIAN_POINT('Ctrl Pts',(-8.72477283526805,9.20902198526999,
10.4538612359307));
#125876=CARTESIAN_POINT('Ctrl Pts',(-9.76034731894279,9.28800554494009,
9.63360384084576));
#125877=CARTESIAN_POINT('Ctrl Pts',(-11.0132544962128,9.36698910461016,
10.0524836691677));
#125878=CARTESIAN_POINT('Ctrl Pts',(-11.3472763600032,9.44597266428026,
11.3306331517947));
#125879=CARTESIAN_POINT('Ctrl Pts',(-10.4595000822287,9.52495622395034,
12.3089429115593));
#125880=CARTESIAN_POINT('Ctrl Pts',(-9.1550191377778,9.60393978362044,12.1002178028771));
#125881=CARTESIAN_POINT('Ctrl Pts',(-8.61682199208564,9.68292334329052,
10.8937433780347));
#125882=CARTESIAN_POINT('Ctrl Pts',(-9.33298094562714,9.76190690296061,
9.78362939348532));
#125883=CARTESIAN_POINT('Ctrl Pts',(-10.6540363147928,9.84089046263071,
9.77659966886485));
#125884=CARTESIAN_POINT('Ctrl Pts',(-11.3819688639842,9.91987402230078,
10.8790292172976));
#125885=CARTESIAN_POINT('Ctrl Pts',(-10.85664184458,9.99885758197089,12.0911629673903));
#125886=CARTESIAN_POINT('Ctrl Pts',(-9.55445608648902,10.077841141641,12.313758917162));
#125887=CARTESIAN_POINT('Ctrl Pts',(-8.65631863034551,10.1568247013111,
11.3449525302601));
#125888=CARTESIAN_POINT('Ctrl Pts',(-8.97671914386957,10.2358082609812,
10.0633206734606));
#125889=CARTESIAN_POINT('Ctrl Pts',(-10.2250975284787,10.3147918206513,
9.63113076812937));
#125890=CARTESIAN_POINT('Ctrl Pts',(-11.2693427818829,10.3937753803214,
10.4403208299646));
#125891=CARTESIAN_POINT('Ctrl Pts',(-11.1624651491776,10.4727589399914,
11.7570644941064));
#125892=CARTESIAN_POINT('Ctrl Pts',(-10.00138824373,10.5517424996615,12.3872526605013));
#125893=CARTESIAN_POINT('Ctrl Pts',(-8.83905238825443,10.6307260593316,
11.7593895667401));
#125894=CARTESIAN_POINT('Ctrl Pts',(-8.72953960352947,10.7097096190017,
10.4428624476065));
#125895=CARTESIAN_POINT('Ctrl Pts',(-9.77216323076523,10.7886931786718,
9.63158402601005));
#125896=CARTESIAN_POINT('Ctrl Pts',(-11.0214041115258,10.8676767383419,
10.0612745277437));
#125897=CARTESIAN_POINT('Ctrl Pts',(-11.3443690756895,10.946660298012,11.3422625594467));
#125898=CARTESIAN_POINT('Ctrl Pts',(-10.4481724134973,11.0256438576821,
12.3128645623428));
#125899=CARTESIAN_POINT('Ctrl Pts',(-9.1455437539441,11.1046274173521,12.0928752879302));
#125900=CARTESIAN_POINT('Ctrl Pts',(-8.61779178979594,11.1836109770222,
10.8817953690904));
#125901=CARTESIAN_POINT('Ctrl Pts',(-9.34351644879403,11.2625945366923,
9.7779111250598));
#125902=CARTESIAN_POINT('Ctrl Pts',(-10.6645832419098,11.3415780963624,
9.78229683972616));
#125903=CARTESIAN_POINT('Ctrl Pts',(-11.3829625723056,11.4205616560325,
10.8909752615822));
#125904=CARTESIAN_POINT('Ctrl Pts',(-10.8471811761249,11.4995452157026,
12.0985244313819));
#125905=CARTESIAN_POINT('Ctrl Pts',(-9.54312058987698,11.5785287753727,
12.3098599467931));
#125906=CARTESIAN_POINT('Ctrl Pts',(-8.65338807963194,11.6575123350428,
11.3333289625656));
#125907=CARTESIAN_POINT('Ctrl Pts',(-8.98485114249471,11.7364958947129,
10.0545135255803));
#125908=CARTESIAN_POINT('Ctrl Pts',(-10.236917470865,11.8154794543829,9.63312692265186));
#125909=CARTESIAN_POINT('Ctrl Pts',(-11.2741315313676,11.894463014053,10.4513100704904));
#125910=CARTESIAN_POINT('Ctrl Pts',(-11.1558800346749,11.9734465737231,
11.7670810085549));
#125911=CARTESIAN_POINT('Ctrl Pts',(-9.98940092419077,12.0524301333932,
12.387212918664));
#125912=CARTESIAN_POINT('Ctrl Pts',(-8.83253404070354,12.1314136930633,
11.749329419215));
#125913=CARTESIAN_POINT('Ctrl Pts',(-8.73440092785076,12.2103972527334,
10.4319054574778));
#125914=CARTESIAN_POINT('Ctrl Pts',(-9.78399674219934,12.2893808124035,
9.62966600679198));
#125915=CARTESIAN_POINT('Ctrl Pts',(-11.0294763327316,12.3683643720736,
10.0701362093231));
#125916=CARTESIAN_POINT('Ctrl Pts',(-11.3413635778319,12.4473479317437,
11.3538650078832));
#125917=CARTESIAN_POINT('Ctrl Pts',(-10.4368071192347,12.5263314914137,
12.3166908798255));
#125918=CARTESIAN_POINT('Ctrl Pts',(-9.13614016215244,12.6053150510838,
12.0854459953874));
#125919=CARTESIAN_POINT('Ctrl Pts',(-8.61884944577582,12.6842986107539,
10.8698661249404));
#125920=CARTESIAN_POINT('Ctrl Pts',(-9.35413044364226,12.763282170424,9.77226502046828));
#125921=CARTESIAN_POINT('Ctrl Pts',(-10.6750239439003,12.8422657300941,
9.78812158819826));
#125922=CARTESIAN_POINT('Ctrl Pts',(-11.3839617293869,12.9212492897642,
10.9028590419362));
#125923=CARTESIAN_POINT('Ctrl Pts',(-10.8374483687411,13.0002328494343,
12.1059391953675));
#125924=CARTESIAN_POINT('Ctrl Pts',(-9.53222139713344,13.0792164091044,
12.3056021927521));
#125925=CARTESIAN_POINT('Ctrl Pts',(-8.6497759936489,13.1581999687745,11.3221918706472));
#125926=CARTESIAN_POINT('Ctrl Pts',(-8.99469613902865,13.2371940103917,
10.0445319382663));
#125927=CARTESIAN_POINT('Ctrl Pts',(-9.82845141092598,13.2898601987855,
9.77351385913679));
#125928=CARTESIAN_POINT('Ctrl Pts',(-10.211245721881,13.316198533956,9.84344365356907));
#125929=CARTESIAN_POINT('Ctrl Pts',(-9.36562697413928,3.60128171446242,
9.68112655748337));
#125930=CARTESIAN_POINT('Ctrl Pts',(-9.36187623516791,3.60107085989914,
9.68293364760113));
#125931=CARTESIAN_POINT('Ctrl Pts',(-9.35813300790377,3.60085902115538,
9.68475611302156));
#125932=CARTESIAN_POINT('Ctrl Pts',(-9.35063355176791,3.60043166338206,
9.68844553523053));
#125933=CARTESIAN_POINT('Ctrl Pts',(-9.34688639229947,3.60021664372616,
9.69030825750773));
#125934=CARTESIAN_POINT('Ctrl Pts',(-9.34313799844363,3.6,9.69219093101808));
#125935=CARTESIAN_POINT('Origin',(-10.,3.6,11.));
#125936=CARTESIAN_POINT('',(-10.,3.5,12.5635));
#125937=CARTESIAN_POINT('Origin',(-10.,3.5,11.));
#125938=CARTESIAN_POINT('Origin',(-10.,3.6,12.5635));
#125939=CARTESIAN_POINT('Origin',(-10.,3.5,11.));
#125940=CARTESIAN_POINT('',(-10.,3.5,8.45));
#125941=CARTESIAN_POINT('Origin',(-10.,3.5,11.));
#125942=CARTESIAN_POINT('Origin',(-10.,13.325,11.));
#125943=CARTESIAN_POINT('',(-11.1135,13.5,11.));
#125944=CARTESIAN_POINT('',(-11.2885,13.325,11.));
#125945=CARTESIAN_POINT('Origin',(-10.,13.5,11.));
#125946=CARTESIAN_POINT('Origin',(-10.,13.5,11.));
#125947=CARTESIAN_POINT('Origin',(-7.21791809774051,2.9,11.4905561019091));
#125948=CARTESIAN_POINT('',(-7.30151407930766,2.9,11.5297865002293));
#125949=CARTESIAN_POINT('',(-7.28305503829031,2.9,11.4251000765));
#125950=CARTESIAN_POINT('Origin',(-10.,2.9,11.));
#125951=CARTESIAN_POINT('',(-7.43949984216826,2.9,11.451485261934));
#125952=CARTESIAN_POINT('',(-7.02412006173947,2.9,11.6871961823661));
#125953=CARTESIAN_POINT('',(-7.43949984216826,2.9,11.451485261934));
#125954=CARTESIAN_POINT('Origin',(-6.96855264488606,0.5,11.3720577014022));
#125955=CARTESIAN_POINT('',(-7.28305503829031,0.8,11.4251000765));
#125956=CARTESIAN_POINT('',(-7.28305503829031,3.5,11.4251000765));
#125957=CARTESIAN_POINT('',(-7.43949984216826,0.65,11.451485261934));
#125958=CARTESIAN_POINT('',(-7.43949984216826,0.5,11.451485261934));
#125959=CARTESIAN_POINT('Ctrl Pts',(-7.28305503829031,0.800000000000006,
11.4251000765));
#125960=CARTESIAN_POINT('Ctrl Pts',(-7.36347059168579,0.722647555637982,
11.4386625549942));
#125961=CARTESIAN_POINT('Ctrl Pts',(-7.43949984216826,0.65,11.451485261934));
#125962=CARTESIAN_POINT('Origin',(-7.43949984216826,0.5,11.451485261934));
#125963=CARTESIAN_POINT('',(-7.30151407930766,0.8,11.5297865002293));
#125964=CARTESIAN_POINT('',(-7.30151407930766,3.5,11.5297865002293));
#125965=CARTESIAN_POINT('Ctrl Pts',(-7.43949984216826,0.65,11.451485261934));
#125966=CARTESIAN_POINT('Ctrl Pts',(-7.37244134059104,0.722647555638358,
11.489538200171));
#125967=CARTESIAN_POINT('Ctrl Pts',(-7.30151407930765,0.800000000000005,
11.5297865002293));
#125968=CARTESIAN_POINT('Origin',(-10.,3.5,11.));
#125969=CARTESIAN_POINT('',(-12.7494863164095,2.9,10.9468493097211));
#125970=CARTESIAN_POINT('',(-12.75,2.9,11.));
#125971=CARTESIAN_POINT('Origin',(-10.,2.9,11.));
#125972=CARTESIAN_POINT('',(-12.75,3.3,11.));
#125973=CARTESIAN_POINT('',(-12.75,3.5,11.));
#125974=CARTESIAN_POINT('',(-10.,3.3,8.25));
#125975=CARTESIAN_POINT('Origin',(-10.,3.3,11.));
#125976=CARTESIAN_POINT('Origin',(-10.,3.3,11.));
#125977=CARTESIAN_POINT('',(-12.7494863164095,2.9,11.0531506902789));
#125978=CARTESIAN_POINT('Origin',(-10.,2.9,11.));
#125979=CARTESIAN_POINT('',(-12.7494863164095,0.8,11.0531506902789));
#125980=CARTESIAN_POINT('',(-12.7494863164095,3.5,11.0531506902789));
#125981=CARTESIAN_POINT('',(-12.7169449617097,0.8,11.4251000765));
#125982=CARTESIAN_POINT('Origin',(-10.,0.8,11.));
#125983=CARTESIAN_POINT('',(-12.7169449617097,2.9,11.4251000765));
#125984=CARTESIAN_POINT('',(-12.7169449617097,3.5,11.4251000765));
#125985=CARTESIAN_POINT('',(-12.6984859206923,2.9,11.5297865002293));
#125986=CARTESIAN_POINT('Origin',(-10.,2.9,11.));
#125987=CARTESIAN_POINT('',(-12.6984859206923,0.8,11.5297865002293));
#125988=CARTESIAN_POINT('',(-12.6984859206923,3.5,11.5297865002293));
#125989=CARTESIAN_POINT('',(-12.6018506091889,0.8,11.8904343925655));
#125990=CARTESIAN_POINT('Origin',(-10.,0.8,11.));
#125991=CARTESIAN_POINT('',(-12.6018506091889,2.9,11.8904343925656));
#125992=CARTESIAN_POINT('',(-12.6018506091889,3.5,11.8904343925655));
#125993=CARTESIAN_POINT('',(-12.5654933957747,2.9,11.9903250154551));
#125994=CARTESIAN_POINT('Origin',(-10.,2.9,11.));
#125995=CARTESIAN_POINT('',(-12.5654933957747,0.8,11.9903250154551));
#125996=CARTESIAN_POINT('',(-12.5654933957747,3.5,11.9903250154551));
#125997=CARTESIAN_POINT('',(-12.4077003425078,0.8,12.3287133101945));
#125998=CARTESIAN_POINT('Origin',(-10.,0.8,11.));
#125999=CARTESIAN_POINT('',(-12.4077003425078,2.9,12.3287133101945));
#126000=CARTESIAN_POINT('',(-12.4077003425078,3.5,12.3287133101945));
#126001=CARTESIAN_POINT('',(-12.3545496522288,2.9,12.420773006215));
#126002=CARTESIAN_POINT('Origin',(-10.,2.9,11.));
#126003=CARTESIAN_POINT('',(-12.3545496522288,0.8,12.420773006215));
#126004=CARTESIAN_POINT('',(-12.3545496522288,3.5,12.420773006215));
#126005=CARTESIAN_POINT('',(-12.1403933192747,0.8,12.7266199462546));
#126006=CARTESIAN_POINT('Origin',(-10.,0.8,11.));
#126007=CARTESIAN_POINT('',(-12.1403933192747,2.9,12.7266199462546));
#126008=CARTESIAN_POINT('',(-12.1403933192747,3.5,12.7266199462546));
#126009=CARTESIAN_POINT('',(-12.0720641089596,2.9,12.8080515281268));
#126010=CARTESIAN_POINT('Origin',(-10.,2.9,11.));
#126011=CARTESIAN_POINT('',(-12.0720641089596,0.8,12.8080515281268));
#126012=CARTESIAN_POINT('',(-12.0720641089596,3.5,12.8080515281268));
#126013=CARTESIAN_POINT('',(-11.8080515281268,0.8,13.0720641089596));
#126014=CARTESIAN_POINT('Origin',(-10.,0.8,11.));
#126015=CARTESIAN_POINT('',(-11.8080515281268,2.9,13.0720641089596));
#126016=CARTESIAN_POINT('',(-11.8080515281268,3.5,13.0720641089596));
#126017=CARTESIAN_POINT('',(-11.7266199462546,2.9,13.1403933192747));
#126018=CARTESIAN_POINT('Origin',(-10.,2.9,11.));
#126019=CARTESIAN_POINT('',(-11.7266199462546,0.8,13.1403933192747));
#126020=CARTESIAN_POINT('',(-11.7266199462546,3.5,13.1403933192747));
#126021=CARTESIAN_POINT('',(-11.420773006215,0.8,13.3545496522288));
#126022=CARTESIAN_POINT('Origin',(-10.,0.8,11.));
#126023=CARTESIAN_POINT('',(-11.420773006215,2.9,13.3545496522288));
#126024=CARTESIAN_POINT('',(-11.420773006215,3.5,13.3545496522288));
#126025=CARTESIAN_POINT('',(-11.3287133101945,2.9,13.4077003425078));
#126026=CARTESIAN_POINT('Origin',(-10.,2.9,11.));
#126027=CARTESIAN_POINT('',(-11.3287133101945,0.8,13.4077003425078));
#126028=CARTESIAN_POINT('',(-11.3287133101945,3.5,13.4077003425078));
#126029=CARTESIAN_POINT('',(-10.9903250154551,0.8,13.5654933957747));
#126030=CARTESIAN_POINT('Origin',(-10.,0.8,11.));
#126031=CARTESIAN_POINT('',(-10.9903250154551,2.9,13.5654933957747));
#126032=CARTESIAN_POINT('',(-10.9903250154551,3.5,13.5654933957747));
#126033=CARTESIAN_POINT('',(-10.8904343925656,2.9,13.6018506091889));
#126034=CARTESIAN_POINT('Origin',(-10.,2.9,11.));
#126035=CARTESIAN_POINT('',(-10.8904343925656,0.8,13.6018506091889));
#126036=CARTESIAN_POINT('',(-10.8904343925656,3.5,13.6018506091889));
#126037=CARTESIAN_POINT('',(-10.5297865002293,0.8,13.6984859206923));
#126038=CARTESIAN_POINT('Origin',(-10.,0.8,11.));
#126039=CARTESIAN_POINT('',(-10.5297865002293,2.9,13.6984859206923));
#126040=CARTESIAN_POINT('',(-10.5297865002293,3.5,13.6984859206923));
#126041=CARTESIAN_POINT('',(-10.4251000765,2.9,13.7169449617097));
#126042=CARTESIAN_POINT('Origin',(-10.,2.9,11.));
#126043=CARTESIAN_POINT('',(-10.4251000765,0.8,13.7169449617097));
#126044=CARTESIAN_POINT('',(-10.4251000765,3.5,13.7169449617097));
#126045=CARTESIAN_POINT('',(-10.0531506902789,0.8,13.7494863164095));
#126046=CARTESIAN_POINT('Origin',(-10.,0.8,11.));
#126047=CARTESIAN_POINT('',(-10.0531506902789,2.9,13.7494863164095));
#126048=CARTESIAN_POINT('',(-10.0531506902789,3.5,13.7494863164095));
#126049=CARTESIAN_POINT('',(-9.94684930972108,2.9,13.7494863164095));
#126050=CARTESIAN_POINT('Origin',(-10.,2.9,11.));
#126051=CARTESIAN_POINT('',(-9.94684930972108,0.8,13.7494863164095));
#126052=CARTESIAN_POINT('',(-9.94684930972108,3.5,13.7494863164095));
#126053=CARTESIAN_POINT('',(-9.57489992349997,0.8,13.7169449617097));
#126054=CARTESIAN_POINT('Origin',(-10.,0.8,11.));
#126055=CARTESIAN_POINT('',(-9.57489992349997,2.9,13.7169449617097));
#126056=CARTESIAN_POINT('',(-9.57489992349997,3.5,13.7169449617097));
#126057=CARTESIAN_POINT('',(-9.4702134997707,2.9,13.6984859206923));
#126058=CARTESIAN_POINT('Origin',(-10.,2.9,11.));
#126059=CARTESIAN_POINT('',(-9.47021349977071,0.8,13.6984859206923));
#126060=CARTESIAN_POINT('',(-9.47021349977071,3.5,13.6984859206923));
#126061=CARTESIAN_POINT('',(-9.10956560743445,0.8,13.6018506091889));
#126062=CARTESIAN_POINT('Origin',(-10.,0.8,11.));
#126063=CARTESIAN_POINT('',(-9.10956560743445,2.9,13.6018506091889));
#126064=CARTESIAN_POINT('',(-9.10956560743445,3.5,13.6018506091889));
#126065=CARTESIAN_POINT('',(-9.0096749845449,2.9,13.5654933957747));
#126066=CARTESIAN_POINT('Origin',(-10.,2.9,11.));
#126067=CARTESIAN_POINT('',(-9.0096749845449,0.8,13.5654933957747));
#126068=CARTESIAN_POINT('',(-9.0096749845449,3.5,13.5654933957747));
#126069=CARTESIAN_POINT('',(-8.67128668980549,0.8,13.4077003425078));
#126070=CARTESIAN_POINT('Origin',(-10.,0.8,11.));
#126071=CARTESIAN_POINT('',(-8.67128668980549,2.9,13.4077003425078));
#126072=CARTESIAN_POINT('',(-8.67128668980549,3.5,13.4077003425078));
#126073=CARTESIAN_POINT('',(-8.57922699378505,2.9,13.3545496522288));
#126074=CARTESIAN_POINT('Origin',(-10.,2.9,11.));
#126075=CARTESIAN_POINT('',(-8.57922699378505,0.8,13.3545496522288));
#126076=CARTESIAN_POINT('',(-8.57922699378505,3.5,13.3545496522288));
#126077=CARTESIAN_POINT('',(-8.27338005374542,0.8,13.1403933192747));
#126078=CARTESIAN_POINT('Origin',(-10.,0.8,11.));
#126079=CARTESIAN_POINT('',(-8.27338005374542,2.9,13.1403933192747));
#126080=CARTESIAN_POINT('',(-8.27338005374542,3.5,13.1403933192747));
#126081=CARTESIAN_POINT('',(-8.19194847187321,2.9,13.0720641089596));
#126082=CARTESIAN_POINT('Origin',(-10.,2.9,11.));
#126083=CARTESIAN_POINT('',(-8.19194847187321,0.8,13.0720641089596));
#126084=CARTESIAN_POINT('',(-8.19194847187321,3.5,13.0720641089596));
#126085=CARTESIAN_POINT('',(-7.92793589104044,0.8,12.8080515281268));
#126086=CARTESIAN_POINT('Origin',(-10.,0.8,11.));
#126087=CARTESIAN_POINT('',(-7.92793589104044,2.9,12.8080515281268));
#126088=CARTESIAN_POINT('',(-7.92793589104044,3.5,12.8080515281268));
#126089=CARTESIAN_POINT('',(-7.85960668072529,2.9,12.7266199462546));
#126090=CARTESIAN_POINT('Origin',(-10.,2.9,11.));
#126091=CARTESIAN_POINT('',(-7.85960668072529,0.8,12.7266199462546));
#126092=CARTESIAN_POINT('',(-7.85960668072529,3.5,12.7266199462546));
#126093=CARTESIAN_POINT('',(-7.64545034777117,0.8,12.420773006215));
#126094=CARTESIAN_POINT('Origin',(-10.,0.8,11.));
#126095=CARTESIAN_POINT('',(-7.64545034777117,2.9,12.420773006215));
#126096=CARTESIAN_POINT('',(-7.64545034777117,3.5,12.420773006215));
#126097=CARTESIAN_POINT('',(-7.59229965749225,2.9,12.3287133101945));
#126098=CARTESIAN_POINT('Origin',(-10.,2.9,11.));
#126099=CARTESIAN_POINT('',(-7.59229965749225,0.8,12.3287133101945));
#126100=CARTESIAN_POINT('',(-7.59229965749225,3.5,12.3287133101945));
#126101=CARTESIAN_POINT('',(-7.43450660422525,0.8,11.9903250154551));
#126102=CARTESIAN_POINT('Origin',(-10.,0.8,11.));
#126103=CARTESIAN_POINT('',(-7.43450660422525,2.9,11.9903250154551));
#126104=CARTESIAN_POINT('',(-7.43450660422525,3.5,11.9903250154551));
#126105=CARTESIAN_POINT('',(-7.39814939081115,2.9,11.8904343925656));
#126106=CARTESIAN_POINT('Origin',(-10.,2.9,11.));
#126107=CARTESIAN_POINT('',(-7.39814939081115,0.8,11.8904343925656));
#126108=CARTESIAN_POINT('',(-7.39814939081115,3.5,11.8904343925656));
#126109=CARTESIAN_POINT('Origin',(-10.,0.8,11.));
#126110=CARTESIAN_POINT('',(-7.25051368359054,0.8,11.0531506902789));
#126111=CARTESIAN_POINT('Origin',(-10.,0.8,11.));
#126112=CARTESIAN_POINT('',(-7.25051368359054,2.9,11.0531506902789));
#126113=CARTESIAN_POINT('',(-7.25051368359054,3.5,11.0531506902789));
#126114=CARTESIAN_POINT('',(-7.25051368359054,2.9,10.9468493097211));
#126115=CARTESIAN_POINT('Origin',(-10.,2.9,11.));
#126116=CARTESIAN_POINT('',(-7.25051368359054,0.8,10.9468493097211));
#126117=CARTESIAN_POINT('',(-7.25051368359054,3.5,10.9468493097211));
#126118=CARTESIAN_POINT('',(-7.28305503829031,0.8,10.5748999235));
#126119=CARTESIAN_POINT('Origin',(-10.,0.8,11.));
#126120=CARTESIAN_POINT('',(-7.28305503829031,2.9,10.5748999235));
#126121=CARTESIAN_POINT('',(-7.28305503829031,3.5,10.5748999235));
#126122=CARTESIAN_POINT('',(-7.30151407930766,2.9,10.4702134997707));
#126123=CARTESIAN_POINT('Origin',(-10.,2.9,11.));
#126124=CARTESIAN_POINT('',(-7.30151407930766,0.8,10.4702134997707));
#126125=CARTESIAN_POINT('',(-7.30151407930766,3.5,10.4702134997707));
#126126=CARTESIAN_POINT('',(-7.39814939081114,0.8,10.1095656074345));
#126127=CARTESIAN_POINT('Origin',(-10.,0.8,11.));
#126128=CARTESIAN_POINT('',(-7.39814939081114,2.9,10.1095656074344));
#126129=CARTESIAN_POINT('',(-7.39814939081114,3.5,10.1095656074345));
#126130=CARTESIAN_POINT('',(-7.43450660422525,2.9,10.0096749845449));
#126131=CARTESIAN_POINT('Origin',(-10.,2.9,11.));
#126132=CARTESIAN_POINT('',(-7.43450660422525,0.8,10.0096749845449));
#126133=CARTESIAN_POINT('',(-7.43450660422525,3.5,10.0096749845449));
#126134=CARTESIAN_POINT('',(-7.59229965749225,0.8,9.67128668980549));
#126135=CARTESIAN_POINT('Origin',(-10.,0.8,11.));
#126136=CARTESIAN_POINT('',(-7.59229965749225,2.9,9.67128668980549));
#126137=CARTESIAN_POINT('',(-7.59229965749225,3.5,9.67128668980549));
#126138=CARTESIAN_POINT('',(-7.64545034777117,2.9,9.57922699378505));
#126139=CARTESIAN_POINT('Origin',(-10.,2.9,11.));
#126140=CARTESIAN_POINT('',(-7.64545034777117,0.8,9.57922699378504));
#126141=CARTESIAN_POINT('',(-7.64545034777117,3.5,9.57922699378504));
#126142=CARTESIAN_POINT('',(-7.85960668072529,0.8,9.27338005374542));
#126143=CARTESIAN_POINT('Origin',(-10.,0.8,11.));
#126144=CARTESIAN_POINT('',(-7.85960668072529,2.9,9.27338005374542));
#126145=CARTESIAN_POINT('',(-7.85960668072529,3.5,9.27338005374542));
#126146=CARTESIAN_POINT('',(-7.92793589104044,2.9,9.19194847187321));
#126147=CARTESIAN_POINT('Origin',(-10.,2.9,11.));
#126148=CARTESIAN_POINT('',(-7.92793589104044,0.8,9.19194847187321));
#126149=CARTESIAN_POINT('',(-7.92793589104044,3.5,9.19194847187321));
#126150=CARTESIAN_POINT('',(-8.19194847187321,0.8,8.92793589104044));
#126151=CARTESIAN_POINT('Origin',(-10.,0.8,11.));
#126152=CARTESIAN_POINT('',(-8.19194847187321,2.9,8.92793589104044));
#126153=CARTESIAN_POINT('',(-8.19194847187321,3.5,8.92793589104044));
#126154=CARTESIAN_POINT('',(-8.27338005374542,2.9,8.85960668072529));
#126155=CARTESIAN_POINT('Origin',(-10.,2.9,11.));
#126156=CARTESIAN_POINT('',(-8.27338005374542,0.8,8.85960668072529));
#126157=CARTESIAN_POINT('',(-8.27338005374542,3.5,8.85960668072529));
#126158=CARTESIAN_POINT('',(-8.57922699378504,0.8,8.64545034777117));
#126159=CARTESIAN_POINT('Origin',(-10.,0.8,11.));
#126160=CARTESIAN_POINT('',(-8.57922699378504,2.9,8.64545034777117));
#126161=CARTESIAN_POINT('',(-8.57922699378504,3.5,8.64545034777117));
#126162=CARTESIAN_POINT('',(-8.67128668980549,2.9,8.59229965749225));
#126163=CARTESIAN_POINT('Origin',(-10.,2.9,11.));
#126164=CARTESIAN_POINT('',(-8.67128668980549,0.8,8.59229965749225));
#126165=CARTESIAN_POINT('',(-8.67128668980549,3.5,8.59229965749225));
#126166=CARTESIAN_POINT('',(-9.00967498454489,0.8,8.43450660422525));
#126167=CARTESIAN_POINT('Origin',(-10.,0.8,11.));
#126168=CARTESIAN_POINT('',(-9.00967498454489,2.9,8.43450660422525));
#126169=CARTESIAN_POINT('',(-9.00967498454489,3.5,8.43450660422525));
#126170=CARTESIAN_POINT('',(-9.10956560743445,2.9,8.39814939081115));
#126171=CARTESIAN_POINT('Origin',(-10.,2.9,11.));
#126172=CARTESIAN_POINT('',(-9.10956560743445,0.8,8.39814939081115));
#126173=CARTESIAN_POINT('',(-9.10956560743445,3.5,8.39814939081115));
#126174=CARTESIAN_POINT('',(-9.47021349977071,0.8,8.30151407930766));
#126175=CARTESIAN_POINT('Origin',(-10.,0.8,11.));
#126176=CARTESIAN_POINT('',(-9.4702134997707,2.9,8.30151407930766));
#126177=CARTESIAN_POINT('',(-9.47021349977071,3.5,8.30151407930766));
#126178=CARTESIAN_POINT('',(-9.57489992349996,2.9,8.28305503829031));
#126179=CARTESIAN_POINT('Origin',(-10.,2.9,11.));
#126180=CARTESIAN_POINT('',(-9.57489992349997,0.8,8.28305503829031));
#126181=CARTESIAN_POINT('',(-9.57489992349997,3.5,8.28305503829031));
#126182=CARTESIAN_POINT('',(-9.94684930972108,0.8,8.25051368359054));
#126183=CARTESIAN_POINT('Origin',(-10.,0.8,11.));
#126184=CARTESIAN_POINT('',(-9.94684930972108,2.9,8.25051368359054));
#126185=CARTESIAN_POINT('',(-9.94684930972108,3.5,8.25051368359054));
#126186=CARTESIAN_POINT('',(-10.0531506902789,2.9,8.25051368359054));
#126187=CARTESIAN_POINT('Origin',(-10.,2.9,11.));
#126188=CARTESIAN_POINT('',(-10.0531506902789,0.8,8.25051368359054));
#126189=CARTESIAN_POINT('',(-10.0531506902789,3.5,8.25051368359054));
#126190=CARTESIAN_POINT('',(-10.4251000765,0.8,8.28305503829031));
#126191=CARTESIAN_POINT('Origin',(-10.,0.8,11.));
#126192=CARTESIAN_POINT('',(-10.4251000765,2.9,8.28305503829031));
#126193=CARTESIAN_POINT('',(-10.4251000765,3.5,8.28305503829031));
#126194=CARTESIAN_POINT('',(-10.5297865002293,2.9,8.30151407930766));
#126195=CARTESIAN_POINT('Origin',(-10.,2.9,11.));
#126196=CARTESIAN_POINT('',(-10.5297865002293,0.8,8.30151407930766));
#126197=CARTESIAN_POINT('',(-10.5297865002293,3.5,8.30151407930766));
#126198=CARTESIAN_POINT('',(-10.8904343925655,0.8,8.39814939081115));
#126199=CARTESIAN_POINT('Origin',(-10.,0.8,11.));
#126200=CARTESIAN_POINT('',(-10.8904343925656,2.9,8.39814939081115));
#126201=CARTESIAN_POINT('',(-10.8904343925655,3.5,8.39814939081115));
#126202=CARTESIAN_POINT('',(-10.9903250154551,2.9,8.43450660422526));
#126203=CARTESIAN_POINT('Origin',(-10.,2.9,11.));
#126204=CARTESIAN_POINT('',(-10.9903250154551,0.8,8.43450660422526));
#126205=CARTESIAN_POINT('',(-10.9903250154551,3.5,8.43450660422526));
#126206=CARTESIAN_POINT('',(-11.3287133101945,0.8,8.59229965749225));
#126207=CARTESIAN_POINT('Origin',(-10.,0.8,11.));
#126208=CARTESIAN_POINT('',(-11.3287133101945,2.9,8.59229965749225));
#126209=CARTESIAN_POINT('',(-11.3287133101945,3.5,8.59229965749225));
#126210=CARTESIAN_POINT('',(-11.420773006215,2.9,8.64545034777117));
#126211=CARTESIAN_POINT('Origin',(-10.,2.9,11.));
#126212=CARTESIAN_POINT('',(-11.420773006215,0.8,8.64545034777117));
#126213=CARTESIAN_POINT('',(-11.420773006215,3.5,8.64545034777117));
#126214=CARTESIAN_POINT('',(-11.7266199462546,0.8,8.85960668072529));
#126215=CARTESIAN_POINT('Origin',(-10.,0.8,11.));
#126216=CARTESIAN_POINT('',(-11.7266199462546,2.9,8.85960668072529));
#126217=CARTESIAN_POINT('',(-11.7266199462546,3.5,8.85960668072529));
#126218=CARTESIAN_POINT('',(-11.8080515281268,2.9,8.92793589104044));
#126219=CARTESIAN_POINT('Origin',(-10.,2.9,11.));
#126220=CARTESIAN_POINT('',(-11.8080515281268,0.8,8.92793589104044));
#126221=CARTESIAN_POINT('',(-11.8080515281268,3.5,8.92793589104044));
#126222=CARTESIAN_POINT('',(-12.0720641089596,0.8,9.19194847187321));
#126223=CARTESIAN_POINT('Origin',(-10.,0.8,11.));
#126224=CARTESIAN_POINT('',(-12.0720641089596,2.9,9.19194847187321));
#126225=CARTESIAN_POINT('',(-12.0720641089596,3.5,9.19194847187321));
#126226=CARTESIAN_POINT('',(-12.1403933192747,2.9,9.27338005374542));
#126227=CARTESIAN_POINT('Origin',(-10.,2.9,11.));
#126228=CARTESIAN_POINT('',(-12.1403933192747,0.8,9.27338005374542));
#126229=CARTESIAN_POINT('',(-12.1403933192747,3.5,9.27338005374542));
#126230=CARTESIAN_POINT('',(-12.3545496522288,0.8,9.57922699378505));
#126231=CARTESIAN_POINT('Origin',(-10.,0.8,11.));
#126232=CARTESIAN_POINT('',(-12.3545496522288,2.9,9.57922699378505));
#126233=CARTESIAN_POINT('',(-12.3545496522288,3.5,9.57922699378505));
#126234=CARTESIAN_POINT('',(-12.4077003425078,2.9,9.67128668980549));
#126235=CARTESIAN_POINT('Origin',(-10.,2.9,11.));
#126236=CARTESIAN_POINT('',(-12.4077003425078,0.8,9.67128668980549));
#126237=CARTESIAN_POINT('',(-12.4077003425078,3.5,9.67128668980549));
#126238=CARTESIAN_POINT('',(-12.5654933957747,0.8,10.0096749845449));
#126239=CARTESIAN_POINT('Origin',(-10.,0.8,11.));
#126240=CARTESIAN_POINT('',(-12.5654933957747,2.9,10.0096749845449));
#126241=CARTESIAN_POINT('',(-12.5654933957747,3.5,10.0096749845449));
#126242=CARTESIAN_POINT('',(-12.6018506091889,2.9,10.1095656074344));
#126243=CARTESIAN_POINT('Origin',(-10.,2.9,11.));
#126244=CARTESIAN_POINT('',(-12.6018506091889,0.8,10.1095656074345));
#126245=CARTESIAN_POINT('',(-12.6018506091889,3.5,10.1095656074345));
#126246=CARTESIAN_POINT('',(-12.6984859206923,0.8,10.4702134997707));
#126247=CARTESIAN_POINT('Origin',(-10.,0.8,11.));
#126248=CARTESIAN_POINT('',(-12.6984859206923,2.9,10.4702134997707));
#126249=CARTESIAN_POINT('',(-12.6984859206923,3.5,10.4702134997707));
#126250=CARTESIAN_POINT('',(-12.7169449617097,2.9,10.5748999235));
#126251=CARTESIAN_POINT('Origin',(-10.,2.9,11.));
#126252=CARTESIAN_POINT('',(-12.7169449617097,0.8,10.5748999235));
#126253=CARTESIAN_POINT('',(-12.7169449617097,3.5,10.5748999235));
#126254=CARTESIAN_POINT('',(-12.7494863164095,0.8,10.9468493097211));
#126255=CARTESIAN_POINT('Origin',(-10.,0.8,11.));
#126256=CARTESIAN_POINT('',(-12.7494863164095,3.5,10.9468493097211));
#126257=CARTESIAN_POINT('Origin',(-7.07921428367087,0.5,11.8928106178175));
#126258=CARTESIAN_POINT('',(-7.55679918595664,2.9,11.8892523726467));
#126259=CARTESIAN_POINT('',(-7.55679918595664,2.9,11.8892523726467));
#126260=CARTESIAN_POINT('',(-7.55679918595664,0.650000000000001,11.8892523726467));
#126261=CARTESIAN_POINT('',(-7.55679918595664,0.5,11.8892523726467));
#126262=CARTESIAN_POINT('Ctrl Pts',(-7.39814939081114,0.800000000000006,
11.8904343925656));
#126263=CARTESIAN_POINT('Ctrl Pts',(-7.47969835093276,0.722647555638146,
11.8898268122335));
#126264=CARTESIAN_POINT('Ctrl Pts',(-7.55679918595664,0.650000000000001,
11.8892523726467));
#126265=CARTESIAN_POINT('Origin',(-7.55679918595664,0.5,11.8892523726467));
#126266=CARTESIAN_POINT('Ctrl Pts',(-7.55679918595664,0.650000000000001,
11.8892523726467));
#126267=CARTESIAN_POINT('Ctrl Pts',(-7.49736727707775,0.722647555638346,
11.9383717878434));
#126268=CARTESIAN_POINT('Ctrl Pts',(-7.43450660422525,0.800000000000006,
11.9903250154551));
#126269=CARTESIAN_POINT('',(-7.18866072953509,2.9,12.193512256469));
#126270=CARTESIAN_POINT('Origin',(-7.34536834627981,2.9,11.966206904895));
#126271=CARTESIAN_POINT('Origin',(-10.,0.65,11.));
#126272=CARTESIAN_POINT('',(-12.6,0.649999999999998,11.));
#126273=CARTESIAN_POINT('Ctrl Pts',(-12.6,0.649999999999998,11.));
#126274=CARTESIAN_POINT('Ctrl Pts',(-12.6726475556382,0.722647555638152,
10.9741697579953));
#126275=CARTESIAN_POINT('Ctrl Pts',(-12.7494863164095,0.800000000000003,
10.9468493097211));
#126276=CARTESIAN_POINT('',(-12.5605001578317,0.650000000000002,10.548514738066));
#126277=CARTESIAN_POINT('Ctrl Pts',(-12.7169449617097,0.800000000000003,
10.5748999235));
#126278=CARTESIAN_POINT('Ctrl Pts',(-12.6365294083145,0.722647555638305,
10.5613374450059));
#126279=CARTESIAN_POINT('Ctrl Pts',(-12.5605001578317,0.650000000000002,
10.548514738066));
#126280=CARTESIAN_POINT('Ctrl Pts',(-12.5605001578317,0.650000000000002,
10.548514738066));
#126281=CARTESIAN_POINT('Ctrl Pts',(-12.6275586594091,0.722647555638513,
10.5104617998289));
#126282=CARTESIAN_POINT('Ctrl Pts',(-12.6984859206923,0.800000000000003,
10.4702134997707));
#126283=CARTESIAN_POINT('',(-12.4432008140434,0.649999999999998,10.1107476273533));
#126284=CARTESIAN_POINT('Ctrl Pts',(-12.6018506091889,0.800000000000003,
10.1095656074344));
#126285=CARTESIAN_POINT('Ctrl Pts',(-12.5203016490671,0.722647555638048,
10.1101731877666));
#126286=CARTESIAN_POINT('Ctrl Pts',(-12.4432008140434,0.649999999999998,
10.1107476273533));
#126287=CARTESIAN_POINT('Ctrl Pts',(-12.4432008140434,0.649999999999998,
10.1107476273533));
#126288=CARTESIAN_POINT('Ctrl Pts',(-12.5026327229224,0.722647555638522,
10.0616282121565));
#126289=CARTESIAN_POINT('Ctrl Pts',(-12.5654933957747,0.800000000000003,
10.0096749845449));
#126290=CARTESIAN_POINT('',(-12.2516660498395,0.65,9.7));
#126291=CARTESIAN_POINT('Ctrl Pts',(-12.4077003425078,0.800000000000003,
9.67128668980549));
#126292=CARTESIAN_POINT('Ctrl Pts',(-12.3274957995475,0.722647555638263,
9.68604586794285));
#126293=CARTESIAN_POINT('Ctrl Pts',(-12.2516660498395,0.65,9.7));
#126294=CARTESIAN_POINT('Ctrl Pts',(-12.2516660498395,0.65,9.7));
#126295=CARTESIAN_POINT('Ctrl Pts',(-12.3016655575427,0.722647555638126,
9.641306576419));
#126296=CARTESIAN_POINT('Ctrl Pts',(-12.3545496522288,0.800000000000003,
9.57922699378504));
#126297=CARTESIAN_POINT('',(-11.9917155521093,0.649999999999998,9.328752214815));
#126298=CARTESIAN_POINT('Ctrl Pts',(-12.1403933192747,0.800000000000003,
9.27338005374542));
#126299=CARTESIAN_POINT('Ctrl Pts',(-12.0639701679277,0.722647555637942,
9.30184237952896));
#126300=CARTESIAN_POINT('Ctrl Pts',(-11.9917155521093,0.649999999999998,
9.328752214815));
#126301=CARTESIAN_POINT('Ctrl Pts',(-11.9917155521093,0.649999999999998,
9.328752214815));
#126302=CARTESIAN_POINT('Ctrl Pts',(-12.0307634488962,0.722647555637936,
9.26226815282488));
#126303=CARTESIAN_POINT('Ctrl Pts',(-12.0720641089596,0.800000000000003,
9.19194847187321));
#126304=CARTESIAN_POINT('',(-11.671247785185,0.649999999999999,9.00828444789066));
#126305=CARTESIAN_POINT('Ctrl Pts',(-11.8080515281268,0.800000000000002,
8.92793589104044));
#126306=CARTESIAN_POINT('Ctrl Pts',(-11.7377318471751,0.722647555637865,
8.96923655110384));
#126307=CARTESIAN_POINT('Ctrl Pts',(-11.671247785185,0.649999999999999,
9.00828444789066));
#126308=CARTESIAN_POINT('Ctrl Pts',(-11.671247785185,0.649999999999999,
9.00828444789066));
#126309=CARTESIAN_POINT('Ctrl Pts',(-11.6981576204713,0.722647555638571,
8.93602983207164));
#126310=CARTESIAN_POINT('Ctrl Pts',(-11.7266199462546,0.800000000000002,
8.85960668072529));
#126311=CARTESIAN_POINT('',(-11.3,0.65,8.74833395016046));
#126312=CARTESIAN_POINT('Ctrl Pts',(-11.420773006215,0.800000000000002,
8.64545034777117));
#126313=CARTESIAN_POINT('Ctrl Pts',(-11.3586934235809,0.722647555637949,
8.69833444245745));
#126314=CARTESIAN_POINT('Ctrl Pts',(-11.3,0.65,8.74833395016046));
#126315=CARTESIAN_POINT('Ctrl Pts',(-11.3,0.65,8.74833395016046));
#126316=CARTESIAN_POINT('Ctrl Pts',(-11.3139541320571,0.722647555638201,
8.67250420045259));
#126317=CARTESIAN_POINT('Ctrl Pts',(-11.3287133101945,0.800000000000003,
8.59229965749224));
#126318=CARTESIAN_POINT('',(-10.8892523726467,0.65,8.55679918595664));
#126319=CARTESIAN_POINT('Ctrl Pts',(-10.9903250154551,0.800000000000002,
8.43450660422526));
#126320=CARTESIAN_POINT('Ctrl Pts',(-10.9383717878433,0.722647555638172,
8.49736727707789));
#126321=CARTESIAN_POINT('Ctrl Pts',(-10.8892523726467,0.65,8.55679918595664));
#126322=CARTESIAN_POINT('Ctrl Pts',(-10.8892523726467,0.65,8.55679918595664));
#126323=CARTESIAN_POINT('Ctrl Pts',(-10.8898268122335,0.722647555638392,
8.4796983509325));
#126324=CARTESIAN_POINT('Ctrl Pts',(-10.8904343925655,0.800000000000002,
8.39814939081114));
#126325=CARTESIAN_POINT('',(-10.451485261934,0.649999999999999,8.43949984216826));
#126326=CARTESIAN_POINT('Ctrl Pts',(-10.5297865002293,0.800000000000002,
8.30151407930766));
#126327=CARTESIAN_POINT('Ctrl Pts',(-10.4895382001709,0.72264755563816,
8.37244134059122));
#126328=CARTESIAN_POINT('Ctrl Pts',(-10.451485261934,0.649999999999999,
8.43949984216826));
#126329=CARTESIAN_POINT('Ctrl Pts',(-10.451485261934,0.649999999999999,
8.43949984216826));
#126330=CARTESIAN_POINT('Ctrl Pts',(-10.4386625549942,0.722647555637904,
8.36347059168587));
#126331=CARTESIAN_POINT('Ctrl Pts',(-10.4251000765,0.800000000000002,8.28305503829031));
#126332=CARTESIAN_POINT('',(-10.,0.649999999999999,8.4));
#126333=CARTESIAN_POINT('Ctrl Pts',(-10.0531506902789,0.800000000000002,
8.25051368359054));
#126334=CARTESIAN_POINT('Ctrl Pts',(-10.0258302420047,0.722647555638087,
8.32735244436191));
#126335=CARTESIAN_POINT('Ctrl Pts',(-10.,0.649999999999999,8.4));
#126336=CARTESIAN_POINT('Ctrl Pts',(-10.,0.649999999999999,8.4));
#126337=CARTESIAN_POINT('Ctrl Pts',(-9.97416975799538,0.722647555637996,
8.32735244436201));
#126338=CARTESIAN_POINT('Ctrl Pts',(-9.94684930972108,0.800000000000002,
8.25051368359054));
#126339=CARTESIAN_POINT('',(-9.54851473806598,0.65,8.43949984216826));
#126340=CARTESIAN_POINT('Ctrl Pts',(-9.57489992349997,0.800000000000002,
8.28305503829031));
#126341=CARTESIAN_POINT('Ctrl Pts',(-9.56133744500582,0.722647555637995,
8.36347059168578));
#126342=CARTESIAN_POINT('Ctrl Pts',(-9.54851473806598,0.65,8.43949984216826));
#126343=CARTESIAN_POINT('Ctrl Pts',(-9.54851473806598,0.65,8.43949984216826));
#126344=CARTESIAN_POINT('Ctrl Pts',(-9.51046179982906,0.72264755563816,
8.37244134059122));
#126345=CARTESIAN_POINT('Ctrl Pts',(-9.4702134997707,0.800000000000002,
8.30151407930766));
#126346=CARTESIAN_POINT('',(-9.11074762735326,0.65,8.55679918595664));
#126347=CARTESIAN_POINT('Ctrl Pts',(-9.10956560743445,0.800000000000002,
8.39814939081114));
#126348=CARTESIAN_POINT('Ctrl Pts',(-9.11017318776655,0.722647555638322,
8.47969835093257));
#126349=CARTESIAN_POINT('Ctrl Pts',(-9.11074762735326,0.65,8.55679918595664));
#126350=CARTESIAN_POINT('Ctrl Pts',(-9.11074762735326,0.65,8.55679918595664));
#126351=CARTESIAN_POINT('Ctrl Pts',(-9.06162821215674,0.722647555638138,
8.49736727707792));
#126352=CARTESIAN_POINT('Ctrl Pts',(-9.00967498454489,0.800000000000001,
8.43450660422525));
#126353=CARTESIAN_POINT('',(-8.7,0.649999999999997,8.74833395016046));
#126354=CARTESIAN_POINT('Ctrl Pts',(-8.67128668980549,0.800000000000001,
8.59229965749225));
#126355=CARTESIAN_POINT('Ctrl Pts',(-8.68604586794282,0.722647555638445,
8.67250420045233));
#126356=CARTESIAN_POINT('Ctrl Pts',(-8.7,0.649999999999997,8.74833395016046));
#126357=CARTESIAN_POINT('Ctrl Pts',(-8.7,0.649999999999997,8.74833395016046));
#126358=CARTESIAN_POINT('Ctrl Pts',(-8.64130657641892,0.722647555638218,
8.69833444245727));
#126359=CARTESIAN_POINT('Ctrl Pts',(-8.57922699378504,0.800000000000001,
8.64545034777117));
#126360=CARTESIAN_POINT('',(-8.328752214815,0.65,9.00828444789066));
#126361=CARTESIAN_POINT('Ctrl Pts',(-8.27338005374542,0.800000000000001,
8.85960668072529));
#126362=CARTESIAN_POINT('Ctrl Pts',(-8.3018423795288,0.722647555638374,
8.93602983207184));
#126363=CARTESIAN_POINT('Ctrl Pts',(-8.328752214815,0.65,9.00828444789066));
#126364=CARTESIAN_POINT('Ctrl Pts',(-8.328752214815,0.65,9.00828444789066));
#126365=CARTESIAN_POINT('Ctrl Pts',(-8.26226815282474,0.722647555638093,
8.96923655110372));
#126366=CARTESIAN_POINT('Ctrl Pts',(-8.19194847187321,0.800000000000001,
8.92793589104044));
#126367=CARTESIAN_POINT('',(-8.00828444789066,0.65,9.328752214815));
#126368=CARTESIAN_POINT('Ctrl Pts',(-7.92793589104044,0.800000000000001,
9.19194847187321));
#126369=CARTESIAN_POINT('Ctrl Pts',(-7.96923655110365,0.722647555638209,
9.26226815282463));
#126370=CARTESIAN_POINT('Ctrl Pts',(-8.00828444789066,0.65,9.328752214815));
#126371=CARTESIAN_POINT('Ctrl Pts',(-8.00828444789066,0.65,9.328752214815));
#126372=CARTESIAN_POINT('Ctrl Pts',(-7.93602983207193,0.722647555638282,
9.30184237952883));
#126373=CARTESIAN_POINT('Ctrl Pts',(-7.85960668072529,0.8,9.27338005374542));
#126374=CARTESIAN_POINT('',(-7.74833395016046,0.65,9.7));
#126375=CARTESIAN_POINT('Ctrl Pts',(-7.64545034777117,0.800000000000001,
9.57922699378505));
#126376=CARTESIAN_POINT('Ctrl Pts',(-7.69833444245722,0.722647555638291,
9.64130657641886));
#126377=CARTESIAN_POINT('Ctrl Pts',(-7.74833395016046,0.65,9.7));
#126378=CARTESIAN_POINT('Ctrl Pts',(-7.74833395016046,0.65,9.7));
#126379=CARTESIAN_POINT('Ctrl Pts',(-7.67250420045258,0.722647555638207,
9.68604586794286));
#126380=CARTESIAN_POINT('Ctrl Pts',(-7.59229965749225,0.800000000000001,
9.67128668980549));
#126381=CARTESIAN_POINT('',(-7.55679918595664,0.65,10.1107476273533));
#126382=CARTESIAN_POINT('Ctrl Pts',(-7.43450660422525,0.800000000000001,
10.0096749845449));
#126383=CARTESIAN_POINT('Ctrl Pts',(-7.49736727707791,0.722647555638159,
10.0616282121567));
#126384=CARTESIAN_POINT('Ctrl Pts',(-7.55679918595664,0.65,10.1107476273533));
#126385=CARTESIAN_POINT('Ctrl Pts',(-7.55679918595664,0.65,10.1107476273533));
#126386=CARTESIAN_POINT('Ctrl Pts',(-7.47969835093245,0.722647555638439,
10.1101731877665));
#126387=CARTESIAN_POINT('Ctrl Pts',(-7.39814939081114,0.800000000000001,
10.1095656074345));
#126388=CARTESIAN_POINT('',(-7.43949984216826,0.65,10.548514738066));
#126389=CARTESIAN_POINT('Ctrl Pts',(-7.30151407930766,0.800000000000001,
10.4702134997707));
#126390=CARTESIAN_POINT('Ctrl Pts',(-7.37244134059127,0.722647555638108,
10.5104617998291));
#126391=CARTESIAN_POINT('Ctrl Pts',(-7.43949984216826,0.65,10.548514738066));
#126392=CARTESIAN_POINT('Ctrl Pts',(-7.43949984216826,0.65,10.548514738066));
#126393=CARTESIAN_POINT('Ctrl Pts',(-7.36347059168572,0.72264755563805,
10.5613374450058));
#126394=CARTESIAN_POINT('Ctrl Pts',(-7.28305503829031,0.800000000000001,
10.5748999235));
#126395=CARTESIAN_POINT('',(-7.4,0.65,11.));
#126396=CARTESIAN_POINT('Ctrl Pts',(-7.25051368359054,0.800000000000001,
10.9468493097211));
#126397=CARTESIAN_POINT('Ctrl Pts',(-7.3273524443617,0.722647555638303,
10.9741697579953));
#126398=CARTESIAN_POINT('Ctrl Pts',(-7.4,0.65,11.));
#126399=CARTESIAN_POINT('Ctrl Pts',(-7.4,0.65,11.));
#126400=CARTESIAN_POINT('Ctrl Pts',(-7.3273524443617,0.722647555638303,
11.0258302420047));
#126401=CARTESIAN_POINT('Ctrl Pts',(-7.25051368359054,0.800000000000001,
11.0531506902789));
#126402=CARTESIAN_POINT('',(-7.74833395016046,0.65,12.3));
#126403=CARTESIAN_POINT('Ctrl Pts',(-7.59229965749224,0.800000000000005,
12.3287133101945));
#126404=CARTESIAN_POINT('Ctrl Pts',(-7.67250420045221,0.722647555638561,
12.3139541320572));
#126405=CARTESIAN_POINT('Ctrl Pts',(-7.74833395016046,0.65,12.3));
#126406=CARTESIAN_POINT('Ctrl Pts',(-7.74833395016046,0.65,12.3));
#126407=CARTESIAN_POINT('Ctrl Pts',(-7.69833444245715,0.722647555638393,
12.3586934235812));
#126408=CARTESIAN_POINT('Ctrl Pts',(-7.64545034777116,0.800000000000006,
12.420773006215));
#126409=CARTESIAN_POINT('',(-8.00828444789066,0.649999999999997,12.671247785185));
#126410=CARTESIAN_POINT('Ctrl Pts',(-7.85960668072528,0.800000000000005,
12.7266199462546));
#126411=CARTESIAN_POINT('Ctrl Pts',(-7.93602983207192,0.722647555638297,
12.6981576204712));
#126412=CARTESIAN_POINT('Ctrl Pts',(-8.00828444789066,0.649999999999997,
12.671247785185));
#126413=CARTESIAN_POINT('Ctrl Pts',(-8.00828444789066,0.649999999999997,
12.671247785185));
#126414=CARTESIAN_POINT('Ctrl Pts',(-7.96923655110345,0.722647555638591,
12.7377318471757));
#126415=CARTESIAN_POINT('Ctrl Pts',(-7.92793589104044,0.800000000000006,
12.8080515281268));
#126416=CARTESIAN_POINT('',(-8.328752214815,0.65,12.9917155521093));
#126417=CARTESIAN_POINT('Ctrl Pts',(-8.19194847187321,0.800000000000005,
13.0720641089596));
#126418=CARTESIAN_POINT('Ctrl Pts',(-8.26226815282437,0.722647555638491,
13.0307634488965));
#126419=CARTESIAN_POINT('Ctrl Pts',(-8.328752214815,0.65,12.9917155521093));
#126420=CARTESIAN_POINT('Ctrl Pts',(-8.328752214815,0.65,12.9917155521093));
#126421=CARTESIAN_POINT('Ctrl Pts',(-8.301842379529,0.722647555637846,13.0639701679276));
#126422=CARTESIAN_POINT('Ctrl Pts',(-8.27338005374542,0.800000000000006,
13.1403933192747));
#126423=CARTESIAN_POINT('',(-8.7,0.650000000000003,13.2516660498395));
#126424=CARTESIAN_POINT('Ctrl Pts',(-8.57922699378504,0.800000000000005,
13.3545496522288));
#126425=CARTESIAN_POINT('Ctrl Pts',(-8.64130657641873,0.72264755563846,
13.3016655575429));
#126426=CARTESIAN_POINT('Ctrl Pts',(-8.7,0.650000000000003,13.2516660498395));
#126427=CARTESIAN_POINT('Ctrl Pts',(-8.7,0.650000000000003,13.2516660498395));
#126428=CARTESIAN_POINT('Ctrl Pts',(-8.68604586794285,0.722647555638247,
13.3274957995475));
#126429=CARTESIAN_POINT('Ctrl Pts',(-8.67128668980549,0.800000000000006,
13.4077003425078));
#126430=CARTESIAN_POINT('',(-9.11074762735326,0.65,13.4432008140434));
#126431=CARTESIAN_POINT('Ctrl Pts',(-9.00967498454489,0.800000000000005,
13.5654933957748));
#126432=CARTESIAN_POINT('Ctrl Pts',(-9.06162821215681,0.722647555638048,
13.502632722922));
#126433=CARTESIAN_POINT('Ctrl Pts',(-9.11074762735326,0.65,13.4432008140434));
#126434=CARTESIAN_POINT('Ctrl Pts',(-9.11074762735326,0.65,13.4432008140434));
#126435=CARTESIAN_POINT('Ctrl Pts',(-9.11017318776655,0.722647555638307,
13.5203016490674));
#126436=CARTESIAN_POINT('Ctrl Pts',(-9.10956560743445,0.800000000000005,
13.6018506091889));
#126437=CARTESIAN_POINT('',(-9.54851473806598,0.65,13.5605001578317));
#126438=CARTESIAN_POINT('Ctrl Pts',(-9.4702134997707,0.800000000000004,
13.6984859206923));
#126439=CARTESIAN_POINT('Ctrl Pts',(-9.51046179982905,0.722647555638188,
13.6275586594088));
#126440=CARTESIAN_POINT('Ctrl Pts',(-9.54851473806598,0.65,13.5605001578317));
#126441=CARTESIAN_POINT('Ctrl Pts',(-9.54851473806598,0.65,13.5605001578317));
#126442=CARTESIAN_POINT('Ctrl Pts',(-9.5613374450058,0.722647555637915,
13.6365294083141));
#126443=CARTESIAN_POINT('Ctrl Pts',(-9.57489992349997,0.800000000000005,
13.7169449617097));
#126444=CARTESIAN_POINT('',(-10.,0.650000000000002,13.6));
#126445=CARTESIAN_POINT('Ctrl Pts',(-9.94684930972108,0.800000000000004,
13.7494863164095));
#126446=CARTESIAN_POINT('Ctrl Pts',(-9.97416975799544,0.722647555637832,
13.6726475556378));
#126447=CARTESIAN_POINT('Ctrl Pts',(-10.,0.650000000000002,13.6));
#126448=CARTESIAN_POINT('Ctrl Pts',(-10.,0.650000000000002,13.6));
#126449=CARTESIAN_POINT('Ctrl Pts',(-10.0258302420048,0.722647555638509,
13.6726475556385));
#126450=CARTESIAN_POINT('Ctrl Pts',(-10.0531506902789,0.800000000000005,
13.7494863164095));
#126451=CARTESIAN_POINT('',(-10.451485261934,0.650000000000004,13.5605001578317));
#126452=CARTESIAN_POINT('Ctrl Pts',(-10.4251000765,0.800000000000005,13.7169449617097));
#126453=CARTESIAN_POINT('Ctrl Pts',(-10.4386625549942,0.722647555638063,
13.6365294083143));
#126454=CARTESIAN_POINT('Ctrl Pts',(-10.451485261934,0.650000000000004,
13.5605001578317));
#126455=CARTESIAN_POINT('Ctrl Pts',(-10.451485261934,0.650000000000004,
13.5605001578317));
#126456=CARTESIAN_POINT('Ctrl Pts',(-10.4895382001709,0.722647555638065,
13.6275586594087));
#126457=CARTESIAN_POINT('Ctrl Pts',(-10.5297865002293,0.800000000000005,
13.6984859206923));
#126458=CARTESIAN_POINT('',(-10.8892523726467,0.65,13.4432008140434));
#126459=CARTESIAN_POINT('Ctrl Pts',(-10.8904343925656,0.800000000000004,
13.6018506091889));
#126460=CARTESIAN_POINT('Ctrl Pts',(-10.8898268122335,0.72264755563811,
13.5203016490672));
#126461=CARTESIAN_POINT('Ctrl Pts',(-10.8892523726467,0.65,13.4432008140434));
#126462=CARTESIAN_POINT('Ctrl Pts',(-10.8892523726467,0.65,13.4432008140434));
#126463=CARTESIAN_POINT('Ctrl Pts',(-10.9383717878432,0.722647555638111,
13.5026327229221));
#126464=CARTESIAN_POINT('Ctrl Pts',(-10.9903250154551,0.800000000000004,
13.5654933957747));
#126465=CARTESIAN_POINT('',(-11.3,0.649999999999998,13.2516660498395));
#126466=CARTESIAN_POINT('Ctrl Pts',(-11.3287133101945,0.800000000000004,
13.4077003425078));
#126467=CARTESIAN_POINT('Ctrl Pts',(-11.3139541320572,0.722647555638314,
13.3274957995475));
#126468=CARTESIAN_POINT('Ctrl Pts',(-11.3,0.649999999999998,13.2516660498395));
#126469=CARTESIAN_POINT('Ctrl Pts',(-11.3,0.649999999999998,13.2516660498395));
#126470=CARTESIAN_POINT('Ctrl Pts',(-11.3586934235808,0.72264755563789,
13.3016655575425));
#126471=CARTESIAN_POINT('Ctrl Pts',(-11.420773006215,0.800000000000004,
13.3545496522288));
#126472=CARTESIAN_POINT('',(-11.671247785185,0.649999999999997,12.9917155521093));
#126473=CARTESIAN_POINT('Ctrl Pts',(-11.7266199462546,0.800000000000004,
13.1403933192747));
#126474=CARTESIAN_POINT('Ctrl Pts',(-11.6981576204711,0.722647555638155,
13.0639701679279));
#126475=CARTESIAN_POINT('Ctrl Pts',(-11.671247785185,0.649999999999997,
12.9917155521093));
#126476=CARTESIAN_POINT('Ctrl Pts',(-11.671247785185,0.649999999999997,
12.9917155521093));
#126477=CARTESIAN_POINT('Ctrl Pts',(-11.7377318471753,0.722647555638136,
13.0307634488963));
#126478=CARTESIAN_POINT('Ctrl Pts',(-11.8080515281268,0.800000000000004,
13.0720641089596));
#126479=CARTESIAN_POINT('',(-11.9917155521093,0.65,12.671247785185));
#126480=CARTESIAN_POINT('Ctrl Pts',(-12.0720641089596,0.800000000000004,
12.8080515281268));
#126481=CARTESIAN_POINT('Ctrl Pts',(-12.0307634488962,0.72264755563786,
12.7377318471751));
#126482=CARTESIAN_POINT('Ctrl Pts',(-11.9917155521093,0.65,12.671247785185));
#126483=CARTESIAN_POINT('Ctrl Pts',(-11.9917155521093,0.65,12.671247785185));
#126484=CARTESIAN_POINT('Ctrl Pts',(-12.0639701679277,0.722647555637912,
12.698157620471));
#126485=CARTESIAN_POINT('Ctrl Pts',(-12.1403933192747,0.800000000000003,
12.7266199462546));
#126486=CARTESIAN_POINT('',(-12.2516660498395,0.649999999999997,12.3));
#126487=CARTESIAN_POINT('Ctrl Pts',(-12.3545496522288,0.800000000000003,
12.420773006215));
#126488=CARTESIAN_POINT('Ctrl Pts',(-12.301665557543,0.722647555638627,
12.3586934235814));
#126489=CARTESIAN_POINT('Ctrl Pts',(-12.2516660498395,0.649999999999997,
12.3));
#126490=CARTESIAN_POINT('Ctrl Pts',(-12.2516660498395,0.649999999999997,
12.3));
#126491=CARTESIAN_POINT('Ctrl Pts',(-12.3274957995473,0.722647555638123,
12.3139541320571));
#126492=CARTESIAN_POINT('Ctrl Pts',(-12.4077003425078,0.800000000000004,
12.3287133101945));
#126493=CARTESIAN_POINT('',(-12.4432008140434,0.65,11.8892523726467));
#126494=CARTESIAN_POINT('Ctrl Pts',(-12.5654933957747,0.800000000000004,
11.9903250154551));
#126495=CARTESIAN_POINT('Ctrl Pts',(-12.5026327229221,0.722647555638167,
11.9383717878433));
#126496=CARTESIAN_POINT('Ctrl Pts',(-12.4432008140434,0.65,11.8892523726467));
#126497=CARTESIAN_POINT('Ctrl Pts',(-12.4432008140434,0.65,11.8892523726467));
#126498=CARTESIAN_POINT('Ctrl Pts',(-12.5203016490672,0.722647555638142,
11.8898268122335));
#126499=CARTESIAN_POINT('Ctrl Pts',(-12.6018506091889,0.800000000000003,
11.8904343925656));
#126500=CARTESIAN_POINT('',(-12.5605001578317,0.65,11.451485261934));
#126501=CARTESIAN_POINT('Ctrl Pts',(-12.6984859206923,0.800000000000003,
11.5297865002293));
#126502=CARTESIAN_POINT('Ctrl Pts',(-12.6275586594089,0.722647555638257,
11.489538200171));
#126503=CARTESIAN_POINT('Ctrl Pts',(-12.5605001578317,0.65,11.451485261934));
#126504=CARTESIAN_POINT('Ctrl Pts',(-12.5605001578317,0.65,11.451485261934));
#126505=CARTESIAN_POINT('Ctrl Pts',(-12.6365294083144,0.72264755563821,
11.4386625549941));
#126506=CARTESIAN_POINT('Ctrl Pts',(-12.7169449617097,0.800000000000003,
11.4251000765));
#126507=CARTESIAN_POINT('Ctrl Pts',(-12.7494863164095,0.800000000000002,
11.0531506902789));
#126508=CARTESIAN_POINT('Ctrl Pts',(-12.6726475556382,0.722647555638153,
11.0258302420047));
#126509=CARTESIAN_POINT('Ctrl Pts',(-12.6,0.649999999999998,11.));
#126510=CARTESIAN_POINT('',(-12.45,0.5,11.));
#126511=CARTESIAN_POINT('',(-12.6,0.65,11.));
#126512=CARTESIAN_POINT('Origin',(-10.,0.5,11.));
#126513=CARTESIAN_POINT('Origin',(-7.55347823430896,2.9,12.4125));
#126514=CARTESIAN_POINT('',(-7.74833395016046,2.9,12.3));
#126515=CARTESIAN_POINT('',(-7.43862251845746,2.9,12.6635640646055));
#126516=CARTESIAN_POINT('',(-7.74833395016046,2.9,12.3));
#126517=CARTESIAN_POINT('Origin',(-7.27862251845746,0.5,12.3864359353945));
#126518=CARTESIAN_POINT('',(-7.74833395016046,0.5,12.3));
#126519=CARTESIAN_POINT('Origin',(-7.74833395016046,0.5,12.3));
#126520=CARTESIAN_POINT('Origin',(-7.56071843093727,0.5,12.8379350986449));
#126521=CARTESIAN_POINT('',(-8.00828444789066,2.9,12.671247785185));
#126522=CARTESIAN_POINT('',(-8.00828444789066,2.9,12.671247785185));
#126523=CARTESIAN_POINT('',(-8.00828444789066,0.5,12.671247785185));
#126524=CARTESIAN_POINT('Origin',(-8.00828444789066,0.5,12.671247785185));
#126525=CARTESIAN_POINT('',(-7.76641046603697,2.9,13.083069320443));
#126526=CARTESIAN_POINT('Origin',(-7.83592444818889,2.9,12.8158749973645));
#126527=CARTESIAN_POINT('Origin',(-8.18412500263553,2.9,13.1640755518111));
#126528=CARTESIAN_POINT('',(-8.328752214815,2.9,12.9917155521093));
#126529=CARTESIAN_POINT('',(-8.16206490135509,2.9,13.4392815690627));
#126530=CARTESIAN_POINT('',(-8.328752214815,2.9,12.9917155521093));
#126531=CARTESIAN_POINT('Origin',(-7.91693067955702,0.5,13.233589533963));
#126532=CARTESIAN_POINT('',(-8.328752214815,0.5,12.9917155521093));
#126533=CARTESIAN_POINT('Origin',(-8.328752214815,0.5,12.9917155521093));
#126534=CARTESIAN_POINT('Origin',(-8.33643593539449,0.5,13.5613774815425));
#126535=CARTESIAN_POINT('',(-8.7,2.9,13.2516660498395));
#126536=CARTESIAN_POINT('',(-8.7,2.9,13.2516660498395));
#126537=CARTESIAN_POINT('',(-8.7,0.5,13.2516660498395));
#126538=CARTESIAN_POINT('Origin',(-8.7,0.5,13.2516660498395));
#126539=CARTESIAN_POINT('',(-8.61356406460551,2.9,13.7213774815425));
#126540=CARTESIAN_POINT('Origin',(-8.5875,2.9,13.446521765691));
#126541=CARTESIAN_POINT('Origin',(-9.03379309510499,2.9,13.6546316537202));
#126542=CARTESIAN_POINT('',(-9.11074762735326,2.9,13.4432008140434));
#126543=CARTESIAN_POINT('',(-9.10718938218246,2.9,13.9207857163291));
#126544=CARTESIAN_POINT('',(-9.11074762735326,2.9,13.4432008140434));
#126545=CARTESIAN_POINT('Origin',(-8.80648774353097,0.5,13.8113392704649));
#126546=CARTESIAN_POINT('',(-9.11074762735326,0.5,13.4432008140434));
#126547=CARTESIAN_POINT('Origin',(-9.11074762735326,0.5,13.4432008140434));
#126548=CARTESIAN_POINT('Origin',(-9.31280381763391,0.5,13.9758799382605));
#126549=CARTESIAN_POINT('',(-9.54851473806598,2.9,13.5605001578317));
#126550=CARTESIAN_POINT('',(-9.54851473806598,2.9,13.5605001578317));
#126551=CARTESIAN_POINT('',(-9.54851473806598,0.5,13.5605001578317));
#126552=CARTESIAN_POINT('Origin',(-9.54851473806598,0.5,13.5605001578317));
#126553=CARTESIAN_POINT('',(-9.62794229859782,2.9,14.0314473551139));
#126554=CARTESIAN_POINT('Origin',(-9.50944389809092,2.9,13.7820819022595));
#126555=CARTESIAN_POINT('Origin',(-10.,2.9,13.825));
#126556=CARTESIAN_POINT('',(-10.,2.9,13.6));
#126557=CARTESIAN_POINT('',(-10.16,2.9,14.05));
#126558=CARTESIAN_POINT('',(-10.,2.9,13.6));
#126559=CARTESIAN_POINT('Origin',(-9.84,0.5,14.05));
#126560=CARTESIAN_POINT('',(-10.,0.5,13.6));
#126561=CARTESIAN_POINT('Origin',(-10.,0.5,13.6));
#126562=CARTESIAN_POINT('Origin',(-10.3720577014022,0.5,14.0314473551139));
#126563=CARTESIAN_POINT('',(-10.451485261934,2.9,13.5605001578317));
#126564=CARTESIAN_POINT('',(-10.451485261934,2.9,13.5605001578317));
#126565=CARTESIAN_POINT('',(-10.451485261934,0.5,13.5605001578317));
#126566=CARTESIAN_POINT('Origin',(-10.451485261934,0.5,13.5605001578317));
#126567=CARTESIAN_POINT('',(-10.6871961823661,2.9,13.9758799382605));
#126568=CARTESIAN_POINT('Origin',(-10.4905561019091,2.9,13.7820819022595));
#126569=CARTESIAN_POINT('Origin',(-10.966206904895,2.9,13.6546316537202));
#126570=CARTESIAN_POINT('',(-10.8892523726467,2.9,13.4432008140434));
#126571=CARTESIAN_POINT('',(-11.193512256469,2.9,13.8113392704649));
#126572=CARTESIAN_POINT('',(-10.8892523726467,2.9,13.4432008140434));
#126573=CARTESIAN_POINT('Origin',(-10.8928106178175,0.5,13.9207857163291));
#126574=CARTESIAN_POINT('',(-10.8892523726467,0.5,13.4432008140434));
#126575=CARTESIAN_POINT('Origin',(-10.8892523726467,0.5,13.4432008140434));
#126576=CARTESIAN_POINT('Origin',(-11.3864359353945,0.5,13.7213774815425));
#126577=CARTESIAN_POINT('',(-11.3,2.9,13.2516660498395));
#126578=CARTESIAN_POINT('',(-11.3,2.9,13.2516660498395));
#126579=CARTESIAN_POINT('',(-11.3,0.5,13.2516660498395));
#126580=CARTESIAN_POINT('Origin',(-11.3,0.5,13.2516660498395));
#126581=CARTESIAN_POINT('',(-11.6635640646055,2.9,13.5613774815425));
#126582=CARTESIAN_POINT('Origin',(-11.4125,2.9,13.446521765691));
#126583=CARTESIAN_POINT('Origin',(-11.8158749973645,2.9,13.1640755518111));
#126584=CARTESIAN_POINT('',(-11.671247785185,2.9,12.9917155521093));
#126585=CARTESIAN_POINT('',(-12.083069320443,2.9,13.233589533963));
#126586=CARTESIAN_POINT('',(-11.671247785185,2.9,12.9917155521093));
#126587=CARTESIAN_POINT('Origin',(-11.8379350986449,0.5,13.4392815690627));
#126588=CARTESIAN_POINT('',(-11.671247785185,0.5,12.9917155521093));
#126589=CARTESIAN_POINT('Origin',(-11.671247785185,0.5,12.9917155521093));
#126590=CARTESIAN_POINT('Origin',(-12.233589533963,0.5,13.083069320443));
#126591=CARTESIAN_POINT('',(-11.9917155521093,2.9,12.671247785185));
#126592=CARTESIAN_POINT('',(-11.9917155521093,2.9,12.671247785185));
#126593=CARTESIAN_POINT('',(-11.9917155521093,0.5,12.671247785185));
#126594=CARTESIAN_POINT('Origin',(-11.9917155521093,0.5,12.671247785185));
#126595=CARTESIAN_POINT('',(-12.4392815690627,2.9,12.8379350986449));
#126596=CARTESIAN_POINT('Origin',(-12.1640755518111,2.9,12.8158749973645));
#126597=CARTESIAN_POINT('Origin',(-12.446521765691,2.9,12.4125));
#126598=CARTESIAN_POINT('',(-12.2516660498395,2.9,12.3));
#126599=CARTESIAN_POINT('',(-12.7213774815425,2.9,12.3864359353945));
#126600=CARTESIAN_POINT('',(-12.2516660498395,2.9,12.3));
#126601=CARTESIAN_POINT('Origin',(-12.5613774815425,0.5,12.6635640646055));
#126602=CARTESIAN_POINT('',(-12.2516660498395,0.5,12.3));
#126603=CARTESIAN_POINT('Origin',(-12.2516660498395,0.5,12.3));
#126604=CARTESIAN_POINT('Origin',(-12.8113392704649,0.5,12.193512256469));
#126605=CARTESIAN_POINT('',(-12.4432008140434,2.9,11.8892523726467));
#126606=CARTESIAN_POINT('',(-12.4432008140434,2.9,11.8892523726467));
#126607=CARTESIAN_POINT('',(-12.4432008140434,0.5,11.8892523726467));
#126608=CARTESIAN_POINT('Origin',(-12.4432008140434,0.5,11.8892523726467));
#126609=CARTESIAN_POINT('',(-12.9207857163291,2.9,11.8928106178175));
#126610=CARTESIAN_POINT('Origin',(-12.6546316537202,2.9,11.966206904895));
#126611=CARTESIAN_POINT('Origin',(-12.7820819022595,2.9,11.4905561019091));
#126612=CARTESIAN_POINT('',(-12.5605001578317,2.9,11.451485261934));
#126613=CARTESIAN_POINT('',(-13.0314473551139,2.9,11.3720577014022));
#126614=CARTESIAN_POINT('',(-12.5605001578317,2.9,11.451485261934));
#126615=CARTESIAN_POINT('Origin',(-12.9758799382605,0.5,11.6871961823661));
#126616=CARTESIAN_POINT('',(-12.5605001578317,0.5,11.451485261934));
#126617=CARTESIAN_POINT('Origin',(-12.5605001578317,0.5,11.451485261934));
#126618=CARTESIAN_POINT('Origin',(-13.05,0.5,11.16));
#126619=CARTESIAN_POINT('',(-12.6,2.9,11.));
#126620=CARTESIAN_POINT('',(-12.6,2.9,11.));
#126621=CARTESIAN_POINT('',(-12.6,0.5,11.));
#126622=CARTESIAN_POINT('Origin',(-12.6,0.5,11.));
#126623=CARTESIAN_POINT('',(-13.05,2.9,10.84));
#126624=CARTESIAN_POINT('Origin',(-12.825,2.9,11.));
#126625=CARTESIAN_POINT('Origin',(-12.7820819022595,2.9,10.5094438980909));
#126626=CARTESIAN_POINT('',(-12.5605001578317,2.9,10.548514738066));
#126627=CARTESIAN_POINT('',(-12.9758799382605,2.9,10.3128038176339));
#126628=CARTESIAN_POINT('',(-12.5605001578317,2.9,10.548514738066));
#126629=CARTESIAN_POINT('Origin',(-13.0314473551139,0.5,10.6279422985978));
#126630=CARTESIAN_POINT('',(-12.5605001578317,0.5,10.548514738066));
#126631=CARTESIAN_POINT('Origin',(-12.5605001578317,0.5,10.548514738066));
#126632=CARTESIAN_POINT('Origin',(-12.9207857163291,0.5,10.1071893821825));
#126633=CARTESIAN_POINT('',(-12.4432008140434,2.9,10.1107476273533));
#126634=CARTESIAN_POINT('',(-12.4432008140434,2.9,10.1107476273533));
#126635=CARTESIAN_POINT('',(-12.4432008140434,0.5,10.1107476273533));
#126636=CARTESIAN_POINT('Origin',(-12.4432008140434,0.5,10.1107476273533));
#126637=CARTESIAN_POINT('',(-12.8113392704649,2.9,9.80648774353097));
#126638=CARTESIAN_POINT('Origin',(-12.6546316537202,2.9,10.033793095105));
#126639=CARTESIAN_POINT('Origin',(-12.446521765691,2.9,9.5875));
#126640=CARTESIAN_POINT('',(-12.2516660498395,2.9,9.7));
#126641=CARTESIAN_POINT('',(-12.5613774815425,2.9,9.33643593539449));
#126642=CARTESIAN_POINT('',(-12.2516660498395,2.9,9.7));
#126643=CARTESIAN_POINT('Origin',(-12.7213774815425,0.5,9.61356406460551));
#126644=CARTESIAN_POINT('',(-12.2516660498395,0.5,9.7));
#126645=CARTESIAN_POINT('Origin',(-12.2516660498395,0.5,9.7));
#126646=CARTESIAN_POINT('Origin',(-12.4392815690627,0.5,9.16206490135509));
#126647=CARTESIAN_POINT('',(-11.9917155521093,2.9,9.328752214815));
#126648=CARTESIAN_POINT('',(-11.9917155521093,2.9,9.328752214815));
#126649=CARTESIAN_POINT('',(-11.9917155521093,0.5,9.328752214815));
#126650=CARTESIAN_POINT('Origin',(-11.9917155521093,0.5,9.328752214815));
#126651=CARTESIAN_POINT('',(-12.233589533963,2.9,8.91693067955702));
#126652=CARTESIAN_POINT('Origin',(-12.1640755518111,2.9,9.18412500263553));
#126653=CARTESIAN_POINT('Origin',(-11.8158749973645,2.9,8.83592444818889));
#126654=CARTESIAN_POINT('',(-11.671247785185,2.9,9.00828444789066));
#126655=CARTESIAN_POINT('',(-11.8379350986449,2.9,8.56071843093727));
#126656=CARTESIAN_POINT('',(-11.671247785185,2.9,9.00828444789066));
#126657=CARTESIAN_POINT('Origin',(-12.083069320443,0.5,8.76641046603697));
#126658=CARTESIAN_POINT('',(-11.671247785185,0.5,9.00828444789066));
#126659=CARTESIAN_POINT('Origin',(-11.671247785185,0.5,9.00828444789066));
#126660=CARTESIAN_POINT('Origin',(-11.6635640646055,0.5,8.43862251845746));
#126661=CARTESIAN_POINT('',(-11.3,2.9,8.74833395016046));
#126662=CARTESIAN_POINT('',(-11.3,2.9,8.74833395016046));
#126663=CARTESIAN_POINT('',(-11.3,0.5,8.74833395016046));
#126664=CARTESIAN_POINT('Origin',(-11.3,0.5,8.74833395016046));
#126665=CARTESIAN_POINT('',(-11.3864359353945,2.9,8.27862251845746));
#126666=CARTESIAN_POINT('Origin',(-11.4125,2.9,8.55347823430896));
#126667=CARTESIAN_POINT('Origin',(-10.966206904895,2.9,8.34536834627981));
#126668=CARTESIAN_POINT('',(-10.8892523726467,2.9,8.55679918595664));
#126669=CARTESIAN_POINT('',(-10.8928106178175,2.9,8.07921428367087));
#126670=CARTESIAN_POINT('',(-10.8892523726467,2.9,8.55679918595664));
#126671=CARTESIAN_POINT('Origin',(-11.193512256469,0.5,8.18866072953509));
#126672=CARTESIAN_POINT('',(-10.8892523726467,0.5,8.55679918595664));
#126673=CARTESIAN_POINT('Origin',(-10.8892523726467,0.5,8.55679918595664));
#126674=CARTESIAN_POINT('Origin',(-10.6871961823661,0.5,8.02412006173947));
#126675=CARTESIAN_POINT('',(-10.451485261934,2.9,8.43949984216826));
#126676=CARTESIAN_POINT('',(-10.451485261934,2.9,8.43949984216826));
#126677=CARTESIAN_POINT('',(-10.451485261934,0.5,8.43949984216826));
#126678=CARTESIAN_POINT('Origin',(-10.451485261934,0.5,8.43949984216826));
#126679=CARTESIAN_POINT('',(-10.3720577014022,2.9,7.96855264488606));
#126680=CARTESIAN_POINT('Origin',(-10.4905561019091,2.9,8.21791809774051));
#126681=CARTESIAN_POINT('Origin',(-10.,2.9,8.175));
#126682=CARTESIAN_POINT('',(-10.,2.9,8.4));
#126683=CARTESIAN_POINT('',(-9.84,2.9,7.95));
#126684=CARTESIAN_POINT('',(-10.,2.9,8.4));
#126685=CARTESIAN_POINT('Origin',(-10.16,0.5,7.95));
#126686=CARTESIAN_POINT('',(-10.,0.5,8.4));
#126687=CARTESIAN_POINT('Origin',(-10.,0.5,8.4));
#126688=CARTESIAN_POINT('Origin',(-9.62794229859782,0.5,7.96855264488606));
#126689=CARTESIAN_POINT('',(-9.54851473806598,2.9,8.43949984216826));
#126690=CARTESIAN_POINT('',(-9.54851473806598,2.9,8.43949984216826));
#126691=CARTESIAN_POINT('',(-9.54851473806598,0.5,8.43949984216826));
#126692=CARTESIAN_POINT('Origin',(-9.54851473806598,0.5,8.43949984216826));
#126693=CARTESIAN_POINT('',(-9.31280381763391,2.9,8.02412006173947));
#126694=CARTESIAN_POINT('Origin',(-9.50944389809092,2.9,8.21791809774051));
#126695=CARTESIAN_POINT('Origin',(-9.03379309510498,2.9,8.34536834627981));
#126696=CARTESIAN_POINT('',(-9.11074762735326,2.9,8.55679918595664));
#126697=CARTESIAN_POINT('',(-8.80648774353097,2.9,8.18866072953509));
#126698=CARTESIAN_POINT('',(-9.11074762735326,2.9,8.55679918595664));
#126699=CARTESIAN_POINT('Origin',(-9.10718938218246,0.5,8.07921428367087));
#126700=CARTESIAN_POINT('',(-9.11074762735326,0.5,8.55679918595664));
#126701=CARTESIAN_POINT('Origin',(-9.11074762735326,0.5,8.55679918595664));
#126702=CARTESIAN_POINT('Origin',(-8.61356406460551,0.5,8.27862251845747));
#126703=CARTESIAN_POINT('',(-8.7,2.9,8.74833395016046));
#126704=CARTESIAN_POINT('',(-8.7,2.9,8.74833395016046));
#126705=CARTESIAN_POINT('',(-8.7,0.5,8.74833395016046));
#126706=CARTESIAN_POINT('Origin',(-8.7,0.5,8.74833395016046));
#126707=CARTESIAN_POINT('',(-8.33643593539449,2.9,8.43862251845747));
#126708=CARTESIAN_POINT('Origin',(-8.5875,2.9,8.55347823430897));
#126709=CARTESIAN_POINT('Origin',(-8.18412500263553,2.9,8.83592444818889));
#126710=CARTESIAN_POINT('',(-8.328752214815,2.9,9.00828444789066));
#126711=CARTESIAN_POINT('',(-7.91693067955702,2.9,8.76641046603697));
#126712=CARTESIAN_POINT('',(-8.328752214815,2.9,9.00828444789066));
#126713=CARTESIAN_POINT('Origin',(-8.16206490135509,0.5,8.56071843093727));
#126714=CARTESIAN_POINT('',(-8.328752214815,0.5,9.00828444789066));
#126715=CARTESIAN_POINT('Origin',(-8.328752214815,0.5,9.00828444789066));
#126716=CARTESIAN_POINT('Origin',(-7.76641046603696,0.5,8.91693067955702));
#126717=CARTESIAN_POINT('',(-8.00828444789066,2.9,9.328752214815));
#126718=CARTESIAN_POINT('',(-8.00828444789066,2.9,9.328752214815));
#126719=CARTESIAN_POINT('',(-8.00828444789066,0.5,9.328752214815));
#126720=CARTESIAN_POINT('Origin',(-8.00828444789066,0.5,9.328752214815));
#126721=CARTESIAN_POINT('',(-7.56071843093727,2.9,9.16206490135509));
#126722=CARTESIAN_POINT('Origin',(-7.83592444818889,2.9,9.18412500263553));
#126723=CARTESIAN_POINT('Origin',(-7.55347823430896,2.9,9.5875));
#126724=CARTESIAN_POINT('',(-7.74833395016046,2.9,9.7));
#126725=CARTESIAN_POINT('',(-7.27862251845746,2.9,9.61356406460551));
#126726=CARTESIAN_POINT('',(-7.74833395016046,2.9,9.7));
#126727=CARTESIAN_POINT('Origin',(-7.43862251845746,0.5,9.33643593539449));
#126728=CARTESIAN_POINT('',(-7.74833395016046,0.5,9.7));
#126729=CARTESIAN_POINT('Origin',(-7.74833395016046,0.5,9.7));
#126730=CARTESIAN_POINT('Origin',(-7.18866072953509,0.5,9.80648774353097));
#126731=CARTESIAN_POINT('',(-7.55679918595664,2.9,10.1107476273533));
#126732=CARTESIAN_POINT('',(-7.55679918595664,2.9,10.1107476273533));
#126733=CARTESIAN_POINT('',(-7.55679918595664,0.5,10.1107476273533));
#126734=CARTESIAN_POINT('Origin',(-7.55679918595664,0.5,10.1107476273533));
#126735=CARTESIAN_POINT('',(-7.07921428367087,2.9,10.1071893821825));
#126736=CARTESIAN_POINT('Origin',(-7.34536834627981,2.9,10.033793095105));
#126737=CARTESIAN_POINT('Origin',(-7.21791809774051,2.9,10.5094438980909));
#126738=CARTESIAN_POINT('',(-7.43949984216826,2.9,10.548514738066));
#126739=CARTESIAN_POINT('',(-6.96855264488606,2.9,10.6279422985978));
#126740=CARTESIAN_POINT('',(-7.43949984216826,2.9,10.548514738066));
#126741=CARTESIAN_POINT('Origin',(-7.02412006173947,0.5,10.3128038176339));
#126742=CARTESIAN_POINT('',(-7.43949984216826,0.5,10.548514738066));
#126743=CARTESIAN_POINT('Origin',(-7.43949984216826,0.5,10.548514738066));
#126744=CARTESIAN_POINT('Origin',(-6.95,0.5,10.84));
#126745=CARTESIAN_POINT('',(-7.4,2.9,11.));
#126746=CARTESIAN_POINT('',(-7.4,2.9,11.));
#126747=CARTESIAN_POINT('',(-7.4,0.5,11.));
#126748=CARTESIAN_POINT('Origin',(-7.4,0.5,11.));
#126749=CARTESIAN_POINT('',(-6.95,2.9,11.16));
#126750=CARTESIAN_POINT('Origin',(-7.175,2.9,11.));
#126751=CARTESIAN_POINT('Origin',(-10.,3.3,11.));
#126752=CARTESIAN_POINT('Origin',(-10.,3.3,8.45));
#126753=CARTESIAN_POINT('Origin',(-10.,0.5,11.));
#126754=CARTESIAN_POINT('',(-11.5933756729741,0.5,11.));
#126755=CARTESIAN_POINT('Origin',(-10.,0.5,11.));
#126756=CARTESIAN_POINT('Origin',(-10.,0.6,11.));
#126757=CARTESIAN_POINT('',(-11.3903449147952,0.7,11.0918519675297));
#126758=CARTESIAN_POINT('',(-11.4433756729741,0.650000000000001,11.));
#126759=CARTESIAN_POINT('Ctrl Pts',(-11.3903449147952,0.699999999999999,
11.0918519675297));
#126760=CARTESIAN_POINT('Ctrl Pts',(-11.4163929392269,0.676982733747201,
11.0467354657773));
#126761=CARTESIAN_POINT('Ctrl Pts',(-11.4433756729741,0.650000000000001,
11.));
#126762=CARTESIAN_POINT('',(-10.7747185946659,0.7,12.1581480324703));
#126763=CARTESIAN_POINT('Origin',(-10.,0.7,11.));
#126764=CARTESIAN_POINT('',(-10.721687836487,0.65,12.25));
#126765=CARTESIAN_POINT('Ctrl Pts',(-10.721687836487,0.65,12.25));
#126766=CARTESIAN_POINT('Ctrl Pts',(-10.7486705702342,0.676982733747207,
12.2032645342227));
#126767=CARTESIAN_POINT('Ctrl Pts',(-10.7747185946659,0.7,12.1581480324703));
#126768=CARTESIAN_POINT('',(-10.6156263201293,0.7,12.25));
#126769=CARTESIAN_POINT('Ctrl Pts',(-10.6156263201293,0.7,12.25));
#126770=CARTESIAN_POINT('Ctrl Pts',(-10.6677223689926,0.67698273374721,
12.25));
#126771=CARTESIAN_POINT('Ctrl Pts',(-10.721687836487,0.65,12.25));
#126772=CARTESIAN_POINT('',(-9.38437367987071,0.7,12.25));
#126773=CARTESIAN_POINT('Origin',(-10.,0.7,11.));
#126774=CARTESIAN_POINT('',(-9.27831216351297,0.65,12.25));
#126775=CARTESIAN_POINT('Ctrl Pts',(-9.27831216351297,0.65,12.25));
#126776=CARTESIAN_POINT('Ctrl Pts',(-9.3322776310074,0.676982733747216,
12.25));
#126777=CARTESIAN_POINT('Ctrl Pts',(-9.38437367987071,0.7,12.25));
#126778=CARTESIAN_POINT('',(-9.2252814053341,0.7,12.1581480324703));
#126779=CARTESIAN_POINT('Ctrl Pts',(-9.22528140533409,0.700000000000001,
12.1581480324703));
#126780=CARTESIAN_POINT('Ctrl Pts',(-9.25132942976576,0.676982733747215,
12.2032645342227));
#126781=CARTESIAN_POINT('Ctrl Pts',(-9.27831216351297,0.65,12.25));
#126782=CARTESIAN_POINT('',(-8.60965508520481,0.7,11.0918519675297));
#126783=CARTESIAN_POINT('Origin',(-10.,0.7,11.));
#126784=CARTESIAN_POINT('',(-8.55662432702594,0.650000000000001,11.));
#126785=CARTESIAN_POINT('Ctrl Pts',(-8.55662432702594,0.650000000000001,
11.));
#126786=CARTESIAN_POINT('Ctrl Pts',(-8.58360706077315,0.676982733747216,
11.0467354657773));
#126787=CARTESIAN_POINT('Ctrl Pts',(-8.60965508520481,0.7,11.0918519675297));
#126788=CARTESIAN_POINT('',(-8.60965508520481,0.7,10.9081480324703));
#126789=CARTESIAN_POINT('Ctrl Pts',(-8.60965508520481,0.7,10.9081480324703));
#126790=CARTESIAN_POINT('Ctrl Pts',(-8.58360706077314,0.676982733747203,
10.9532645342227));
#126791=CARTESIAN_POINT('Ctrl Pts',(-8.55662432702594,0.650000000000001,
11.));
#126792=CARTESIAN_POINT('',(-9.22528140533409,0.7,9.84185196752971));
#126793=CARTESIAN_POINT('Origin',(-10.,0.7,11.));
#126794=CARTESIAN_POINT('',(-9.27831216351297,0.649999999999999,9.75));
#126795=CARTESIAN_POINT('Ctrl Pts',(-9.27831216351297,0.649999999999999,
9.75));
#126796=CARTESIAN_POINT('Ctrl Pts',(-9.25132942976575,0.676982733747217,
9.79673546577728));
#126797=CARTESIAN_POINT('Ctrl Pts',(-9.22528140533409,0.7,9.84185196752971));
#126798=CARTESIAN_POINT('',(-9.38437367987072,0.7,9.75));
#126799=CARTESIAN_POINT('Ctrl Pts',(-9.38437367987071,0.7,9.75));
#126800=CARTESIAN_POINT('Ctrl Pts',(-9.33227763100738,0.676982733747206,
9.75));
#126801=CARTESIAN_POINT('Ctrl Pts',(-9.27831216351297,0.649999999999999,
9.75));
#126802=CARTESIAN_POINT('',(-10.6156263201293,0.7,9.75));
#126803=CARTESIAN_POINT('Origin',(-10.,0.7,11.));
#126804=CARTESIAN_POINT('',(-10.721687836487,0.649999999999999,9.75));
#126805=CARTESIAN_POINT('Ctrl Pts',(-10.721687836487,0.649999999999999,
9.75));
#126806=CARTESIAN_POINT('Ctrl Pts',(-10.6677223689926,0.67698273374721,
9.75));
#126807=CARTESIAN_POINT('Ctrl Pts',(-10.6156263201293,0.7,9.75));
#126808=CARTESIAN_POINT('',(-10.7747185946659,0.7,9.84185196752971));
#126809=CARTESIAN_POINT('Ctrl Pts',(-10.7747185946659,0.7,9.84185196752971));
#126810=CARTESIAN_POINT('Ctrl Pts',(-10.7486705702342,0.676982733747205,
9.79673546577726));
#126811=CARTESIAN_POINT('Ctrl Pts',(-10.721687836487,0.649999999999999,
9.75));
#126812=CARTESIAN_POINT('',(-11.3903449147952,0.7,10.9081480324703));
#126813=CARTESIAN_POINT('Origin',(-10.,0.7,11.));
#126814=CARTESIAN_POINT('Ctrl Pts',(-11.4433756729741,0.650000000000001,
11.));
#126815=CARTESIAN_POINT('Ctrl Pts',(-11.4163929392269,0.676982733747204,
10.9532645342227));
#126816=CARTESIAN_POINT('Ctrl Pts',(-11.3903449147952,0.7,10.9081480324703));
#126817=CARTESIAN_POINT('',(-11.4933756729741,0.6,11.));
#126818=CARTESIAN_POINT('Origin',(-10.,0.6,11.));
#126819=CARTESIAN_POINT('',(-11.3903449147952,0.5,10.9081480324703));
#126820=CARTESIAN_POINT('',(-11.3903449147952,0.6,10.9081480324703));
#126821=CARTESIAN_POINT('',(-10.7747185946659,0.5,9.84185196752971));
#126822=CARTESIAN_POINT('',(-10.7747185946659,0.6,9.84185196752971));
#126823=CARTESIAN_POINT('Origin',(-10.,0.5,11.));
#126824=CARTESIAN_POINT('Origin',(-10.,0.6,11.));
#126825=CARTESIAN_POINT('',(-9.38437367987072,0.5,9.75));
#126826=CARTESIAN_POINT('',(-9.38437367987072,0.6,9.75));
#126827=CARTESIAN_POINT('',(-10.6156263201293,0.5,9.75));
#126828=CARTESIAN_POINT('Origin',(-10.,0.5,11.));
#126829=CARTESIAN_POINT('',(-10.6156263201293,0.6,9.75));
#126830=CARTESIAN_POINT('Origin',(-10.,0.6,11.));
#126831=CARTESIAN_POINT('',(-10.7747185946659,0.5,12.1581480324703));
#126832=CARTESIAN_POINT('',(-10.7747185946659,0.6,12.1581480324703));
#126833=CARTESIAN_POINT('',(-11.3903449147952,0.5,11.0918519675297));
#126834=CARTESIAN_POINT('',(-11.3903449147952,0.6,11.0918519675297));
#126835=CARTESIAN_POINT('Origin',(-10.,0.5,11.));
#126836=CARTESIAN_POINT('Origin',(-10.,0.6,11.));
#126837=CARTESIAN_POINT('',(-8.60965508520481,0.5,10.9081480324703));
#126838=CARTESIAN_POINT('',(-8.60965508520481,0.6,10.9081480324703));
#126839=CARTESIAN_POINT('',(-9.22528140533409,0.5,9.84185196752971));
#126840=CARTESIAN_POINT('Origin',(-10.,0.5,11.));
#126841=CARTESIAN_POINT('',(-9.22528140533409,0.6,9.84185196752971));
#126842=CARTESIAN_POINT('Origin',(-10.,0.6,11.));
#126843=CARTESIAN_POINT('',(-9.38437367987071,0.5,12.25));
#126844=CARTESIAN_POINT('',(-9.38437367987071,0.6,12.25));
#126845=CARTESIAN_POINT('',(-10.6156263201293,0.5,12.25));
#126846=CARTESIAN_POINT('',(-10.6156263201293,0.6,12.25));
#126847=CARTESIAN_POINT('Origin',(-10.,0.5,11.));
#126848=CARTESIAN_POINT('Origin',(-10.,0.6,11.));
#126849=CARTESIAN_POINT('',(-9.2252814053341,0.5,12.1581480324703));
#126850=CARTESIAN_POINT('',(-9.2252814053341,0.6,12.1581480324703));
#126851=CARTESIAN_POINT('',(-8.60965508520481,0.5,11.0918519675297));
#126852=CARTESIAN_POINT('Origin',(-10.,0.5,11.));
#126853=CARTESIAN_POINT('',(-8.60965508520481,0.6,11.0918519675297));
#126854=CARTESIAN_POINT('Origin',(-10.721687836487,0.5,12.25));
#126855=CARTESIAN_POINT('',(-10.3608439182435,0.5,12.25));
#126856=CARTESIAN_POINT('',(-10.721687836487,1.8,12.25));
#126857=CARTESIAN_POINT('',(-10.721687836487,0.5,12.25));
#126858=CARTESIAN_POINT('',(-9.27831216351297,1.8,12.25));
#126859=CARTESIAN_POINT('',(-9.27831216351297,1.8,12.25));
#126860=CARTESIAN_POINT('',(-9.27831216351297,0.5,12.25));
#126861=CARTESIAN_POINT('Origin',(-11.4433756729741,0.5,11.));
#126862=CARTESIAN_POINT('',(-11.2629537138523,0.5,11.3125));
#126863=CARTESIAN_POINT('',(-11.4433756729741,1.8,11.));
#126864=CARTESIAN_POINT('',(-11.4433756729741,0.5,11.));
#126865=CARTESIAN_POINT('',(-10.721687836487,1.8,12.25));
#126866=CARTESIAN_POINT('Origin',(-10.721687836487,0.5,9.75));
#126867=CARTESIAN_POINT('',(-10.9021097956088,0.5,10.0625));
#126868=CARTESIAN_POINT('',(-10.721687836487,1.8,9.75));
#126869=CARTESIAN_POINT('',(-10.721687836487,0.5,9.75));
#126870=CARTESIAN_POINT('',(-11.4433756729741,1.8,11.));
#126871=CARTESIAN_POINT('Origin',(-10.,0.5,11.));
#126872=CARTESIAN_POINT('Origin',(-10.,0.5,11.));
#126873=CARTESIAN_POINT('Origin',(-10.,0.5,11.));
#126874=CARTESIAN_POINT('',(-9.63915608175648,0.5,9.75));
#126875=CARTESIAN_POINT('Origin',(-10.,0.5,11.));
#126876=CARTESIAN_POINT('Origin',(-10.,0.5,11.));
#126877=CARTESIAN_POINT('',(-8.73704628614769,0.5,10.6875));
#126878=CARTESIAN_POINT('Origin',(-10.,0.5,11.));
#126879=CARTESIAN_POINT('',(-9.09789020439121,0.5,11.9375));
#126880=CARTESIAN_POINT('Origin',(-10.,1.8,11.));
#126881=CARTESIAN_POINT('',(-8.55662432702594,1.8,11.));
#126882=CARTESIAN_POINT('',(-9.27831216351297,1.8,9.75));
#126883=CARTESIAN_POINT('',(-9.27831216351297,1.8,9.75));
#126884=CARTESIAN_POINT('Origin',(-10.,1.8,11.));
#126885=CARTESIAN_POINT('Origin',(-10.,1.8,11.));
#126886=CARTESIAN_POINT('',(-10.721687836487,1.8,9.75));
#126887=CARTESIAN_POINT('Origin',(-10.,1.8,11.));
#126888=CARTESIAN_POINT('Origin',(-10.,1.8,11.));
#126889=CARTESIAN_POINT('Origin',(-10.,1.8,11.));
#126890=CARTESIAN_POINT('Origin',(-10.,1.8,11.));
#126891=CARTESIAN_POINT('Origin',(-10.,1.8,11.));
#126892=CARTESIAN_POINT('Origin',(-10.,1.8,11.));
#126893=CARTESIAN_POINT('Origin',(-10.,1.8,11.));
#126894=CARTESIAN_POINT('Origin',(-10.,1.8,11.));
#126895=CARTESIAN_POINT('',(-8.55662432702594,1.8,11.));
#126896=CARTESIAN_POINT('Origin',(-10.,1.8,11.));
#126897=CARTESIAN_POINT('Origin',(-10.,2.23363380017626,11.));
#126898=CARTESIAN_POINT('',(-10.,2.66726760035252,11.));
#126899=CARTESIAN_POINT('',(-10.721687836487,2.23363380017626,11.));
#126900=CARTESIAN_POINT('Origin',(-8.55662432702594,0.5,11.));
#126901=CARTESIAN_POINT('',(-8.55662432702594,0.5,11.));
#126902=CARTESIAN_POINT('',(-9.27831216351297,0.5,9.75));
#126903=CARTESIAN_POINT('Origin',(-9.27831216351297,0.5,12.25));
#126904=CARTESIAN_POINT('Origin',(-9.27831216351297,0.5,9.75));
#126905=CARTESIAN_POINT('',(0.,0.,0.));
#126906=CARTESIAN_POINT('Origin',(16.125,15.,5.5));
#126907=CARTESIAN_POINT('',(14.1122359168897,14.0332500271131,5.50022896121196));
#126908=CARTESIAN_POINT('',(14.0542640831103,14.0332504905991,5.50097394714278));
#126909=CARTESIAN_POINT('',(16.125,14.03325,5.5));
#126910=CARTESIAN_POINT('',(13.98325,15.4251191285151,6.36826222368048));
#126911=CARTESIAN_POINT('Ctrl Pts',(14.1122359168897,14.0332500271131,5.50022896121196));
#126912=CARTESIAN_POINT('Ctrl Pts',(14.1111983227026,14.0332537377696,5.51589658043436));
#126913=CARTESIAN_POINT('Ctrl Pts',(14.1101607285155,14.0336383013732,5.53155887807419));
#126914=CARTESIAN_POINT('Ctrl Pts',(14.1091231343284,14.0344030805415,5.54720330107296));
#126915=CARTESIAN_POINT('Ctrl Pts',(14.1064784426769,14.0363524024504,5.58707888577847));
#126916=CARTESIAN_POINT('Ctrl Pts',(14.1038337510254,14.0407811038833,5.62693592160445));
#126917=CARTESIAN_POINT('Ctrl Pts',(14.1011890593739,14.0476849049741,5.66643774297254));
#126918=CARTESIAN_POINT('Ctrl Pts',(14.0985483650438,14.0545782713088,5.7058798592786));
#126919=CARTESIAN_POINT('Ctrl Pts',(14.0959076707138,14.0639392494708,5.74496723770123));
#126920=CARTESIAN_POINT('Ctrl Pts',(14.0932669763837,14.0757117090939,5.78336675492011));
#126921=CARTESIAN_POINT('Ctrl Pts',(14.0906289292766,14.0874723671522,5.82172777768616));
#126922=CARTESIAN_POINT('Ctrl Pts',(14.0879908821695,14.1016395563674,5.85940173231856));
#126923=CARTESIAN_POINT('Ctrl Pts',(14.0853528350624,14.1181064745837,5.89606738357096));
#126924=CARTESIAN_POINT('Ctrl Pts',(14.0827160901279,14.1345652645259,5.93271493620557));
#126925=CARTESIAN_POINT('Ctrl Pts',(14.0800793451934,14.1533212931685,5.96835462533446));
#126926=CARTESIAN_POINT('Ctrl Pts',(14.0774426002589,14.1742196360123,6.00268514295958));
#126927=CARTESIAN_POINT('Ctrl Pts',(14.0748035134053,14.1951365404644,6.03704615245806));
#126928=CARTESIAN_POINT('Ctrl Pts',(14.0721644265518,14.2181992557027,6.07009515110953));
#126929=CARTESIAN_POINT('Ctrl Pts',(14.0695253396983,14.2432080435773,6.10155755933573));
#126930=CARTESIAN_POINT('Ctrl Pts',(14.0668852468224,14.2682263648249,6.13303196106091));
#126931=CARTESIAN_POINT('Ctrl Pts',(14.0642451539465,14.2951918386584,6.16291811904539));
#126932=CARTESIAN_POINT('Ctrl Pts',(14.0616050610706,14.3238654659778,6.19097587107123));
#126933=CARTESIAN_POINT('Ctrl Pts',(14.0589588945366,14.3526050583283,6.21909817127799));
#126934=CARTESIAN_POINT('Ctrl Pts',(14.0563127280027,14.3830602017073,6.24538326799888));
#126935=CARTESIAN_POINT('Ctrl Pts',(14.0536665614687,14.4149576099238,6.26963040760742));
#126936=CARTESIAN_POINT('Ctrl Pts',(14.0511732300339,14.4450127140055,6.29247710097102));
#126937=CARTESIAN_POINT('Ctrl Pts',(14.048679898599,14.4763476453378,6.31351461671014));
#126938=CARTESIAN_POINT('Ctrl Pts',(14.0461865671642,14.5087133853044,6.3326121694528));
#126939=CARTESIAN_POINT('Ctrl Pts',(14.0434435871445,14.5443197939875,6.3536218935779));
#126940=CARTESIAN_POINT('Ctrl Pts',(14.0407006071248,14.5813433744591,6.3723835458022));
#126941=CARTESIAN_POINT('Ctrl Pts',(14.0379576271051,14.6194779862857,6.38871174155561));
#126942=CARTESIAN_POINT('Ctrl Pts',(14.0352193759872,14.6575468539824,6.40501178747424));
#126943=CARTESIAN_POINT('Ctrl Pts',(14.0324811248693,14.6967224595233,6.41888647636587));
#126944=CARTESIAN_POINT('Ctrl Pts',(14.0297428737515,14.7366742891112,6.43019628707327));
#126945=CARTESIAN_POINT('Ctrl Pts',(14.0270082901897,14.7765726080571,6.4414909496576));
#126946=CARTESIAN_POINT('Ctrl Pts',(14.0242737066278,14.8172445670197,6.4502273957799));
#126947=CARTESIAN_POINT('Ctrl Pts',(14.021539123066,14.8583423608962,6.45631515505274));
#126948=CARTESIAN_POINT('Ctrl Pts',(14.0188071523524,14.8994008865283,6.46239709757493));
#126949=CARTESIAN_POINT('Ctrl Pts',(14.0160751816388,14.9408839010166,6.46583529299521));
#126950=CARTESIAN_POINT('Ctrl Pts',(14.0133432109251,14.9824337948278,6.46659039460148));
#126951=CARTESIAN_POINT('Ctrl Pts',(14.0106119531324,15.0239728459946,6.46734529916036));
#126952=CARTESIAN_POINT('Ctrl Pts',(14.0078806953396,15.065578196097,6.46541847609278));
#126953=CARTESIAN_POINT('Ctrl Pts',(14.0051494375469,15.1068898107475,6.46082263236164));
#126954=CARTESIAN_POINT('Ctrl Pts',(14.0024188047339,15.148191972273,6.45622784027387));
#126955=CARTESIAN_POINT('Ctrl Pts',(13.9996881719209,15.1891999892098,6.44896530702385));
#126956=CARTESIAN_POINT('Ctrl Pts',(13.9969575391078,15.2295595518161,6.43909955524959));
#126957=CARTESIAN_POINT('Ctrl Pts',(13.9942248485379,15.26994952868,6.42922636881807));
#126958=CARTESIAN_POINT('Ctrl Pts',(13.9914921579679,15.309689544406,6.41674617983749));
#126959=CARTESIAN_POINT('Ctrl Pts',(13.988759467398,15.3484380403758,6.40177408175168));
#126960=CARTESIAN_POINT('Ctrl Pts',(13.9869229782653,15.3744787463884,6.39171216851125));
#126961=CARTESIAN_POINT('Ctrl Pts',(13.9850864891327,15.4000719306852,6.38052584937186));
#126962=CARTESIAN_POINT('Ctrl Pts',(13.98325,15.4251191285151,6.36826222368047));
#126963=CARTESIAN_POINT('',(13.98325,14.5748808714849,6.36826222368045));
#126964=CARTESIAN_POINT('Origin',(13.98325,15.,5.5));
#126965=CARTESIAN_POINT('Ctrl Pts',(13.98325,14.5748808714849,6.36826222368047));
#126966=CARTESIAN_POINT('Ctrl Pts',(13.9859825949665,14.5376120167465,6.35001462218978));
#126967=CARTESIAN_POINT('Ctrl Pts',(13.9887151899329,14.5014867905651,6.32934731978482));
#126968=CARTESIAN_POINT('Ctrl Pts',(13.9914477848994,14.466822900776,6.30642900701992));
#126969=CARTESIAN_POINT('Ctrl Pts',(13.9941787447248,14.4321797533039,6.28352440820663));
#126970=CARTESIAN_POINT('Ctrl Pts',(13.9969097045501,14.3989966643142,6.25837177022466));
#126971=CARTESIAN_POINT('Ctrl Pts',(13.9996406643755,14.3675639083938,6.23118407568403));
#126972=CARTESIAN_POINT('Ctrl Pts',(14.002371037551,14.3361379046864,6.2040022214554));
#126973=CARTESIAN_POINT('Ctrl Pts',(14.0051014107265,14.3064619012838,6.17478653584945));
#126974=CARTESIAN_POINT('Ctrl Pts',(14.0078317839019,14.2787924412534,6.14378973252666));
#126975=CARTESIAN_POINT('Ctrl Pts',(14.0105626175321,14.2511183149989,6.11278770185105));
#126976=CARTESIAN_POINT('Ctrl Pts',(14.0132934511623,14.2254517655684,6.0800043671736));
#126977=CARTESIAN_POINT('Ctrl Pts',(14.0160242847925,14.2020100731701,6.04572670740766));
#126978=CARTESIAN_POINT('Ctrl Pts',(14.0187591076052,14.1785341373134,6.01139897507887));
#126979=CARTESIAN_POINT('Ctrl Pts',(14.0214939304178,14.1572898554751,5.9755730130028));
#126980=CARTESIAN_POINT('Ctrl Pts',(14.0242287532304,14.1384510620468,5.93856469307472));
#126981=CARTESIAN_POINT('Ctrl Pts',(14.0269655875177,14.1195984126002,5.90152915335883));
#126982=CARTESIAN_POINT('Ctrl Pts',(14.029702421805,14.1031549952832,5.86331002558253));
#126983=CARTESIAN_POINT('Ctrl Pts',(14.0324392560923,14.0892468712491,5.82424419959424));
#126984=CARTESIAN_POINT('Ctrl Pts',(14.035182303232,14.075307174561,5.78508969077501));
#126985=CARTESIAN_POINT('Ctrl Pts',(14.0379253503717,14.0639144231692,5.74508517045302));
#126986=CARTESIAN_POINT('Ctrl Pts',(14.0406683975114,14.0551446589734,5.70458237224525));
#126987=CARTESIAN_POINT('Ctrl Pts',(14.0425349293738,14.0491771916046,5.67702186762344));
#126988=CARTESIAN_POINT('Ctrl Pts',(14.0444014612362,14.0444231647546,5.64923090555547));
#126989=CARTESIAN_POINT('Ctrl Pts',(14.0462679930987,14.0408928035711,5.62132167266533));
#126990=CARTESIAN_POINT('Ctrl Pts',(14.0489333564359,14.0358515313298,5.58146794843325));
#126991=CARTESIAN_POINT('Ctrl Pts',(14.0515987197731,14.0332910885869,5.54127190906272));
#126992=CARTESIAN_POINT('Ctrl Pts',(14.0542640831103,14.0332504905991,5.50097394714278));
#126993=CARTESIAN_POINT('Origin',(16.125,15.,5.5));
#126994=CARTESIAN_POINT('',(14.5114930218304,14.0332500860612,5.50040792073653));
#126995=CARTESIAN_POINT('',(14.4551338463882,14.0332500192795,5.50019307213798));
#126996=CARTESIAN_POINT('',(16.125,14.03325,5.5));
#126997=CARTESIAN_POINT('Ctrl Pts',(14.5116785698828,14.0335723061034,5.50041943332155));
#126998=CARTESIAN_POINT('Ctrl Pts',(14.5088403565566,14.033538001356,5.54511906159122));
#126999=CARTESIAN_POINT('Ctrl Pts',(14.5060695122599,14.0365700498625,5.58972837050457));
#127000=CARTESIAN_POINT('Ctrl Pts',(14.5033211490731,14.0426309602475,5.63384343118924));
#127001=CARTESIAN_POINT('Ctrl Pts',(14.5007334695076,14.0483375182553,5.67537929574192));
#127002=CARTESIAN_POINT('Ctrl Pts',(14.4981651521549,14.0567300004624,5.71647784890844));
#127003=CARTESIAN_POINT('Ctrl Pts',(14.4955573715337,14.0677447980235,5.75679634653785));
#127004=CARTESIAN_POINT('Ctrl Pts',(14.4953774892451,14.0685045885435,5.75957747911091));
#127005=CARTESIAN_POINT('Ctrl Pts',(14.4951974191857,14.0692768613978,5.76235492004761));
#127006=CARTESIAN_POINT('Ctrl Pts',(14.4950171420486,14.0700615983275,5.76512856562658));
#127007=CARTESIAN_POINT('Ctrl Pts',(14.4925397852085,14.0808454028149,5.80324382503531));
#127008=CARTESIAN_POINT('Ctrl Pts',(14.490022367042,14.0939818279592,5.84063784347691));
#127009=CARTESIAN_POINT('Ctrl Pts',(14.4874062601009,14.1093818608135,5.87701664459744));
#127010=CARTESIAN_POINT('Ctrl Pts',(14.4874052936255,14.1093875500886,5.87703008411471));
#127011=CARTESIAN_POINT('Ctrl Pts',(14.4874043271367,14.1093932396726,5.87704352349411));
#127012=CARTESIAN_POINT('Ctrl Pts',(14.4874033606344,14.1093989295655,5.87705696273564));
#127013=CARTESIAN_POINT('Ctrl Pts',(14.4849361871077,14.1239234199081,5.91136308009952));
#127014=CARTESIAN_POINT('Ctrl Pts',(14.4823758020564,14.1405099798208,5.94487254352574));
#127015=CARTESIAN_POINT('Ctrl Pts',(14.4797777976776,14.1590269386098,5.97734260524887));
#127016=CARTESIAN_POINT('Ctrl Pts',(14.47956279882,14.1605593166989,5.98002967776994));
#127017=CARTESIAN_POINT('Ctrl Pts',(14.4793475423282,14.1621048891765,5.98270961773312));
#127018=CARTESIAN_POINT('Ctrl Pts',(14.4791320597088,14.1636635672483,5.98538228026991));
#127019=CARTESIAN_POINT('Ctrl Pts',(14.4763169539401,14.1840264329138,6.02029845006232));
#127020=CARTESIAN_POINT('Ctrl Pts',(14.4734638889733,14.2066307295246,6.05397573758949));
#127021=CARTESIAN_POINT('Ctrl Pts',(14.470628262562,14.2312768890253,6.08613865119781));
#127022=CARTESIAN_POINT('Ctrl Pts',(14.4677955122579,14.2558980505222,6.1182689427404));
#127023=CARTESIAN_POINT('Ctrl Pts',(14.4649804629347,14.2825567348882,6.14888817681659));
#127024=CARTESIAN_POINT('Ctrl Pts',(14.4622166564524,14.3110285961508,6.17774935316013));
#127025=CARTESIAN_POINT('Ctrl Pts',(14.4594543129969,14.3394853857735,6.206595251779));
#127026=CARTESIAN_POINT('Ctrl Pts',(14.4567432386662,14.3697533971121,6.23368500019935));
#127027=CARTESIAN_POINT('Ctrl Pts',(14.4540924994083,14.4015849102876,6.2587974481407));
#127028=CARTESIAN_POINT('Ctrl Pts',(14.4514398306896,14.4334395934721,6.28392817531496));
#127029=CARTESIAN_POINT('Ctrl Pts',(14.4488475087101,14.4668601036537,6.30707858920841));
#127030=CARTESIAN_POINT('Ctrl Pts',(14.4463001328731,14.5015742709219,6.32805323402867));
#127031=CARTESIAN_POINT('Ctrl Pts',(14.4437519600193,14.5362992994732,6.34903444134405));
#127032=CARTESIAN_POINT('Ctrl Pts',(14.4412485066232,14.5723188931445,6.36783820572832));
#127033=CARTESIAN_POINT('Ctrl Pts',(14.4387523046875,14.6093355894634,6.38429837617079));
#127034=CARTESIAN_POINT('Ctrl Pts',(14.4362510339094,14.6464274526973,6.40079197099611));
#127035=CARTESIAN_POINT('Ctrl Pts',(14.4337565422159,14.6845205677269,6.41493187379764));
#127036=CARTESIAN_POINT('Ctrl Pts',(14.4312145763807,14.723288942022,6.42658707969176));
#127037=CARTESIAN_POINT('Ctrl Pts',(14.4290152593111,14.7568314649641,6.43667120156187));
#127038=CARTESIAN_POINT('Ctrl Pts',(14.4267797932423,14.7908789865304,6.44489554530127));
#127039=CARTESIAN_POINT('Ctrl Pts',(14.424468769591,14.8252041506766,6.45120324226616));
#127040=CARTESIAN_POINT('Ctrl Pts',(14.4244678046359,14.8252184829579,6.45120587600994));
#127041=CARTESIAN_POINT('Ctrl Pts',(14.4244668396677,14.8252328152881,6.45120850942005));
#127042=CARTESIAN_POINT('Ctrl Pts',(14.4244658746863,14.8252471476672,6.45121114249652));
#127043=CARTESIAN_POINT('Ctrl Pts',(14.4219984901291,14.861893957556,6.45794372000282));
#127044=CARTESIAN_POINT('Ctrl Pts',(14.4194378465614,14.8990090466855,6.46251513142114));
#127045=CARTESIAN_POINT('Ctrl Pts',(14.4168395113487,14.9363172191443,6.46490193969772));
#127046=CARTESIAN_POINT('Ctrl Pts',(14.4166239691842,14.9394120793466,6.46509993486765));
#127047=CARTESIAN_POINT('Ctrl Pts',(14.4164081676501,14.9425082419749,6.46528291083921));
#127048=CARTESIAN_POINT('Ctrl Pts',(14.4161921384662,14.9456055359566,6.4654508621258));
#127049=CARTESIAN_POINT('Ctrl Pts',(14.413376132906,14.9859796970517,6.4676401577952));
#127050=CARTESIAN_POINT('Ctrl Pts',(14.4105220809119,15.0265513156988,6.46727432489245));
#127051=CARTESIAN_POINT('Ctrl Pts',(14.4076853995713,15.0669803348007,6.46436865337555));
#127052=CARTESIAN_POINT('Ctrl Pts',(14.4048515996756,15.1073682869015,6.46146593338254));
#127053=CARTESIAN_POINT('Ctrl Pts',(14.4020354334159,15.1476140253573,6.45602883499858));
#127054=CARTESIAN_POINT('Ctrl Pts',(14.3992704634175,15.1873876882495,6.44810901078328));
#127055=CARTESIAN_POINT('Ctrl Pts',(14.3965069638831,15.227140198748,6.4401933984818));
#127056=CARTESIAN_POINT('Ctrl Pts',(14.3937946868122,15.2664211557774,6.42979775620122));
#127057=CARTESIAN_POINT('Ctrl Pts',(14.3911427161659,15.3049094453059,6.41700746938872));
#127058=CARTESIAN_POINT('Ctrl Pts',(14.3884888357345,15.3434254517178,6.40420797180351));
#127059=CARTESIAN_POINT('Ctrl Pts',(14.3858952722682,15.3811475644302,6.38901026555577));
#127060=CARTESIAN_POINT('Ctrl Pts',(14.383346641176,15.417762688279,6.37153428391848));
#127061=CARTESIAN_POINT('Ctrl Pts',(14.3807972220512,15.4543891334649,6.35405289873591));
#127062=CARTESIAN_POINT('Ctrl Pts',(14.3782925079189,15.4899076987036,6.33429157452673));
#127063=CARTESIAN_POINT('Ctrl Pts',(14.3757950489659,15.524015849635,6.31240749055365));
#127064=CARTESIAN_POINT('Ctrl Pts',(14.3732925477779,15.5581928630837,6.29047922379516));
#127065=CARTESIAN_POINT('Ctrl Pts',(14.3707968286401,15.5909533370189,6.26641922298146));
#127066=CARTESIAN_POINT('Ctrl Pts',(14.3682536676265,15.6220084037581,6.24042783540193));
#127067=CARTESIAN_POINT('Ctrl Pts',(14.366060413606,15.6487906836117,6.21801253609562));
#127068=CARTESIAN_POINT('Ctrl Pts',(14.3638312674251,15.6743044740454,6.19416128864694));
#127069=CARTESIAN_POINT('Ctrl Pts',(14.3615272302636,15.6983787715834,6.16903122376138));
#127070=CARTESIAN_POINT('Ctrl Pts',(14.3615262729411,15.6983887744026,6.16902078227308));
#127071=CARTESIAN_POINT('Ctrl Pts',(14.3615253156056,15.698398776974,6.16901034056392));
#127072=CARTESIAN_POINT('Ctrl Pts',(14.3615243582573,15.6984087792974,6.16899989863392));
#127073=CARTESIAN_POINT('Ctrl Pts',(14.3590557745127,15.724200407049,6.14207471742743));
#127074=CARTESIAN_POINT('Ctrl Pts',(14.3564941307412,15.7484423252867,6.11356820325169));
#127075=CARTESIAN_POINT('Ctrl Pts',(14.3538950518424,15.7709633825522,6.08369774166327));
#127076=CARTESIAN_POINT('Ctrl Pts',(14.3536810497184,15.7728177141348,6.08123827718705));
#127077=CARTESIAN_POINT('Ctrl Pts',(14.3534667938033,15.7746603762586,6.07876959493171));
#127078=CARTESIAN_POINT('Ctrl Pts',(14.3532523151472,15.7764912722831,6.07629183189533));
#127079=CARTESIAN_POINT('Ctrl Pts',(14.3504371854622,15.8005226134114,6.04377006770674));
#127080=CARTESIAN_POINT('Ctrl Pts',(14.3475843160472,15.8225280060186,6.00967836065559));
#127081=CARTESIAN_POINT('Ctrl Pts',(14.3447490096124,15.8423332260637,5.97430917337171));
#127082=CARTESIAN_POINT('Ctrl Pts',(14.3419165707059,15.8621184158121,5.93897575722877));
#127083=CARTESIAN_POINT('Ctrl Pts',(14.3391019560053,15.8797081859031,5.90236752879608));
#127084=CARTESIAN_POINT('Ctrl Pts',(14.3363385738576,15.8949642554464,5.86478844189219));
#127085=CARTESIAN_POINT('Ctrl Pts',(14.3335766497244,15.9102122755886,5.82722918245047));
#127086=CARTESIAN_POINT('Ctrl Pts',(14.3308659836563,15.9231291137436,5.78870010211487));
#127087=CARTESIAN_POINT('Ctrl Pts',(14.3282154840765,15.9336094584268,5.74951641888195));
#127088=CARTESIAN_POINT('Ctrl Pts',(14.3255630606859,15.9440974100534,5.7103042949754));
#127089=CARTESIAN_POINT('Ctrl Pts',(14.3229708137538,15.9521451873804,5.6704366245497));
#127090=CARTESIAN_POINT('Ctrl Pts',(14.320423176276,15.9576807446635,5.63024095734538));
#127091=CARTESIAN_POINT('Ctrl Pts',(14.3178747428045,15.9632180314978,5.59003273124878));
#127092=CARTESIAN_POINT('Ctrl Pts',(14.3153706899478,15.9662412003968,5.54949633524583));
#127093=CARTESIAN_POINT('Ctrl Pts',(14.3128733974786,15.9667151448827,5.50897101865864));
#127094=CARTESIAN_POINT('Ctrl Pts',(14.3103710528751,15.9671900481795,5.46836371754517));
#127095=CARTESIAN_POINT('Ctrl Pts',(14.3078749910923,15.9651048371898,5.42776767871473));
#127096=CARTESIAN_POINT('Ctrl Pts',(14.3053308585778,15.9604680307702,5.3875345185831));
#127097=CARTESIAN_POINT('Ctrl Pts',(14.303138146851,15.9564717059903,5.35285876112074));
#127098=CARTESIAN_POINT('Ctrl Pts',(14.3009091203456,15.9505804056575,5.31845292054379));
#127099=CARTESIAN_POINT('Ctrl Pts',(14.2986048211183,15.942831329532,5.28454592146491));
#127100=CARTESIAN_POINT('Ctrl Pts',(14.2986038416525,15.9428280357083,5.28453150894942));
#127101=CARTESIAN_POINT('Ctrl Pts',(14.298602862173,15.9428247415491,5.28451709652346));
#127102=CARTESIAN_POINT('Ctrl Pts',(14.2986018826799,15.9428214470546,5.28450268418704));
#127103=CARTESIAN_POINT('Ctrl Pts',(14.2961366610282,15.9345297506763,5.24822922312637));
#127104=CARTESIAN_POINT('Ctrl Pts',(14.2935781335832,15.924073286213,5.21237753911605));
#127105=CARTESIAN_POINT('Ctrl Pts',(14.2909818963397,15.9115388193728,5.17720913033834));
#127106=CARTESIAN_POINT('Ctrl Pts',(14.2907666596865,15.9104996706205,5.17429355294933));
#127107=CARTESIAN_POINT('Ctrl Pts',(14.2905511638554,15.9094462629078,5.17138269029546));
#127108=CARTESIAN_POINT('Ctrl Pts',(14.2903354405245,15.9083786584267,5.16847670107737));
#127109=CARTESIAN_POINT('Ctrl Pts',(14.2875218445659,15.8944543061485,5.13057500779491));
#127110=CARTESIAN_POINT('Ctrl Pts',(14.2846701831178,15.87811090771,5.09349839386361));
#127111=CARTESIAN_POINT('Ctrl Pts',(14.2818359302662,15.8594963284814,5.05755251441345));
#127112=CARTESIAN_POINT('Ctrl Pts',(14.2790045544142,15.8409006445809,5.02164312298594));
#127113=CARTESIAN_POINT('Ctrl Pts',(14.2761908500345,15.8200386295198,4.98686196663159));
#127114=CARTESIAN_POINT('Ctrl Pts',(14.2734284767015,15.7970875597742,4.95349099618714));
#127115=CARTESIAN_POINT('Ctrl Pts',(14.2706675599086,15.7741485916347,4.9201376215387));
#127116=CARTESIAN_POINT('Ctrl Pts',(14.2679580014553,15.7491228171391,4.88819290788565));
#127117=CARTESIAN_POINT('Ctrl Pts',(14.2653090168416,15.7222150559174,4.85791742985194));
#127118=CARTESIAN_POINT('Ctrl Pts',(14.2626580642003,15.695287303936,4.82761945905849));
#127119=CARTESIAN_POINT('Ctrl Pts',(14.2600677008402,15.666474700163,4.79899332828456));
#127120=CARTESIAN_POINT('Ctrl Pts',(14.2575226891931,15.6360106072016,4.77227856898802));
#127121=CARTESIAN_POINT('Ctrl Pts',(14.2549768648779,15.6055367865065,4.74555527918762));
#127122=CARTESIAN_POINT('Ctrl Pts',(14.2524761691731,15.5734102739615,4.72074487036412));
#127123=CARTESIAN_POINT('Ctrl Pts',(14.2499832776,15.5398943800745,4.69806242359263));
#127124=CARTESIAN_POINT('Ctrl Pts',(14.2474852548137,15.5063094991516,4.6753332886804));
#127125=CARTESIAN_POINT('Ctrl Pts',(14.2449945709537,15.4713293200612,4.6547414257863));
#127126=CARTESIAN_POINT('Ctrl Pts',(14.242457039379,15.4352512774438,4.63647233143748));
#127127=CARTESIAN_POINT('Ctrl Pts',(14.2402402023742,15.4037327967545,4.62051209480407));
#127128=CARTESIAN_POINT('Ctrl Pts',(14.2379869886449,15.3713769033494,4.60632454098609));
#127129=CARTESIAN_POINT('Ctrl Pts',(14.235656781393,15.3384033970721,4.59400783432258));
#127130=CARTESIAN_POINT('Ctrl Pts',(14.2356558203857,15.3383897983766,4.59400275475534));
#127131=CARTESIAN_POINT('Ctrl Pts',(14.2356548593654,15.3383761995759,4.59399767550574));
#127132=CARTESIAN_POINT('Ctrl Pts',(14.2356538983319,15.3383626006697,4.59399259657377));
#127133=CARTESIAN_POINT('Ctrl Pts',(14.2331860372601,15.3034416400178,4.5809502841007));
#127134=CARTESIAN_POINT('Ctrl Pts',(14.2306246417521,15.2676820685573,4.56995633681078));
#127135=CARTESIAN_POINT('Ctrl Pts',(14.2280251500428,15.231350777683,4.56108170256948));
#127136=CARTESIAN_POINT('Ctrl Pts',(14.2278066760094,15.2282973177971,4.56033583477878));
#127137=CARTESIAN_POINT('Ctrl Pts',(14.2275879328817,15.2252398485238,4.55960492749181));
#127138=CARTESIAN_POINT('Ctrl Pts',(14.2273689535708,15.2221785440531,4.5588890172329));
#127139=CARTESIAN_POINT('Ctrl Pts',(14.2245487183885,15.1827519948523,4.54966880692146));
#127140=CARTESIAN_POINT('Ctrl Pts',(14.2216899483003,15.1426837765983,4.54293735587022));
#127141=CARTESIAN_POINT('Ctrl Pts',(14.2188481867355,15.1023123613639,4.53873890097382));
#127142=CARTESIAN_POINT('Ctrl Pts',(14.2160093354378,15.0619822907662,4.5345447457432));
#127143=CARTESIAN_POINT('Ctrl Pts',(14.2131877587133,15.0213495988083,4.53287808223543));
#127144=CARTESIAN_POINT('Ctrl Pts',(14.2104171666861,14.9807489761677,4.53374553378922));
#127145=CARTESIAN_POINT('Ctrl Pts',(14.2076480828385,14.9401704545925,4.53461251314327));
#127146=CARTESIAN_POINT('Ctrl Pts',(14.2049300097636,14.899623953611,4.53801078983452));
#127147=CARTESIAN_POINT('Ctrl Pts',(14.2022721750058,14.859441399294,4.54391225339522));
#127148=CARTESIAN_POINT('Ctrl Pts',(14.1996125229251,14.8192313697284,4.54981775214436));
#127149=CARTESIAN_POINT('Ctrl Pts',(14.1970131149593,14.7793858445733,4.55822998985528));
#127150=CARTESIAN_POINT('Ctrl Pts',(14.1944587042042,14.7402348772394,4.56908545335078));
#127151=CARTESIAN_POINT('Ctrl Pts',(14.1919035486396,14.7010724943514,4.57994408205877));
#127152=CARTESIAN_POINT('Ctrl Pts',(14.1893931603709,14.6626052316451,4.5932476505405));
#127153=CARTESIAN_POINT('Ctrl Pts',(14.1868902327606,14.6251592912233,4.60889411841261));
#127154=CARTESIAN_POINT('Ctrl Pts',(14.1843823843619,14.5876397315939,4.6245713474448));
#127155=CARTESIAN_POINT('Ctrl Pts',(14.1818815218484,14.5511458636003,4.64260116181636));
#127156=CARTESIAN_POINT('Ctrl Pts',(14.1793335983198,14.5159979928109,4.6628366008176));
#127157=CARTESIAN_POINT('Ctrl Pts',(14.1771666143414,14.4861050733328,4.68004664327771));
#127158=CARTESIAN_POINT('Ctrl Pts',(14.1749649995716,14.4571859046301,4.69885152483509));
#127159=CARTESIAN_POINT('Ctrl Pts',(14.1726914868891,14.4294289454477,4.71913157462172));
#127160=CARTESIAN_POINT('Ctrl Pts',(14.1726905696894,14.4294177475014,4.71913975617028));
#127161=CARTESIAN_POINT('Ctrl Pts',(14.1726896524781,14.4294065497437,4.7191479379589));
#127162=CARTESIAN_POINT('Ctrl Pts',(14.1726887352551,14.4293953521745,4.71915611998757));
#127163=CARTESIAN_POINT('Ctrl Pts',(14.1702276700408,14.3993503723837,4.7411098925167));
#127164=CARTESIAN_POINT('Ctrl Pts',(14.1676751843725,14.3705448742591,4.7648871771113));
#127165=CARTESIAN_POINT('Ctrl Pts',(14.1650863475534,14.3431869183278,4.79030482883998));
#127166=CARTESIAN_POINT('Ctrl Pts',(14.1648865805999,14.3410758484172,4.79226617565611));
#127167=CARTESIAN_POINT('Ctrl Pts',(14.164686597197,14.338973404483,4.79423726507427));
#127168=CARTESIAN_POINT('Ctrl Pts',(14.1644864226476,14.3368796851395,4.79621800045316));
#127169=CARTESIAN_POINT('Ctrl Pts',(14.1616962574177,14.3076960405111,4.82382679987533));
#127170=CARTESIAN_POINT('Ctrl Pts',(14.1588695674215,14.2802055500566,4.85331483920632));
#127171=CARTESIAN_POINT('Ctrl Pts',(14.156060252777,14.2546295215275,4.88442864994626));
#127172=CARTESIAN_POINT('Ctrl Pts',(14.1532536793199,14.2290784487964,4.91551210139964));
#127173=CARTESIAN_POINT('Ctrl Pts',(14.1504647355591,14.2054378478206,4.94821799952283));
#127174=CARTESIAN_POINT('Ctrl Pts',(14.1477259358544,14.183895624954,4.98227469858544));
#127175=CARTESIAN_POINT('Ctrl Pts',(14.1449884348389,14.1623636170198,5.01631524857737));
#127176=CARTESIAN_POINT('Ctrl Pts',(14.1423011064742,14.1429279597531,5.05170527324956));
#127177=CARTESIAN_POINT('Ctrl Pts',(14.1396725517865,14.1257457157262,5.08815597903113));
#127178=CARTESIAN_POINT('Ctrl Pts',(14.1370420635292,14.1085508324096,5.12463349801744));
#127179=CARTESIAN_POINT('Ctrl Pts',(14.1344703559481,14.0936128247948,5.16217325154629));
#127180=CARTESIAN_POINT('Ctrl Pts',(14.1319421762138,14.0810576269801,5.20046860430385));
#127181=CARTESIAN_POINT('Ctrl Pts',(14.1294129994541,14.0684974778359,5.23877905940494));
#127182=CARTESIAN_POINT('Ctrl Pts',(14.1269271291977,14.0583223397542,5.27784570733791));
#127183=CARTESIAN_POINT('Ctrl Pts',(14.1244478852292,14.0506233282853,5.31734438360384));
#127184=CARTESIAN_POINT('Ctrl Pts',(14.1219640356409,14.0429100145852,5.35691643541916));
#127185=CARTESIAN_POINT('Ctrl Pts',(14.1194863411734,14.0376825908161,5.39692205552027));
#127186=CARTESIAN_POINT('Ctrl Pts',(14.1169619848924,14.0349910449687,5.43701843224845));
#127187=CARTESIAN_POINT('Ctrl Pts',(14.1156350303954,14.0335762055133,5.45809551546768));
#127188=CARTESIAN_POINT('Ctrl Pts',(14.1142949564463,14.032861337069,5.47919739534369));
#127189=CARTESIAN_POINT('Ctrl Pts',(14.1129332120935,14.0328481709776,5.50027263358238));
#127190=CARTESIAN_POINT('Ctrl Pts',(14.0538074365636,14.033250458383,5.50094142621558));
#127191=CARTESIAN_POINT('Ctrl Pts',(14.0562298969709,14.0332173341493,5.46692618718686));
#127192=CARTESIAN_POINT('Ctrl Pts',(14.0586822435128,14.0349794725945,5.43293283883328));
#127193=CARTESIAN_POINT('Ctrl Pts',(14.0648394380835,14.0439380481791,5.34756452147048));
#127194=CARTESIAN_POINT('Ctrl Pts',(14.0685139854803,14.0534823431676,5.29653817716552));
#127195=CARTESIAN_POINT('Ctrl Pts',(14.073292532037,14.0717735384525,5.22921867651981));
#127196=CARTESIAN_POINT('Ctrl Pts',(14.0745054503242,14.0769541103416,5.21205339106437));
#127197=CARTESIAN_POINT('Ctrl Pts',(14.0763431736832,14.0856359270963,5.18593637599146));
#127198=CARTESIAN_POINT('Ctrl Pts',(14.0769792030934,14.0887979658629,5.17687698556369));
#127199=CARTESIAN_POINT('Ctrl Pts',(14.0781476880215,14.0948982604325,5.16020151974847));
#127200=CARTESIAN_POINT('Ctrl Pts',(14.0786813697705,14.0977990797569,5.15257278058654));
#127201=CARTESIAN_POINT('Ctrl Pts',(14.0798616675843,14.1044689192757,5.13567916947201));
#127202=CARTESIAN_POINT('Ctrl Pts',(14.0805065495745,14.1082858432902,5.12643412964555));
#127203=CARTESIAN_POINT('Ctrl Pts',(14.0823886423087,14.1199291866492,5.09942846028579));
#127204=CARTESIAN_POINT('Ctrl Pts',(14.0836120505354,14.1281479705073,5.08184175657311));
#127205=CARTESIAN_POINT('Ctrl Pts',(14.0898489125388,14.1732929774851,4.99236700713743));
#127206=CARTESIAN_POINT('Ctrl Pts',(14.0945506468488,14.2185943630929,4.92507303055884));
#127207=CARTESIAN_POINT('Ctrl Pts',(14.100891051039,14.2876979893702,4.845920389463));
#127208=CARTESIAN_POINT('Ctrl Pts',(14.1023712695334,14.304336948238,4.82825075003465));
#127209=CARTESIAN_POINT('Ctrl Pts',(14.1048548421149,14.3326635447107,4.80035165159155));
#127210=CARTESIAN_POINT('Ctrl Pts',(14.1058369951912,14.343964587907,4.78974425133705));
#127211=CARTESIAN_POINT('Ctrl Pts',(14.1072458427187,14.3602143297748,4.77521064450908));
#127212=CARTESIAN_POINT('Ctrl Pts',(14.1076564355509,14.3649546192145,4.77105372452122));
#127213=CARTESIAN_POINT('Ctrl Pts',(14.108379896014,14.373306426234,4.76387303393529));
#127214=CARTESIAN_POINT('Ctrl Pts',(14.1086912360883,14.3768999623784,4.7608287852438));
#127215=CARTESIAN_POINT('Ctrl Pts',(14.109386972226,14.384930810515,4.75412565978937));
#127216=CARTESIAN_POINT('Ctrl Pts',(14.109772260729,14.3893787892095,4.75047990547109));
#127217=CARTESIAN_POINT('Ctrl Pts',(14.110887089195,14.4022581175886,4.740114186977));
#127218=CARTESIAN_POINT('Ctrl Pts',(14.1116228582927,14.4107694325652,4.73349551720651));
#127219=CARTESIAN_POINT('Ctrl Pts',(14.1154811581633,14.4555444676834,4.69986347141738));
#127220=CARTESIAN_POINT('Ctrl Pts',(14.118712859258,14.4935576325376,4.6752783834827));
#127221=CARTESIAN_POINT('Ctrl Pts',(14.1254702415451,14.5761740704372,4.62971762131015));
#127222=CARTESIAN_POINT('Ctrl Pts',(14.1289861315741,14.6209502950831,4.60930256375851));
#127223=CARTESIAN_POINT('Ctrl Pts',(14.1344617560915,14.6946508693338,4.58226941888499));
#127224=CARTESIAN_POINT('Ctrl Pts',(14.1364765865886,14.7226624763879,4.57341934839747));
#127225=CARTESIAN_POINT('Ctrl Pts',(14.1392511245881,14.7625124044787,4.56279870544198));
#127226=CARTESIAN_POINT('Ctrl Pts',(14.140043589744,14.7740445547766,4.55995171285887));
#127227=CARTESIAN_POINT('Ctrl Pts',(14.1414148525698,14.7942535674138,4.55535602478808));
#127228=CARTESIAN_POINT('Ctrl Pts',(14.141996514414,14.8029072034539,4.55351266648904));
#127229=CARTESIAN_POINT('Ctrl Pts',(14.1432016613457,14.8209996978987,4.54991758918165));
#127230=CARTESIAN_POINT('Ctrl Pts',(14.1438244356717,14.8304418250294,4.54818713429662));
#127231=CARTESIAN_POINT('Ctrl Pts',(14.1454695678927,14.8556156080642,4.54396005235854));
#127232=CARTESIAN_POINT('Ctrl Pts',(14.1464844010567,14.8713861882827,4.54171102193587));
#127233=CARTESIAN_POINT('Ctrl Pts',(14.1508445664755,14.9400366908152,4.53364624476629));
#127234=CARTESIAN_POINT('Ctrl Pts',(14.1540735081881,14.9932916363082,4.53181049264748));
#127235=CARTESIAN_POINT('Ctrl Pts',(14.1598362811027,15.0884752531637,4.53638728429054));
#127236=CARTESIAN_POINT('Ctrl Pts',(14.1623702637541,15.130339926785,4.54115253636299));
#127237=CARTESIAN_POINT('Ctrl Pts',(14.1663312027684,15.1931919320012,4.55249970137794));
#127238=CARTESIAN_POINT('Ctrl Pts',(14.1677015580241,15.2144870976862,4.55709222244319));
#127239=CARTESIAN_POINT('Ctrl Pts',(14.1695863090062,15.2428444032365,4.5642180588735));
#127240=CARTESIAN_POINT('Ctrl Pts',(14.1700711776451,15.2500599526167,4.5661203195351));
#127241=CARTESIAN_POINT('Ctrl Pts',(14.1708942699946,15.2621593251666,4.56946039176176));
#127242=CARTESIAN_POINT('Ctrl Pts',(14.1712301225547,15.2670552952967,4.57085364870826));
#127243=CARTESIAN_POINT('Ctrl Pts',(14.1719411960869,15.2773292754341,4.57386524977325));
#127244=CARTESIAN_POINT('Ctrl Pts',(14.1723168407206,15.2827045380052,4.57549189133028));
#127245=CARTESIAN_POINT('Ctrl Pts',(14.1733863088937,15.2978695982969,4.58022570243608));
#127246=CARTESIAN_POINT('Ctrl Pts',(14.1740856867667,15.3076241825002,4.58344209223064));
#127247=CARTESIAN_POINT('Ctrl Pts',(14.1786600515643,15.3704941391684,4.60528890325809));
#127248=CARTESIAN_POINT('Ctrl Pts',(14.1827078615811,15.421943866773,4.62837146042055));
#127249=CARTESIAN_POINT('Ctrl Pts',(14.1911444005081,15.5249886555182,4.68587331240808));
#127250=CARTESIAN_POINT('Ctrl Pts',(14.195505187317,15.5758914854332,4.72104774407341));
#127251=CARTESIAN_POINT('Ctrl Pts',(14.2006519395827,15.6339492893575,4.7699895313703));
#127252=CARTESIAN_POINT('Ctrl Pts',(14.2016046648137,15.6445981934798,4.77937513898573));
#127253=CARTESIAN_POINT('Ctrl Pts',(14.2031586635232,15.6617952939285,4.79521847992429));
#127254=CARTESIAN_POINT('Ctrl Pts',(14.2037653420745,15.6684645990472,4.80154091628627));
#127255=CARTESIAN_POINT('Ctrl Pts',(14.2049450575848,15.6813407454673,4.8141007718935));
#127256=CARTESIAN_POINT('Ctrl Pts',(14.2055183698493,15.6875545619149,4.82032971576615));
#127257=CARTESIAN_POINT('Ctrl Pts',(14.2069026431817,15.7024437741181,4.83566836223354));
#127258=CARTESIAN_POINT('Ctrl Pts',(14.2077097247531,15.7110282107699,4.84486437490422));
#127259=CARTESIAN_POINT('Ctrl Pts',(14.2106425099764,15.7418240337471,4.87917275436612));
#127260=CARTESIAN_POINT('Ctrl Pts',(14.2127233586005,15.7629056182872,4.90526920859455));
#127261=CARTESIAN_POINT('Ctrl Pts',(14.2150217214187,15.7849707871205,4.93569257943748));
#127262=CARTESIAN_POINT('Ctrl Pts',(14.2152692219312,15.787330577067,4.93898969316743));
#127263=CARTESIAN_POINT('Ctrl Pts',(14.2188786518254,15.8214967901948,4.98736712741556));
#127264=CARTESIAN_POINT('Ctrl Pts',(14.2221530407581,15.8494069651619,5.03507306952823));
#127265=CARTESIAN_POINT('Ctrl Pts',(14.2275518021116,15.8874656116362,5.11512289154344));
#127266=CARTESIAN_POINT('Ctrl Pts',(14.2296198384497,15.9002550104573,5.14607054801264));
#127267=CARTESIAN_POINT('Ctrl Pts',(14.2323007783964,15.9141898787153,5.18546579218286));
#127268=CARTESIAN_POINT('Ctrl Pts',(14.232839792009,15.9168650652493,5.1933514336952));
#127269=CARTESIAN_POINT('Ctrl Pts',(14.2337230818305,15.9210382703056,5.20619583261487));
#127270=CARTESIAN_POINT('Ctrl Pts',(14.2340639359194,15.9225989396651,5.21113397979167));
#127271=CARTESIAN_POINT('Ctrl Pts',(14.2347501019306,15.925639860556,5.22103190062307));
#127272=CARTESIAN_POINT('Ctrl Pts',(14.2350954089997,15.9271200976424,5.22599147306835));
#127273=CARTESIAN_POINT('Ctrl Pts',(14.2360079109081,15.9309029679066,5.2390477339749));
#127274=CARTESIAN_POINT('Ctrl Pts',(14.2365785600612,15.9331397498161,5.24716286591365));
#127275=CARTESIAN_POINT('Ctrl Pts',(14.2394144071364,15.9436398845298,5.28729648574071));
#127276=CARTESIAN_POINT('Ctrl Pts',(14.2417455464504,15.9503619509647,5.31969259336735));
#127277=CARTESIAN_POINT('Ctrl Pts',(14.2484337760382,15.9646979021073,5.41246738656664));
#127278=CARTESIAN_POINT('Ctrl Pts',(14.2528257146872,15.9682938845111,5.47331688320412));
#127279=CARTESIAN_POINT('Ctrl Pts',(14.2593574026124,15.9650055546371,5.56647811701911));
#127280=CARTESIAN_POINT('Ctrl Pts',(14.261588860755,15.9622360533886,5.59877870816187));
#127281=CARTESIAN_POINT('Ctrl Pts',(14.2645866769297,15.9562115238328,5.64286859119123));
#127282=CARTESIAN_POINT('Ctrl Pts',(14.2653947411797,15.9543488134276,5.65482337484774));
#127283=CARTESIAN_POINT('Ctrl Pts',(14.2667737312296,15.9507568693147,5.67533711894123));
#127284=CARTESIAN_POINT('Ctrl Pts',(14.2673479363237,15.9491352300182,5.68391316794778));
#127285=CARTESIAN_POINT('Ctrl Pts',(14.2685199265679,15.9455662090536,5.70148134278337));
#127286=CARTESIAN_POINT('Ctrl Pts',(14.2691172484402,15.9436061537407,5.71047000585123));
#127287=CARTESIAN_POINT('Ctrl Pts',(14.2706524219015,15.9382040773192,5.73364897897117));
#127288=CARTESIAN_POINT('Ctrl Pts',(14.271584093476,15.9345682870344,5.74779202658948));
#127289=CARTESIAN_POINT('Ctrl Pts',(14.2773436026378,15.9098805000807,5.83553297934397));
#127290=CARTESIAN_POINT('Ctrl Pts',(14.2818839662849,15.8804705215952,5.90649425481911));
#127291=CARTESIAN_POINT('Ctrl Pts',(14.2883263767746,15.8282079114558,5.99958963713148));
#127292=CARTESIAN_POINT('Ctrl Pts',(14.2901616680309,15.8121941481268,6.02522241750458));
#127293=CARTESIAN_POINT('Ctrl Pts',(14.2931641365855,15.7847834849569,6.06483923095255));
#127294=CARTESIAN_POINT('Ctrl Pts',(14.2943002889114,15.7741497210443,6.07932770744158));
#127295=CARTESIAN_POINT('Ctrl Pts',(14.2959033858421,15.7589086727182,6.09892422491411));
#127296=CARTESIAN_POINT('Ctrl Pts',(14.2963497249731,15.7546407704728,6.10429289395318));
#127297=CARTESIAN_POINT('Ctrl Pts',(14.2971210819535,15.7472319858605,6.11341164415223));
#127298=CARTESIAN_POINT('Ctrl Pts',(14.2974441824521,15.7441191560303,6.11718406180125));
#127299=CARTESIAN_POINT('Ctrl Pts',(14.2981480058826,15.7373200442749,6.12529764501526));
#127300=CARTESIAN_POINT('Ctrl Pts',(14.2985293648129,15.7336239914721,6.12962991330551));
#127301=CARTESIAN_POINT('Ctrl Pts',(14.2996216634735,15.7229976900521,6.14186476824886));
#127302=CARTESIAN_POINT('Ctrl Pts',(14.3003384686996,15.7159767534749,6.14968708430807));
#127303=CARTESIAN_POINT('Ctrl Pts',(14.3044085354346,15.6757742429175,6.19303519951512));
#127304=CARTESIAN_POINT('Ctrl Pts',(14.3078899126151,15.640079903932,6.22613054288866));
#127305=CARTESIAN_POINT('Ctrl Pts',(14.3147129407198,15.5655382584345,6.28546161181057));
#127306=CARTESIAN_POINT('Ctrl Pts',(14.3180456350148,15.5269651067212,6.31184477239251));
#127307=CARTESIAN_POINT('Ctrl Pts',(14.3232772103154,15.4620851176591,6.34964115626188));
#127308=CARTESIAN_POINT('Ctrl Pts',(14.3252253721968,15.4369156463575,6.3628544131446));
#127309=CARTESIAN_POINT('Ctrl Pts',(14.3279202225422,15.4006491977218,6.3798986582361));
#127310=CARTESIAN_POINT('Ctrl Pts',(14.3286977110921,15.3900108241399,6.38466547652845));
#127311=CARTESIAN_POINT('Ctrl Pts',(14.3300457407502,15.3712655780084,6.39266091520018));
#127312=CARTESIAN_POINT('Ctrl Pts',(14.3306190435817,15.363196562391,6.39597427657361));
#127313=CARTESIAN_POINT('Ctrl Pts',(14.3318087705913,15.346254832935,6.4026645309419));
#127314=CARTESIAN_POINT('Ctrl Pts',(14.3324244689336,15.3373749684169,6.40602086387693));
#127315=CARTESIAN_POINT('Ctrl Pts',(14.3340532461462,15.3135977422034,6.4146099094455));
#127316=CARTESIAN_POINT('Ctrl Pts',(14.3350587781171,15.2986188613529,6.41960950940615));
#127317=CARTESIAN_POINT('Ctrl Pts',(14.3401981095314,15.2206754135691,6.44351974746627));
#127318=CARTESIAN_POINT('Ctrl Pts',(14.3441366015729,15.1560237701942,6.45633922979636));
#127319=CARTESIAN_POINT('Ctrl Pts',(14.3510961220375,15.0410709992831,6.46715574788448));
#127320=CARTESIAN_POINT('Ctrl Pts',(14.35410137129,14.9912954059873,6.46798768348413));
#127321=CARTESIAN_POINT('Ctrl Pts',(14.3579027833784,14.9317812315508,6.46439108698719));
#127322=CARTESIAN_POINT('Ctrl Pts',(14.3585416376089,14.9218895376033,6.46364034094103));
#127323=CARTESIAN_POINT('Ctrl Pts',(14.3595482136472,14.9065113741516,6.46223486976764));
#127324=CARTESIAN_POINT('Ctrl Pts',(14.3599106000204,14.9010157121724,6.46168507055188));
#127325=CARTESIAN_POINT('Ctrl Pts',(14.3606016758154,14.8906198245719,6.4605549890717));
#127326=CARTESIAN_POINT('Ctrl Pts',(14.3609298642706,14.8857188557905,6.45998423188809));
#127327=CARTESIAN_POINT('Ctrl Pts',(14.3617487697514,14.8735745741501,6.45847562269793));
#127328=CARTESIAN_POINT('Ctrl Pts',(14.3622417891364,14.866337211546,6.45749316379624));
#127329=CARTESIAN_POINT('Ctrl Pts',(14.3640750732588,14.8396716374609,6.45356515508447));
#127330=CARTESIAN_POINT('Ctrl Pts',(14.3654381198333,14.8203245545211,6.45010962946027));
#127331=CARTESIAN_POINT('Ctrl Pts',(14.371967727122,14.7293121834208,6.43097508460043));
#127332=CARTESIAN_POINT('Ctrl Pts',(14.3773037500281,14.6594765869179,6.40776175072064));
#127333=CARTESIAN_POINT('Ctrl Pts',(14.384909787144,14.5612826379397,6.36217770800166));
#127334=CARTESIAN_POINT('Ctrl Pts',(14.3873192278779,14.5304465306348,6.34577972707653));
#127335=CARTESIAN_POINT('Ctrl Pts',(14.3905103992866,14.4899251778128,6.32133036014429));
#127336=CARTESIAN_POINT('Ctrl Pts',(14.3913408313173,14.4794129864875,6.31470796619853));
#127337=CARTESIAN_POINT('Ctrl Pts',(14.3927489294437,14.4616531781826,6.30303561884774));
#127338=CARTESIAN_POINT('Ctrl Pts',(14.3933301394323,14.4543419954351,6.29808574499851));
#127339=CARTESIAN_POINT('Ctrl Pts',(14.3945090759668,14.4395576050809,6.28777814870805));
#127340=CARTESIAN_POINT('Ctrl Pts',(14.3951064302479,14.4320909619195,6.28241256606969));
#127341=CARTESIAN_POINT('Ctrl Pts',(14.396626734096,14.4131618440449,6.26839620454434));
#127342=CARTESIAN_POINT('Ctrl Pts',(14.3975438698829,14.4018132770824,6.25959490953729));
#127343=CARTESIAN_POINT('Ctrl Pts',(14.4033927086036,14.3300346616598,6.20132080991892));
#127344=CARTESIAN_POINT('Ctrl Pts',(14.4080240120743,14.275593022949,6.14493406245014));
#127345=CARTESIAN_POINT('Ctrl Pts',(14.4145133974075,14.2108923797592,6.0592591840226));
#127346=CARTESIAN_POINT('Ctrl Pts',(14.4162947064593,14.1943295068235,6.03512289845086));
#127347=CARTESIAN_POINT('Ctrl Pts',(14.4192203826514,14.1695835970152,5.99530281122447));
#127348=CARTESIAN_POINT('Ctrl Pts',(14.4203360031198,14.1606914331173,5.98008053510531));
#127349=CARTESIAN_POINT('Ctrl Pts',(14.4219165073331,14.1489337304065,5.9586268082552));
#127350=CARTESIAN_POINT('Ctrl Pts',(14.4223618035421,14.1457103794684,5.95259427997009));
#127351=CARTESIAN_POINT('Ctrl Pts',(14.423133118597,14.1402855927444,5.94217730081682));
#127352=CARTESIAN_POINT('Ctrl Pts',(14.4234572622124,14.1380530602517,5.9378094326138));
#127353=CARTESIAN_POINT('Ctrl Pts',(14.4241647359729,14.1332838695781,5.928300793185));
#127354=CARTESIAN_POINT('Ctrl Pts',(14.4245487248028,14.1307596602008,5.92315440185414));
#127355=CARTESIAN_POINT('Ctrl Pts',(14.4256571491854,14.1236521900996,5.90833162511792));
#127356=CARTESIAN_POINT('Ctrl Pts',(14.4263877194663,14.1191838667779,5.89860145106974));
#127357=CARTESIAN_POINT('Ctrl Pts',(14.4301212655879,14.0973870322842,5.84897986492439));
#127358=CARTESIAN_POINT('Ctrl Pts',(14.4332254534356,14.0826042506681,5.80802844442641));
#127359=CARTESIAN_POINT('Ctrl Pts',(14.4391598882848,14.0597802042454,5.72835150250859));
#127360=CARTESIAN_POINT('Ctrl Pts',(14.4419832177582,14.0512557819224,5.68984829087294));
#127361=CARTESIAN_POINT('Ctrl Pts',(14.4474218957436,14.0392090698258,5.61363227443366));
#127362=CARTESIAN_POINT('Ctrl Pts',(14.4500365217652,14.0355034701813,5.5760167974511));
#127363=CARTESIAN_POINT('Ctrl Pts',(14.4534425855343,14.0335053004661,5.52558891189949));
#127364=CARTESIAN_POINT('Ctrl Pts',(14.4542920249362,14.0332525553951,5.51289190225747));
#127365=CARTESIAN_POINT('Ctrl Pts',(14.4551338463912,14.0332500192795,5.50019307209264));
#127366=CARTESIAN_POINT('Origin',(16.125,15.,5.5));
#127367=CARTESIAN_POINT('',(14.9122050450034,14.0332503695598,5.49915468993569));
#127368=CARTESIAN_POINT('',(14.8539665893558,14.0332503192036,5.49922960238524));
#127369=CARTESIAN_POINT('',(16.125,14.03325,5.5));
#127370=CARTESIAN_POINT('Ctrl Pts',(14.9122050445523,14.0332503695571,5.49915469624611));
#127371=CARTESIAN_POINT('Ctrl Pts',(14.9082502315315,14.0332019940531,5.55448037106382));
#127372=CARTESIAN_POINT('Ctrl Pts',(14.9043425918772,14.0379029547454,5.60971498880857));
#127373=CARTESIAN_POINT('Ctrl Pts',(14.899465079513,14.050066977222,5.68026935697303));
#127374=CARTESIAN_POINT('Ctrl Pts',(14.8983696073238,14.0532324042794,5.69621661959429));
#127375=CARTESIAN_POINT('Ctrl Pts',(14.8966351867929,14.0589431604573,5.72161487145916));
#127376=CARTESIAN_POINT('Ctrl Pts',(14.8959884324965,14.0612322696413,5.73111963710856));
#127377=CARTESIAN_POINT('Ctrl Pts',(14.8947549069735,14.0659050797534,5.74930553296568));
#127378=CARTESIAN_POINT('Ctrl Pts',(14.8941675098451,14.0682666184343,5.75799124682317));
#127379=CARTESIAN_POINT('Ctrl Pts',(14.8928007927342,14.0740800376407,5.77825101499658));
#127380=CARTESIAN_POINT('Ctrl Pts',(14.8920246108413,14.077628225723,5.7897960224413));
#127381=CARTESIAN_POINT('Ctrl Pts',(14.8893424690424,14.0907416551355,5.82978017153723));
#127382=CARTESIAN_POINT('Ctrl Pts',(14.887471616334,14.1014139303266,5.85783938413386));
#127383=CARTESIAN_POINT('Ctrl Pts',(14.8824737577382,14.1338351668622,5.93243344243876));
#127384=CARTESIAN_POINT('Ctrl Pts',(14.8794103816961,14.158011932621,5.97780380570704));
#127385=CARTESIAN_POINT('Ctrl Pts',(14.8738290093159,14.2078040631002,6.05562276626686));
#127386=CARTESIAN_POINT('Ctrl Pts',(14.8713285836058,14.2321092845856,6.08875650907772));
#127387=CARTESIAN_POINT('Ctrl Pts',(14.8680391683436,14.2653117869397,6.12845317398805));
#127388=CARTESIAN_POINT('Ctrl Pts',(14.8673515195187,14.2723155091575,6.13654962252689));
#127389=CARTESIAN_POINT('Ctrl Pts',(14.8662747045411,14.2833481443383,6.14888352908781));
#127390=CARTESIAN_POINT('Ctrl Pts',(14.8658917949038,14.2872837060635,6.15320379413745));
#127391=CARTESIAN_POINT('Ctrl Pts',(14.8651692104273,14.2947274045547,6.16122776019404));
#127392=CARTESIAN_POINT('Ctrl Pts',(14.8648301958532,14.29822606158,6.16493978621154));
#127393=CARTESIAN_POINT('Ctrl Pts',(14.8640013338561,14.3067975837921,6.17389105620963));
#127394=CARTESIAN_POINT('Ctrl Pts',(14.8635093366963,14.311900593296,6.17910083501389));
#127395=CARTESIAN_POINT('Ctrl Pts',(14.8616506922213,14.3312521590897,6.19841523774386));
#127396=CARTESIAN_POINT('Ctrl Pts',(14.8602601107601,14.3458785675009,6.21213239542386));
#127397=CARTESIAN_POINT('Ctrl Pts',(14.8563343075277,14.3878317057881,6.24909410500529));
#127398=CARTESIAN_POINT('Ctrl Pts',(14.8537656270426,14.4160413212151,6.27128726434364));
#127399=CARTESIAN_POINT('Ctrl Pts',(14.8465672445191,14.4984028839494,6.32896949270947));
#127400=CARTESIAN_POINT('Ctrl Pts',(14.8419697127358,14.55498719631,6.36067191768671));
#127401=CARTESIAN_POINT('Ctrl Pts',(14.8364694708892,14.6290544025969,6.39289588266202));
#127402=CARTESIAN_POINT('Ctrl Pts',(14.8353870985073,14.6439451282188,6.39893752468016));
#127403=CARTESIAN_POINT('Ctrl Pts',(14.8336681639751,14.6680922729971,6.40804055571155));
#127404=CARTESIAN_POINT('Ctrl Pts',(14.8330240428701,14.6772558909764,6.41133783073744));
#127405=CARTESIAN_POINT('Ctrl Pts',(14.8317923816868,14.6949940721784,6.41741930660174));
#127406=CARTESIAN_POINT('Ctrl Pts',(14.831204261519,14.7035607805634,6.42022312419855));
#127407=CARTESIAN_POINT('Ctrl Pts',(14.8298310914207,14.7237813525899,6.42652947532849));
#127408=CARTESIAN_POINT('Ctrl Pts',(14.8290492726973,14.73546475944,6.42993265204433));
#127409=CARTESIAN_POINT('Ctrl Pts',(14.8263170151823,14.7768525511048,6.44114502876785));
#127410=CARTESIAN_POINT('Ctrl Pts',(14.8244035820216,14.8068629438175,6.44775898429116));
#127411=CARTESIAN_POINT('Ctrl Pts',(14.8192180719922,14.8901229161273,6.46198846762755));
#127412=CARTESIAN_POINT('Ctrl Pts',(14.8160166896129,14.9437686689442,6.46660899051327));
#127413=CARTESIAN_POINT('Ctrl Pts',(14.8102680296816,15.0387520554816,6.46685254576769));
#127414=CARTESIAN_POINT('Ctrl Pts',(14.8077459676647,15.0799431242302,6.46432043434005));
#127415=CARTESIAN_POINT('Ctrl Pts',(14.804539681343,15.1296271005955,6.45806095118941));
#127416=CARTESIAN_POINT('Ctrl Pts',(14.8039674307318,15.1383965417581,6.45683350454771));
#127417=CARTESIAN_POINT('Ctrl Pts',(14.8030364083054,15.1524803602225,6.45466455680153));
#127418=CARTESIAN_POINT('Ctrl Pts',(14.8026815762018,15.1578060834347,6.45379867523597));
#127419=CARTESIAN_POINT('Ctrl Pts',(14.8019701441423,15.1683936638962,6.45198619648021));
#127420=CARTESIAN_POINT('Ctrl Pts',(14.8016135968478,15.1736554617176,6.45104044143365));
#127421=CARTESIAN_POINT('Ctrl Pts',(14.8006762223517,15.1873807585009,6.44845576079329));
#127422=CARTESIAN_POINT('Ctrl Pts',(14.8000918421118,15.195830475384,6.44674721614167));
#127423=CARTESIAN_POINT('Ctrl Pts',(14.7970262403958,15.2396615804815,6.43727265424319));
#127424=CARTESIAN_POINT('Ctrl Pts',(14.7944665863109,15.2746059060149,6.42763613005524));
#127425=CARTESIAN_POINT('Ctrl Pts',(14.7858956768326,15.3884708324279,6.38923752049845));
#127426=CARTESIAN_POINT('Ctrl Pts',(14.7798545262504,15.464203214228,6.35215809855692));
#127427=CARTESIAN_POINT('Ctrl Pts',(14.7731435505965,15.5465954303663,6.29753387804318));
#127428=CARTESIAN_POINT('Ctrl Pts',(14.7721437969525,15.5588030513961,6.28902854314845));
#127429=CARTESIAN_POINT('Ctrl Pts',(14.7705225650791,15.5784783068559,6.27463454822229));
#127430=CARTESIAN_POINT('Ctrl Pts',(14.769895019805,15.5860636137766,6.2689117544654));
#127431=CARTESIAN_POINT('Ctrl Pts',(14.7686731848782,15.6007656562799,6.25747570490312));
#127432=CARTESIAN_POINT('Ctrl Pts',(14.7680786266893,15.6078882784428,6.25177168576603));
#127433=CARTESIAN_POINT('Ctrl Pts',(14.76665494423,15.6248578655109,6.23778301235662));
#127434=CARTESIAN_POINT('Ctrl Pts',(14.7658297805056,15.6346224062644,6.22940081676402));
#127435=CARTESIAN_POINT('Ctrl Pts',(14.7626615950873,15.6717823853933,6.19619016999649));
#127436=CARTESIAN_POINT('Ctrl Pts',(14.7603745784783,15.6979135602774,6.16999209656738));
#127437=CARTESIAN_POINT('Ctrl Pts',(14.7556529509188,15.7493805434745,6.11210553044752));
#127438=CARTESIAN_POINT('Ctrl Pts',(14.753229851437,15.7743523385292,6.08019212950624));
#127439=CARTESIAN_POINT('Ctrl Pts',(14.7481999229132,15.8214839937927,6.01147367533789));
#127440=CARTESIAN_POINT('Ctrl Pts',(14.7455958591552,15.8433397127383,5.97457206542411));
#127441=CARTESIAN_POINT('Ctrl Pts',(14.7421881672977,15.8675450821781,5.92671718709921));
#127442=CARTESIAN_POINT('Ctrl Pts',(14.7414951109509,15.8722542247513,5.91700668115971));
#127443=CARTESIAN_POINT('Ctrl Pts',(14.7404116117773,15.8792690490483,5.90190281299664));
#127444=CARTESIAN_POINT('Ctrl Pts',(14.7400275474056,15.8816900022901,5.89656357284522));
#127445=CARTESIAN_POINT('Ctrl Pts',(14.7393041424174,15.8861244866421,5.88654227507385));
#127446=CARTESIAN_POINT('Ctrl Pts',(14.738965483854,15.8881497844291,5.88186580352009));
#127447=CARTESIAN_POINT('Ctrl Pts',(14.7381394003303,15.8929693640861,5.87049149197632));
#127448=CARTESIAN_POINT('Ctrl Pts',(14.7376498625717,15.8957253323618,5.86377788833509));
#127449=CARTESIAN_POINT('Ctrl Pts',(14.7358132560148,15.9057047352811,5.83866670748072));
#127450=CARTESIAN_POINT('Ctrl Pts',(14.7344429502974,15.9124385988233,5.82008107117521));
#127451=CARTESIAN_POINT('Ctrl Pts',(14.7305995272493,15.929506637127,5.76804499072815));
#127452=CARTESIAN_POINT('Ctrl Pts',(14.7280943600802,15.9386008413785,5.73421988092676));
#127453=CARTESIAN_POINT('Ctrl Pts',(14.7208563744918,15.9595146758142,5.63530316622377));
#127454=CARTESIAN_POINT('Ctrl Pts',(14.7161542580187,15.9665213324667,5.56938649679398));
#127455=CARTESIAN_POINT('Ctrl Pts',(14.7105657765703,15.9667983767351,5.4872971117587));
#127456=CARTESIAN_POINT('Ctrl Pts',(14.7094904065259,15.9664567536837,5.47133192676454));
#127457=CARTESIAN_POINT('Ctrl Pts',(14.7077797185688,15.9652712938315,5.44567379571244));
#127458=CARTESIAN_POINT('Ctrl Pts',(14.7071369735811,15.9646763973644,5.43597291943918));
#127459=CARTESIAN_POINT('Ctrl Pts',(14.7059061951079,15.9632474002824,5.41728728704957));
#127460=CARTESIAN_POINT('Ctrl Pts',(14.7053176066802,15.962433603545,5.40830204570714));
#127461=CARTESIAN_POINT('Ctrl Pts',(14.703940672026,15.9602216474156,5.38717591945265));
#127462=CARTESIAN_POINT('Ctrl Pts',(14.7031556100191,15.9587188079405,5.37504739345968));
#127463=CARTESIAN_POINT('Ctrl Pts',(14.7003942497529,15.952574188684,5.33214097749989));
#127464=CARTESIAN_POINT('Ctrl Pts',(14.698456081271,15.9466765411517,5.30156099766003));
#127465=CARTESIAN_POINT('Ctrl Pts',(14.6937404033701,15.9284967959997,5.22688803593776));
#127466=CARTESIAN_POINT('Ctrl Pts',(14.6910033671348,15.9145418097206,5.18328261107043));
#127467=CARTESIAN_POINT('Ctrl Pts',(14.6853251765019,15.8795652913527,5.09587817113486));
#127468=CARTESIAN_POINT('Ctrl Pts',(14.6823887788008,15.8582288404779,5.05234870484421));
#127469=CARTESIAN_POINT('Ctrl Pts',(14.6787150291129,15.8291643817197,5.00283485030576));
#127470=CARTESIAN_POINT('Ctrl Pts',(14.6781329998098,15.8244946211923,4.99512836903688));
#127471=CARTESIAN_POINT('Ctrl Pts',(14.677189944024,15.8168399441178,4.98288536912214));
#127472=CARTESIAN_POINT('Ctrl Pts',(14.6768330415415,15.8139232201728,4.97830658048361));
#127473=CARTESIAN_POINT('Ctrl Pts',(14.6761215872298,15.8080742197859,4.96929303593452));
#127474=CARTESIAN_POINT('Ctrl Pts',(14.6757671397886,15.8051436320107,4.96485744499979));
#127475=CARTESIAN_POINT('Ctrl Pts',(14.674841602851,15.797444688353,4.95341110597143));
#127476=CARTESIAN_POINT('Ctrl Pts',(14.6742671143401,15.7926205064848,4.94643864762816));
#127477=CARTESIAN_POINT('Ctrl Pts',(14.6713956144491,15.7682556047653,4.9121952545743));
#127478=CARTESIAN_POINT('Ctrl Pts',(14.6690311693775,15.7473977718306,4.88589314109405));
#127479=CARTESIAN_POINT('Ctrl Pts',(14.6630790220272,15.6921283389582,4.82319284441154));
#127480=CARTESIAN_POINT('Ctrl Pts',(14.6594734827413,15.6561727673762,4.78827869070979));
#127481=CARTESIAN_POINT('Ctrl Pts',(14.6531348239278,15.5871663563082,4.73096545598608));
#127482=CARTESIAN_POINT('Ctrl Pts',(14.650380596341,15.5551238753468,4.70752500037806));
#127483=CARTESIAN_POINT('Ctrl Pts',(14.6467841020732,15.5103514241787,4.67882425787979));
#127484=CARTESIAN_POINT('Ctrl Pts',(14.6458786938504,15.4988226797119,4.67177047825377));
#127485=CARTESIAN_POINT('Ctrl Pts',(14.64443000349,15.4799660419588,4.66076980395346));
#127486=CARTESIAN_POINT('Ctrl Pts',(14.6438814412111,15.4727288015102,4.65667194354024));
#127487=CARTESIAN_POINT('Ctrl Pts',(14.6427347177708,15.4573998471345,4.6482517515532));
#127488=CARTESIAN_POINT('Ctrl Pts',(14.6421373227796,15.4492976435309,4.643950155745));
#127489=CARTESIAN_POINT('Ctrl Pts',(14.6406931155981,15.4294358553151,4.63376488305315));
#127490=CARTESIAN_POINT('Ctrl Pts',(14.6398505661163,15.4176149092576,4.62800444645703));
#127491=CARTESIAN_POINT('Ctrl Pts',(14.6364709951382,15.3693157286907,4.6056754448396));
#127492=CARTESIAN_POINT('Ctrl Pts',(14.6340009148641,15.3319397893059,4.59113972351818));
#127493=CARTESIAN_POINT('Ctrl Pts',(14.6278618132826,15.2357165728949,4.56044913332094));
#127494=CARTESIAN_POINT('Ctrl Pts',(14.6242567606021,15.1760500560231,4.54746453832502));
#127495=CARTESIAN_POINT('Ctrl Pts',(14.6190133279191,15.0915560248888,4.53729148298161));
#127496=CARTESIAN_POINT('Ctrl Pts',(14.6175009091381,15.067452211537,4.53530305421131));
#127497=CARTESIAN_POINT('Ctrl Pts',(14.6154359475302,15.0353597594244,4.53386416798412));
#127498=CARTESIAN_POINT('Ctrl Pts',(14.6149205339466,15.0274143647318,4.5336060837923));
#127499=CARTESIAN_POINT('Ctrl Pts',(14.6140621467026,15.0143082696865,4.53334211882138));
#127500=CARTESIAN_POINT('Ctrl Pts',(14.6137221313539,15.0091488777585,4.53327952207602));
#127501=CARTESIAN_POINT('Ctrl Pts',(14.613010956915,14.998430177031,4.53323529113415));
#127502=CARTESIAN_POINT('Ctrl Pts',(14.6126394857917,14.9928711456732,4.53326030268536));
#127503=CARTESIAN_POINT('Ctrl Pts',(14.6116180051611,14.9776842480105,4.53345962584562));
#127504=CARTESIAN_POINT('Ctrl Pts',(14.6109632759731,14.968058544759,4.53372984411391));
#127505=CARTESIAN_POINT('Ctrl Pts',(14.6094608041157,14.9461794271081,4.53467130868604));
#127506=CARTESIAN_POINT('Ctrl Pts',(14.6086095314212,14.933931621619,4.5354321806694));
#127507=CARTESIAN_POINT('Ctrl Pts',(14.6057057967256,14.8925534764597,4.53879447288777));
#127508=CARTESIAN_POINT('Ctrl Pts',(14.6036226884099,14.863528698632,4.54248434612449));
#127509=CARTESIAN_POINT('Ctrl Pts',(14.5960022598032,14.7585440238953,4.56070149758644));
#127510=CARTESIAN_POINT('Ctrl Pts',(14.5904708961661,14.684216038275,4.58301183391919));
#127511=CARTESIAN_POINT('Ctrl Pts',(14.5842342283134,14.5999532496313,4.61978339676486));
#127512=CARTESIAN_POINT('Ctrl Pts',(14.5832537069768,14.5867069224777,4.62592475039473));
#127513=CARTESIAN_POINT('Ctrl Pts',(14.5816552061013,14.5651259510178,4.63653062352975));
#127514=CARTESIAN_POINT('Ctrl Pts',(14.5810314904395,14.5567090438686,4.64082135655579));
#127515=CARTESIAN_POINT('Ctrl Pts',(14.579811341566,14.5402577407379,4.64951395562614));
#127516=CARTESIAN_POINT('Ctrl Pts',(14.5792147191394,14.5322203603309,4.65390799865534));
#127517=CARTESIAN_POINT('Ctrl Pts',(14.5777762731377,14.5128697541313,4.66484703435202));
#127518=CARTESIAN_POINT('Ctrl Pts',(14.5769386255146,14.501624274912,4.67150859096992));
#127519=CARTESIAN_POINT('Ctrl Pts',(14.5736219373558,14.457255414414,4.69902208360296));
#127520=CARTESIAN_POINT('Ctrl Pts',(14.5712064497555,14.4252750890677,4.72164977927811));
#127521=CARTESIAN_POINT('Ctrl Pts',(14.5664464018773,14.3642607584039,4.77063712231256));
#127522=CARTESIAN_POINT('Ctrl Pts',(14.5641060511043,14.3352829038458,4.7969453683536));
#127523=CARTESIAN_POINT('Ctrl Pts',(14.5592268717289,14.278871373715,4.854774045929));
#127524=CARTESIAN_POINT('Ctrl Pts',(14.5566899910943,14.2517280401488,4.88645994979635));
#127525=CARTESIAN_POINT('Ctrl Pts',(14.5533592993974,14.2202763431769,4.92837797760429));
#127526=CARTESIAN_POINT('Ctrl Pts',(14.5526700346192,14.2139796722366,4.93706773094576));
#127527=CARTESIAN_POINT('Ctrl Pts',(14.5515911953127,14.2044759999329,4.95065370560499));
#127528=CARTESIAN_POINT('Ctrl Pts',(14.5512079122834,14.2011664297671,4.95547754070249));
#127529=CARTESIAN_POINT('Ctrl Pts',(14.5504848886374,14.1950526914254,4.96456426501141));
#127530=CARTESIAN_POINT('Ctrl Pts',(14.5501458129865,14.1922381766586,4.96881977839053));
#127531=CARTESIAN_POINT('Ctrl Pts',(14.5493172244318,14.1854854581694,4.97920758696076));
#127532=CARTESIAN_POINT('Ctrl Pts',(14.5488255691205,14.1815827254473,4.98536242537818));
#127533=CARTESIAN_POINT('Ctrl Pts',(14.5469711567296,14.1672353732425,5.00856500997365));
#127534=CARTESIAN_POINT('Ctrl Pts',(14.5455846230981,14.1572514370523,5.02589029574184));
#127535=CARTESIAN_POINT('Ctrl Pts',(14.5416753705875,14.1309579236532,5.07497584409133));
#127536=CARTESIAN_POINT('Ctrl Pts',(14.539119511168,14.1158596103938,5.10734847516064));
#127537=CARTESIAN_POINT('Ctrl Pts',(14.5349381316765,14.094136932669,5.16157142395839));
#127538=CARTESIAN_POINT('Ctrl Pts',(14.5333130107176,14.0864333917894,5.18295443030695));
#127539=CARTESIAN_POINT('Ctrl Pts',(14.5283691455784,14.0651672292543,5.24922053192097));
#127540=CARTESIAN_POINT('Ctrl Pts',(14.5250962434043,14.0541074190835,5.29483917715732));
#127541=CARTESIAN_POINT('Ctrl Pts',(14.5209959470131,14.0441465257483,5.35461181805245));
#127542=CARTESIAN_POINT('Ctrl Pts',(14.5200767952742,14.0421804495769,5.36818448974565));
#127543=CARTESIAN_POINT('Ctrl Pts',(14.5186120224877,14.0394824416279,5.39008482047922));
#127544=CARTESIAN_POINT('Ctrl Pts',(14.5180609006384,14.0385686284797,5.39838773804601));
#127545=CARTESIAN_POINT('Ctrl Pts',(14.5169589273949,14.0369471206663,5.4151112500359));
#127546=CARTESIAN_POINT('Ctrl Pts',(14.516408200888,14.0362419895932,5.42353135916073));
#127547=CARTESIAN_POINT('Ctrl Pts',(14.5151899372806,14.0349185707578,5.4422885572769));
#127548=CARTESIAN_POINT('Ctrl Pts',(14.5145241424782,14.0343557906081,5.45262859988518));
#127549=CARTESIAN_POINT('Ctrl Pts',(14.5130663179659,14.0334812575654,5.47544717241359));
#127550=CARTESIAN_POINT('Ctrl Pts',(14.5122765758975,14.0332448196436,5.48792679808038));
#127551=CARTESIAN_POINT('Ctrl Pts',(14.5114930218304,14.0332500860612,5.50040792073653));
#127552=CARTESIAN_POINT('Ctrl Pts',(14.4551338463912,14.0332500192795,5.50019307209264));
#127553=CARTESIAN_POINT('Ctrl Pts',(14.4557159012467,14.0332482657504,5.49141280673769));
#127554=CARTESIAN_POINT('Ctrl Pts',(14.4562942528936,14.0333661289407,5.48263269314337));
#127555=CARTESIAN_POINT('Ctrl Pts',(14.4574635793255,14.0338492876714,5.46477361229857));
#127556=CARTESIAN_POINT('Ctrl Pts',(14.4580542373397,14.034222986886,5.45569574024463));
#127557=CARTESIAN_POINT('Ctrl Pts',(14.4595354630645,14.0354890840162,5.4327989780009));
#127558=CARTESIAN_POINT('Ctrl Pts',(14.4604207967587,14.0365505226987,5.41899123835604));
#127559=CARTESIAN_POINT('Ctrl Pts',(14.4650053873969,14.0436467522466,5.34696613391879));
#127560=CARTESIAN_POINT('Ctrl Pts',(14.4685476779816,14.0546624594865,5.2893607311592));
#127561=CARTESIAN_POINT('Ctrl Pts',(14.4757658684554,14.0877605023073,5.17413416999683));
#127562=CARTESIAN_POINT('Ctrl Pts',(14.479426002587,14.1102705154676,5.11692170777077));
#127563=CARTESIAN_POINT('Ctrl Pts',(14.483965621619,14.1425127685023,5.05343691195598));
#127564=CARTESIAN_POINT('Ctrl Pts',(14.4846011352322,14.147115545359,5.04470774992328));
#127565=CARTESIAN_POINT('Ctrl Pts',(14.4856025939995,14.1544887193919,5.0312287888832));
#127566=CARTESIAN_POINT('Ctrl Pts',(14.4859632321623,14.1571675212422,5.02642932608613));
#127567=CARTESIAN_POINT('Ctrl Pts',(14.4866555699781,14.1623511374431,5.01732542404476));
#127568=CARTESIAN_POINT('Ctrl Pts',(14.4869868289616,14.1648485199009,5.01301708039379));
#127569=CARTESIAN_POINT('Ctrl Pts',(14.4878107610462,14.1711046219397,5.00241406197519));
#127570=CARTESIAN_POINT('Ctrl Pts',(14.4883057356817,14.1749018322251,4.99614256077822));
#127571=CARTESIAN_POINT('Ctrl Pts',(14.4902692504298,14.1901304906588,4.97162461667665));
#127572=CARTESIAN_POINT('Ctrl Pts',(14.4917657964724,14.2020981350885,4.95372018681841));
#127573=CARTESIAN_POINT('Ctrl Pts',(14.4961702948044,14.2385962620791,4.90287711021017));
#127574=CARTESIAN_POINT('Ctrl Pts',(14.4991211079901,14.2646398645396,4.8710829498318));
#127575=CARTESIAN_POINT('Ctrl Pts',(14.5061953170165,14.3320353697439,4.79873554605297));
#127576=CARTESIAN_POINT('Ctrl Pts',(14.510285943358,14.3751670120194,4.76004449787031));
#127577=CARTESIAN_POINT('Ctrl Pts',(14.5153187040557,14.4343689216037,4.71582855177125));
#127578=CARTESIAN_POINT('Ctrl Pts',(14.516400641743,14.4474714974782,4.70654194660089));
#127579=CARTESIAN_POINT('Ctrl Pts',(14.5181056704665,14.4687134886681,4.69226792451271));
#127580=CARTESIAN_POINT('Ctrl Pts',(14.5187365154515,14.4767054256657,4.68706749218021));
#127581=CARTESIAN_POINT('Ctrl Pts',(14.5199338244367,14.4921227089064,4.67735690435418));
#127582=CARTESIAN_POINT('Ctrl Pts',(14.5205009648824,14.4995344255461,4.67282696943287));
#127583=CARTESIAN_POINT('Ctrl Pts',(14.5218103802034,14.5168932448561,4.6625362522747));
#127584=CARTESIAN_POINT('Ctrl Pts',(14.5225499023867,14.526884154408,4.65685168556305));
#127585=CARTESIAN_POINT('Ctrl Pts',(14.5250292573993,14.5609821559958,4.63824780755595));
#127586=CARTESIAN_POINT('Ctrl Pts',(14.5267403140545,14.5855362681686,4.62617305998854));
#127587=CARTESIAN_POINT('Ctrl Pts',(14.5311224474528,14.6505720098178,4.5975502014663));
#127588=CARTESIAN_POINT('Ctrl Pts',(14.5337490469884,14.6917221508466,4.58267748243849));
#127589=CARTESIAN_POINT('Ctrl Pts',(14.5395743864789,14.7847373792455,4.55602862925647));
#127590=CARTESIAN_POINT('Ctrl Pts',(14.5427652566447,14.836846771476,4.54564175129847));
#127591=CARTESIAN_POINT('Ctrl Pts',(14.5468001361465,14.8998548988134,4.53839489916365));
#127592=CARTESIAN_POINT('Ctrl Pts',(14.5474676877465,14.9101898745843,4.53737466675388));
#127593=CARTESIAN_POINT('Ctrl Pts',(14.548512639153,14.9261882144473,4.53605523187129));
#127594=CARTESIAN_POINT('Ctrl Pts',(14.5488841207593,14.9318414667097,4.53563901667661));
#127595=CARTESIAN_POINT('Ctrl Pts',(14.5495835673948,14.9424139890842,4.53495405114045));
#127596=CARTESIAN_POINT('Ctrl Pts',(14.5499108904544,14.9473321502888,4.5346731510154));
#127597=CARTESIAN_POINT('Ctrl Pts',(14.5507065417269,14.9592192347822,4.53408532927657));
#127598=CARTESIAN_POINT('Ctrl Pts',(14.5511768112331,14.9661896320437,4.5338162317592));
#127599=CARTESIAN_POINT('Ctrl Pts',(14.5529151395704,14.9917750737023,4.53310568110659));
#127600=CARTESIAN_POINT('Ctrl Pts',(14.5542039680372,15.0103978073792,4.53312665888173));
#127601=CARTESIAN_POINT('Ctrl Pts',(14.5577476100555,15.0609540829293,4.53464425953279));
#127602=CARTESIAN_POINT('Ctrl Pts',(14.5600301234813,15.0928325337556,4.53718692109876));
#127603=CARTESIAN_POINT('Ctrl Pts',(14.5674990162854,15.1962873302107,4.55062462628029));
#127604=CARTESIAN_POINT('Ctrl Pts',(14.5726644261818,15.2667892039884,4.56797572184593));
#127605=CARTESIAN_POINT('Ctrl Pts',(14.5786123827311,15.3489033941455,4.59827878527939));
#127606=CARTESIAN_POINT('Ctrl Pts',(14.579630627688,15.3629809491717,4.60385291308143));
#127607=CARTESIAN_POINT('Ctrl Pts',(14.5812601175737,15.3855300777399,4.61340003716616));
#127608=CARTESIAN_POINT('Ctrl Pts',(14.5818779547303,15.3940846158589,4.61716917772784));
#127609=CARTESIAN_POINT('Ctrl Pts',(14.5830658599349,15.4105350766351,4.62470404567787));
#127610=CARTESIAN_POINT('Ctrl Pts',(14.5836363872476,15.4184371663903,4.62845401565536));
#127611=CARTESIAN_POINT('Ctrl Pts',(14.5849768638616,15.4369975247548,4.63757254426081));
#127612=CARTESIAN_POINT('Ctrl Pts',(14.5857436224197,15.447609568049,4.64303229492802));
#127613=CARTESIAN_POINT('Ctrl Pts',(14.5884575631631,15.4851102835891,4.66321261214065));
#127614=CARTESIAN_POINT('Ctrl Pts',(14.5903675005709,15.5113978943296,4.67901426358274));
#127615=CARTESIAN_POINT('Ctrl Pts',(14.5953389059958,15.578742943513,4.72398791356286));
#127616=CARTESIAN_POINT('Ctrl Pts',(14.5983422152116,15.6183475668038,4.75516134902374));
#127617=CARTESIAN_POINT('Ctrl Pts',(14.6038990812618,15.6860108712211,4.8175525768507));
#127618=CARTESIAN_POINT('Ctrl Pts',(14.6064373574725,15.7148105584246,4.84778028997057));
#127619=CARTESIAN_POINT('Ctrl Pts',(14.6097623376094,15.7483675553722,4.88790199022174));
#127620=CARTESIAN_POINT('Ctrl Pts',(14.6104434347544,15.7550350304846,4.89614566936446));
#127621=CARTESIAN_POINT('Ctrl Pts',(14.611504992425,15.7650840915549,4.90899701496086));
#127622=CARTESIAN_POINT('Ctrl Pts',(14.6118792284899,15.7685628582689,4.91352807022952));
#127623=CARTESIAN_POINT('Ctrl Pts',(14.6125804643426,15.7749581463652,4.92201248536826));
#127624=CARTESIAN_POINT('Ctrl Pts',(14.612906768711,15.7778849985179,4.92595764914075));
#127625=CARTESIAN_POINT('Ctrl Pts',(14.6136951202583,15.7848408067519,4.93548440557271));
#127626=CARTESIAN_POINT('Ctrl Pts',(14.614159018699,15.7888403838212,4.94108695626274));
#127627=CARTESIAN_POINT('Ctrl Pts',(14.6158444974217,15.8030494123182,4.96144710578652));
#127628=CARTESIAN_POINT('Ctrl Pts',(14.6170853162429,15.8129067507068,4.9764447485323));
#127629=CARTESIAN_POINT('Ctrl Pts',(14.6204480868898,15.8381711372003,5.0173186496646));
#127630=CARTESIAN_POINT('Ctrl Pts',(14.6225948515494,15.8527959785939,5.04365476593296));
#127631=CARTESIAN_POINT('Ctrl Pts',(14.6301976509346,15.8999830525677,5.13884489829768));
#127632=CARTESIAN_POINT('Ctrl Pts',(14.6356427312191,15.9256280953443,5.21083030648119));
#127633=CARTESIAN_POINT('Ctrl Pts',(14.6418039581923,15.9458104016349,5.29934583783434));
#127634=CARTESIAN_POINT('Ctrl Pts',(14.6427865455595,15.9487374722334,5.31367593675688));
#127635=CARTESIAN_POINT('Ctrl Pts',(14.6443737348601,15.9529823288549,5.33716363010445));
#127636=CARTESIAN_POINT('Ctrl Pts',(14.6449843084876,15.9544957307331,5.34628301196179));
#127637=CARTESIAN_POINT('Ctrl Pts',(14.6461678317978,15.95719323404,5.36411768773545));
#127638=CARTESIAN_POINT('Ctrl Pts',(14.6467411093006,15.9583896561407,5.37283017084212));
#127639=CARTESIAN_POINT('Ctrl Pts',(14.6481033879374,15.9609660470993,5.39370082847558));
#127640=CARTESIAN_POINT('Ctrl Pts',(14.6488888923635,15.962234425322,5.40587141970355));
#127641=CARTESIAN_POINT('Ctrl Pts',(14.6517815828048,15.9660854818773,5.45114552820237));
#127642=CARTESIAN_POINT('Ctrl Pts',(14.6538442387805,15.9671935734666,5.48435279840596));
#127643=CARTESIAN_POINT('Ctrl Pts',(14.6598091123436,15.9654237582607,5.58180581490235));
#127644=CARTESIAN_POINT('Ctrl Pts',(14.6636037643855,15.9578535960652,5.64577815765663));
#127645=CARTESIAN_POINT('Ctrl Pts',(14.6693117446593,15.9377319730729,5.73686899247888));
#127646=CARTESIAN_POINT('Ctrl Pts',(14.6711148826084,15.9301979215612,5.76491448124882));
#127647=CARTESIAN_POINT('Ctrl Pts',(14.6735043371278,15.9189299611452,5.80040089062594));
#127648=CARTESIAN_POINT('Ctrl Pts',(14.6740359025913,15.9163457797879,5.80819372108466));
#127649=CARTESIAN_POINT('Ctrl Pts',(14.6748764519703,15.9121460387369,5.82033842157776));
#127650=CARTESIAN_POINT('Ctrl Pts',(14.675181735813,15.9105977838248,5.8247133724245));
#127651=CARTESIAN_POINT('Ctrl Pts',(14.6758259784563,15.9072843803776,5.83386607760869));
#127652=CARTESIAN_POINT('Ctrl Pts',(14.6761653252999,15.905512880837,5.83864128992218));
#127653=CARTESIAN_POINT('Ctrl Pts',(14.6770386651027,15.9008851741584,5.85081965484903));
#127654=CARTESIAN_POINT('Ctrl Pts',(14.6775755743344,15.8979754398581,5.85820193569529));
#127655=CARTESIAN_POINT('Ctrl Pts',(14.6800175767679,15.884437799348,5.89134635985226));
#127656=CARTESIAN_POINT('Ctrl Pts',(14.6819697987547,15.872790597227,5.9166755171201));
#127657=CARTESIAN_POINT('Ctrl Pts',(14.689109918682,15.8268024962347,6.00627028080881));
#127658=CARTESIAN_POINT('Ctrl Pts',(14.6943907107138,15.7863146418972,6.06711833970452));
#127659=CARTESIAN_POINT('Ctrl Pts',(14.701377771157,15.7216688968061,6.14385932824967));
#127660=CARTESIAN_POINT('Ctrl Pts',(14.703261944121,15.7030737018993,6.16411478350293));
#127661=CARTESIAN_POINT('Ctrl Pts',(14.7058247355717,15.6761417083022,6.19105020445264));
#127662=CARTESIAN_POINT('Ctrl Pts',(14.706532875664,15.6685213505722,6.19842480885201));
#127663=CARTESIAN_POINT('Ctrl Pts',(14.7078169050663,15.6543800455728,6.21166650507075));
#127664=CARTESIAN_POINT('Ctrl Pts',(14.7083944155844,15.6478977234032,6.21757299764084));
#127665=CARTESIAN_POINT('Ctrl Pts',(14.7095651813831,15.6345107927995,6.22944143597547));
#127666=CARTESIAN_POINT('Ctrl Pts',(14.710158079161,15.6276003635259,6.23539550424442));
#127667=CARTESIAN_POINT('Ctrl Pts',(14.7116513684583,15.6098708426011,6.25023940366577));
#127668=CARTESIAN_POINT('Ctrl Pts',(14.7125463587244,15.5989407745463,6.25899379929153));
#127669=CARTESIAN_POINT('Ctrl Pts',(14.7174033083303,15.5380465800803,6.30563183241361));
#127670=CARTESIAN_POINT('Ctrl Pts',(14.7211824159237,15.4846770430772,6.33882422675857));
#127671=CARTESIAN_POINT('Ctrl Pts',(14.7283344787804,15.3781693045675,6.3914826904229));
#127672=CARTESIAN_POINT('Ctrl Pts',(14.7316991174617,15.3258115969497,6.41192033966295));
#127673=CARTESIAN_POINT('Ctrl Pts',(14.7359168818552,15.2622411376113,6.43055803270327));
#127674=CARTESIAN_POINT('Ctrl Pts',(14.7365699982163,15.252453310958,6.43326093514765));
#127675=CARTESIAN_POINT('Ctrl Pts',(14.7375969941586,15.2371873302122,6.43721891303761));
#127676=CARTESIAN_POINT('Ctrl Pts',(14.7379652636439,15.2317374444656,6.43858130900884));
#127677=CARTESIAN_POINT('Ctrl Pts',(14.7386623784725,15.221474396713,6.44105209599221));
#127678=CARTESIAN_POINT('Ctrl Pts',(14.7389906395166,15.2166641389722,6.44217121705684));
#127679=CARTESIAN_POINT('Ctrl Pts',(14.7397936848036,15.204947506812,6.44480266017057));
#127680=CARTESIAN_POINT('Ctrl Pts',(14.7402705064242,15.1980328122773,6.44627614641491));
#127681=CARTESIAN_POINT('Ctrl Pts',(14.7420657915134,15.1721325136019,6.45149906326037));
#127682=CARTESIAN_POINT('Ctrl Pts',(14.7434067537731,15.1530529724865,6.45475376161493));
#127683=CARTESIAN_POINT('Ctrl Pts',(14.7471538836816,15.1001484395617,6.46215207725746));
#127684=CARTESIAN_POINT('Ctrl Pts',(14.7495911485891,15.0661824292158,6.46508341685769));
#127685=CARTESIAN_POINT('Ctrl Pts',(14.7569322804306,14.9637293019913,6.46849079877257));
#127686=CARTESIAN_POINT('Ctrl Pts',(14.7618075388576,14.8952648637467,6.46349543267255));
#127687=CARTESIAN_POINT('Ctrl Pts',(14.7675260069024,14.8125533357465,6.44853168723102));
#127688=CARTESIAN_POINT('Ctrl Pts',(14.7685755823343,14.7972809606664,6.44538545153537));
#127689=CARTESIAN_POINT('Ctrl Pts',(14.7702421680797,14.7728953674135,6.43974364925108));
#127690=CARTESIAN_POINT('Ctrl Pts',(14.7708663356886,14.7637315276876,6.43748165849733));
#127691=CARTESIAN_POINT('Ctrl Pts',(14.7720584679983,14.7461760629583,6.43287451330997));
#127692=CARTESIAN_POINT('Ctrl Pts',(14.7726270019202,14.7377801782427,6.43054941933844));
#127693=CARTESIAN_POINT('Ctrl Pts',(14.7739507486897,14.7181851831991,6.42483665532532));
#127694=CARTESIAN_POINT('Ctrl Pts',(14.7747030032042,14.7070137287492,6.42135850441716));
#127695=CARTESIAN_POINT('Ctrl Pts',(14.7772893928943,14.6685210105139,6.40860312307736));
#127696=CARTESIAN_POINT('Ctrl Pts',(14.7790910270293,14.6415526442626,6.39830600372744));
#127697=CARTESIAN_POINT('Ctrl Pts',(14.7838239786133,14.5710000785529,6.36768316142892));
#127698=CARTESIAN_POINT('Ctrl Pts',(14.786699852823,14.5284044492095,6.34528864055014));
#127699=CARTESIAN_POINT('Ctrl Pts',(14.7923937280301,14.4482914393166,6.29522154189329));
#127700=CARTESIAN_POINT('Ctrl Pts',(14.7952041116426,14.4107598617516,6.26782469489093));
#127701=CARTESIAN_POINT('Ctrl Pts',(14.798825981993,14.3672804095238,6.23101513923496));
#127702=CARTESIAN_POINT('Ctrl Pts',(14.7995048468504,14.3593286917441,6.22405625977445));
#127703=CARTESIAN_POINT('Ctrl Pts',(14.8005636588418,14.3472619004382,6.21314170038985));
#127704=CARTESIAN_POINT('Ctrl Pts',(14.8009374319884,14.3430648764696,6.2092773441921));
#127705=CARTESIAN_POINT('Ctrl Pts',(14.8016383620152,14.3353163936808,6.20201525729485));
#127706=CARTESIAN_POINT('Ctrl Pts',(14.8019648323866,14.3317562701737,6.19862724776633));
#127707=CARTESIAN_POINT('Ctrl Pts',(14.8027543665008,14.3232612522442,6.19041858379502));
#127708=CARTESIAN_POINT('Ctrl Pts',(14.8032192960369,14.3183519161801,6.18557205067067));
#127709=CARTESIAN_POINT('Ctrl Pts',(14.8049131101738,14.3007856258145,6.16785526842038));
#127710=CARTESIAN_POINT('Ctrl Pts',(14.8061614693273,14.2884385929593,6.1546844059523));
#127711=CARTESIAN_POINT('Ctrl Pts',(14.809552233321,14.2563097125978,6.11842878111755));
#127712=CARTESIAN_POINT('Ctrl Pts',(14.8117198883546,14.2372360730487,6.09474398093096));
#127713=CARTESIAN_POINT('Ctrl Pts',(14.8193008655827,14.1747571118368,6.00920115099284));
#127714=CARTESIAN_POINT('Ctrl Pts',(14.8247014641308,14.1374981619209,5.94317728032089));
#127715=CARTESIAN_POINT('Ctrl Pts',(14.830829231318,14.1026231417896,5.85991208247549));
#127716=CARTESIAN_POINT('Ctrl Pts',(14.8318177769152,14.0972506323274,5.84621604777781));
#127717=CARTESIAN_POINT('Ctrl Pts',(14.8334120657391,14.0890082139625,5.82370557210395));
#127718=CARTESIAN_POINT('Ctrl Pts',(14.8340238820166,14.0859489460937,5.81496350975598));
#127719=CARTESIAN_POINT('Ctrl Pts',(14.8352081690579,14.0802331754215,5.79784515952652));
#127720=CARTESIAN_POINT('Ctrl Pts',(14.8357809898768,14.0775643267897,5.78947398464046));
#127721=CARTESIAN_POINT('Ctrl Pts',(14.8371395329623,14.0714678942418,5.76941068086777));
#127722=CARTESIAN_POINT('Ctrl Pts',(14.8379218122652,14.0681464402074,5.75768769972735));
#127723=CARTESIAN_POINT('Ctrl Pts',(14.8395761523705,14.0615377959022,5.73256100977512));
#127724=CARTESIAN_POINT('Ctrl Pts',(14.8404461779773,14.0583141926738,5.7191433310388));
#127725=CARTESIAN_POINT('Ctrl Pts',(14.845648774081,14.0406118807541,5.63783476903828));
#127726=CARTESIAN_POINT('Ctrl Pts',(14.8497692954516,14.0331928278937,5.56861699671362));
#127727=CARTESIAN_POINT('Ctrl Pts',(14.8539665691581,14.033250331692,5.49919917142664));
#127728=CARTESIAN_POINT('Origin',(16.125,15.,5.5));
#127729=CARTESIAN_POINT('',(15.3122364200794,14.0332501750868,5.50058183360759));
#127730=CARTESIAN_POINT('',(15.2539186838427,14.0332502815979,5.50073788408625));
#127731=CARTESIAN_POINT('',(16.125,14.03325,5.5));
#127732=CARTESIAN_POINT('Ctrl Pts',(15.3128321466295,14.0332501978693,5.50061853078022));
#127733=CARTESIAN_POINT('Ctrl Pts',(15.3115187040417,14.0332638396951,5.52194039987235));
#127734=CARTESIAN_POINT('Ctrl Pts',(15.3101876143888,14.0339828660901,5.54325476764825));
#127735=CARTESIAN_POINT('Ctrl Pts',(15.3083790219664,14.0358729530645,5.57150927105893));
#127736=CARTESIAN_POINT('Ctrl Pts',(15.3079288180362,14.0364158523844,5.57848644909956));
#127737=CARTESIAN_POINT('Ctrl Pts',(15.3071453680829,14.0374835322328,5.59051753162644));
#127738=CARTESIAN_POINT('Ctrl Pts',(15.3068138862805,14.0379725046415,5.59557441990132));
#127739=CARTESIAN_POINT('Ctrl Pts',(15.306156146715,14.039015099918,5.60553648913005));
#127740=CARTESIAN_POINT('Ctrl Pts',(15.3058300085175,14.0395664581816,5.61044156497212));
#127741=CARTESIAN_POINT('Ctrl Pts',(15.3051079721908,14.0408618432062,5.62122136784803));
#127742=CARTESIAN_POINT('Ctrl Pts',(15.3047112602944,14.0416222809291,5.6270935364513));
#127743=CARTESIAN_POINT('Ctrl Pts',(15.3035651261934,14.0439593190561,5.64392486281022));
#127744=CARTESIAN_POINT('Ctrl Pts',(15.3028091909319,14.0456702614042,5.65486405339201));
#127745=CARTESIAN_POINT('Ctrl Pts',(15.2983855678006,14.0566730876314,5.71808044788869));
#127746=CARTESIAN_POINT('Ctrl Pts',(15.2945699991171,14.07007083561,5.76954720982888));
#127747=CARTESIAN_POINT('Ctrl Pts',(15.2883795028949,14.0986762662122,5.85119564355005));
#127748=CARTESIAN_POINT('Ctrl Pts',(15.2859971059405,14.1113575208729,5.88214870315479));
#127749=CARTESIAN_POINT('Ctrl Pts',(15.2812617651042,14.1401358777695,5.94316777095965));
#127750=CARTESIAN_POINT('Ctrl Pts',(15.2789134700689,14.1562710933651,5.97316589341539));
#127751=CARTESIAN_POINT('Ctrl Pts',(15.2757712375708,14.1804831742435,6.01298687661458));
#127752=CARTESIAN_POINT('Ctrl Pts',(15.2749316322307,14.1872182451739,6.02359259654184));
#127753=CARTESIAN_POINT('Ctrl Pts',(15.2734983980139,14.1991710494237,6.04162799799324));
#127754=CARTESIAN_POINT('Ctrl Pts',(15.2729012825498,14.2042900859759,6.04912078665659));
#127755=CARTESIAN_POINT('Ctrl Pts',(15.2716807686209,14.2150374634005,6.06438589252334));
#127756=CARTESIAN_POINT('Ctrl Pts',(15.2710578969236,14.2206775625385,6.0721487295442));
#127757=CARTESIAN_POINT('Ctrl Pts',(15.2694496980913,14.235637224425,6.09210695476351));
#127758=CARTESIAN_POINT('Ctrl Pts',(15.2684711943613,14.245133475394,6.1041669215372));
#127759=CARTESIAN_POINT('Ctrl Pts',(15.2629625348449,14.3007436687247,6.17143099904223));
#127760=CARTESIAN_POINT('Ctrl Pts',(15.2586755591041,14.3526170486515,6.22157835515635));
#127761=CARTESIAN_POINT('Ctrl Pts',(15.2517457763976,14.4435331535795,6.29170016046074));
#127762=CARTESIAN_POINT('Ctrl Pts',(15.2491403377796,14.4791910352566,6.31559902256754));
#127763=CARTESIAN_POINT('Ctrl Pts',(15.2457139439915,14.5259039493217,6.3425919521112));
#127764=CARTESIAN_POINT('Ctrl Pts',(15.2450027918963,14.5355889408296,6.34796851752898));
#127765=CARTESIAN_POINT('Ctrl Pts',(15.2439010976513,14.5505319641898,6.35593127250696));
#127766=CARTESIAN_POINT('Ctrl Pts',(15.2435174260375,14.5557250091717,6.35863821644771));
#127767=CARTESIAN_POINT('Ctrl Pts',(15.2427943175024,14.56548390062,6.36361293959962));
#127768=CARTESIAN_POINT('Ctrl Pts',(15.2424555554474,14.5700435867575,6.36589204176814));
#127769=CARTESIAN_POINT('Ctrl Pts',(15.2416285914776,14.581148132739,6.37133317894235));
#127770=CARTESIAN_POINT('Ctrl Pts',(15.2411382647219,14.5877109347826,6.3744576115256));
#127771=CARTESIAN_POINT('Ctrl Pts',(15.2393872358782,14.6110937954121,6.38526804429975));
#127772=CARTESIAN_POINT('Ctrl Pts',(15.2381066469615,14.6280975515904,6.39254468642281));
#127773=CARTESIAN_POINT('Ctrl Pts',(15.2325441423059,14.701940794573,6.42166899836418));
#127774=CARTESIAN_POINT('Ctrl Pts',(15.2281351401414,14.7605661354887,6.43860771142775));
#127775=CARTESIAN_POINT('Ctrl Pts',(15.2216090235543,14.8508778384536,6.45568329931842));
#127776=CARTESIAN_POINT('Ctrl Pts',(15.2194300351935,14.8816225354205,6.45997658592658));
#127777=CARTESIAN_POINT('Ctrl Pts',(15.2157619620799,14.9345858496299,6.46478875885003));
#127778=CARTESIAN_POINT('Ctrl Pts',(15.2142546488528,14.9567126562855,6.46603452202677));
#127779=CARTESIAN_POINT('Ctrl Pts',(15.2120405778929,14.9897492895735,6.46675696293682));
#127780=CARTESIAN_POINT('Ctrl Pts',(15.2113166874645,15.0006378908934,6.46681110448699));
#127781=CARTESIAN_POINT('Ctrl Pts',(15.2100691471211,15.0195473747028,6.46658565207274));
#127782=CARTESIAN_POINT('Ctrl Pts',(15.2095429880161,15.02756797352,6.46639015718251));
#127783=CARTESIAN_POINT('Ctrl Pts',(15.2083575996848,15.0457346205461,6.46572100170452));
#127784=CARTESIAN_POINT('Ctrl Pts',(15.2077002665615,15.0558776006124,6.46518724347849));
#127785=CARTESIAN_POINT('Ctrl Pts',(15.2059108829298,15.0836585950152,6.4632858934019));
#127786=CARTESIAN_POINT('Ctrl Pts',(15.2047887247483,15.1012708838623,6.46159385452689));
#127787=CARTESIAN_POINT('Ctrl Pts',(15.1990713239709,15.1917177073616,6.45039167419396));
#127788=CARTESIAN_POINT('Ctrl Pts',(15.1947180110117,15.2633402485568,6.43308762765077));
#127789=CARTESIAN_POINT('Ctrl Pts',(15.1879918923192,15.3676629205402,6.394900222755));
#127790=CARTESIAN_POINT('Ctrl Pts',(15.1856893642871,15.4022212976442,6.37990903033206));
#127791=CARTESIAN_POINT('Ctrl Pts',(15.1826265938316,15.4451842621796,6.35821135318109));
#127792=CARTESIAN_POINT('Ctrl Pts',(15.1819515987372,15.4544761783783,6.35332709802575));
#127793=CARTESIAN_POINT('Ctrl Pts',(15.1808942376215,15.4687222803984,6.34554001992032));
#127794=CARTESIAN_POINT('Ctrl Pts',(15.180517914238,15.4737335205734,6.34274257569455));
#127795=CARTESIAN_POINT('Ctrl Pts',(15.1797994870259,15.4831815477642,6.33735747055257));
#127796=CARTESIAN_POINT('Ctrl Pts',(15.1794579141628,15.4876230909291,6.33477880771696));
#127797=CARTESIAN_POINT('Ctrl Pts',(15.1786917750274,15.4974770424425,6.32895234884509));
#127798=CARTESIAN_POINT('Ctrl Pts',(15.1782661551395,15.5028785969426,6.32568669363078));
#127799=CARTESIAN_POINT('Ctrl Pts',(15.1767365279009,15.5220468193235,6.31384017546189));
#127800=CARTESIAN_POINT('Ctrl Pts',(15.1756169167759,15.5356283090814,6.30496643302873));
#127801=CARTESIAN_POINT('Ctrl Pts',(15.1691365325615,15.6120399606369,6.2522512593837));
#127802=CARTESIAN_POINT('Ctrl Pts',(15.1635541137289,15.6697063774724,6.20140518916088));
#127803=CARTESIAN_POINT('Ctrl Pts',(15.1556708014497,15.7444309020794,6.11780977981688));
#127804=CARTESIAN_POINT('Ctrl Pts',(15.1532173907206,15.7666198071558,6.0900515812407));
#127805=CARTESIAN_POINT('Ctrl Pts',(15.1499635952347,15.7946161493953,6.05077448259291));
#127806=CARTESIAN_POINT('Ctrl Pts',(15.1491130743593,15.8017942561891,6.04027155402949));
#127807=CARTESIAN_POINT('Ctrl Pts',(15.1476672079899,15.8137484842671,6.02201702099355));
#127808=CARTESIAN_POINT('Ctrl Pts',(15.14706821163,15.8186260840331,6.01433423938282));
#127809=CARTESIAN_POINT('Ctrl Pts',(15.1458489345443,15.8283960603813,5.99845423969093));
#127810=CARTESIAN_POINT('Ctrl Pts',(15.1452291127318,15.8332769713166,5.99025112090035));
#127811=CARTESIAN_POINT('Ctrl Pts',(15.143639827844,15.8455615270486,5.96889138662987));
#127812=CARTESIAN_POINT('Ctrl Pts',(15.1426768750275,15.8527800934401,5.95563096839243));
#127813=CARTESIAN_POINT('Ctrl Pts',(15.1370604225208,15.8934553924482,5.87655484565393));
#127814=CARTESIAN_POINT('Ctrl Pts',(15.1326665494928,15.9195942117416,5.80725164799159));
#127815=CARTESIAN_POINT('Ctrl Pts',(15.1256897907898,15.9477537718199,5.69520915942276));
#127816=CARTESIAN_POINT('Ctrl Pts',(15.1231528619947,15.9552888987025,5.65416303838326));
#127817=CARTESIAN_POINT('Ctrl Pts',(15.1198086302791,15.9614283904363,5.60188692141483));
#127818=CARTESIAN_POINT('Ctrl Pts',(15.1191053099038,15.9625208066296,5.59098993250991));
#127819=CARTESIAN_POINT('Ctrl Pts',(15.118013209201,15.9639108358018,5.57426617935566));
#127820=CARTESIAN_POINT('Ctrl Pts',(15.1176311161427,15.9643412369382,5.56845099934459));
#127821=CARTESIAN_POINT('Ctrl Pts',(15.1169090801069,15.9650497320371,5.55753814918427));
#127822=CARTESIAN_POINT('Ctrl Pts',(15.1165697816303,15.9653400933337,5.55244161788744));
#127823=CARTESIAN_POINT('Ctrl Pts',(15.1157388347372,15.9659484926609,5.5400329799026));
#127824=CARTESIAN_POINT('Ctrl Pts',(15.1152450093898,15.966223874153,5.53271921514453));
#127825=CARTESIAN_POINT('Ctrl Pts',(15.1134684198291,15.9669105107585,5.50659754613027));
#127826=CARTESIAN_POINT('Ctrl Pts',(15.112165056105,15.9668557794016,5.48778267660359));
#127827=CARTESIAN_POINT('Ctrl Pts',(15.1070213867429,15.9645020198274,5.41445796172126));
#127828=CARTESIAN_POINT('Ctrl Pts',(15.103081557505,15.9581398280082,5.3601806381725));
#127829=CARTESIAN_POINT('Ctrl Pts',(15.0967378311562,15.9403384593363,5.2729341326345));
#127830=CARTESIAN_POINT('Ctrl Pts',(15.0943046223575,15.9316384624109,5.23952838127793));
#127831=CARTESIAN_POINT('Ctrl Pts',(15.0902749733644,15.913961005331,5.18401679659159));
#127832=CARTESIAN_POINT('Ctrl Pts',(15.0886548438555,15.9059187776485,5.1616489492879));
#127833=CARTESIAN_POINT('Ctrl Pts',(15.0863122829395,15.8928998164517,5.12924401333605));
#127834=CARTESIAN_POINT('Ctrl Pts',(15.0855696324456,15.8885607021878,5.11896197060088));
#127835=CARTESIAN_POINT('Ctrl Pts',(15.0842506818744,15.8804757800673,5.10069345267799));
#127836=CARTESIAN_POINT('Ctrl Pts',(15.0836722360708,15.8767969287001,5.09267890754575));
#127837=CARTESIAN_POINT('Ctrl Pts',(15.082429290043,15.8686056626878,5.07545926848846));
#127838=CARTESIAN_POINT('Ctrl Pts',(15.0817661513036,15.8640554272843,5.06627328713382));
#127839=CARTESIAN_POINT('Ctrl Pts',(15.0799420589107,15.8510462098436,5.04102799096384));
#127840=CARTESIAN_POINT('Ctrl Pts',(15.0787916716643,15.842279575443,5.02513145226642));
#127841=CARTESIAN_POINT('Ctrl Pts',(15.0723122670322,15.7898213633755,4.9360376525949));
#127842=CARTESIAN_POINT('Ctrl Pts',(15.0673232111859,15.7370519080608,4.86863218129446));
#127843=CARTESIAN_POINT('Ctrl Pts',(15.0603111804128,15.6551531066365,4.78849366376793));
#127844=CARTESIAN_POINT('Ctrl Pts',(15.0584879480145,15.6332549899201,4.76893594634241));
#127845=CARTESIAN_POINT('Ctrl Pts',(15.0560773584071,15.6041438666722,4.74522650533729));
#127846=CARTESIAN_POINT('Ctrl Pts',(15.0555460661274,15.597718613909,4.74012811094686));
#127847=CARTESIAN_POINT('Ctrl Pts',(15.0546651201179,15.5870673348336,4.73189507147508));
#127848=CARTESIAN_POINT('Ctrl Pts',(15.0543186587826,15.5828790296137,4.72871193978219));
#127849=CARTESIAN_POINT('Ctrl Pts',(15.0536505535982,15.5748089187273,4.72268189211238));
#127850=CARTESIAN_POINT('Ctrl Pts',(15.0533293378125,15.5709314564826,4.71982950359688));
#127851=CARTESIAN_POINT('Ctrl Pts',(15.0524295618524,15.5600726717527,4.71196572568825));
#127852=CARTESIAN_POINT('Ctrl Pts',(15.0518470585849,15.5530457714742,4.70701842554861));
#127853=CARTESIAN_POINT('Ctrl Pts',(15.0490234461091,15.5189554020508,4.68369055142465));
#127854=CARTESIAN_POINT('Ctrl Pts',(15.0467188459707,15.4910386608113,4.66659946174765));
#127855=CARTESIAN_POINT('Ctrl Pts',(15.0400845651691,15.4091899059507,4.62203195702067));
#127856=CARTESIAN_POINT('Ctrl Pts',(15.0357198800467,15.3534649020903,4.59815310887772));
#127857=CARTESIAN_POINT('Ctrl Pts',(15.0292075009051,15.26496571232,4.56970291212749));
#127858=CARTESIAN_POINT('Ctrl Pts',(15.0269712323874,15.2335756724448,4.5613295048864));
#127859=CARTESIAN_POINT('Ctrl Pts',(15.0239489083797,15.1897113268647,4.55196598554933));
#127860=CARTESIAN_POINT('Ctrl Pts',(15.0231217250932,15.177553012943,4.54961385137285));
#127861=CARTESIAN_POINT('Ctrl Pts',(15.02170280573,15.1564402375478,4.54594872547178));
#127862=CARTESIAN_POINT('Ctrl Pts',(15.0211077682847,15.1475065810969,4.54452671407416));
#127863=CARTESIAN_POINT('Ctrl Pts',(15.0198854750664,15.1289972334731,4.54184629424673));
#127864=CARTESIAN_POINT('Ctrl Pts',(15.0192588271024,15.1194199769279,4.54060556072871));
#127865=CARTESIAN_POINT('Ctrl Pts',(15.0176273001013,15.0942690734407,4.53772973175266));
#127866=CARTESIAN_POINT('Ctrl Pts',(15.0166296378564,15.0786711503579,4.53632909129133));
#127867=CARTESIAN_POINT('Ctrl Pts',(15.011269537487,14.9938627887962,4.53078662344062));
#127868=CARTESIAN_POINT('Ctrl Pts',(15.0071290071239,14.9243940946235,4.53372002828192));
#127869=CARTESIAN_POINT('Ctrl Pts',(15.0009454308747,14.8230145011772,4.54900936861542));
#127870=CARTESIAN_POINT('Ctrl Pts',(14.9989350347673,14.7904755410969,4.55564504470598));
#127871=CARTESIAN_POINT('Ctrl Pts',(14.9960491627224,14.7455579781982,4.56724107661652));
#127872=CARTESIAN_POINT('Ctrl Pts',(14.9952193504079,14.7328411236088,4.57080354413752));
#127873=CARTESIAN_POINT('Ctrl Pts',(14.9937300057537,14.7104633526326,4.57756973114395));
#127874=CARTESIAN_POINT('Ctrl Pts',(14.9930751978536,14.7007724033555,4.58066768950022));
#127875=CARTESIAN_POINT('Ctrl Pts',(14.9920426312248,14.6857570868489,4.58573027222678));
#127876=CARTESIAN_POINT('Ctrl Pts',(14.9916704730272,14.6803977851802,4.58758991458406));
#127877=CARTESIAN_POINT('Ctrl Pts',(14.9909582270133,14.6702481069535,4.59121217865941));
#127878=CARTESIAN_POINT('Ctrl Pts',(14.9906186381051,14.6654548183314,4.59296574939043));
#127879=CARTESIAN_POINT('Ctrl Pts',(14.9897659496777,14.6535285212784,4.59743624132784));
#127880=CARTESIAN_POINT('Ctrl Pts',(14.9892503045753,14.6464134727812,4.60019980945992));
#127881=CARTESIAN_POINT('Ctrl Pts',(14.9872860892301,14.6196474496576,4.6109625204421));
#127882=CARTESIAN_POINT('Ctrl Pts',(14.985811097909,14.6002300986498,4.61952309002513));
#127883=CARTESIAN_POINT('Ctrl Pts',(14.9802232581377,14.5286638553669,4.65393003468471));
#127884=CARTESIAN_POINT('Ctrl Pts',(14.9760134215237,14.4786005077096,4.68382918436755));
#127885=CARTESIAN_POINT('Ctrl Pts',(14.968652902069,14.3947067747054,4.7448190749534));
#127886=CARTESIAN_POINT('Ctrl Pts',(14.9654782581637,14.3598167515312,4.77415943030465));
#127887=CARTESIAN_POINT('Ctrl Pts',(14.9614817512756,14.3173890120216,4.81528728728529));
#127888=CARTESIAN_POINT('Ctrl Pts',(14.9605735723496,14.3078563922139,4.82492480625402));
#127889=CARTESIAN_POINT('Ctrl Pts',(14.9590603694239,14.2921662457343,4.84146948247668));
#127890=CARTESIAN_POINT('Ctrl Pts',(14.9584508006636,14.2858997376889,4.84827007783757));
#127891=CARTESIAN_POINT('Ctrl Pts',(14.9572340344631,14.2735056373434,4.86211393900355));
#127892=CARTESIAN_POINT('Ctrl Pts',(14.956626978591,14.2673805664822,4.86915813286785));
#127893=CARTESIAN_POINT('Ctrl Pts',(14.9551183803638,14.2523152344109,4.88699957353619));
#127894=CARTESIAN_POINT('Ctrl Pts',(14.9542220666886,14.2435058161574,4.89790481424447));
#127895=CARTESIAN_POINT('Ctrl Pts',(14.950008530195,14.2028438979122,4.9505424864222));
#127896=CARTESIAN_POINT('Ctrl Pts',(14.9468130005764,14.1741869395769,4.99463371501952));
#127897=CARTESIAN_POINT('Ctrl Pts',(14.9407566682124,14.1265046941246,5.08298099063761));
#127898=CARTESIAN_POINT('Ctrl Pts',(14.9378978596329,14.1069237497955,5.1267531216575));
#127899=CARTESIAN_POINT('Ctrl Pts',(14.9334956103003,14.0827088315208,5.19384314020128));
#127900=CARTESIAN_POINT('Ctrl Pts',(14.9320265113891,14.0755555474625,5.21617367668182));
#127901=CARTESIAN_POINT('Ctrl Pts',(14.9300236955881,14.0671460194274,5.24613391511602));
#127902=CARTESIAN_POINT('Ctrl Pts',(14.9295252595741,14.0651589059166,5.25355191618772));
#127903=CARTESIAN_POINT('Ctrl Pts',(14.928683711039,14.0619840548635,5.26599507709466));
#127904=CARTESIAN_POINT('Ctrl Pts',(14.9283432209048,14.0607477792286,5.27100768150966));
#127905=CARTESIAN_POINT('Ctrl Pts',(14.9276236281917,14.0582371400365,5.28154983310003));
#127906=CARTESIAN_POINT('Ctrl Pts',(14.9272441229189,14.0569712273344,5.28708102523874));
#127907=CARTESIAN_POINT('Ctrl Pts',(14.926176787709,14.05357027302,5.30256651822618));
#127908=CARTESIAN_POINT('Ctrl Pts',(14.9254835499426,14.051543739425,5.31254357874149));
#127909=CARTESIAN_POINT('Ctrl Pts',(14.9207115794005,14.0387995091024,5.38079479053979));
#127910=CARTESIAN_POINT('Ctrl Pts',(14.9164398917085,14.033302170455,5.43991149677583));
#127911=CARTESIAN_POINT('Ctrl Pts',(14.9122050445523,14.0332503695571,5.49915469624611));
#127912=CARTESIAN_POINT('Ctrl Pts',(14.8539665810176,14.0332503318545,5.49919897528513));
#127913=CARTESIAN_POINT('Ctrl Pts',(14.8558549326386,14.0332762091239,5.46796792693476));
#127914=CARTESIAN_POINT('Ctrl Pts',(14.8577581847734,14.0348154625899,5.43675845838677));
#127915=CARTESIAN_POINT('Ctrl Pts',(14.8605946150658,14.0392314940276,5.3917112377512));
#127916=CARTESIAN_POINT('Ctrl Pts',(14.8614847410138,14.0409049080245,5.37777423204118));
#127917=CARTESIAN_POINT('Ctrl Pts',(14.8627517596201,14.0436733221221,5.35830839272474));
#127918=CARTESIAN_POINT('Ctrl Pts',(14.8631166435777,14.0445142291266,5.35274456016862));
#127919=CARTESIAN_POINT('Ctrl Pts',(14.8637821071157,14.0461252016181,5.34268099238523));
#127920=CARTESIAN_POINT('Ctrl Pts',(14.8640818186184,14.0468786680796,5.33817872286671));
#127921=CARTESIAN_POINT('Ctrl Pts',(14.8647099688217,14.048514859091,5.32880989749035));
#127922=CARTESIAN_POINT('Ctrl Pts',(14.8650387425845,14.0494030701827,5.3239446190901));
#127923=CARTESIAN_POINT('Ctrl Pts',(14.8657702516262,14.0514497993923,5.31320069712283));
#127924=CARTESIAN_POINT('Ctrl Pts',(14.8661738854635,14.0526257151797,5.30732560453291));
#127925=CARTESIAN_POINT('Ctrl Pts',(14.8675880700547,14.0569091543951,5.28691263633314));
#127926=CARTESIAN_POINT('Ctrl Pts',(14.8686117796016,14.0602971917482,5.27243650363474));
#127927=CARTESIAN_POINT('Ctrl Pts',(14.8735956716226,14.0782115819465,5.20313613859358));
#127928=CARTESIAN_POINT('Ctrl Pts',(14.8776924171568,14.0972093275343,5.14958512720541));
#127929=CARTESIAN_POINT('Ctrl Pts',(14.8853234017605,14.1416662074297,5.05235147699662));
#127930=CARTESIAN_POINT('Ctrl Pts',(14.8888576076852,14.1660695181915,5.00838298236998));
#127931=CARTESIAN_POINT('Ctrl Pts',(14.8924482469444,14.1951529194408,4.96443215744462));
#127932=CARTESIAN_POINT('Ctrl Pts',(14.8926172683426,14.1965321741247,4.96236518896761));
#127933=CARTESIAN_POINT('Ctrl Pts',(14.893120764164,14.2006713364915,4.95621369059276));
#127934=CARTESIAN_POINT('Ctrl Pts',(14.8934544166077,14.2034545619316,4.95214488304287));
#127935=CARTESIAN_POINT('Ctrl Pts',(14.89382996039,14.2066328046397,4.9475740209656));
#127936=CARTESIAN_POINT('Ctrl Pts',(14.8938729491642,14.2069972975998,4.94705092189678));
#127937=CARTESIAN_POINT('Ctrl Pts',(14.8947431350746,14.2143891381514,4.93646492411304));
#127938=CARTESIAN_POINT('Ctrl Pts',(14.8955632878081,14.2216072298334,4.92653602848337));
#127939=CARTESIAN_POINT('Ctrl Pts',(14.8969592621612,14.2343223843272,4.90972819327763));
#127940=CARTESIAN_POINT('Ctrl Pts',(14.8975384804261,14.2397277714504,4.90278214696305));
#127941=CARTESIAN_POINT('Ctrl Pts',(14.898717838094,14.2509967323547,4.88870227065746));
#127942=CARTESIAN_POINT('Ctrl Pts',(14.8993175475896,14.2568691797244,4.88157668026877));
#127943=CARTESIAN_POINT('Ctrl Pts',(14.9008533157214,14.2722677981187,4.8634282310708));
#127944=CARTESIAN_POINT('Ctrl Pts',(14.9017833109925,14.2819428466171,4.85253437608647));
#127945=CARTESIAN_POINT('Ctrl Pts',(14.9075433867644,14.3439653721751,4.78579968115972));
#127946=CARTESIAN_POINT('Ctrl Pts',(14.9120878973818,14.4025421757983,4.73612260574871));
#127947=CARTESIAN_POINT('Ctrl Pts',(14.9185202179851,14.4913208750057,4.67735392864183));
#127948=CARTESIAN_POINT('Ctrl Pts',(14.9203403558027,14.5170251371223,4.6620047304029));
#127949=CARTESIAN_POINT('Ctrl Pts',(14.9233214216175,14.5591543194831,4.63943030916546));
#127950=CARTESIAN_POINT('Ctrl Pts',(14.9244522587349,14.5751407195806,4.63142668193206));
#127951=CARTESIAN_POINT('Ctrl Pts',(14.9260507683635,14.5975689097484,4.62096527824274));
#127952=CARTESIAN_POINT('Ctrl Pts',(14.9264982660378,14.6038298230795,4.61812585432861));
#127953=CARTESIAN_POINT('Ctrl Pts',(14.9272721788027,14.6146148636183,4.61337269141147));
#127954=CARTESIAN_POINT('Ctrl Pts',(14.9275966852868,14.6191242007814,4.61142624836499));
#127955=CARTESIAN_POINT('Ctrl Pts',(14.9283035821782,14.6289158871917,4.60728792616736));
#127956=CARTESIAN_POINT('Ctrl Pts',(14.9286866130523,14.6342029060707,4.60510852746667));
#127957=CARTESIAN_POINT('Ctrl Pts',(14.9297887897135,14.6493722954778,4.59901233268742));
#127958=CARTESIAN_POINT('Ctrl Pts',(14.9305139615139,14.6593000403027,4.5952115832427));
#127959=CARTESIAN_POINT('Ctrl Pts',(14.934158868369,14.7090324736193,4.57710648399116));
#127960=CARTESIAN_POINT('Ctrl Pts',(14.9371745209061,14.7496804682625,4.5652625658698));
#127961=CARTESIAN_POINT('Ctrl Pts',(14.9429112311599,14.8279256677443,4.54793448615564));
#127962=CARTESIAN_POINT('Ctrl Pts',(14.9456253764104,14.8653323927021,4.54192736048103));
#127963=CARTESIAN_POINT('Ctrl Pts',(14.951135891985,14.942939007336,4.53410079947701));
#127964=CARTESIAN_POINT('Ctrl Pts',(14.9539216891916,14.9830979306594,4.53256408050875));
#127965=CARTESIAN_POINT('Ctrl Pts',(14.9575056111915,15.036150698145,4.53383984075792));
#127966=CARTESIAN_POINT('Ctrl Pts',(14.9583699522567,15.0490536486216,4.53440894116425));
#127967=CARTESIAN_POINT('Ctrl Pts',(14.9598175113917,15.0708365814087,4.53580749674134));
#127968=CARTESIAN_POINT('Ctrl Pts',(14.9604047868712,15.0797232129623,4.53650157094055));
#127969=CARTESIAN_POINT('Ctrl Pts',(14.9615816840999,15.09762498287,4.53814913865886));
#127970=CARTESIAN_POINT('Ctrl Pts',(14.9621711181229,15.1066388471809,4.53910672698923));
#127971=CARTESIAN_POINT('Ctrl Pts',(14.9636426450116,15.1292510942968,4.54183105936492));
#127972=CARTESIAN_POINT('Ctrl Pts',(14.9645196651774,15.1428280879056,4.54376063091443));
#127973=CARTESIAN_POINT('Ctrl Pts',(14.9686771474817,15.2075664959849,4.55437097514698));
#127974=CARTESIAN_POINT('Ctrl Pts',(14.9718380269747,15.258016882701,4.56687285525153));
#127975=CARTESIAN_POINT('Ctrl Pts',(14.9773168223527,15.3441311709988,4.59573543590412));
#127976=CARTESIAN_POINT('Ctrl Pts',(14.979644635833,15.3802558777713,4.61032254342958));
#127977=CARTESIAN_POINT('Ctrl Pts',(14.9839861422621,15.4445451444208,4.64091511863044));
#127978=CARTESIAN_POINT('Ctrl Pts',(14.9859832988042,15.4729728670161,4.65623257557793));
#127979=CARTESIAN_POINT('Ctrl Pts',(14.98858287211,15.5076312366802,4.67720959325779));
#127980=CARTESIAN_POINT('Ctrl Pts',(14.9891165686507,15.5146288374633,4.68156816124849));
#127981=CARTESIAN_POINT('Ctrl Pts',(14.9899929972897,15.5259113205249,4.68879753698097));
#127982=CARTESIAN_POINT('Ctrl Pts',(14.9903323911074,15.5302306453159,4.69161419281713));
#127983=CARTESIAN_POINT('Ctrl Pts',(14.9910201754643,15.5388786346381,4.69735272189946));
#127984=CARTESIAN_POINT('Ctrl Pts',(14.9913686041748,15.5432065504057,4.7002753746579));
#127985=CARTESIAN_POINT('Ctrl Pts',(14.9922934473557,15.5545605967957,4.70807747736854));
#127986=CARTESIAN_POINT('Ctrl Pts',(14.9928734340796,15.5615458428177,4.71301525328606));
#127987=CARTESIAN_POINT('Ctrl Pts',(14.9959086467107,15.5974523716931,4.73911851733851));
#127988=CARTESIAN_POINT('Ctrl Pts',(14.9984409206017,15.6252434408736,4.7617858653979));
#127989=CARTESIAN_POINT('Ctrl Pts',(15.0051685527126,15.6949028932764,4.82536283210728));
#127990=CARTESIAN_POINT('Ctrl Pts',(15.0093832253419,15.7344342735321,4.8686264048768));
#127991=CARTESIAN_POINT('Ctrl Pts',(15.0149946989902,15.7829243606754,4.93245728888567));
#127992=CARTESIAN_POINT('Ctrl Pts',(15.0164950713777,15.7954513642682,4.95015227267371));
#127993=CARTESIAN_POINT('Ctrl Pts',(15.0191426873818,15.8167800563305,4.98253661041792));
#127994=CARTESIAN_POINT('Ctrl Pts',(15.0202972161193,15.8258062453848,4.99706647843543));
#127995=CARTESIAN_POINT('Ctrl Pts',(15.022087731005,15.839361098514,5.02023612097309));
#127996=CARTESIAN_POINT('Ctrl Pts',(15.0227328918443,15.8441523102461,5.02871736499166));
#127997=CARTESIAN_POINT('Ctrl Pts',(15.0239415550327,15.8529481199525,5.04485206504839));
#127998=CARTESIAN_POINT('Ctrl Pts',(15.0245059636964,15.8569798869569,5.05248953158339));
#127999=CARTESIAN_POINT('Ctrl Pts',(15.0257871429126,15.8659538671048,5.07005531497917));
#128000=CARTESIAN_POINT('Ctrl Pts',(15.0265015513066,15.8708287222622,5.08001680419696));
#128001=CARTESIAN_POINT('Ctrl Pts',(15.0287868868942,15.8859878561271,5.11239301889865));
#128002=CARTESIAN_POINT('Ctrl Pts',(15.0303350964681,15.8955867052198,5.135118845976));
#128003=CARTESIAN_POINT('Ctrl Pts',(15.0366258561397,15.9315041825646,5.23014315551879));
#128004=CARTESIAN_POINT('Ctrl Pts',(15.0411387039992,15.9500153359253,5.30508204924268));
#128005=CARTESIAN_POINT('Ctrl Pts',(15.0475893202087,15.9629298487889,5.40957597345322));
#128006=CARTESIAN_POINT('Ctrl Pts',(15.0493543222572,15.9651682519459,5.43786835121357));
#128007=CARTESIAN_POINT('Ctrl Pts',(15.0516888492181,15.9664381607476,5.47418465962399));
#128008=CARTESIAN_POINT('Ctrl Pts',(15.052205584009,15.9666182087185,5.48215682133561));
#128009=CARTESIAN_POINT('Ctrl Pts',(15.053061313484,15.9667516940837,5.49523078718063));
#128010=CARTESIAN_POINT('Ctrl Pts',(15.0533972665399,15.9667633999231,5.50033182378754));
#128011=CARTESIAN_POINT('Ctrl Pts',(15.0540862309273,15.9667050099805,5.5107222964774));
#128012=CARTESIAN_POINT('Ctrl Pts',(15.0544393745736,15.9666318706065,5.5160114787546));
#128013=CARTESIAN_POINT('Ctrl Pts',(15.0553906227592,15.9663198904836,5.53016822416586));
#128014=CARTESIAN_POINT('Ctrl Pts',(15.0559926520036,15.9660024009317,5.5390333238352));
#128015=CARTESIAN_POINT('Ctrl Pts',(15.0599378396757,15.9631472154489,5.59659696446058));
#128016=CARTESIAN_POINT('Ctrl Pts',(15.063422369787,15.9570500258061,5.64504441845719));
#128017=CARTESIAN_POINT('Ctrl Pts',(15.070197412373,15.9381798347286,5.73775374878803));
#128018=CARTESIAN_POINT('Ctrl Pts',(15.0734786383384,15.9258479260395,5.78198307317516));
#128019=CARTESIAN_POINT('Ctrl Pts',(15.0788652705024,15.8999424193179,5.85451366478185));
#128020=CARTESIAN_POINT('Ctrl Pts',(15.0810082591409,15.8880495797593,5.88333352566741));
#128021=CARTESIAN_POINT('Ctrl Pts',(15.0839142169799,15.8696781507091,5.9223853191918));
#128022=CARTESIAN_POINT('Ctrl Pts',(15.0847151318455,15.8643702865876,5.93314370950165));
#128023=CARTESIAN_POINT('Ctrl Pts',(15.0860888627734,15.8548439365061,5.95157952656161));
#128024=CARTESIAN_POINT('Ctrl Pts',(15.086664795789,15.8507189134806,5.95930334555372));
#128025=CARTESIAN_POINT('Ctrl Pts',(15.0878466013729,15.8419852658515,5.97513506042166));
#128026=CARTESIAN_POINT('Ctrl Pts',(15.0884519249566,15.837363103714,5.98323447305798));
#128027=CARTESIAN_POINT('Ctrl Pts',(15.0900222162392,15.8249885746461,6.00420749910005));
#128028=CARTESIAN_POINT('Ctrl Pts',(15.0909805645968,15.8170518170708,6.01696974465591));
#128029=CARTESIAN_POINT('Ctrl Pts',(15.0965547845518,15.768699680378,6.09082256474307));
#128030=CARTESIAN_POINT('Ctrl Pts',(15.1009149472164,15.721745201398,6.14734487463986));
#128031=CARTESIAN_POINT('Ctrl Pts',(15.1072382475006,15.6460911361247,6.21983729270203));
#128032=CARTESIAN_POINT('Ctrl Pts',(15.1091517538356,15.6222759664719,6.24052134374049));
#128033=CARTESIAN_POINT('Ctrl Pts',(15.1122655312471,15.5829793705503,6.27141527928985));
#128034=CARTESIAN_POINT('Ctrl Pts',(15.1134323329086,15.5681411528647,6.28240782978899));
#128035=CARTESIAN_POINT('Ctrl Pts',(15.11507326176,15.547294198884,6.29694603670392));
#128036=CARTESIAN_POINT('Ctrl Pts',(15.1155257784418,15.541547393456,6.30086224746086));
#128037=CARTESIAN_POINT('Ctrl Pts',(15.1163053944488,15.5316618215477,6.30744380501268));
#128038=CARTESIAN_POINT('Ctrl Pts',(15.1166305044437,15.5275440873005,6.31014012715346));
#128039=CARTESIAN_POINT('Ctrl Pts',(15.1173350462375,15.5186341185695,6.31587770147371));
#128040=CARTESIAN_POINT('Ctrl Pts',(15.1177150697724,15.5138356432399,6.31890823693493));
#128041=CARTESIAN_POINT('Ctrl Pts',(15.1188001964196,15.5001473534116,6.32738557071843));
#128042=CARTESIAN_POINT('Ctrl Pts',(15.1195110558699,15.4911959980626,6.332730885825));
#128043=CARTESIAN_POINT('Ctrl Pts',(15.1237309887301,15.4380533847637,6.36331012224213));
#128044=CARTESIAN_POINT('Ctrl Pts',(15.1273810804493,15.3920148235246,6.38516591382389));
#128045=CARTESIAN_POINT('Ctrl Pts',(15.1342575143636,15.3022907154883,6.41938248701817));
#128046=CARTESIAN_POINT('Ctrl Pts',(15.1374773849574,15.2590283907437,6.43249599343638));
#128047=CARTESIAN_POINT('Ctrl Pts',(15.1425611810656,15.187837164456,6.44873560615895));
#128048=CARTESIAN_POINT('Ctrl Pts',(15.1444708147778,15.1604122611922,6.45375584555286));
#128049=CARTESIAN_POINT('Ctrl Pts',(15.1471220787523,15.1213517888635,6.45917310057196));
#128050=CARTESIAN_POINT('Ctrl Pts',(15.1478932630662,15.1098692356007,6.46055612229073));
#128051=CARTESIAN_POINT('Ctrl Pts',(15.1492330095174,15.0897167969318,6.46261727527569));
#128052=CARTESIAN_POINT('Ctrl Pts',(15.149804264225,15.0810576332602,6.46338506870814));
#128053=CARTESIAN_POINT('Ctrl Pts',(15.1509921116202,15.0629195479231,6.46474704979121));
#128054=CARTESIAN_POINT('Ctrl Pts',(15.1516079489227,15.0534398217715,6.46531856680731));
#128055=CARTESIAN_POINT('Ctrl Pts',(15.1532424665448,15.0280905710061,6.46647225414388));
#128056=CARTESIAN_POINT('Ctrl Pts',(15.154253446412,15.012212181767,6.46680329202504));
#128057=CARTESIAN_POINT('Ctrl Pts',(15.1609027458769,14.9066879660855,6.4664029256953));
#128058=CARTESIAN_POINT('Ctrl Pts',(15.1661386762117,14.8175337566911,6.45359706158965));
#128059=CARTESIAN_POINT('Ctrl Pts',(15.1734339440527,14.7029615484193,6.42046258289272));
#128060=CARTESIAN_POINT('Ctrl Pts',(15.1752738000915,14.6748986871526,6.41092919993062));
#128061=CARTESIAN_POINT('Ctrl Pts',(15.1776939620517,14.6398088291808,6.39718056825162));
#128062=CARTESIAN_POINT('Ctrl Pts',(15.1782165817196,14.6323344928509,6.39414356577471));
#128063=CARTESIAN_POINT('Ctrl Pts',(15.179079474914,14.6201803554466,6.38902689245148));
#128064=CARTESIAN_POINT('Ctrl Pts',(15.1794166047572,14.6154773288351,6.38700286987054));
#128065=CARTESIAN_POINT('Ctrl Pts',(15.1800620274693,14.6065652712186,6.38308322626607));
#128066=CARTESIAN_POINT('Ctrl Pts',(15.180369868567,14.602353321299,6.3811946363177));
#128067=CARTESIAN_POINT('Ctrl Pts',(15.1812209518324,14.5908101304022,6.37591919196636));
#128068=CARTESIAN_POINT('Ctrl Pts',(15.1817676460518,14.583507734283,6.37247060833897));
#128069=CARTESIAN_POINT('Ctrl Pts',(15.1841737987554,14.5518183394844,6.35701668932205));
#128070=CARTESIAN_POINT('Ctrl Pts',(15.1860774848475,14.5279024098573,6.34407820156081));
#128071=CARTESIAN_POINT('Ctrl Pts',(15.1926762531006,14.447954088701,6.29636499799892));
#128072=CARTESIAN_POINT('Ctrl Pts',(15.1974512250076,14.3949414675465,6.25687327661972));
#128073=CARTESIAN_POINT('Ctrl Pts',(15.2044301543389,14.3216413202208,6.18960909714398));
#128074=CARTESIAN_POINT('Ctrl Pts',(15.2067435746684,14.2981170208507,6.1656515019892));
#128075=CARTESIAN_POINT('Ctrl Pts',(15.2098325211374,14.2677512615314,6.13132243708263));
#128076=CARTESIAN_POINT('Ctrl Pts',(15.2106527486208,14.2597941505056,6.12197392083528));
#128077=CARTESIAN_POINT('Ctrl Pts',(15.2120488059361,14.24644116107,6.1056666537016));
#128078=CARTESIAN_POINT('Ctrl Pts',(15.2126280335836,14.2409584965958,6.09878128209072));
#128079=CARTESIAN_POINT('Ctrl Pts',(15.2137350816395,14.2305952992747,6.08539560753445));
#128080=CARTESIAN_POINT('Ctrl Pts',(15.2142633955932,14.2257012441749,6.07890677496729));
#128081=CARTESIAN_POINT('Ctrl Pts',(15.2156629134787,14.2128807085597,6.06145504961809));
#128082=CARTESIAN_POINT('Ctrl Pts',(15.2165285376058,14.2051013532032,6.05038597494936));
#128083=CARTESIAN_POINT('Ctrl Pts',(15.2202744839761,14.1721541455819,6.00134964794791));
#128084=CARTESIAN_POINT('Ctrl Pts',(15.2230656553926,14.1494538634748,5.96179234756547));
#128085=CARTESIAN_POINT('Ctrl Pts',(15.2287015850314,14.10891463461,5.8779374158332));
#128086=CARTESIAN_POINT('Ctrl Pts',(15.2315357052326,14.091395533674,5.83362776174672));
#128087=CARTESIAN_POINT('Ctrl Pts',(15.236310394775,14.0680976172899,5.75903257109432));
#128088=CARTESIAN_POINT('Ctrl Pts',(15.2382062936243,14.0603746270103,5.72944218633089));
#128089=CARTESIAN_POINT('Ctrl Pts',(15.2406904548279,14.0523879097482,5.6915803885933));
#128090=CARTESIAN_POINT('Ctrl Pts',(15.2412172162665,14.0508096788004,5.68360131419087));
#128091=CARTESIAN_POINT('Ctrl Pts',(15.2420851632927,14.048399878698,5.67055534588784));
#128092=CARTESIAN_POINT('Ctrl Pts',(15.2424231328278,14.0475076319733,5.66549985939347));
#128093=CARTESIAN_POINT('Ctrl Pts',(15.2431112989799,14.0457846563646,5.65526168066202));
#128094=CARTESIAN_POINT('Ctrl Pts',(15.2434615711857,14.0449557938717,5.6500788881891));
#128095=CARTESIAN_POINT('Ctrl Pts',(15.2443967277159,14.0428686250736,5.63630993516556));
#128096=CARTESIAN_POINT('Ctrl Pts',(15.2449853205082,14.0416836874877,5.62771334991782));
#128097=CARTESIAN_POINT('Ctrl Pts',(15.2482857692243,14.0357394374377,5.5798316231963));
#128098=CARTESIAN_POINT('Ctrl Pts',(15.2510914423754,14.0332804794478,5.54030229138642));
#128099=CARTESIAN_POINT('Ctrl Pts',(15.2539186841775,14.0332502815961,5.50073787940146));
#128100=CARTESIAN_POINT('Origin',(16.125,15.,5.5));
#128101=CARTESIAN_POINT('',(15.7122357911024,14.0332500106539,5.50014352462477));
#128102=CARTESIAN_POINT('',(15.6551382358657,14.0332501289961,5.49997318520408));
#128103=CARTESIAN_POINT('',(16.125,14.03325,5.5));
#128104=CARTESIAN_POINT('Ctrl Pts',(15.7122357911024,14.0332500106539,5.50014352462477));
#128105=CARTESIAN_POINT('Ctrl Pts',(15.7094099671659,14.0332564146756,5.5432795924672));
#128106=CARTESIAN_POINT('Ctrl Pts',(15.7065841432294,14.0361541789593,5.58634795534859));
#128107=CARTESIAN_POINT('Ctrl Pts',(15.7037583192929,14.0418907006428,5.62896562714666));
#128108=CARTESIAN_POINT('Ctrl Pts',(15.7009265505009,14.0476392905914,5.67167295629949));
#128109=CARTESIAN_POINT('Ctrl Pts',(15.698094781709,14.0562384428576,5.71392724228728));
#128110=CARTESIAN_POINT('Ctrl Pts',(15.695263012917,14.0675847152264,5.75535719927296));
#128111=CARTESIAN_POINT('Ctrl Pts',(15.6924211308671,14.0789715091871,5.79693511743532));
#128112=CARTESIAN_POINT('Ctrl Pts',(15.6895792488172,14.0931248786537,5.83768237429134));
#128113=CARTESIAN_POINT('Ctrl Pts',(15.6867373667672,14.1098920983802,5.87724459701101));
#128114=CARTESIAN_POINT('Ctrl Pts',(15.6853373489891,14.1181522602357,5.89673443303386));
#128115=CARTESIAN_POINT('Ctrl Pts',(15.683937331211,14.1270460641763,5.91593703186562));
#128116=CARTESIAN_POINT('Ctrl Pts',(15.6825373134329,14.1365512304826,5.93481235598685));
#128117=CARTESIAN_POINT('Ctrl Pts',(15.679865827169,14.1546888010333,5.97082987655267));
#128118=CARTESIAN_POINT('Ctrl Pts',(15.6771943409051,14.1751255833383,6.00579345392184));
#128119=CARTESIAN_POINT('Ctrl Pts',(15.6745228546412,14.1977155281612,6.03939335252336));
#128120=CARTESIAN_POINT('Ctrl Pts',(15.6718553725082,14.2202716142683,6.07294289024849));
#128121=CARTESIAN_POINT('Ctrl Pts',(15.6691878903751,14.2449741607053,6.10513230764752));
#128122=CARTESIAN_POINT('Ctrl Pts',(15.6665204082421,14.2716314227655,6.13567663021175));
#128123=CARTESIAN_POINT('Ctrl Pts',(15.6638556317917,14.2982616458102,6.1661899710342));
#128124=CARTESIAN_POINT('Ctrl Pts',(15.6611908553412,14.3268422802672,6.19506107808628));
#128125=CARTESIAN_POINT('Ctrl Pts',(15.6585260788908,14.3571403207815,6.22203669943783));
#128126=CARTESIAN_POINT('Ctrl Pts',(15.6558627144059,14.3874223074955,6.24899802741495));
#128127=CARTESIAN_POINT('Ctrl Pts',(15.653199349921,14.4194194621698,6.2740654698766));
#128128=CARTESIAN_POINT('Ctrl Pts',(15.6505359854361,14.4528630279837,6.29702364855303));
#128129=CARTESIAN_POINT('Ctrl Pts',(15.6478706894586,14.4863308473314,6.3199984766791));
#128130=CARTESIAN_POINT('Ctrl Pts',(15.6452053934811,14.5212466954558,6.34086064546375));
#128131=CARTESIAN_POINT('Ctrl Pts',(15.6425400975035,14.5573117999295,6.35943744392386));
#128132=CARTESIAN_POINT('Ctrl Pts',(15.6398739707978,14.5933881452929,6.37802003246119));
#128133=CARTESIAN_POINT('Ctrl Pts',(15.6372078440922,14.6306139278099,6.39431558677765));
#128134=CARTESIAN_POINT('Ctrl Pts',(15.6345417173865,14.6686683079245,6.40819869650116));
#128135=CARTESIAN_POINT('Ctrl Pts',(15.6318701892867,14.7067997836646,6.42210993247515));
#128136=CARTESIAN_POINT('Ctrl Pts',(15.6291986611868,14.7457626493866,6.43359878644248));
#128137=CARTESIAN_POINT('Ctrl Pts',(15.626527133087,14.785220543638,6.44258970269405));
#128138=CARTESIAN_POINT('Ctrl Pts',(15.6242183374809,14.8193209571353,6.45035985788643));
#128139=CARTESIAN_POINT('Ctrl Pts',(15.6219095418748,14.8537906613752,6.45626514772572));
#128140=CARTESIAN_POINT('Ctrl Pts',(15.6196007462687,14.8884094044249,6.46028803047794));
#128141=CARTESIAN_POINT('Ctrl Pts',(15.6169292600077,14.9284664351057,6.46494287128482));
#128142=CARTESIAN_POINT('Ctrl Pts',(15.6142577737468,14.9689073831686,6.46709775641789));
#128143=CARTESIAN_POINT('Ctrl Pts',(15.6115862874858,15.0093932329593,6.46670436518854));
#128144=CARTESIAN_POINT('Ctrl Pts',(15.6089188053556,15.0498184009337,6.46631156358975));
#128145=CARTESIAN_POINT('Ctrl Pts',(15.6062513232255,15.0902877576254,6.46337804032544));
#128146=CARTESIAN_POINT('Ctrl Pts',(15.6035838410953,15.1304578434037,6.45790725730336));
#128147=CARTESIAN_POINT('Ctrl Pts',(15.6009190646478,15.1705871838286,6.45244202341028));
#128148=CARTESIAN_POINT('Ctrl Pts',(15.5982542882002,15.210417276379,6.44444469806571));
#128149=CARTESIAN_POINT('Ctrl Pts',(15.5955895117527,15.2496084706341,6.43397064937166));
#128150=CARTESIAN_POINT('Ctrl Pts',(15.5929261472706,15.2887788989391,6.42350215048481));
#128151=CARTESIAN_POINT('Ctrl Pts',(15.5902627827886,15.3273105348896,6.41055967751139));
#128152=CARTESIAN_POINT('Ctrl Pts',(15.5875994183065,15.3648757042798,6.39524928535371));
#128153=CARTESIAN_POINT('Ctrl Pts',(15.5849341223318,15.4024681162237,6.37992778998027));
#128154=CARTESIAN_POINT('Ctrl Pts',(15.5822688263571,15.4390921149018,6.36223515721037));
#128155=CARTESIAN_POINT('Ctrl Pts',(15.5796035303823,15.4744391601403,6.34232597361434));
#128156=CARTESIAN_POINT('Ctrl Pts',(15.5769374036794,15.5097972224617,6.32241058465871));
#128157=CARTESIAN_POINT('Ctrl Pts',(15.5742712769765,15.5438770409738,6.30027757895607));
#128158=CARTESIAN_POINT('Ctrl Pts',(15.5716051502736,15.5763974500778,6.27612598335827));
#128159=CARTESIAN_POINT('Ctrl Pts',(15.5689336221764,15.6089837433537,6.2519254582445));
#128160=CARTESIAN_POINT('Ctrl Pts',(15.5662620940793,15.6400038623056,6.22569854672883));
#128161=CARTESIAN_POINT('Ctrl Pts',(15.5635905659821,15.6692097481378,6.1976846533337));
#128162=CARTESIAN_POINT('Ctrl Pts',(15.5612817703563,15.6944501420275,6.1734744065451));
#128163=CARTESIAN_POINT('Ctrl Pts',(15.5589729747304,15.7183359451346,6.14793029980389));
#128164=CARTESIAN_POINT('Ctrl Pts',(15.5566641791045,15.7407313988466,6.12122665530606));
#128165=CARTESIAN_POINT('Ctrl Pts',(15.5539926928445,15.7666449730963,6.09032811297994));
#128166=CARTESIAN_POINT('Ctrl Pts',(15.5513212065844,15.7906815336472,6.05773428587259));
#128167=CARTESIAN_POINT('Ctrl Pts',(15.5486497203244,15.8126143105961,6.02370177077642));
#128168=CARTESIAN_POINT('Ctrl Pts',(15.5459822381952,15.8345142138186,5.98972026498004));
#128169=CARTESIAN_POINT('Ctrl Pts',(15.543314756066,15.854316251522,5.95430482073426));
#128170=CARTESIAN_POINT('Ctrl Pts',(15.5406472739369,15.8718344621854,5.91774421964397));
#128171=CARTESIAN_POINT('Ctrl Pts',(15.5379824974903,15.8893349037631,5.88122070273224));
#128172=CARTESIAN_POINT('Ctrl Pts',(15.5353177210438,15.904555847848,5.84355485155328));
#128173=CARTESIAN_POINT('Ctrl Pts',(15.5326529445972,15.9173567825961,5.80506080693013));
#128174=CARTESIAN_POINT('Ctrl Pts',(15.5299895801162,15.9301509346069,5.76658715886398));
#128175=CARTESIAN_POINT('Ctrl Pts',(15.5273262156352,15.940527431882,5.72728674056244));
#128176=CARTESIAN_POINT('Ctrl Pts',(15.5246628511542,15.9483946844153,5.68749156000431));
#128177=CARTESIAN_POINT('Ctrl Pts',(15.5219975551806,15.9562676423413,5.64766751967154));
#128178=CARTESIAN_POINT('Ctrl Pts',(15.5193322592069,15.9616275970754,5.6073485735361));
#128179=CARTESIAN_POINT('Ctrl Pts',(15.5166669632333,15.9644340161173,5.56687743308424));
#128180=CARTESIAN_POINT('Ctrl Pts',(15.5140008365315,15.9672413098729,5.52639367845503));
#128181=CARTESIAN_POINT('Ctrl Pts',(15.5113347098296,15.9674934680987,5.48575822120119));
#128182=CARTESIAN_POINT('Ctrl Pts',(15.5086685831278,15.9652021295355,5.44531534365053));
#128183=CARTESIAN_POINT('Ctrl Pts',(15.5059970550318,15.9629061488739,5.40479053153749));
#128184=CARTESIAN_POINT('Ctrl Pts',(15.5033255269358,15.9580564395887,5.3644596626397));
#128185=CARTESIAN_POINT('Ctrl Pts',(15.5006539988398,15.9507165702229,5.32466156837791));
#128186=CARTESIAN_POINT('Ctrl Pts',(15.4983452032066,15.9443732873784,5.29026714580888));
#128187=CARTESIAN_POINT('Ctrl Pts',(15.4960364075735,15.9361710558104,5.25627072857965));
#128188=CARTESIAN_POINT('Ctrl Pts',(15.4937276119403,15.9261808322606,5.2228815624086));
#128189=CARTESIAN_POINT('Ctrl Pts',(15.4910561256672,15.9146212361253,5.18424726415616));
#128190=CARTESIAN_POINT('Ctrl Pts',(15.4883846393942,15.9006135505576,5.1462485987931));
#128191=CARTESIAN_POINT('Ctrl Pts',(15.4857131531211,15.884247409928,5.10921606924586));
#128192=CARTESIAN_POINT('Ctrl Pts',(15.4830456709788,15.8679057995266,5.07223904553962));
#128193=CARTESIAN_POINT('Ctrl Pts',(15.4803781888366,15.8492129552526,5.03622582607153));
#128194=CARTESIAN_POINT('Ctrl Pts',(15.4777107066943,15.8283078328668,5.00149052515366));
#128195=CARTESIAN_POINT('Ctrl Pts',(15.4750459302346,15.8074239149815,4.96679045697406));
#128196=CARTESIAN_POINT('Ctrl Pts',(15.472381153775,15.7843324571946,4.93336624305674));
#128197=CARTESIAN_POINT('Ctrl Pts',(15.4697163773154,15.7592185875527,4.90150797932261));
#128198=CARTESIAN_POINT('Ctrl Pts',(15.4670530128213,15.7341180248127,4.86966659609304));
#128199=CARTESIAN_POINT('Ctrl Pts',(15.4643896483272,15.706997533657,4.83938997890157));
#128200=CARTESIAN_POINT('Ctrl Pts',(15.4617262838331,15.6780840657846,4.81093718557081));
#128201=CARTESIAN_POINT('Ctrl Pts',(15.4590609878465,15.6491496296419,4.78246375805457));
#128202=CARTESIAN_POINT('Ctrl Pts',(15.4563956918599,15.6184200302807,4.75581721475183));
#128203=CARTESIAN_POINT('Ctrl Pts',(15.4537303958733,15.5861592338527,4.73121985257867));
#128204=CARTESIAN_POINT('Ctrl Pts',(15.4510642691587,15.5538883822751,4.70661482381985));
#128205=CARTESIAN_POINT('Ctrl Pts',(15.448398142444,15.5200858646421,4.68406058283007));
#128206=CARTESIAN_POINT('Ctrl Pts',(15.4457320157293,15.4850456458025,4.66373671371512));
#128207=CARTESIAN_POINT('Ctrl Pts',(15.4430604876207,15.4499344378296,4.64337166980436));
#128208=CARTESIAN_POINT('Ctrl Pts',(15.4403889595121,15.4135810415084,4.62524629374348));
#128209=CARTESIAN_POINT('Ctrl Pts',(15.4377174314035,15.3763034226429,4.609493797547));
#128210=CARTESIAN_POINT('Ctrl Pts',(15.435408635861,15.3440872539292,4.5958801309403));
#128211=CARTESIAN_POINT('Ctrl Pts',(15.4330998403186,15.3111813702823,4.5840380148832));
#128212=CARTESIAN_POINT('Ctrl Pts',(15.4307910447761,15.2777995621772,4.57402323692537));
#128213=CARTESIAN_POINT('Ctrl Pts',(15.4281195585274,15.2391737767107,4.56243522876013));
#128214=CARTESIAN_POINT('Ctrl Pts',(15.4254480722788,15.1997328148548,4.55324151762621));
#128215=CARTESIAN_POINT('Ctrl Pts',(15.4227765860301,15.1598020183826,4.54654896432965));
#128216=CARTESIAN_POINT('Ctrl Pts',(15.4201091039122,15.1199310717899,4.53986644210044));
#128217=CARTESIAN_POINT('Ctrl Pts',(15.4174416217942,15.0795723137171,4.53567776410846));
#128218=CARTESIAN_POINT('Ctrl Pts',(15.4147741396763,15.0390645168156,4.5340395836133));
#128219=CARTESIAN_POINT('Ctrl Pts',(15.4121093632409,14.9985978078139,4.53240306475864));
#128220=CARTESIAN_POINT('Ctrl Pts',(15.4094445868055,14.9579829410967,4.53331195070426));
#128221=CARTESIAN_POINT('Ctrl Pts',(15.4067798103701,14.9175640157947,4.53677112221025));
#128222=CARTESIAN_POINT('Ctrl Pts',(15.4041164459001,14.87716650697,4.54022846083059));
#128223=CARTESIAN_POINT('Ctrl Pts',(15.4014530814301,14.836965316024,4.54623335958583));
#128224=CARTESIAN_POINT('Ctrl Pts',(15.3987897169601,14.7973016141674,4.55473869915201));
#128225=CARTESIAN_POINT('Ctrl Pts',(15.3961244209971,14.7576091478806,4.56325020685768));
#128226=CARTESIAN_POINT('Ctrl Pts',(15.3934591250342,14.7184555246137,4.57426566442385));
#128227=CARTESIAN_POINT('Ctrl Pts',(15.3907938290712,14.680171563261,4.58768682265733));
#128228=CARTESIAN_POINT('Ctrl Pts',(15.3881277023799,14.6418756694357,4.60111216404211));
#128229=CARTESIAN_POINT('Ctrl Pts',(15.3854615756886,14.6044505216104,4.61694448124139));
#128230=CARTESIAN_POINT('Ctrl Pts',(15.3827954489973,14.5682077573255,4.63503698248647));
#128231=CARTESIAN_POINT('Ctrl Pts',(15.3801239209114,14.5318915676205,4.6531661379308));
#128232=CARTESIAN_POINT('Ctrl Pts',(15.3774523928255,14.4967630587329,4.67356433679313));
#128233=CARTESIAN_POINT('Ctrl Pts',(15.3747808647396,14.4631083325078,4.69603924232742));
#128234=CARTESIAN_POINT('Ctrl Pts',(15.3724720690303,14.4340231479225,4.71546257002381));
#128235=CARTESIAN_POINT('Ctrl Pts',(15.3701632733211,14.4060384251854,4.73643608570972));
#128236=CARTESIAN_POINT('Ctrl Pts',(15.3678544776119,14.37931831527,4.75881189382131));
#128237=CARTESIAN_POINT('Ctrl Pts',(15.3652184319464,14.3488108824808,4.7843592611125));
#128238=CARTESIAN_POINT('Ctrl Pts',(15.362582386281,14.3198040591793,4.81186000691865));
#128239=CARTESIAN_POINT('Ctrl Pts',(15.3599463406155,14.2925623556372,4.84110885433293));
#128240=CARTESIAN_POINT('Ctrl Pts',(15.3573142732769,14.2653617653438,4.87031355931191));
#128241=CARTESIAN_POINT('Ctrl Pts',(15.3546822059383,14.2399214422276,4.90126072057937));
#128242=CARTESIAN_POINT('Ctrl Pts',(15.3520501385997,14.216471745972,4.93370587356051));
#128243=CARTESIAN_POINT('Ctrl Pts',(15.3494206841004,14.1930453281058,4.96611881840993));
#128244=CARTESIAN_POINT('Ctrl Pts',(15.3467912296011,14.1716059838233,5.00002633051279));
#128245=CARTESIAN_POINT('Ctrl Pts',(15.3441617751018,14.1523439514045,5.03515079242886));
#128246=CARTESIAN_POINT('Ctrl Pts',(15.3415013288499,14.1328548893326,5.07068924463591));
#128247=CARTESIAN_POINT('Ctrl Pts',(15.3388408825981,14.1155951837442,5.10747301979994));
#128248=CARTESIAN_POINT('Ctrl Pts',(15.3361804363462,14.100715181879,5.14518684015803));
#128249=CARTESIAN_POINT('Ctrl Pts',(15.3335506383373,14.086006597088,5.1824661986926));
#128250=CARTESIAN_POINT('Ctrl Pts',(15.3309208403284,14.0736233230897,5.22065368630612));
#128251=CARTESIAN_POINT('Ctrl Pts',(15.3282910423195,14.0636614816181,5.25942622442494));
#128252=CARTESIAN_POINT('Ctrl Pts',(15.3256152719462,14.0535254939173,5.29887655804275));
#128253=CARTESIAN_POINT('Ctrl Pts',(15.3229395015728,14.0458966007295,5.33893197443122));
#128254=CARTESIAN_POINT('Ctrl Pts',(15.3202637311995,14.0408216861288,5.37924187522471));
#128255=CARTESIAN_POINT('Ctrl Pts',(15.3175879608261,14.0357467715282,5.4195517760182));
#128256=CARTESIAN_POINT('Ctrl Pts',(15.3149121904528,14.0332258206287,5.46011550819873));
#128257=CARTESIAN_POINT('Ctrl Pts',(15.3122364200794,14.0332501750868,5.50058183360759));
#128258=CARTESIAN_POINT('Ctrl Pts',(15.2539186841775,14.0332502815961,5.50073787940146));
#128259=CARTESIAN_POINT('Ctrl Pts',(15.2595175253243,14.0331904802114,5.42238771578732));
#128260=CARTESIAN_POINT('Ctrl Pts',(15.2651438586834,14.0426560102427,5.34430511256021));
#128261=CARTESIAN_POINT('Ctrl Pts',(15.271565093549,14.0652663824751,5.25275041137276));
#128262=CARTESIAN_POINT('Ctrl Pts',(15.2726381794736,14.0694672655116,5.23738207371249));
#128263=CARTESIAN_POINT('Ctrl Pts',(15.2743325847113,14.0767786539322,5.21301868091487));
#128264=CARTESIAN_POINT('Ctrl Pts',(15.2749614962956,14.0796452960216,5.20395412346234));
#128265=CARTESIAN_POINT('Ctrl Pts',(15.2761570694372,14.085387311679,5.18668753596458));
#128266=CARTESIAN_POINT('Ctrl Pts',(15.276724379512,14.0882404775814,5.1784791590938));
#128267=CARTESIAN_POINT('Ctrl Pts',(15.27803698782,14.0951400850736,5.15946026762035));
#128268=CARTESIAN_POINT('Ctrl Pts',(15.2787794827675,14.0992702753139,5.14868140367013));
#128269=CARTESIAN_POINT('Ctrl Pts',(15.2812841727986,14.1139675115272,5.11228931581595));
#128270=CARTESIAN_POINT('Ctrl Pts',(15.2830167148293,14.1254424768501,5.08705631314722));
#128271=CARTESIAN_POINT('Ctrl Pts',(15.2874793866644,14.1582192186663,5.02249798807187));
#128272=CARTESIAN_POINT('Ctrl Pts',(15.2901626456772,14.1811919509576,4.98409622350412));
#128273=CARTESIAN_POINT('Ctrl Pts',(15.2959559396889,14.2361896734283,4.90514370521323));
#128274=CARTESIAN_POINT('Ctrl Pts',(15.2990594701861,14.2689690534642,4.8652931613692));
#128275=CARTESIAN_POINT('Ctrl Pts',(15.3030003780523,14.3120236313532,4.82073327307412));
#128276=CARTESIAN_POINT('Ctrl Pts',(15.3036719877099,14.3194060763851,4.81333657408827));
#128277=CARTESIAN_POINT('Ctrl Pts',(15.3047218384011,14.3309841852592,4.80210626059355));
#128278=CARTESIAN_POINT('Ctrl Pts',(15.3050940666254,14.3350964201846,4.79818730595112));
#128279=CARTESIAN_POINT('Ctrl Pts',(15.3057938835754,14.3428349785455,4.79094153052705));
#128280=CARTESIAN_POINT('Ctrl Pts',(15.3061208141385,14.3464525298845,4.78760581235585));
#128281=CARTESIAN_POINT('Ctrl Pts',(15.3069139442854,14.3552364194114,4.77962946099534));
#128282=CARTESIAN_POINT('Ctrl Pts',(15.3073820555686,14.3604275142673,4.77501667815));
#128283=CARTESIAN_POINT('Ctrl Pts',(15.3091023901688,14.3795453598865,4.75839377318508));
#128284=CARTESIAN_POINT('Ctrl Pts',(15.3103748567058,14.3937635676673,4.74672644657944));
#128285=CARTESIAN_POINT('Ctrl Pts',(15.3138562153588,14.4330743508532,4.71630241881851));
#128286=CARTESIAN_POINT('Ctrl Pts',(15.3160918018314,14.4587597698188,4.69834832589819));
#128287=CARTESIAN_POINT('Ctrl Pts',(15.3236054598915,14.5476077030973,4.64246266708636));
#128288=CARTESIAN_POINT('Ctrl Pts',(15.3288656385872,14.6142334565252,4.61049629414746));
#128289=CARTESIAN_POINT('Ctrl Pts',(15.3348866777584,14.6980003878017,4.58150887271192));
#128290=CARTESIAN_POINT('Ctrl Pts',(15.3358933898418,14.7122614167875,4.57694189438178));
#128291=CARTESIAN_POINT('Ctrl Pts',(15.3375092098169,14.7355571417003,4.57007404361211));
#128292=CARTESIAN_POINT('Ctrl Pts',(15.3381247066906,14.7445286602044,4.56756945868733));
#128293=CARTESIAN_POINT('Ctrl Pts',(15.3393111473073,14.7620063289039,4.56296140818578));
#128294=CARTESIAN_POINT('Ctrl Pts',(15.3398825085595,14.7705076020362,4.56084316667103));
#128295=CARTESIAN_POINT('Ctrl Pts',(15.3412297070632,14.7907445399543,4.55609198365884));
#128296=CARTESIAN_POINT('Ctrl Pts',(15.3420022598421,14.8025030099882,4.55356186142754));
#128297=CARTESIAN_POINT('Ctrl Pts',(15.3447696829348,14.8451331349749,4.54521807193019));
#128298=CARTESIAN_POINT('Ctrl Pts',(15.3467252102816,14.8762378004628,4.54069010368549));
#128299=CARTESIAN_POINT('Ctrl Pts',(15.3514496561643,14.9529169220548,4.53332034134832));
#128300=CARTESIAN_POINT('Ctrl Pts',(15.3541789790425,14.9985759484482,4.5321753616651));
#128301=CARTESIAN_POINT('Ctrl Pts',(15.3598641700541,15.0927766311417,4.53648149448564));
#128302=CARTESIAN_POINT('Ctrl Pts',(15.3628155112691,15.1411638987668,4.54237428355098));
#128303=CARTESIAN_POINT('Ctrl Pts',(15.3664979756387,15.1975919734861,4.55361656136522));
#128304=CARTESIAN_POINT('Ctrl Pts',(15.3670708445496,15.2062642604029,4.55546877102017));
#128305=CARTESIAN_POINT('Ctrl Pts',(15.3679954241269,15.2200662570228,4.55861571081712));
#128306=CARTESIAN_POINT('Ctrl Pts',(15.3683430831841,15.2252131590899,4.55983375557463));
#128307=CARTESIAN_POINT('Ctrl Pts',(15.3690308380418,15.2353043623555,4.56230951467175));
#128308=CARTESIAN_POINT('Ctrl Pts',(15.3693707721161,15.240249170188,4.56356424595803));
#128309=CARTESIAN_POINT('Ctrl Pts',(15.3702475396231,15.2528993368111,4.56688097626477));
#128310=CARTESIAN_POINT('Ctrl Pts',(15.3707873323813,15.2605894086003,4.56899928191545));
#128311=CARTESIAN_POINT('Ctrl Pts',(15.3732688099982,15.2955360976485,4.57909257136174));
#128312=CARTESIAN_POINT('Ctrl Pts',(15.3752594338012,15.3224572591916,4.5881704660809));
#128313=CARTESIAN_POINT('Ctrl Pts',(15.3827472689139,15.4209004838652,4.62627076379622));
#128314=CARTESIAN_POINT('Ctrl Pts',(15.388341942421,15.4892823035855,4.66264371626222));
#128315=CARTESIAN_POINT('Ctrl Pts',(15.3953810119013,15.5726812983413,4.72074398337533));
#128316=CARTESIAN_POINT('Ctrl Pts',(15.3970502948583,15.5922139612932,4.73548276092965));
#128317=CARTESIAN_POINT('Ctrl Pts',(15.3994338596525,15.6197355960493,4.75793826128105));
#128318=CARTESIAN_POINT('Ctrl Pts',(15.4001700862239,15.628182909002,4.7650754576437));
#128319=CARTESIAN_POINT('Ctrl Pts',(15.4014707398241,15.6430036933045,4.77803993586671));
#128320=CARTESIAN_POINT('Ctrl Pts',(15.4020373695996,15.6494249200041,4.78381052429582));
#128321=CARTESIAN_POINT('Ctrl Pts',(15.4032370690625,15.6629387313244,4.79628625208128));
#128322=CARTESIAN_POINT('Ctrl Pts',(15.4038690925951,15.6700088488294,4.80301438019936));
#128323=CARTESIAN_POINT('Ctrl Pts',(15.4056027911921,15.6892525902552,4.82189075010275));
#128324=CARTESIAN_POINT('Ctrl Pts',(15.4066949683271,15.7012061262668,4.8342588248614));
#128325=CARTESIAN_POINT('Ctrl Pts',(15.4091470682088,15.7275759455093,4.86304183611818));
#128326=CARTESIAN_POINT('Ctrl Pts',(15.410498926853,15.741778737318,4.87963973937127));
#128327=CARTESIAN_POINT('Ctrl Pts',(15.4154846561445,15.7925530256519,4.94321612271183));
#128328=CARTESIAN_POINT('Ctrl Pts',(15.4190123229926,15.8253223624569,4.99305673929817));
#128329=CARTESIAN_POINT('Ctrl Pts',(15.4247358514212,15.8695540187805,5.07611653611215));
#128330=CARTESIAN_POINT('Ctrl Pts',(15.4268684103275,15.8841570916619,5.10748614819478));
#128331=CARTESIAN_POINT('Ctrl Pts',(15.4296291407849,15.900214819738,5.14745067038789));
#128332=CARTESIAN_POINT('Ctrl Pts',(15.4301786956532,15.903278335539,5.15537558380203));
#128333=CARTESIAN_POINT('Ctrl Pts',(15.4310745959043,15.9080512390398,5.16822348659012));
#128334=CARTESIAN_POINT('Ctrl Pts',(15.4314173194299,15.9098260360525,5.17312190559403));
#128335=CARTESIAN_POINT('Ctrl Pts',(15.4321047003577,15.9132822545413,5.182907277898));
#128336=CARTESIAN_POINT('Ctrl Pts',(15.4324493133189,15.9149642504095,5.18779383731844));
#128337=CARTESIAN_POINT('Ctrl Pts',(15.4333527908699,15.9192447024389,5.20056119476978));
#128338=CARTESIAN_POINT('Ctrl Pts',(15.4339149519035,15.9217809555641,5.2084622155463));
#128339=CARTESIAN_POINT('Ctrl Pts',(15.4367482152983,15.9339491700872,5.24811606702138));
#128340=CARTESIAN_POINT('Ctrl Pts',(15.4390859610181,15.9420427515469,5.28031477274497));
#128341=CARTESIAN_POINT('Ctrl Pts',(15.4453039460653,15.958945657235,5.3659832860125));
#128342=CARTESIAN_POINT('Ctrl Pts',(15.449209686754,15.9649460527726,5.4198943911944));
#128343=CARTESIAN_POINT('Ctrl Pts',(15.4556654627283,15.9674068762499,5.51144914686525));
#128344=CARTESIAN_POINT('Ctrl Pts',(15.4582583897597,15.9662381513011,5.54890367014075));
#128345=CARTESIAN_POINT('Ctrl Pts',(15.4616577381952,15.9617497432213,5.59904148996148));
#128346=CARTESIAN_POINT('Ctrl Pts',(15.4625206312506,15.9603433534721,5.61185908856759));
#128347=CARTESIAN_POINT('Ctrl Pts',(15.4639074929291,15.957646952564,5.632597849062));
#128348=CARTESIAN_POINT('Ctrl Pts',(15.464436222963,15.9565140375325,5.64053746051362));
#128349=CARTESIAN_POINT('Ctrl Pts',(15.4655452710826,15.9539157168945,5.65725638997519));
#128350=CARTESIAN_POINT('Ctrl Pts',(15.466124830147,15.9524275986089,5.66603145841488));
#128351=CARTESIAN_POINT('Ctrl Pts',(15.4675315732024,15.9484969641867,5.68741384494798));
#128352=CARTESIAN_POINT('Ctrl Pts',(15.4683546334165,15.9459239946132,5.69999565311109));
#128353=CARTESIAN_POINT('Ctrl Pts',(15.471666645392,15.9344651598364,5.75084587317177));
#128354=CARTESIAN_POINT('Ctrl Pts',(15.4740909316105,15.9235009668209,5.78860914971829));
#128355=CARTESIAN_POINT('Ctrl Pts',(15.4788342431152,15.8972327725345,5.86204532493796));
#128356=CARTESIAN_POINT('Ctrl Pts',(15.4811501695692,15.8820210232896,5.89767125469481));
#128357=CARTESIAN_POINT('Ctrl Pts',(15.4860487463233,15.8457283743711,5.9702679012516));
#128358=CARTESIAN_POINT('Ctrl Pts',(15.4886303141887,15.8242627263851,6.00695028648403));
#128359=CARTESIAN_POINT('Ctrl Pts',(15.4920048188514,15.7944923541623,6.05090895071373));
#128360=CARTESIAN_POINT('Ctrl Pts',(15.4926882691952,15.7883812723433,6.05961926377231));
#128361=CARTESIAN_POINT('Ctrl Pts',(15.4937527482016,15.7787655165545,6.07285474545321));
#128362=CARTESIAN_POINT('Ctrl Pts',(15.4941275003126,15.7753621355024,6.07745289333438));
#128363=CARTESIAN_POINT('Ctrl Pts',(15.494829163135,15.7689614443556,6.08594196020945));
#128364=CARTESIAN_POINT('Ctrl Pts',(15.4951553696684,15.7659749888083,6.0898406530489));
#128365=CARTESIAN_POINT('Ctrl Pts',(15.495942745915,15.7587393314746,6.09913888136806));
#128366=CARTESIAN_POINT('Ctrl Pts',(15.4964057535631,15.754462096117,6.10451609669501));
#128367=CARTESIAN_POINT('Ctrl Pts',(15.4980837101978,15.7388688129166,6.12369624834307));
#128368=CARTESIAN_POINT('Ctrl Pts',(15.4993176807345,15.7272289604491,6.13723000673157));
#128369=CARTESIAN_POINT('Ctrl Pts',(15.502655045806,15.695138258194,6.17251724551104));
#128370=CARTESIAN_POINT('Ctrl Pts',(15.5047828528751,15.6740433257741,6.19365845577138));
#128371=CARTESIAN_POINT('Ctrl Pts',(15.5124052651986,15.595389322123,6.2655044195885));
#128372=CARTESIAN_POINT('Ctrl Pts',(15.5178905971892,15.5328100143352,6.31031044419269));
#128373=CARTESIAN_POINT('Ctrl Pts',(15.5240820642154,15.4528373572988,6.35425725070756));
#128374=CARTESIAN_POINT('Ctrl Pts',(15.525059223476,15.4399331329825,6.36097386694533));
#128375=CARTESIAN_POINT('Ctrl Pts',(15.5266400262731,15.4186016663122,6.37147195617902));
#128376=CARTESIAN_POINT('Ctrl Pts',(15.5272495474524,15.4102635372747,6.3754282182494));
#128377=CARTESIAN_POINT('Ctrl Pts',(15.5284326071863,15.3938632580389,6.38292400139175));
#128378=CARTESIAN_POINT('Ctrl Pts',(15.5290064523207,15.3858069091369,6.38647396776245));
#128379=CARTESIAN_POINT('Ctrl Pts',(15.5303726562686,15.3663914478694,6.39471440624157));
#128380=CARTESIAN_POINT('Ctrl Pts',(15.5311614651041,15.3549890365193,6.39929937583708));
#128381=CARTESIAN_POINT('Ctrl Pts',(15.534086927839,15.3120279578001,6.41562976076759));
#128382=CARTESIAN_POINT('Ctrl Pts',(15.5361776435485,15.2799485835347,6.42594191674715));
#128383=CARTESIAN_POINT('Ctrl Pts',(15.5423065447752,15.1830825156925,6.45158400748197));
#128384=CARTESIAN_POINT('Ctrl Pts',(15.5462283213267,15.1171895063828,6.46192375117493));
#128385=CARTESIAN_POINT('Ctrl Pts',(15.5519423630345,15.0242398087023,6.46681086157044));
#128386=CARTESIAN_POINT('Ctrl Pts',(15.5535977767732,14.9976760462093,6.46711176052837));
#128387=CARTESIAN_POINT('Ctrl Pts',(15.5558182452771,14.9631215654536,6.46607962100183));
#128388=CARTESIAN_POINT('Ctrl Pts',(15.5563377434236,14.9551106019397,6.46574053707156));
#128389=CARTESIAN_POINT('Ctrl Pts',(15.5571638134655,14.9425066079403,6.46504988575111));
#128390=CARTESIAN_POINT('Ctrl Pts',(15.5574668997558,14.9379100917275,6.46476505599464));
#128391=CARTESIAN_POINT('Ctrl Pts',(15.5581116526307,14.9281956485794,6.46409337719542));
#128392=CARTESIAN_POINT('Ctrl Pts',(15.5584537639934,14.9230784772076,6.46369859419588));
#128393=CARTESIAN_POINT('Ctrl Pts',(15.5593430615093,14.9098665445954,6.46257341604216));
#128394=CARTESIAN_POINT('Ctrl Pts',(15.5598933645677,14.9017775582408,6.46178166045271));
#128395=CARTESIAN_POINT('Ctrl Pts',(15.5625286244504,14.8634057878595,6.45753670700769));
#128396=CARTESIAN_POINT('Ctrl Pts',(15.5646699072689,14.83328986756,6.45275490439155));
#128397=CARTESIAN_POINT('Ctrl Pts',(15.5703459190587,14.7550868435611,6.43651656000711));
#128398=CARTESIAN_POINT('Ctrl Pts',(15.5739088101027,14.707561063446,6.42278133980252));
#128399=CARTESIAN_POINT('Ctrl Pts',(15.5805301500298,14.6201060648715,6.39006730536638));
#128400=CARTESIAN_POINT('Ctrl Pts',(15.5835940321438,14.5800147872644,6.37186727593042));
#128401=CARTESIAN_POINT('Ctrl Pts',(15.587479917268,14.5294478088551,6.34461080200532));
#128402=CARTESIAN_POINT('Ctrl Pts',(15.5883821034378,14.5177324230444,6.33797660247071));
#128403=CARTESIAN_POINT('Ctrl Pts',(15.5898144589288,14.4991820497335,6.32695393233695));
#128404=CARTESIAN_POINT('Ctrl Pts',(15.5903500168414,14.4922575025864,6.32272048020689));
#128405=CARTESIAN_POINT('Ctrl Pts',(15.591460417144,14.4779290080856,6.31371066973453));
#128406=CARTESIAN_POINT('Ctrl Pts',(15.5920346500362,14.470535367909,6.3089192706395));
#128407=CARTESIAN_POINT('Ctrl Pts',(15.593403725678,14.4529554477259,6.29718240656121));
#128408=CARTESIAN_POINT('Ctrl Pts',(15.5941949781779,14.4428343610594,6.29014176203187));
#128409=CARTESIAN_POINT('Ctrl Pts',(15.597145384632,14.4052919229046,6.26294552855077));
#128410=CARTESIAN_POINT('Ctrl Pts',(15.5992575048577,14.3788051221356,6.24153951114497));
#128411=CARTESIAN_POINT('Ctrl Pts',(15.6055182180954,14.3026712494375,6.17306157283416));
#128412=CARTESIAN_POINT('Ctrl Pts',(15.6095429016476,14.2568382359838,6.12208441508455));
#128413=CARTESIAN_POINT('Ctrl Pts',(15.6152678327459,14.2023282709744,6.04674681527668));
#128414=CARTESIAN_POINT('Ctrl Pts',(15.6168076195095,14.1886586594488,6.02624831485754));
#128415=CARTESIAN_POINT('Ctrl Pts',(15.6188948470073,14.1716889935412,5.99856588892394));
#128416=CARTESIAN_POINT('Ctrl Pts',(15.6194033044282,14.1676718847976,5.9918302229538));
#128417=CARTESIAN_POINT('Ctrl Pts',(15.6202161738297,14.1614426568302,5.98109049224276));
#128418=CARTESIAN_POINT('Ctrl Pts',(15.6205172921297,14.1591761531177,5.97711815719065));
#128419=CARTESIAN_POINT('Ctrl Pts',(15.6211629005091,14.1544061167868,5.96861851320094));
#128420=CARTESIAN_POINT('Ctrl Pts',(15.6215078898227,14.15191058755,5.96408692232078));
#128421=CARTESIAN_POINT('Ctrl Pts',(15.6224134841664,14.1454951233105,5.95221262582946));
#128422=CARTESIAN_POINT('Ctrl Pts',(15.6229774125683,14.1416335211085,5.94483909431455));
#128423=CARTESIAN_POINT('Ctrl Pts',(15.6258430362792,14.122653464822,5.90743012096101));
#128424=CARTESIAN_POINT('Ctrl Pts',(15.6282131481239,14.109015440328,5.87667270225498));
#128425=CARTESIAN_POINT('Ctrl Pts',(15.6341222070828,14.079387692006,5.79918683639663));
#128426=CARTESIAN_POINT('Ctrl Pts',(15.6376782398824,14.0653197678851,5.75181932782896));
#128427=CARTESIAN_POINT('Ctrl Pts',(15.6440752975221,14.0462744567851,5.6634081089236));
#128428=CARTESIAN_POINT('Ctrl Pts',(15.6469311412012,14.0401895872312,5.62271656071804));
#128429=CARTESIAN_POINT('Ctrl Pts',(15.6505836809088,14.0356195354829,5.56887037062414));
#128430=CARTESIAN_POINT('Ctrl Pts',(15.6514499965795,14.0347845031464,5.55596320297559));
#128431=CARTESIAN_POINT('Ctrl Pts',(15.652814918391,14.0338689125233,5.53541916057281));
#128432=CARTESIAN_POINT('Ctrl Pts',(15.6533186235992,14.0336194235813,5.5277917655005));
#128433=CARTESIAN_POINT('Ctrl Pts',(15.6542613554327,14.0333199090117,5.51343345209547));
#128434=CARTESIAN_POINT('Ctrl Pts',(15.6547009683701,14.0332498134312,5.50670346095259));
#128435=CARTESIAN_POINT('Ctrl Pts',(15.6551384615117,14.0332500003729,5.49997314748094));
#128436=CARTESIAN_POINT('Origin',(16.125,15.,5.5));
#128437=CARTESIAN_POINT('',(16.1125616277506,14.0332502848258,5.49925789884204));
#128438=CARTESIAN_POINT('',(16.0537548202437,14.0332502522516,5.49930162248347));
#128439=CARTESIAN_POINT('',(16.125,14.03325,5.5));
#128440=CARTESIAN_POINT('Ctrl Pts',(16.1125616274111,14.033250284824,5.49925790359377));
#128441=CARTESIAN_POINT('Ctrl Pts',(16.1073559830469,14.0331943674599,5.57210301548347));
#128442=CARTESIAN_POINT('Ctrl Pts',(16.1021282237257,14.0413721963873,5.64473355734449));
#128443=CARTESIAN_POINT('Ctrl Pts',(16.095897439841,14.0616857744272,5.73345544885228));
#128444=CARTESIAN_POINT('Ctrl Pts',(16.094669390181,14.0662345449869,5.75103223120923));
#128445=CARTESIAN_POINT('Ctrl Pts',(16.0927719147452,14.0741224866012,5.77831900578406));
#128446=CARTESIAN_POINT('Ctrl Pts',(16.0920921318069,14.0771256816659,5.78812088588505));
#128447=CARTESIAN_POINT('Ctrl Pts',(16.0908368400081,14.0830012481834,5.80626231593391));
#128448=CARTESIAN_POINT('Ctrl Pts',(16.0902601005158,14.0858329075989,5.8146138150736));
#128449=CARTESIAN_POINT('Ctrl Pts',(16.0889617871747,14.0925057374861,5.83344299829025));
#128450=CARTESIAN_POINT('Ctrl Pts',(16.0882424962458,14.096414885327,5.84389537154835));
#128451=CARTESIAN_POINT('Ctrl Pts',(16.0860092111178,14.109210081522,5.8763817862009));
#128452=CARTESIAN_POINT('Ctrl Pts',(16.0845157678623,14.1187281521941,5.89815825158713));
#128453=CARTESIAN_POINT('Ctrl Pts',(16.0809031029579,14.1440057637913,5.95063138391362));
#128454=CARTESIAN_POINT('Ctrl Pts',(16.078809013189,14.1606243097535,5.98087779207209));
#128455=CARTESIAN_POINT('Ctrl Pts',(16.0734365601449,14.2076013074271,6.05649210963097));
#128456=CARTESIAN_POINT('Ctrl Pts',(16.0701897651757,14.2402434620536,6.10029018998348));
#128457=CARTESIAN_POINT('Ctrl Pts',(16.0656260447405,14.288895528575,6.15520303986655));
#128458=CARTESIAN_POINT('Ctrl Pts',(16.0644371463051,14.3017995191111,6.16893690240557));
#128459=CARTESIAN_POINT('Ctrl Pts',(16.062750268492,14.3202639751207,6.1874722759581));
#128460=CARTESIAN_POINT('Ctrl Pts',(16.0622742452965,14.3254910182834,6.192601486775));
#128461=CARTESIAN_POINT('Ctrl Pts',(16.0614589014763,14.3344601364066,6.20120490522481));
#128462=CARTESIAN_POINT('Ctrl Pts',(16.0611218387834,14.3381723436076,6.20470971418489));
#128463=CARTESIAN_POINT('Ctrl Pts',(16.0603950642301,14.3461822873295,6.21215303019434));
#128464=CARTESIAN_POINT('Ctrl Pts',(16.0600047745553,14.3504879477886,6.21608213887289));
#128465=CARTESIAN_POINT('Ctrl Pts',(16.0588744813706,14.362976643957,6.22727333580981));
#128466=CARTESIAN_POINT('Ctrl Pts',(16.058128059539,14.3712475054409,6.23443552314028));
#128467=CARTESIAN_POINT('Ctrl Pts',(16.0545092689552,14.4115370495578,6.26814505305229));
#128468=CARTESIAN_POINT('Ctrl Pts',(16.0515456005969,14.4451229683162,6.29274609434139));
#128469=CARTESIAN_POINT('Ctrl Pts',(16.043276719109,14.5425596783632,6.35488407467061));
#128470=CARTESIAN_POINT('Ctrl Pts',(16.0379924889092,14.6093055432432,6.38737810176765));
#128471=CARTESIAN_POINT('Ctrl Pts',(16.0319421746931,14.6933319620555,6.41694464235156));
#128472=CARTESIAN_POINT('Ctrl Pts',(16.0309287361999,14.7076662587569,6.42161477257108));
#128473=CARTESIAN_POINT('Ctrl Pts',(16.0292913167586,14.7312421915324,6.42869037841406));
#128474=CARTESIAN_POINT('Ctrl Pts',(16.0286610296978,14.7404201317674,6.43129741836877));
#128475=CARTESIAN_POINT('Ctrl Pts',(16.0274378193656,14.7584269456808,6.43612545573894));
#128476=CARTESIAN_POINT('Ctrl Pts',(16.0268445729351,14.7672515363398,6.43835844503077));
#128477=CARTESIAN_POINT('Ctrl Pts',(16.0254305771287,14.7884945760319,6.4434156971549));
#128478=CARTESIAN_POINT('Ctrl Pts',(16.0246136474746,14.8009400422729,6.44611990737854));
#128479=CARTESIAN_POINT('Ctrl Pts',(16.0215367331926,14.8484118352093,6.45545655901631));
#128480=CARTESIAN_POINT('Ctrl Pts',(16.0193283921805,14.8837437051285,6.46039630739235));
#128481=CARTESIAN_POINT('Ctrl Pts',(16.0124157158759,14.9965974235826,6.46985328539258));
#128482=CARTESIAN_POINT('Ctrl Pts',(16.0078753691624,15.0744140903304,6.46699909607143));
#128483=CARTESIAN_POINT('Ctrl Pts',(16.0020477843197,15.1662616544443,6.45247046237586));
#128484=CARTESIAN_POINT('Ctrl Pts',(16.0010696607862,15.1814181938449,6.44970011013545));
#128485=CARTESIAN_POINT('Ctrl Pts',(15.9996738685021,15.2025621558754,6.44531077170842));
#128486=CARTESIAN_POINT('Ctrl Pts',(15.9992709533124,15.2086108024591,6.44399439109653));
#128487=CARTESIAN_POINT('Ctrl Pts',(15.9985297113356,15.2196286601962,6.44148548914403));
#128488=CARTESIAN_POINT('Ctrl Pts',(15.9981923869776,15.2246017348553,6.44031150915673));
#128489=CARTESIAN_POINT('Ctrl Pts',(15.9974663490607,15.2352135883743,6.43771740832042));
#128490=CARTESIAN_POINT('Ctrl Pts',(15.9970770749847,15.2408489572423,6.43628582474119));
#128491=CARTESIAN_POINT('Ctrl Pts',(15.995952781455,15.2569798491264,6.43203274359874));
#128492=CARTESIAN_POINT('Ctrl Pts',(15.9952114432159,15.2674408200437,6.42908506722868));
#128493=CARTESIAN_POINT('Ctrl Pts',(15.9916446776112,15.3170433086303,6.41420106422892));
#128494=CARTESIAN_POINT('Ctrl Pts',(15.9887306260668,15.3554478431438,6.39996461843803));
#128495=CARTESIAN_POINT('Ctrl Pts',(15.9804320678423,15.4614362444033,6.35283034363875));
#128496=CARTESIAN_POINT('Ctrl Pts',(15.9750660572825,15.5262661104544,6.31442665335761));
#128497=CARTESIAN_POINT('Ctrl Pts',(15.9689536860992,15.5978685415422,6.25985613153497));
#128498=CARTESIAN_POINT('Ctrl Pts',(15.9679509490473,15.6095237368577,6.25053913234669));
#128499=CARTESIAN_POINT('Ctrl Pts',(15.9663261872256,15.6282477851073,6.23484741094146));
#128500=CARTESIAN_POINT('Ctrl Pts',(15.9656980436076,15.6354460790801,6.22863179193351));
#128501=CARTESIAN_POINT('Ctrl Pts',(15.9644759158744,15.6493653068344,6.21624955454216));
#128502=CARTESIAN_POINT('Ctrl Pts',(15.9638816512118,15.6560929831189,6.21009205944995));
#128503=CARTESIAN_POINT('Ctrl Pts',(15.962460125571,15.6720790679656,6.19503963314108));
#128504=CARTESIAN_POINT('Ctrl Pts',(15.9616367936941,15.6812495234686,6.18605355218398));
#128505=CARTESIAN_POINT('Ctrl Pts',(15.9584893577171,15.7159125441216,6.15070680890273));
#128506=CARTESIAN_POINT('Ctrl Pts',(15.9562202487941,15.7400777548757,6.12308542872458));
#128507=CARTESIAN_POINT('Ctrl Pts',(15.9498144328366,15.804643749653,6.04021293969853));
#128508=CARTESIAN_POINT('Ctrl Pts',(15.9457875645173,15.8408253560152,5.98196804449622));
#128509=CARTESIAN_POINT('Ctrl Pts',(15.9402269200436,15.8798947322617,5.90106336349003));
#128510=CARTESIAN_POINT('Ctrl Pts',(15.9388782115468,15.888584078633,5.88142463579809));
#128511=CARTESIAN_POINT('Ctrl Pts',(15.9370031330575,15.8994776365651,5.85440693460589));
#128512=CARTESIAN_POINT('Ctrl Pts',(15.9365056978748,15.9022587194492,5.84726573151318));
#128513=CARTESIAN_POINT('Ctrl Pts',(15.9356686667423,15.9067518716136,5.83530987135058));
#128514=CARTESIAN_POINT('Ctrl Pts',(15.9353317191763,15.908511261121,5.83051316738401));
#128515=CARTESIAN_POINT('Ctrl Pts',(15.9346166376098,15.9121397299699,5.82037278509638));
#128516=CARTESIAN_POINT('Ctrl Pts',(15.9342380639457,15.9140000086389,5.81502633019523));
#128517=CARTESIAN_POINT('Ctrl Pts',(15.93317608188,15.9190535362268,5.8000808184879));
#128518=CARTESIAN_POINT('Ctrl Pts',(15.9324873479841,15.9221431322509,5.79044779964323));
#128519=CARTESIAN_POINT('Ctrl Pts',(15.9281517841875,15.9404672238376,5.73007327912846));
#128520=CARTESIAN_POINT('Ctrl Pts',(15.924349236942,15.9516591132974,5.67820312908497));
#128521=CARTESIAN_POINT('Ctrl Pts',(15.916132519835,15.9665836474667,5.56437766626793));
#128522=CARTESIAN_POINT('Ctrl Pts',(15.9117461075325,15.9687232192829,5.50243460987787));
#128523=CARTESIAN_POINT('Ctrl Pts',(15.9064304147305,15.9639366710472,5.42454243712536));
#128524=CARTESIAN_POINT('Ctrl Pts',(15.9053393085399,15.9625375900903,5.40840747885397));
#128525=CARTESIAN_POINT('Ctrl Pts',(15.9036100489793,15.9596462679916,5.38261209180479));
#128526=CARTESIAN_POINT('Ctrl Pts',(15.9029641722851,15.9584118198074,5.37292649376607));
#128527=CARTESIAN_POINT('Ctrl Pts',(15.9017312762011,15.9557572080952,5.3543469783687));
#128528=CARTESIAN_POINT('Ctrl Pts',(15.9011436460825,15.9543590823371,5.34545099653667));
#128529=CARTESIAN_POINT('Ctrl Pts',(15.8997748191213,15.9507903213054,5.32464353548988));
#128530=CARTESIAN_POINT('Ctrl Pts',(15.8989967908379,15.9485197929731,5.31275057335208));
#128531=CARTESIAN_POINT('Ctrl Pts',(15.8962983639835,15.9398001781217,5.27131858690539));
#128532=CARTESIAN_POINT('Ctrl Pts',(15.8944136832919,15.9321892938038,5.24204081877785));
#128533=CARTESIAN_POINT('Ctrl Pts',(15.8893558698805,15.9077602843337,5.16341248924754));
#128534=CARTESIAN_POINT('Ctrl Pts',(15.8862485699041,15.8883060403032,5.11499035224674));
#128535=CARTESIAN_POINT('Ctrl Pts',(15.8806789894354,15.8471673321851,5.03254271394913));
#128536=CARTESIAN_POINT('Ctrl Pts',(15.8782375274485,15.8270833828993,4.99786332735044));
#128537=CARTESIAN_POINT('Ctrl Pts',(15.8750144861897,15.7990008719898,4.95564993973623));
#128538=CARTESIAN_POINT('Ctrl Pts',(15.8743291145243,15.7929453549398,4.94686617922809));
#128539=CARTESIAN_POINT('Ctrl Pts',(15.8732551152119,15.7833542775733,4.93343517430583));
#128540=CARTESIAN_POINT('Ctrl Pts',(15.8728726930437,15.7799196945114,4.92871645235685));
#128541=CARTESIAN_POINT('Ctrl Pts',(15.8721504365594,15.7734021494417,4.91993041514342));
#128542=CARTESIAN_POINT('Ctrl Pts',(15.8718112531023,15.7703293785615,4.91585596661415));
#128543=CARTESIAN_POINT('Ctrl Pts',(15.8709811507635,15.7627780275539,4.90600618291672));
#128544=CARTESIAN_POINT('Ctrl Pts',(15.870488065974,15.7582660066827,4.90025703066892));
#128545=CARTESIAN_POINT('Ctrl Pts',(15.8686196874381,15.7410549471082,4.87883163906568));
#128546=CARTESIAN_POINT('Ctrl Pts',(15.8672201502287,15.7279321758293,4.86350397432698));
#128547=CARTESIAN_POINT('Ctrl Pts',(15.8632575633959,15.6899121629053,4.82181037763897));
#128548=CARTESIAN_POINT('Ctrl Pts',(15.8606604227985,15.6639970871807,4.79641801618213));
#128549=CARTESIAN_POINT('Ctrl Pts',(15.8534787222765,15.5885074171763,4.73034453724786));
#128550=CARTESIAN_POINT('Ctrl Pts',(15.8489268378337,15.5362136648007,4.693037912234));
#128551=CARTESIAN_POINT('Ctrl Pts',(15.8434657664078,15.4666340831746,4.65317210454957));
#128552=CARTESIAN_POINT('Ctrl Pts',(15.8423808925587,15.4524639338855,4.64551694431356));
#128553=CARTESIAN_POINT('Ctrl Pts',(15.8406589966178,15.4294213407824,4.63380265317274));
#128554=CARTESIAN_POINT('Ctrl Pts',(15.8400143687425,15.4206677263204,4.62951783061913));
#128555=CARTESIAN_POINT('Ctrl Pts',(15.838782346825,15.4036983782576,4.62152724831228));
#128556=CARTESIAN_POINT('Ctrl Pts',(15.8381943639143,15.3954927257299,4.61780259071355));
#128557=CARTESIAN_POINT('Ctrl Pts',(15.8368224349295,15.3761033054182,4.60932638574957));
#128558=CARTESIAN_POINT('Ctrl Pts',(15.8360417020124,15.3648795183189,4.60466981425817));
#128559=CARTESIAN_POINT('Ctrl Pts',(15.8333192262497,15.3251158797495,4.58904450315052));
#128560=CARTESIAN_POINT('Ctrl Pts',(15.8314141134521,15.2961451865936,4.57921851476289));
#128561=CARTESIAN_POINT('Ctrl Pts',(15.8262660012174,15.2155572451679,4.55608374604975));
#128562=CARTESIAN_POINT('Ctrl Pts',(15.8230922472621,15.1632324420339,4.54564256033955));
#128563=CARTESIAN_POINT('Ctrl Pts',(15.8173350719284,15.0686926629639,4.53478396086078));
#128564=CARTESIAN_POINT('Ctrl Pts',(15.8147743925482,15.026809915178,4.5327145625386));
#128565=CARTESIAN_POINT('Ctrl Pts',(15.8115255278422,14.9760738062427,4.53350553199079));
#128566=CARTESIAN_POINT('Ctrl Pts',(15.8109531070492,14.96721997769,4.53376530989647));
#128567=CARTESIAN_POINT('Ctrl Pts',(15.8100218722228,14.9529800087402,4.53437905809718));
#128568=CARTESIAN_POINT('Ctrl Pts',(15.809667000976,14.9475908691475,4.53465655717467));
#128569=CARTESIAN_POINT('Ctrl Pts',(15.8089555572655,14.9368682529702,4.53529873918228));
#128570=CARTESIAN_POINT('Ctrl Pts',(15.8085990383027,14.9315349269467,4.53566257452602));
#128571=CARTESIAN_POINT('Ctrl Pts',(15.8076618416041,14.9176116924178,4.53672848678808));
#128572=CARTESIAN_POINT('Ctrl Pts',(15.8070776133299,14.9090278545961,4.537501221983));
#128573=CARTESIAN_POINT('Ctrl Pts',(15.8040153368434,14.864470739322,4.54211368751897));
#128574=CARTESIAN_POINT('Ctrl Pts',(15.8014590544304,14.8287264076335,4.54785546372532));
#128575=CARTESIAN_POINT('Ctrl Pts',(15.7928856231723,14.7112997070172,4.57354475315133));
#128576=CARTESIAN_POINT('Ctrl Pts',(15.7868381870474,14.6318810072862,4.60213547723658));
#128577=CARTESIAN_POINT('Ctrl Pts',(15.7801230651489,14.5439488588012,4.64744873911932));
#128578=CARTESIAN_POINT('Ctrl Pts',(15.7791246067988,14.5309002559615,4.6545582416056));
#128579=CARTESIAN_POINT('Ctrl Pts',(15.7775049051969,14.5097870996908,4.66670108745569));
#128580=CARTESIAN_POINT('Ctrl Pts',(15.776877617437,14.5016241029278,4.67155733980715));
#128581=CARTESIAN_POINT('Ctrl Pts',(15.7756559013371,14.4857597468186,4.68131457768487));
#128582=CARTESIAN_POINT('Ctrl Pts',(15.7750612097264,14.4780536370423,4.6862058846313));
#128583=CARTESIAN_POINT('Ctrl Pts',(15.7736365671182,14.4596419585907,4.69826148246447));
#128584=CARTESIAN_POINT('Ctrl Pts',(15.7728105906044,14.4490078972017,4.70553213359073));
#128585=CARTESIAN_POINT('Ctrl Pts',(15.7696331587769,14.4083170644561,4.73456313829603));
#128586=CARTESIAN_POINT('Ctrl Pts',(15.7673381622905,14.3793760434723,4.75783518360754));
#128587=CARTESIAN_POINT('Ctrl Pts',(15.7626474974636,14.3222751668091,4.80943309727329));
#128588=CARTESIAN_POINT('Ctrl Pts',(15.760261589418,14.2943883250774,4.83795329979655));
#128589=CARTESIAN_POINT('Ctrl Pts',(15.7552454367953,14.2400622752341,4.90085723786862));
#128590=CARTESIAN_POINT('Ctrl Pts',(15.752617197068,14.214016412403,4.93545910567804));
#128591=CARTESIAN_POINT('Ctrl Pts',(15.7491813586544,14.184464340448,4.98074645913912));
#128592=CARTESIAN_POINT('Ctrl Pts',(15.7484865023856,14.1787037845835,4.98990671889887));
#128593=CARTESIAN_POINT('Ctrl Pts',(15.7474007824598,14.1700581736333,5.0041809125312));
#128594=CARTESIAN_POINT('Ctrl Pts',(15.7470163382586,14.167063739241,5.00922797156989));
#128595=CARTESIAN_POINT('Ctrl Pts',(15.7462926923989,14.1615560709209,5.01870664496249));
#128596=CARTESIAN_POINT('Ctrl Pts',(15.7459541803669,14.1590316310737,5.02313134562218));
#128597=CARTESIAN_POINT('Ctrl Pts',(15.7451291088517,14.1530020924413,5.03389637229565));
#128598=CARTESIAN_POINT('Ctrl Pts',(15.7446404493503,14.1495331288844,5.04025644040136));
#128599=CARTESIAN_POINT('Ctrl Pts',(15.7428114142325,14.1369132693476,5.0640256102066));
#128600=CARTESIAN_POINT('Ctrl Pts',(15.7414480344349,14.128223346219,5.0816727081945));
#128601=CARTESIAN_POINT('Ctrl Pts',(15.7376324537265,14.1057011687235,5.1311640244244));
#128602=CARTESIAN_POINT('Ctrl Pts',(15.7351486685707,14.0930366145623,5.1635069369349));
#128603=CARTESIAN_POINT('Ctrl Pts',(15.7278996638257,14.0612440498586,5.25964275582242));
#128604=CARTESIAN_POINT('Ctrl Pts',(15.7231644495544,14.0469256598392,5.32482494169527));
#128605=CARTESIAN_POINT('Ctrl Pts',(15.7175674127192,14.0376531348269,5.40651769189749));
#128606=CARTESIAN_POINT('Ctrl Pts',(15.7165132149986,14.0362660019894,5.42210738489885));
#128607=CARTESIAN_POINT('Ctrl Pts',(15.714831220477,14.034639859842,5.44729886644916));
#128608=CARTESIAN_POINT('Ctrl Pts',(15.7141963539579,14.0341643724357,5.4568820073503));
#128609=CARTESIAN_POINT('Ctrl Pts',(15.7131667839531,14.0336210085073,5.47253949885804));
#128610=CARTESIAN_POINT('Ctrl Pts',(15.7127695005825,14.033467586689,5.47861002314708));
#128611=CARTESIAN_POINT('Ctrl Pts',(15.712039416012,14.0332899944767,5.48981660510008));
#128612=CARTESIAN_POINT('Ctrl Pts',(15.7117061358681,14.0332495375256,5.49495213410438));
#128613=CARTESIAN_POINT('Ctrl Pts',(15.7113740739618,14.0332500039877,5.50008780779963));
#128614=CARTESIAN_POINT('Ctrl Pts',(15.6551384581207,14.0332500003715,5.49997319964798));
#128615=CARTESIAN_POINT('Ctrl Pts',(15.6556495968289,14.0332502183577,5.4921099366161));
#128616=CARTESIAN_POINT('Ctrl Pts',(15.6561578055333,14.0333463724681,5.48424677980226));
#128617=CARTESIAN_POINT('Ctrl Pts',(15.6573484241237,14.033798881653,5.46572713321696));
#128618=CARTESIAN_POINT('Ctrl Pts',(15.6580283880359,14.0342356103667,5.45507352796589));
#128619=CARTESIAN_POINT('Ctrl Pts',(15.6617082259838,14.037576120969,5.39705588127462));
#128620=CARTESIAN_POINT('Ctrl Pts',(15.6646079478208,14.0437879373676,5.34994525653666));
#128621=CARTESIAN_POINT('Ctrl Pts',(15.6704414463854,14.0634145221551,5.25541265464075));
#128622=CARTESIAN_POINT('Ctrl Pts',(15.6733649236248,14.0770394133501,5.2081803913445));
#128623=CARTESIAN_POINT('Ctrl Pts',(15.6774960081779,14.1005487027816,5.1451423642523));
#128624=CARTESIAN_POINT('Ctrl Pts',(15.6786251467091,14.1073857738489,5.12827920656151));
#128625=CARTESIAN_POINT('Ctrl Pts',(15.6805818802552,14.1198309164871,5.09991070985696));
#128626=CARTESIAN_POINT('Ctrl Pts',(15.6813991922176,14.1251992305403,5.08830516989108));
#128627=CARTESIAN_POINT('Ctrl Pts',(15.6826228397123,14.1334520128632,5.07135449587531));
#128628=CARTESIAN_POINT('Ctrl Pts',(15.6830194641986,14.1361594377544,5.06592413039527));
#128629=CARTESIAN_POINT('Ctrl Pts',(15.6837397968014,14.1411301617844,5.05618489242835));
#128630=CARTESIAN_POINT('Ctrl Pts',(15.6840624216962,14.1433751537788,5.05186707499766));
#128631=CARTESIAN_POINT('Ctrl Pts',(15.6848048829462,14.1485840898269,5.0420308463886));
#128632=CARTESIAN_POINT('Ctrl Pts',(15.6852259411836,14.1515691507101,5.03652412511972));
#128633=CARTESIAN_POINT('Ctrl Pts',(15.6866173536018,14.161541143299,5.01854738052514));
#128634=CARTESIAN_POINT('Ctrl Pts',(15.6875996397597,14.1687508306791,5.00620383994242));
#128635=CARTESIAN_POINT('Ctrl Pts',(15.6941483204363,14.2180765640143,4.92589741317553));
#128636=CARTESIAN_POINT('Ctrl Pts',(15.6999872079677,14.2682113875373,4.86322338049762));
#128637=CARTESIAN_POINT('Ctrl Pts',(15.7081339108804,14.3511848613971,4.78241330925159));
#128638=CARTESIAN_POINT('Ctrl Pts',(15.7106125132494,14.3782515483434,4.75883798787974));
#128639=CARTESIAN_POINT('Ctrl Pts',(15.7138765173973,14.4164526171131,4.72913375534097));
#128640=CARTESIAN_POINT('Ctrl Pts',(15.7147136754323,14.4264850772212,4.72164084558442));
#128641=CARTESIAN_POINT('Ctrl Pts',(15.7161294287509,14.4438469533974,4.70919184046298));
#128642=CARTESIAN_POINT('Ctrl Pts',(15.7167116718776,14.4511037888662,4.70413775406642));
#128643=CARTESIAN_POINT('Ctrl Pts',(15.7178186215378,14.4651194074766,4.69465936131876));
#128644=CARTESIAN_POINT('Ctrl Pts',(15.7183438958634,14.4718662552249,4.69021882792767));
#128645=CARTESIAN_POINT('Ctrl Pts',(15.719721822269,14.4898123269664,4.67872707399137));
#128646=CARTESIAN_POINT('Ctrl Pts',(15.7205692250919,14.5011022717516,4.67182021025378));
#128647=CARTESIAN_POINT('Ctrl Pts',(15.723984186577,14.5475708974944,4.64468726595321));
#128648=CARTESIAN_POINT('Ctrl Pts',(15.7264829027725,14.583866292559,4.62645250553793));
#128649=CARTESIAN_POINT('Ctrl Pts',(15.7319567291149,14.6668035989688,4.5911313558562));
#128650=CARTESIAN_POINT('Ctrl Pts',(15.7349056641051,14.7138282020511,4.57524728398047));
#128651=CARTESIAN_POINT('Ctrl Pts',(15.7399808421712,14.7946213794426,4.55471292055863));
#128652=CARTESIAN_POINT('Ctrl Pts',(15.7420681749885,14.8277912890577,4.54811149338693));
#128653=CARTESIAN_POINT('Ctrl Pts',(15.7447703229556,14.8694819431896,4.54206469782178));
#128654=CARTESIAN_POINT('Ctrl Pts',(15.7453096313878,14.8777437365132,4.54097528646347));
#128655=CARTESIAN_POINT('Ctrl Pts',(15.7461929413554,14.8911575645331,4.53938266114961));
#128656=CARTESIAN_POINT('Ctrl Pts',(15.7465335047767,14.8963015658865,4.53881376447233));
#128657=CARTESIAN_POINT('Ctrl Pts',(15.7472210774897,14.9066249222412,4.5377558932344));
#128658=CARTESIAN_POINT('Ctrl Pts',(15.7475680956959,14.9118041444458,4.53726737142786));
#128659=CARTESIAN_POINT('Ctrl Pts',(15.7484850491741,14.9254153347025,4.53609427002527));
#128660=CARTESIAN_POINT('Ctrl Pts',(15.7490584536928,14.9338525903833,4.53547854511962));
#128661=CARTESIAN_POINT('Ctrl Pts',(15.7519292209816,14.9757796125655,4.53297152893087));
#128662=CARTESIAN_POINT('Ctrl Pts',(15.7542940832517,15.0093412069448,4.53271358788778));
#128663=CARTESIAN_POINT('Ctrl Pts',(15.760983417264,15.103149922085,4.53687512608228));
#128664=CARTESIAN_POINT('Ctrl Pts',(15.7653396320154,15.1630776095258,4.54519314191467));
#128665=CARTESIAN_POINT('Ctrl Pts',(15.7711071588488,15.2432217311859,4.56408794958034));
#128666=CARTESIAN_POINT('Ctrl Pts',(15.7726288027139,15.264427148629,4.56985669030132));
#128667=CARTESIAN_POINT('Ctrl Pts',(15.7753092775567,15.301920988245,4.58144265248999));
#128668=CARTESIAN_POINT('Ctrl Pts',(15.7764756701517,15.3182842604172,4.58698352848051));
#128669=CARTESIAN_POINT('Ctrl Pts',(15.7782801457926,15.3436613847601,4.59634191004306));
#128670=CARTESIAN_POINT('Ctrl Pts',(15.7789276438771,15.3527800360638,4.59986259447048));
#128671=CARTESIAN_POINT('Ctrl Pts',(15.7801383285016,15.3698468925271,4.6067512559654));
#128672=CARTESIAN_POINT('Ctrl Pts',(15.7807024570464,15.37780636179,4.61008854171932));
#128673=CARTESIAN_POINT('Ctrl Pts',(15.7819798221948,15.39583715518,4.61793410787388));
#128674=CARTESIAN_POINT('Ctrl Pts',(15.7826907509582,15.4058782316501,4.62250916332058));
#128675=CARTESIAN_POINT('Ctrl Pts',(15.7848901727664,15.4369312719251,4.63730509228897));
#128676=CARTESIAN_POINT('Ctrl Pts',(15.7863588192133,15.4576532673498,4.64811675903615));
#128677=CARTESIAN_POINT('Ctrl Pts',(15.7922723748994,15.540522683884,4.69525134327923));
#128678=CARTESIAN_POINT('Ctrl Pts',(15.7965164386462,15.5989097446057,4.73770593838504));
#128679=CARTESIAN_POINT('Ctrl Pts',(15.8023028676483,15.6690964596576,4.80182458192056));
#128680=CARTESIAN_POINT('Ctrl Pts',(15.8037226294215,15.6855835680331,4.81800730850678));
#128681=CARTESIAN_POINT('Ctrl Pts',(15.8061199086769,15.7118617024375,4.84571692157959));
#128682=CARTESIAN_POINT('Ctrl Pts',(15.807079980182,15.7219904025015,4.85691117888819));
#128683=CARTESIAN_POINT('Ctrl Pts',(15.8084755192149,15.7360741506229,4.87322878254368));
#128684=CARTESIAN_POINT('Ctrl Pts',(15.8088969642284,15.7402467681037,4.87816237568118));
#128685=CARTESIAN_POINT('Ctrl Pts',(15.8096117892207,15.747182311838,4.8865315098997));
#128686=CARTESIAN_POINT('Ctrl Pts',(15.8099033142593,15.7499717246646,4.8899447511957));
#128687=CARTESIAN_POINT('Ctrl Pts',(15.8105801278236,15.7563564828769,4.89786738072869));
#128688=CARTESIAN_POINT('Ctrl Pts',(15.8109665163487,15.7599348152839,4.90238984881359));
#128689=CARTESIAN_POINT('Ctrl Pts',(15.8120878830152,15.7701349206172,4.91552098218511));
#128690=CARTESIAN_POINT('Ctrl Pts',(15.812829197302,15.7766521450197,4.92420929122086));
#128691=CARTESIAN_POINT('Ctrl Pts',(15.8183939215017,15.8240102643661,4.98961096486209));
#128692=CARTESIAN_POINT('Ctrl Pts',(15.8234709983416,15.8587383718413,5.05049170923649));
#128693=CARTESIAN_POINT('Ctrl Pts',(15.8307644690659,15.8996150391371,5.14452254674572));
#128694=CARTESIAN_POINT('Ctrl Pts',(15.8330623195544,15.9111067314229,5.17510573418608));
#128695=CARTESIAN_POINT('Ctrl Pts',(15.8368919777386,15.9279591086787,5.22793856746538));
#128696=CARTESIAN_POINT('Ctrl Pts',(15.8384448507,15.9341183064918,5.24990269183507));
#128697=CARTESIAN_POINT('Ctrl Pts',(15.840696681109,15.9420387944436,5.28254921162091));
#128698=CARTESIAN_POINT('Ctrl Pts',(15.8414142747615,15.944406667795,5.29307489941878));
#128699=CARTESIAN_POINT('Ctrl Pts',(15.8426946429158,15.9483466975313,5.31206855077032));
#128700=CARTESIAN_POINT('Ctrl Pts',(15.8432593611036,15.9499827970973,5.32052191916797));
#128701=CARTESIAN_POINT('Ctrl Pts',(15.8444682820853,15.9532633789661,5.33877586173613));
#128702=CARTESIAN_POINT('Ctrl Pts',(15.8451112535044,15.9548701352099,5.34858226943635));
#128703=CARTESIAN_POINT('Ctrl Pts',(15.8468804235149,15.9589026517713,5.37581903027254));
#128704=CARTESIAN_POINT('Ctrl Pts',(15.8479966524727,15.9610042059478,5.39329393506057));
#128705=CARTESIAN_POINT('Ctrl Pts',(15.8545268951363,15.9706074357716,5.496950134613));
#128706=CARTESIAN_POINT('Ctrl Pts',(15.8595840556235,15.9669913184988,5.58375782895399));
#128707=CARTESIAN_POINT('Ctrl Pts',(15.8666728770546,15.946747677258,5.69782838226927));
#128708=CARTESIAN_POINT('Ctrl Pts',(15.868496601459,15.9403051845685,5.72647972006876));
#128709=CARTESIAN_POINT('Ctrl Pts',(15.8708983239596,15.9304491184675,5.76255432464798));
#128710=CARTESIAN_POINT('Ctrl Pts',(15.871419710188,15.9282312113452,5.77029084997551));
#128711=CARTESIAN_POINT('Ctrl Pts',(15.8722811003307,15.9244458825671,5.78289847482078));
#128712=CARTESIAN_POINT('Ctrl Pts',(15.8726179820302,15.9229358580818,5.78778661656662));
#128713=CARTESIAN_POINT('Ctrl Pts',(15.8732634045381,15.9199886419105,5.79706531648785));
#128714=CARTESIAN_POINT('Ctrl Pts',(15.8735714989943,15.9185586435891,5.80145798981087));
#128715=CARTESIAN_POINT('Ctrl Pts',(15.8744241590459,15.9145363041837,5.81351944294505));
#128716=CARTESIAN_POINT('Ctrl Pts',(15.8749721973459,15.9118791010769,5.82116598092802));
#128717=CARTESIAN_POINT('Ctrl Pts',(15.8773956789997,15.8998033461968,5.85455747446959));
#128718=CARTESIAN_POINT('Ctrl Pts',(15.8793161102307,15.8893888740733,5.87992660886625));
#128719=CARTESIAN_POINT('Ctrl Pts',(15.8859175388306,15.8503958555049,5.96448942326975));
#128720=CARTESIAN_POINT('Ctrl Pts',(15.8906762551205,15.8168644909113,6.02120727481705));
#128721=CARTESIAN_POINT('Ctrl Pts',(15.897636606641,15.7579411560756,6.1010436350139));
#128722=CARTESIAN_POINT('Ctrl Pts',(15.8999468814423,15.7366542436428,6.12695231414162));
#128723=CARTESIAN_POINT('Ctrl Pts',(15.90303247286,15.7057910856038,6.16076853548565));
#128724=CARTESIAN_POINT('Ctrl Pts',(15.9038523613196,15.6973475798021,6.16967342055236));
#128725=CARTESIAN_POINT('Ctrl Pts',(15.9052480253838,15.6825610211547,6.18468493276363));
#128726=CARTESIAN_POINT('Ctrl Pts',(15.9058271938336,15.6763000639869,6.19086991303629));
#128727=CARTESIAN_POINT('Ctrl Pts',(15.9070065679208,15.6632982184298,6.20336782836127));
#128728=CARTESIAN_POINT('Ctrl Pts',(15.9076063421276,15.6565495669797,6.20967140581826));
#128729=CARTESIAN_POINT('Ctrl Pts',(15.9091425272377,15.6389200761236,6.22567146424163));
#128730=CARTESIAN_POINT('Ctrl Pts',(15.9100728680037,15.6279082204021,6.23522053800172));
#128731=CARTESIAN_POINT('Ctrl Pts',(15.915830814087,15.5577701062863,6.29331597926802));
#128732=CARTESIAN_POINT('Ctrl Pts',(15.9203732033247,15.4932732108086,6.33494926264737));
#128733=CARTESIAN_POINT('Ctrl Pts',(15.9268042514346,15.3976379172647,6.38169507271811));
#128734=CARTESIAN_POINT('Ctrl Pts',(15.9286254623712,15.3701422803926,6.39358636157927));
#128735=CARTESIAN_POINT('Ctrl Pts',(15.9316080605303,15.3254158137158,6.41051079135322));
#128736=CARTESIAN_POINT('Ctrl Pts',(15.9327393183586,15.3085192665266,6.41637390037019));
#128737=CARTESIAN_POINT('Ctrl Pts',(15.934338322435,15.2849154045754,6.42383767467148));
#128738=CARTESIAN_POINT('Ctrl Pts',(15.9347858770212,15.2783380058633,6.42584058283552));
#128739=CARTESIAN_POINT('Ctrl Pts',(15.9355598521304,15.2670262431559,6.42915374076354));
#128740=CARTESIAN_POINT('Ctrl Pts',(15.935884363089,15.2623023036063,6.43049835511877));
#128741=CARTESIAN_POINT('Ctrl Pts',(15.9365912256314,15.2520567199103,6.43333041791334));
#128742=CARTESIAN_POINT('Ctrl Pts',(15.9369742170835,15.2465320688042,6.43480489627575));
#128743=CARTESIAN_POINT('Ctrl Pts',(15.9380761707549,15.2307028056774,6.43887950368638));
#128744=CARTESIAN_POINT('Ctrl Pts',(15.9388011554398,15.2203682864799,6.44135875367847));
#128745=CARTESIAN_POINT('Ctrl Pts',(15.9424423921174,15.1687580899615,6.45284364187224));
#128746=CARTESIAN_POINT('Ctrl Pts',(15.9454543412342,15.126966868417,6.4593065775544));
#128747=CARTESIAN_POINT('Ctrl Pts',(15.951257877836,15.0462047926802,6.4664258556855));
#128748=CARTESIAN_POINT('Ctrl Pts',(15.954042640131,15.007346450168,6.46750199061406));
#128749=CARTESIAN_POINT('Ctrl Pts',(15.958655195215,14.9420423647818,6.46537489174267));
#128750=CARTESIAN_POINT('Ctrl Pts',(15.9605045263738,14.9156022496462,6.46342357262938));
#128751=CARTESIAN_POINT('Ctrl Pts',(15.963681653053,14.8696376880029,6.45812417505072));
#128752=CARTESIAN_POINT('Ctrl Pts',(15.9650219014629,14.8500744705347,6.45525844546418));
#128753=CARTESIAN_POINT('Ctrl Pts',(15.9670294859375,14.820518681379,6.44999848045933));
#128754=CARTESIAN_POINT('Ctrl Pts',(15.9677100502371,14.8104546261503,6.44804178253842));
#128755=CARTESIAN_POINT('Ctrl Pts',(15.9689518730169,14.792015703491,6.44415143309504));
#128756=CARTESIAN_POINT('Ctrl Pts',(15.9695145567794,14.7836319507952,6.44226549940818));
#128757=CARTESIAN_POINT('Ctrl Pts',(15.97075085654,14.7651552245341,6.43784952796542));
#128758=CARTESIAN_POINT('Ctrl Pts',(15.9714227744784,14.7550756222975,6.43526780567692));
#128759=CARTESIAN_POINT('Ctrl Pts',(15.9733680741889,14.7258069711588,6.42726548471068));
#128760=CARTESIAN_POINT('Ctrl Pts',(15.9746278503047,14.7067409635156,6.42141321759786));
#128761=CARTESIAN_POINT('Ctrl Pts',(15.9806347414312,14.6156644581305,6.39034369214941));
#128762=CARTESIAN_POINT('Ctrl Pts',(15.9851298013793,14.546632536636,6.35725360489714));
#128763=CARTESIAN_POINT('Ctrl Pts',(15.9918929929511,14.452719114953,6.29768950848176));
#128764=CARTESIAN_POINT('Ctrl Pts',(15.99404625264,14.4242687532711,6.2774046174881));
#128765=CARTESIAN_POINT('Ctrl Pts',(15.9968232857152,14.3904205001339,6.25039246145946));
#128766=CARTESIAN_POINT('Ctrl Pts',(15.9973663748209,14.3839287480584,6.24507195223129));
#128767=CARTESIAN_POINT('Ctrl Pts',(15.9982543279225,14.373537835885,6.23632712616542));
#128768=CARTESIAN_POINT('Ctrl Pts',(15.9985956860415,14.3695953827067,6.23295463382176));
#128769=CARTESIAN_POINT('Ctrl Pts',(15.999241680192,14.3622368376419,6.22655662785863));
#128770=CARTESIAN_POINT('Ctrl Pts',(15.9995457796194,14.3588146258465,6.22353831869193));
#128771=CARTESIAN_POINT('Ctrl Pts',(16.000373167727,14.3496125276711,6.21530573460485));
#128772=CARTESIAN_POINT('Ctrl Pts',(16.0008996015816,14.3438741803584,6.21004581367135));
#128773=CARTESIAN_POINT('Ctrl Pts',(16.0030642831221,14.3207251506482,6.18830656958076));
#128774=CARTESIAN_POINT('Ctrl Pts',(16.0047368448663,14.3038679605313,6.17125274416622));
#128775=CARTESIAN_POINT('Ctrl Pts',(16.0113023671196,14.2410214078813,6.1027575353815));
#128776=CARTESIAN_POINT('Ctrl Pts',(16.01630831422,14.1999535371934,6.04707578193256));
#128777=CARTESIAN_POINT('Ctrl Pts',(16.0235491174608,14.1479415560903,5.95800439584722));
#128778=CARTESIAN_POINT('Ctrl Pts',(16.0259051241987,14.1322952893734,5.92762203977659));
#128779=CARTESIAN_POINT('Ctrl Pts',(16.0290394146784,14.1132274373277,5.88521717439445));
#128780=CARTESIAN_POINT('Ctrl Pts',(16.0298641707206,14.1083822948082,5.8738659395957));
#128781=CARTESIAN_POINT('Ctrl Pts',(16.0312654862192,14.1004521176434,5.85425530381771));
#128782=CARTESIAN_POINT('Ctrl Pts',(16.0318455100048,14.0972603708278,5.84604101408276));
#128783=CARTESIAN_POINT('Ctrl Pts',(16.0329524808061,14.0913466456947,5.83018246880816));
#128784=CARTESIAN_POINT('Ctrl Pts',(16.033479941589,14.0886077307911,5.82254537533416));
#128785=CARTESIAN_POINT('Ctrl Pts',(16.0348734441661,14.0815859498073,5.8021621692857));
#128786=CARTESIAN_POINT('Ctrl Pts',(16.0357339988198,14.077472213602,5.78935938792309));
#128787=CARTESIAN_POINT('Ctrl Pts',(16.0393555836553,14.0611420155299,5.73464236295716));
#128788=CARTESIAN_POINT('Ctrl Pts',(16.0420355822339,14.0515043265455,5.69201022281936));
#128789=CARTESIAN_POINT('Ctrl Pts',(16.0477147800653,14.0370689530188,5.59938527521914));
#128790=CARTESIAN_POINT('Ctrl Pts',(16.0506938265694,14.03321407643,5.54937935504139));
#128791=CARTESIAN_POINT('Ctrl Pts',(16.053754820006,14.0332502522502,5.49930162637244));
#128792=CARTESIAN_POINT('Origin',(16.125,15.,5.5));
#128793=CARTESIAN_POINT('',(16.5125067421103,14.0332503216444,5.50077380256718));
#128794=CARTESIAN_POINT('',(16.4541432637038,14.0332503253858,5.5007624277622));
#128795=CARTESIAN_POINT('',(16.125,14.03325,5.5));
#128796=CARTESIAN_POINT('Ctrl Pts',(16.5125067496464,14.0332503339973,5.50080360660429));
#128797=CARTESIAN_POINT('Ctrl Pts',(16.5105833290927,14.0332767876738,5.53262773901946));
#128798=CARTESIAN_POINT('Ctrl Pts',(16.5086462365695,14.0348746414668,5.5644291826904));
#128799=CARTESIAN_POINT('Ctrl Pts',(16.5057673491034,14.0394468958017,5.61020150264302));
#128800=CARTESIAN_POINT('Ctrl Pts',(16.5048693988576,14.0411665401289,5.62427786879034));
#128801=CARTESIAN_POINT('Ctrl Pts',(16.5035762620414,14.0440418281855,5.64416854663637));
#128802=CARTESIAN_POINT('Ctrl Pts',(16.5031929469513,14.044942389746,5.65001850948271));
#128803=CARTESIAN_POINT('Ctrl Pts',(16.5024976571657,14.0466608445872,5.66053812421363));
#128804=CARTESIAN_POINT('Ctrl Pts',(16.502186679749,14.0474594861647,5.66521077990356));
#128805=CARTESIAN_POINT('Ctrl Pts',(16.5015377746353,14.0491870160363,5.67488896340818));
#128806=CARTESIAN_POINT('Ctrl Pts',(16.5011995249584,14.0501211071857,5.67989320238334));
#128807=CARTESIAN_POINT('Ctrl Pts',(16.5003764658171,14.05247528727,5.69197550914361));
#128808=CARTESIAN_POINT('Ctrl Pts',(16.4998895827829,14.0539351985892,5.69904537483077));
#128809=CARTESIAN_POINT('Ctrl Pts',(16.4981632417358,14.0593509290644,5.7238651141439));
#128810=CARTESIAN_POINT('Ctrl Pts',(16.4969045717342,14.0637280485396,5.74151812196225));
#128811=CARTESIAN_POINT('Ctrl Pts',(16.490577773891,14.0879326106587,5.82854903437541));
#128812=CARTESIAN_POINT('Ctrl Pts',(16.4853308474073,14.1149860537522,5.89567975587241));
#128813=CARTESIAN_POINT('Ctrl Pts',(16.4776819913718,14.1665691581234,5.99125035059317));
#128814=CARTESIAN_POINT('Ctrl Pts',(16.4751589135872,14.1856813043854,6.02232123930006));
#128815=CARTESIAN_POINT('Ctrl Pts',(16.4718074907172,14.2140212633326,6.06304185307378));
#128816=CARTESIAN_POINT('Ctrl Pts',(16.4709266512986,14.2217577424303,6.07368782440317));
#128817=CARTESIAN_POINT('Ctrl Pts',(16.4694454835682,14.2352536902985,6.09148358160653));
#128818=CARTESIAN_POINT('Ctrl Pts',(16.4688410400938,14.2409018434157,6.09871507734019));
#128819=CARTESIAN_POINT('Ctrl Pts',(16.4676963510626,14.251863695255,6.11234531265085));
#128820=CARTESIAN_POINT('Ctrl Pts',(16.4671554464197,14.2571586528099,6.11875799172183));
#128821=CARTESIAN_POINT('Ctrl Pts',(16.4657444459347,14.2712686335921,6.13540425095298));
#128822=CARTESIAN_POINT('Ctrl Pts',(16.4648797475106,14.2802166869923,6.1455230259763));
#128823=CARTESIAN_POINT('Ctrl Pts',(16.461511913143,14.3162073295224,6.1845432797082));
#128824=CARTESIAN_POINT('Ctrl Pts',(16.4590730686303,14.3448031643363,6.21196173385888));
#128825=CARTESIAN_POINT('Ctrl Pts',(16.4536224152011,14.4132311964921,6.26994730214302));
#128826=CARTESIAN_POINT('Ctrl Pts',(16.4506403796383,14.4539200831638,6.29932035565807));
#128827=CARTESIAN_POINT('Ctrl Pts',(16.445543604979,14.5253700556522,6.34288756493675));
#128828=CARTESIAN_POINT('Ctrl Pts',(16.4434695215582,14.5549270863108,6.35886126532734));
#128829=CARTESIAN_POINT('Ctrl Pts',(16.4407728297959,14.5929123534625,6.37690200949856));
#128830=CARTESIAN_POINT('Ctrl Pts',(16.4402240491711,14.6006202661687,6.38043926690264));
#128831=CARTESIAN_POINT('Ctrl Pts',(16.4393218150596,14.6132346716849,6.3860284502893));
#128832=CARTESIAN_POINT('Ctrl Pts',(16.4389718679392,14.6181135211208,6.3881421894044));
#128833=CARTESIAN_POINT('Ctrl Pts',(16.4382596672256,14.6280082235383,6.39233242108524));
#128834=CARTESIAN_POINT('Ctrl Pts',(16.4378973396688,14.6330245921608,6.39440710977871));
#128835=CARTESIAN_POINT('Ctrl Pts',(16.4369275308173,14.6464121815821,6.39981241746529));
#128836=CARTESIAN_POINT('Ctrl Pts',(16.4363160620137,14.6548127332749,6.40306836327861));
#128837=CARTESIAN_POINT('Ctrl Pts',(16.4323846413182,14.7086425547327,6.4230713203994));
#128838=CARTESIAN_POINT('Ctrl Pts',(16.4289264463184,14.7552266076856,6.43650143293388));
#128839=CARTESIAN_POINT('Ctrl Pts',(16.4221879859515,14.8473778614359,6.45572113315245));
#128840=CARTESIAN_POINT('Ctrl Pts',(16.4189169113154,14.8927495167184,6.46187021627812));
#128841=CARTESIAN_POINT('Ctrl Pts',(16.4135422864062,14.9694444752851,6.46676797918873));
#128842=CARTESIAN_POINT('Ctrl Pts',(16.4114017438431,15.000580521315,6.46725073126526));
#128843=CARTESIAN_POINT('Ctrl Pts',(16.4084827310651,15.0439008706756,6.46582999369363));
#128844=CARTESIAN_POINT('Ctrl Pts',(16.4076668319409,15.0561049215193,6.4651979713166));
#128845=CARTESIAN_POINT('Ctrl Pts',(16.4062608491905,15.0772924543401,6.46369747005433));
#128846=CARTESIAN_POINT('Ctrl Pts',(16.4056676309965,15.0862815971163,6.46293428251287));
#128847=CARTESIAN_POINT('Ctrl Pts',(16.4044433308546,15.1049294714602,6.46108782294924));
#128848=CARTESIAN_POINT('Ctrl Pts',(16.4038129343279,15.114585226447,6.45998449694793));
#128849=CARTESIAN_POINT('Ctrl Pts',(16.4021583210635,15.140055576125,6.45668431419686));
#128850=CARTESIAN_POINT('Ctrl Pts',(16.4011417183137,15.1558355601533,6.45424093648017));
#128851=CARTESIAN_POINT('Ctrl Pts',(16.3959680353904,15.2366295709528,6.43967295207971));
#128852=CARTESIAN_POINT('Ctrl Pts',(16.3920085456699,15.300335843104,6.42129158068097));
#128853=CARTESIAN_POINT('Ctrl Pts',(16.3859133527246,15.3941259789592,6.38345628137011));
#128854=CARTESIAN_POINT('Ctrl Pts',(16.3837980252179,15.4258440445157,6.36861202104873));
#128855=CARTESIAN_POINT('Ctrl Pts',(16.3803960164886,15.4741039117932,6.34274646252821));
#128856=CARTESIAN_POINT('Ctrl Pts',(16.3791500298384,15.4912307212228,6.3328795717899));
#128857=CARTESIAN_POINT('Ctrl Pts',(16.377407529083,15.5142157246497,6.31868211822658));
#128858=CARTESIAN_POINT('Ctrl Pts',(16.3769357001066,15.520346252571,6.31479935688548));
#128859=CARTESIAN_POINT('Ctrl Pts',(16.3761251778817,15.5307064696131,6.30807312470866));
#128860=CARTESIAN_POINT('Ctrl Pts',(16.3757886726384,15.5349583907188,6.30526458435078));
#128861=CARTESIAN_POINT('Ctrl Pts',(16.3750601723402,15.5440539669144,6.29915280820992));
#128862=CARTESIAN_POINT('Ctrl Pts',(16.3746675601561,15.5488898559573,6.29583908644269));
#128863=CARTESIAN_POINT('Ctrl Pts',(16.3735448055558,15.5625412267501,6.28630107701731));
#128864=CARTESIAN_POINT('Ctrl Pts',(16.3728085309313,15.5712827612458,6.27997307590908));
#128865=CARTESIAN_POINT('Ctrl Pts',(16.3691133829193,15.6142033227395,6.24779426345757));
#128866=CARTESIAN_POINT('Ctrl Pts',(16.3660570863485,15.6467406059271,6.21983884390686));
#128867=CARTESIAN_POINT('Ctrl Pts',(16.3600940012295,15.7061948721333,6.16146252113395));
#128868=CARTESIAN_POINT('Ctrl Pts',(16.3571940440591,15.7332683582405,6.13131743001137));
#128869=CARTESIAN_POINT('Ctrl Pts',(16.3517402020986,15.7812996795712,6.0705636992478));
#128870=CARTESIAN_POINT('Ctrl Pts',(16.3491822507258,15.802545971781,6.04027090694735));
#128871=CARTESIAN_POINT('Ctrl Pts',(16.3458183843617,15.8287792606081,5.99789161319542));
#128872=CARTESIAN_POINT('Ctrl Pts',(16.3449576887603,15.8353327290766,5.98681657709178));
#128873=CARTESIAN_POINT('Ctrl Pts',(16.3435000074547,15.8461523719744,5.96766973471541));
#128874=CARTESIAN_POINT('Ctrl Pts',(16.3428992164216,15.8505287572435,5.95966255009034));
#128875=CARTESIAN_POINT('Ctrl Pts',(16.3416808417757,15.8592295487312,5.94319343332397));
#128876=CARTESIAN_POINT('Ctrl Pts',(16.3410636563806,15.8635438790499,5.9347272893724));
#128877=CARTESIAN_POINT('Ctrl Pts',(16.3394908009555,15.8742910998221,5.91284614105817));
#128878=CARTESIAN_POINT('Ctrl Pts',(16.3385413732388,15.8805405562273,5.89934349793339));
#128879=CARTESIAN_POINT('Ctrl Pts',(16.332295108105,15.9199737298078,5.80871233210587));
#128880=CARTESIAN_POINT('Ctrl Pts',(16.3273495203905,15.9432985493906,5.72769122974226));
#128881=CARTESIAN_POINT('Ctrl Pts',(16.3200477566085,15.9612845257851,5.6088568530949));
#128882=CARTESIAN_POINT('Ctrl Pts',(16.3178178811493,15.9646875339598,5.57276785108625));
#128883=CARTESIAN_POINT('Ctrl Pts',(16.3149442696165,15.9663839654178,5.52796267925683));
#128884=CARTESIAN_POINT('Ctrl Pts',(16.3143867042571,15.9665948786398,5.51934446607222));
#128885=CARTESIAN_POINT('Ctrl Pts',(16.3134737168902,15.9667498180917,5.50537903400174));
#128886=CARTESIAN_POINT('Ctrl Pts',(16.3131219619996,15.9667647804515,5.50003286266465));
#128887=CARTESIAN_POINT('Ctrl Pts',(16.312410198331,15.9667057461933,5.48929122597609));
#128888=CARTESIAN_POINT('Ctrl Pts',(16.3120501637509,15.9666309194127,5.48389597062502));
#128889=CARTESIAN_POINT('Ctrl Pts',(16.3110932217846,15.9663140171604,5.4696487643885));
#128890=CARTESIAN_POINT('Ctrl Pts',(16.3104925017385,15.9659954783744,5.46079923998198));
#128891=CARTESIAN_POINT('Ctrl Pts',(16.3070636144001,15.9635049902982,5.41074739728882));
#128892=CARTESIAN_POINT('Ctrl Pts',(16.3041343731744,15.9588187660242,5.3697164409778));
#128893=CARTESIAN_POINT('Ctrl Pts',(16.297345241201,15.9420303529762,5.27623484555285));
#128894=CARTESIAN_POINT('Ctrl Pts',(16.2934868792006,15.9281411983399,5.22423415052124));
#128895=CARTESIAN_POINT('Ctrl Pts',(16.2875848626558,15.8996373303231,5.1447521848488));
#128896=CARTESIAN_POINT('Ctrl Pts',(16.285473783497,15.8879005292606,5.11635782049986));
#128897=CARTESIAN_POINT('Ctrl Pts',(16.2825867308426,15.8696528814523,5.07755774600721));
#128898=CARTESIAN_POINT('Ctrl Pts',(16.2817744334564,15.8642673541312,5.0666461545593));
#128899=CARTESIAN_POINT('Ctrl Pts',(16.2803725654047,15.8545360746065,5.04783310926381));
#128900=CARTESIAN_POINT('Ctrl Pts',(16.2797799131304,15.8502832165091,5.03988560038536));
#128901=CARTESIAN_POINT('Ctrl Pts',(16.2785548882698,15.8412053636816,5.02347724557386));
#128902=CARTESIAN_POINT('Ctrl Pts',(16.277923226749,15.8363623956584,5.01502747122555));
#128903=CARTESIAN_POINT('Ctrl Pts',(16.2762608297667,15.8231924246876,4.99283336980867));
#128904=CARTESIAN_POINT('Ctrl Pts',(16.2752378440435,15.8146488336771,4.9792206967599));
#128905=CARTESIAN_POINT('Ctrl Pts',(16.2701509049664,15.7700356661606,4.91192431939944));
#128906=CARTESIAN_POINT('Ctrl Pts',(16.2662741490846,15.7289829632749,4.86174241477248));
#128907=CARTESIAN_POINT('Ctrl Pts',(16.2602151736066,15.6578375874246,4.79067444988966));
#128908=CARTESIAN_POINT('Ctrl Pts',(16.2580485319236,15.6310612995862,4.76675082340595));
#128909=CARTESIAN_POINT('Ctrl Pts',(16.2545754400448,15.5873452483631,4.73186377613888));
#128910=CARTESIAN_POINT('Ctrl Pts',(16.2533117489838,15.5712869796003,4.71984696064718));
#128911=CARTESIAN_POINT('Ctrl Pts',(16.2515484702936,15.5488956134504,4.70415305503031));
#128912=CARTESIAN_POINT('Ctrl Pts',(16.2510743394036,15.5428762737919,4.70003493957868));
#128913=CARTESIAN_POINT('Ctrl Pts',(16.2502611746449,15.5325686457607,4.69315291275355));
#128914=CARTESIAN_POINT('Ctrl Pts',(16.2499243671422,15.5283040703061,4.69035415593343));
#128915=CARTESIAN_POINT('Ctrl Pts',(16.2491968308511,15.5191064601562,4.68442155726726));
#128916=CARTESIAN_POINT('Ctrl Pts',(16.2488055066962,15.5141670868817,4.68129864069463));
#128917=CARTESIAN_POINT('Ctrl Pts',(16.2476900501384,15.5001011134725,4.67258292767819));
#128918=CARTESIAN_POINT('Ctrl Pts',(16.2469599023281,15.4909097978122,4.66709683449133));
#128919=CARTESIAN_POINT('Ctrl Pts',(16.2433973225832,15.4460542455253,4.64132391580039));
#128920=CARTESIAN_POINT('Ctrl Pts',(16.240475408915,15.4092164110101,4.62317027294435));
#128921=CARTESIAN_POINT('Ctrl Pts',(16.2338672770681,15.3239351901979,4.58769096576293));
#128922=CARTESIAN_POINT('Ctrl Pts',(16.2301866545479,15.2750300868017,4.57177533213881));
#128923=CARTESIAN_POINT('Ctrl Pts',(16.224505195386,15.1959067865099,4.55283236172576));
#128924=CARTESIAN_POINT('Ctrl Pts',(16.2224436336864,15.1664123835201,4.54720766327891));
#128925=CARTESIAN_POINT('Ctrl Pts',(16.2196104692767,15.1247455712622,4.5412560498023));
#128926=CARTESIAN_POINT('Ctrl Pts',(16.2188043644101,15.1127584103614,4.5397724318742));
#128927=CARTESIAN_POINT('Ctrl Pts',(16.2174095527018,15.091794750482,4.5375758247239));
#128928=CARTESIAN_POINT('Ctrl Pts',(16.2168178550086,15.0828304716686,4.53676291006744));
#128929=CARTESIAN_POINT('Ctrl Pts',(16.2155914811344,15.0641091732799,4.53532848462104));
#128930=CARTESIAN_POINT('Ctrl Pts',(16.2149575611769,15.0543514160391,4.53472954383689));
#128931=CARTESIAN_POINT('Ctrl Pts',(16.2132812720016,15.0283499304566,4.53352909284104));
#128932=CARTESIAN_POINT('Ctrl Pts',(16.2122468971076,15.0120969092273,4.53318903332481));
#128933=CARTESIAN_POINT('Ctrl Pts',(16.2076907582181,14.9397485130913,4.53350018663546));
#128934=CARTESIAN_POINT('Ctrl Pts',(16.2043028997232,14.8837801471013,4.53862290095077));
#128935=CARTESIAN_POINT('Ctrl Pts',(16.1984056776056,14.7874136864648,4.55598663306492));
#128936=CARTESIAN_POINT('Ctrl Pts',(16.1958960845821,14.7467867791296,4.56606379037165));
#128937=CARTESIAN_POINT('Ctrl Pts',(16.1923816050153,14.6926719960557,4.58327795169618));
#128938=CARTESIAN_POINT('Ctrl Pts',(16.191445103013,14.6785096318547,4.58814819509471));
#128939=CARTESIAN_POINT('Ctrl Pts',(16.1897854025014,14.6539936673505,4.59722101823879));
#128940=CARTESIAN_POINT('Ctrl Pts',(16.1890686235036,14.6435889703397,4.6012778932845));
#128941=CARTESIAN_POINT('Ctrl Pts',(16.1879600399008,14.6278222529524,4.60774230519148));
#128942=CARTESIAN_POINT('Ctrl Pts',(16.1875752388561,14.6224076891339,4.6100201621208));
#128943=CARTESIAN_POINT('Ctrl Pts',(16.1868513421799,14.6123381537226,4.61436475152856));
#128944=CARTESIAN_POINT('Ctrl Pts',(16.186512942971,14.6076782375176,4.6164191432923));
#128945=CARTESIAN_POINT('Ctrl Pts',(16.1856887333997,14.5964391663997,4.62148048269541));
#128946=CARTESIAN_POINT('Ctrl Pts',(16.1852008343408,14.5898772232002,4.62452459259364));
#128947=CARTESIAN_POINT('Ctrl Pts',(16.1834671880298,14.5668584894024,4.6355186429366));
#128948=CARTESIAN_POINT('Ctrl Pts',(16.1822020298152,14.5505944871386,4.64386089036813));
#128949=CARTESIAN_POINT('Ctrl Pts',(16.1758347889273,14.4709245792262,4.68762144287024));
#128950=CARTESIAN_POINT('Ctrl Pts',(16.1705527963481,14.411413153113,4.72964548942773));
#128951=CARTESIAN_POINT('Ctrl Pts',(16.1628632965646,14.3298252397355,4.80228126590489));
#128952=CARTESIAN_POINT('Ctrl Pts',(16.1603311325907,14.3038857561274,4.82815838849209));
#128953=CARTESIAN_POINT('Ctrl Pts',(16.1569943374277,14.270918967912,4.86501097649619));
#128954=CARTESIAN_POINT('Ctrl Pts',(16.1561360899593,14.2625548258743,4.87474416999497));
#128955=CARTESIAN_POINT('Ctrl Pts',(16.1546812546512,14.2485825220966,4.89167403351593));
#128956=CARTESIAN_POINT('Ctrl Pts',(16.1540808987697,14.2428780848884,4.89878862059772));
#128957=CARTESIAN_POINT('Ctrl Pts',(16.1528623276605,14.2314307233898,4.91348717253875));
#128958=CARTESIAN_POINT('Ctrl Pts',(16.1522445250428,14.2256973545143,4.92107733386379));
#128959=CARTESIAN_POINT('Ctrl Pts',(16.1506678157201,14.2112561108543,4.94079389072775));
#128960=CARTESIAN_POINT('Ctrl Pts',(16.1497152138452,14.2027152243588,4.95303983756325));
#128961=CARTESIAN_POINT('Ctrl Pts',(16.1434818965528,14.148172879607,5.03523680137596));
#128962=CARTESIAN_POINT('Ctrl Pts',(16.1385497351003,14.1111431539906,5.11070798638034));
#128963=CARTESIAN_POINT('Ctrl Pts',(16.1312558261808,14.0726417439136,5.2244394773653));
#128964=CARTESIAN_POINT('Ctrl Pts',(16.129018523802,14.0629382069889,5.25949725084588));
#128965=CARTESIAN_POINT('Ctrl Pts',(16.1261364894884,14.0534029649584,5.30344456693666));
#128966=CARTESIAN_POINT('Ctrl Pts',(16.1255785422586,14.0516867644825,5.31189901630506));
#128967=CARTESIAN_POINT('Ctrl Pts',(16.1246650866699,14.049090417552,5.32562934748641));
#128968=CARTESIAN_POINT('Ctrl Pts',(16.1243132524631,14.048140472526,5.33089176424303));
#128969=CARTESIAN_POINT('Ctrl Pts',(16.1236015033954,14.0463200395838,5.34147809013245));
#128970=CARTESIAN_POINT('Ctrl Pts',(16.123241564777,14.045450362164,5.34680193121465));
#128971=CARTESIAN_POINT('Ctrl Pts',(16.1222851609598,14.0432718646222,5.36087725537264));
#128972=CARTESIAN_POINT('Ctrl Pts',(16.121684890353,14.042038601067,5.3696396999101));
#128973=CARTESIAN_POINT('Ctrl Pts',(16.1183149889578,14.0358443564242,5.41850148246738));
#128974=CARTESIAN_POINT('Ctrl Pts',(16.1154484691767,14.0332812943534,5.45886092356221));
#128975=CARTESIAN_POINT('Ctrl Pts',(16.1125616274111,14.033250284824,5.49925790359377));
#128976=CARTESIAN_POINT('Ctrl Pts',(16.053754820006,14.0332502522502,5.49930162637244));
#128977=CARTESIAN_POINT('Ctrl Pts',(16.0555819563119,14.0332718459438,5.46940975039724));
#128978=CARTESIAN_POINT('Ctrl Pts',(16.057436656885,14.0346798156171,5.43953772406872));
#128979=CARTESIAN_POINT('Ctrl Pts',(16.0598841511539,14.0382394990734,5.40155965248761));
#128980=CARTESIAN_POINT('Ctrl Pts',(16.0604187513643,14.0391154732059,5.39334786253083));
#128981=CARTESIAN_POINT('Ctrl Pts',(16.0612629771265,14.0406489664404,5.38053124940146));
#128982=CARTESIAN_POINT('Ctrl Pts',(16.0615688488107,14.0412347263295,5.37591802802548));
#128983=CARTESIAN_POINT('Ctrl Pts',(16.0622130668265,14.0425305617261,5.36627008813138));
#128984=CARTESIAN_POINT('Ctrl Pts',(16.0625517873068,14.0432471089392,5.36123647498748));
#128985=CARTESIAN_POINT('Ctrl Pts',(16.0634214757567,14.0451769564426,5.34840585914653));
#128986=CARTESIAN_POINT('Ctrl Pts',(16.0639553143812,14.0464460612491,5.34061774197943));
#128987=CARTESIAN_POINT('Ctrl Pts',(16.0663566565632,14.0525344365228,5.30593535241904));
#128988=CARTESIAN_POINT('Ctrl Pts',(16.0682694646484,14.0583968933431,5.27923903652652));
#128989=CARTESIAN_POINT('Ctrl Pts',(16.0750854160738,14.0829892584866,5.18624867227684));
#128990=CARTESIAN_POINT('Ctrl Pts',(16.0800765446964,14.1076639584807,5.12173240742865));
#128991=CARTESIAN_POINT('Ctrl Pts',(16.0870558284045,14.1530248046447,5.03289004412398));
#128992=CARTESIAN_POINT('Ctrl Pts',(16.0891806549669,14.1683738677505,5.00607995663884));
#128993=CARTESIAN_POINT('Ctrl Pts',(16.0920883336116,14.191578068668,4.96970764348981));
#128994=CARTESIAN_POINT('Ctrl Pts',(16.0929079081642,14.1983712564409,4.95949340138138));
#128995=CARTESIAN_POINT('Ctrl Pts',(16.0942974387616,14.210319119209,4.94224954269159));
#128996=CARTESIAN_POINT('Ctrl Pts',(16.0948708566776,14.215377689847,4.93515550387149));
#128997=CARTESIAN_POINT('Ctrl Pts',(16.0960432973002,14.2259818498573,4.92070184048405));
#128998=CARTESIAN_POINT('Ctrl Pts',(16.0966418341509,14.2315381593906,4.91335115833387));
#128999=CARTESIAN_POINT('Ctrl Pts',(16.0981703737362,14.2460893286805,4.89466233865598));
#129000=CARTESIAN_POINT('Ctrl Pts',(16.0990944271931,14.2552353971504,4.88344448320808));
#129001=CARTESIAN_POINT('Ctrl Pts',(16.1011050177788,14.2758737295597,4.85926081712003));
#129002=CARTESIAN_POINT('Ctrl Pts',(16.1021873478148,14.2874696480597,4.84638994532465));
#129003=CARTESIAN_POINT('Ctrl Pts',(16.1055902500676,14.3253562935794,4.80654508529898));
#129004=CARTESIAN_POINT('Ctrl Pts',(16.1078682504463,14.3528806535515,4.78079164693743));
#129005=CARTESIAN_POINT('Ctrl Pts',(16.1139258859375,14.4301931704857,4.71649434272923));
#129006=CARTESIAN_POINT('Ctrl Pts',(16.117670177814,14.4823506215545,4.68109946682399));
#129007=CARTESIAN_POINT('Ctrl Pts',(16.1223188099944,14.5464647938768,4.64617680842324));
#129008=CARTESIAN_POINT('Ctrl Pts',(16.1229705672337,14.5554379546427,4.64147056287598));
#129009=CARTESIAN_POINT('Ctrl Pts',(16.1239958646515,14.5694939218463,4.63437792200988));
#129010=CARTESIAN_POINT('Ctrl Pts',(16.1243638230733,14.574526620658,4.63189317193628));
#129011=CARTESIAN_POINT('Ctrl Pts',(16.1250607111793,14.5840290738574,4.62730408717964));
#129012=CARTESIAN_POINT('Ctrl Pts',(16.1253890620748,14.5884937611469,4.62518997569645));
#129013=CARTESIAN_POINT('Ctrl Pts',(16.126192815156,14.5993953378329,4.62012979386847));
#129014=CARTESIAN_POINT('Ctrl Pts',(16.1266702639879,14.6058486684773,4.61722007520581));
#129015=CARTESIAN_POINT('Ctrl Pts',(16.1284711138808,14.6301269272565,4.60659261258317));
#129016=CARTESIAN_POINT('Ctrl Pts',(16.129817186576,14.6481501389731,4.59934223363141));
#129017=CARTESIAN_POINT('Ctrl Pts',(16.1335846756384,14.6985543858762,4.58080938405562));
#129018=CARTESIAN_POINT('Ctrl Pts',(16.1360375367235,14.7313358084232,4.5706990887894));
#129019=CARTESIAN_POINT('Ctrl Pts',(16.1433672498332,14.8306037706531,4.54577573045922));
#129020=CARTESIAN_POINT('Ctrl Pts',(16.1482149169212,14.8982011135298,4.53621636898596));
#129021=CARTESIAN_POINT('Ctrl Pts',(16.1539109873521,14.9818674666426,4.53329375290289));
#129022=CARTESIAN_POINT('Ctrl Pts',(16.1549631029394,14.9974963037979,4.53312692868293));
#129023=CARTESIAN_POINT('Ctrl Pts',(16.1566326969434,15.0225677401307,4.53346729123608));
#129024=CARTESIAN_POINT('Ctrl Pts',(16.1572573791698,15.0320102538792,4.53373392160617));
#129025=CARTESIAN_POINT('Ctrl Pts',(16.1584498772752,15.0501484063339,4.53451227727555));
#129026=CARTESIAN_POINT('Ctrl Pts',(16.1590182710538,15.0588439629896,4.53500321163347));
#129027=CARTESIAN_POINT('Ctrl Pts',(16.1603407678721,15.0791848369827,4.53642759482995));
#129028=CARTESIAN_POINT('Ctrl Pts',(16.1610919300268,15.0908223665397,4.53745476216955));
#129029=CARTESIAN_POINT('Ctrl Pts',(16.1636690133816,15.1309975136282,4.54173590611325));
#129030=CARTESIAN_POINT('Ctrl Pts',(16.1654627657949,15.1594080479737,4.54605046192239));
#129031=CARTESIAN_POINT('Ctrl Pts',(16.1701640731988,15.2343399312697,4.56087180181358));
#129032=CARTESIAN_POINT('Ctrl Pts',(16.1730172316831,15.2803461713758,4.57356422097476));
#129033=CARTESIAN_POINT('Ctrl Pts',(16.1787162285089,15.3694052072202,4.60537950240581));
#129034=CARTESIAN_POINT('Ctrl Pts',(16.1815549913394,15.4123684772372,4.62435319659485));
#129035=CARTESIAN_POINT('Ctrl Pts',(16.185210668159,15.4631481152362,4.65134698056224));
#129036=CARTESIAN_POINT('Ctrl Pts',(16.1858922141997,15.4724331653336,4.65648058310527));
#129037=CARTESIAN_POINT('Ctrl Pts',(16.1869543414194,15.486586057409,4.6646125304026));
#129038=CARTESIAN_POINT('Ctrl Pts',(16.1873286887992,15.4915152264921,4.66750315688759));
#129039=CARTESIAN_POINT('Ctrl Pts',(16.1880300502723,15.5006339746254,4.67295990331286));
#129040=CARTESIAN_POINT('Ctrl Pts',(16.188356367525,15.5048300567797,4.67551451943533));
#129041=CARTESIAN_POINT('Ctrl Pts',(16.1891446420696,15.5148576292771,4.68172464765833));
#129042=CARTESIAN_POINT('Ctrl Pts',(16.189608448849,15.5206697978628,4.68541060307389));
#129043=CARTESIAN_POINT('Ctrl Pts',(16.1912929689092,15.5414822470832,4.69892315883016));
#129044=CARTESIAN_POINT('Ctrl Pts',(16.1925328904097,15.5562469401256,4.70910406541835));
#129045=CARTESIAN_POINT('Ctrl Pts',(16.1958922765854,15.5949938927054,4.73744355292568));
#129046=CARTESIAN_POINT('Ctrl Pts',(16.1980364977369,15.6184259371827,4.75632047196069));
#129047=CARTESIAN_POINT('Ctrl Pts',(16.2056416428003,15.697989998802,4.82678158290062));
#129048=CARTESIAN_POINT('Ctrl Pts',(16.2110918332478,15.748878039024,4.88388414344253));
#129049=CARTESIAN_POINT('Ctrl Pts',(16.2172569433786,15.8009026229382,4.95835979279725));
#129050=CARTESIAN_POINT('Ctrl Pts',(16.2182388589736,15.8089990149851,4.97052879371185));
#129051=CARTESIAN_POINT('Ctrl Pts',(16.2198252972878,15.8217604464134,4.99068600300294));
#129052=CARTESIAN_POINT('Ctrl Pts',(16.2204357789459,15.8265920278571,4.99856544970122));
#129053=CARTESIAN_POINT('Ctrl Pts',(16.2216193473308,15.8357999017637,5.01407670127965));
#129054=CARTESIAN_POINT('Ctrl Pts',(16.2221927588863,15.8401864708521,5.02170131654289));
#129055=CARTESIAN_POINT('Ctrl Pts',(16.2235557245544,15.8504287389778,5.04007997375903));
#129056=CARTESIAN_POINT('Ctrl Pts',(16.2243417740469,15.8561854728063,5.05088762188908));
#129057=CARTESIAN_POINT('Ctrl Pts',(16.227239467204,15.8768169956357,5.09146042536855));
#129058=CARTESIAN_POINT('Ctrl Pts',(16.2293063746298,15.8903581951927,5.12187933196215));
#129059=CARTESIAN_POINT('Ctrl Pts',(16.2352954848077,15.9254941227428,5.21322716348978));
#129060=CARTESIAN_POINT('Ctrl Pts',(16.2391088623504,15.9425817734535,5.27568512856025));
#129061=CARTESIAN_POINT('Ctrl Pts',(16.2448166196166,15.9580729218002,5.367627419638));
#129062=CARTESIAN_POINT('Ctrl Pts',(16.2465970441174,15.9615741159089,5.39607148352723));
#129063=CARTESIAN_POINT('Ctrl Pts',(16.2489608799098,15.9644455666248,5.43278878124079));
#129064=CARTESIAN_POINT('Ctrl Pts',(16.2494910307638,15.9649801737885,5.44095889178846));
#129065=CARTESIAN_POINT('Ctrl Pts',(16.2503298970423,15.9656549013487,5.45376499970002));
#129066=CARTESIAN_POINT('Ctrl Pts',(16.2506349383385,15.96586554976,5.45839709914998));
#129067=CARTESIAN_POINT('Ctrl Pts',(16.251279245037,15.9662378066673,5.46812445058905));
#129068=CARTESIAN_POINT('Ctrl Pts',(16.2516189049702,15.9663924479576,5.473219742582));
#129069=CARTESIAN_POINT('Ctrl Pts',(16.2524940798626,15.9666852625476,5.48627107258372));
#129070=CARTESIAN_POINT('Ctrl Pts',(16.2530325341783,15.9667655109834,5.49422790787831));
#129071=CARTESIAN_POINT('Ctrl Pts',(16.2554955991826,15.9666839199583,5.53033580943649));
#129072=CARTESIAN_POINT('Ctrl Pts',(16.2574683007548,15.9653907052195,5.55846845862868));
#129073=CARTESIAN_POINT('Ctrl Pts',(16.2647895119291,15.9561536310308,5.66128852147467));
#129074=CARTESIAN_POINT('Ctrl Pts',(16.2702333969029,15.940743235831,5.73504947665471));
#129075=CARTESIAN_POINT('Ctrl Pts',(16.2772266606601,15.9088359282518,5.83057313849593));
#129076=CARTESIAN_POINT('Ctrl Pts',(16.2789785324675,15.8997603374191,5.85453191607225));
#129077=CARTESIAN_POINT('Ctrl Pts',(16.2814650842699,15.8852922571526,5.88857778491875));
#129078=CARTESIAN_POINT('Ctrl Pts',(16.2822239390347,15.8806565489891,5.89897260156269));
#129079=CARTESIAN_POINT('Ctrl Pts',(16.2835517291197,15.8721571675057,5.91716068530542));
#129080=CARTESIAN_POINT('Ctrl Pts',(16.2841231560472,15.8683699337616,5.92498803342029));
#129081=CARTESIAN_POINT('Ctrl Pts',(16.2853107069492,15.8602299270374,5.94124830887897));
#129082=CARTESIAN_POINT('Ctrl Pts',(16.2859260842179,15.8558575379562,5.94967041546211));
#129083=CARTESIAN_POINT('Ctrl Pts',(16.2875577939642,15.8438563384391,5.97197774949159));
#129084=CARTESIAN_POINT('Ctrl Pts',(16.2885664745828,15.8360088712636,5.98574244971829));
#129085=CARTESIAN_POINT('Ctrl Pts',(16.2926839045276,15.8022629910539,6.04169125814592));
#129086=CARTESIAN_POINT('Ctrl Pts',(16.2956914034513,15.7734815322143,6.08205013252692));
#129087=CARTESIAN_POINT('Ctrl Pts',(16.3021599277745,15.7046674943836,6.16437131770244));
#129088=CARTESIAN_POINT('Ctrl Pts',(16.3055992079153,15.663704117734,6.20529508273831));
#129089=CARTESIAN_POINT('Ctrl Pts',(16.3101749489064,15.6076863394042,6.2520326389051));
#129090=CARTESIAN_POINT('Ctrl Pts',(16.3111390442231,15.5958094859388,6.26147670762929));
#129091=CARTESIAN_POINT('Ctrl Pts',(16.3125067639051,15.5789534788129,6.27424423018538));
#129092=CARTESIAN_POINT('Ctrl Pts',(16.3128958436033,15.5741576632889,6.27780732316254));
#129093=CARTESIAN_POINT('Ctrl Pts',(16.3136121387264,15.5653349339167,6.28423618964113));
#129094=CARTESIAN_POINT('Ctrl Pts',(16.3139384238034,15.5613185732635,6.28711590440737));
#129095=CARTESIAN_POINT('Ctrl Pts',(16.3146393646178,15.5526996209826,6.29319613851485));
#129096=CARTESIAN_POINT('Ctrl Pts',(16.3150145322228,15.5480912150758,6.29638746936009));
#129097=CARTESIAN_POINT('Ctrl Pts',(16.3160916029437,15.5348671155656,6.30537604157011));
#129098=CARTESIAN_POINT('Ctrl Pts',(16.3167992844313,15.526185680561,6.31107460096355));
#129099=CARTESIAN_POINT('Ctrl Pts',(16.3201163458357,15.4854549542159,6.33688141864371));
#129100=CARTESIAN_POINT('Ctrl Pts',(16.3228032263679,15.4523368304037,6.35523559072662));
#129101=CARTESIAN_POINT('Ctrl Pts',(16.3307390306942,15.3522597246387,6.40325693894611));
#129102=CARTESIAN_POINT('Ctrl Pts',(16.3359912106291,15.2828951386583,6.42732600845898));
#129103=CARTESIAN_POINT('Ctrl Pts',(16.3422235840022,15.1940225214801,6.44724896933727));
#129104=CARTESIAN_POINT('Ctrl Pts',(16.3434330740238,15.176466966323,6.45067598539669));
#129105=CARTESIAN_POINT('Ctrl Pts',(16.345295180927,15.1489663819463,6.4552562361265));
#129106=CARTESIAN_POINT('Ctrl Pts',(16.3459579893046,15.1390821658714,6.45674532835271));
#129107=CARTESIAN_POINT('Ctrl Pts',(16.347182567944,15.1206490448173,6.45923063267351));
#129108=CARTESIAN_POINT('Ctrl Pts',(16.3477455081437,15.1121065874911,6.46026648364706));
#129109=CARTESIAN_POINT('Ctrl Pts',(16.3490012102111,15.0929047273911,6.46233514805039));
#129110=CARTESIAN_POINT('Ctrl Pts',(16.3496919785407,15.0822396054252,6.46330518915648));
#129111=CARTESIAN_POINT('Ctrl Pts',(16.3518074732707,15.0492888858854,6.4657509581501));
#129112=CARTESIAN_POINT('Ctrl Pts',(16.3532141709048,15.0269658218279,6.46663191895112));
#129113=CARTESIAN_POINT('Ctrl Pts',(16.3565700675411,14.972988426526,6.46689048349058));
#129114=CARTESIAN_POINT('Ctrl Pts',(16.3584985430995,14.941356136694,6.46548843927558));
#129115=CARTESIAN_POINT('Ctrl Pts',(16.3642716971533,14.8462900695013,6.45658448504985));
#129116=CARTESIAN_POINT('Ctrl Pts',(16.3680484538433,14.7834840701583,6.44435164053158));
#129117=CARTESIAN_POINT('Ctrl Pts',(16.3730332238562,14.7072178167024,6.42148448941474));
#129118=CARTESIAN_POINT('Ctrl Pts',(16.3740353051051,14.6922018603671,6.41657804507553));
#129119=CARTESIAN_POINT('Ctrl Pts',(16.3754520638716,14.6715342055773,6.40925979595582));
#129120=CARTESIAN_POINT('Ctrl Pts',(16.3758510071461,14.665774370436,6.40715840873849));
#129121=CARTESIAN_POINT('Ctrl Pts',(16.3765761119717,14.6554224610014,6.4032697054944));
#129122=CARTESIAN_POINT('Ctrl Pts',(16.3769011878553,14.6508232350615,6.40150176212317));
#129123=CARTESIAN_POINT('Ctrl Pts',(16.3775931230447,14.6411260930492,6.39768883801965));
#129124=CARTESIAN_POINT('Ctrl Pts',(16.3779604224687,14.6360318313754,6.39563547252004));
#129125=CARTESIAN_POINT('Ctrl Pts',(16.3789919111365,14.6218656165419,6.38978462049598));
#129126=CARTESIAN_POINT('Ctrl Pts',(16.3796611730217,14.612833968551,6.38589205264213));
#129127=CARTESIAN_POINT('Ctrl Pts',(16.3836687509982,14.5596026171385,6.36198031061316));
#129128=CARTESIAN_POINT('Ctrl Pts',(16.3871400720182,14.5169049940767,6.33879574815456));
#129129=CARTESIAN_POINT('Ctrl Pts',(16.3954742107645,14.4190986987596,6.27573465308383));
#129130=CARTESIAN_POINT('Ctrl Pts',(16.400306105088,14.3660865474963,6.23305330499322));
#129131=CARTESIAN_POINT('Ctrl Pts',(16.4059868914364,14.3069109109654,6.17414900444205));
#129132=CARTESIAN_POINT('Ctrl Pts',(16.4070381380039,14.2961126589939,6.16286652063453));
#129133=CARTESIAN_POINT('Ctrl Pts',(16.4087067033969,14.2792299066624,6.14434866722932));
#129134=CARTESIAN_POINT('Ctrl Pts',(16.4093312101,14.2729703044962,6.13727746300967));
#129135=CARTESIAN_POINT('Ctrl Pts',(16.410523584144,14.2611382889258,6.12351005784185));
#129136=CARTESIAN_POINT('Ctrl Pts',(16.4110920264144,14.2555508324878,6.11682806799188));
#129137=CARTESIAN_POINT('Ctrl Pts',(16.4124149520153,14.2426788650934,6.10100487352368));
#129138=CARTESIAN_POINT('Ctrl Pts',(16.4131664884989,14.2354682233647,6.09180515428526));
#129139=CARTESIAN_POINT('Ctrl Pts',(16.4157377233576,14.2111799663433,6.05963186357591));
#129140=CARTESIAN_POINT('Ctrl Pts',(16.4175255265102,14.1949560879664,6.03603114700165));
#129141=CARTESIAN_POINT('Ctrl Pts',(16.4222100246314,14.1546708132903,5.97146385631119));
#129142=CARTESIAN_POINT('Ctrl Pts',(16.4250527344463,14.1325402281817,5.92938723815914));
#129143=CARTESIAN_POINT('Ctrl Pts',(16.4307339682298,14.0949094875043,5.84293924459934));
#129144=CARTESIAN_POINT('Ctrl Pts',(16.4335655236157,14.0793719926254,5.79872946429754));
#129145=CARTESIAN_POINT('Ctrl Pts',(16.4372258037383,14.0642575755087,5.74312335052918));
#129146=CARTESIAN_POINT('Ctrl Pts',(16.437921091114,14.061592897999,5.73262617341984));
#129147=CARTESIAN_POINT('Ctrl Pts',(16.4390001810718,14.0577819076502,5.71648051314522));
#129148=CARTESIAN_POINT('Ctrl Pts',(16.4393774384625,14.0565087467374,5.71086250755645));
#129149=CARTESIAN_POINT('Ctrl Pts',(16.4400484530062,14.0543498145954,5.70092469376081));
#129150=CARTESIAN_POINT('Ctrl Pts',(16.440341062479,14.0534432703204,5.69660966509531));
#129151=CARTESIAN_POINT('Ctrl Pts',(16.4409560897577,14.051610135042,5.68757754432826));
#129152=CARTESIAN_POINT('Ctrl Pts',(16.4412787784145,14.0506891607529,5.68285950682528));
#129153=CARTESIAN_POINT('Ctrl Pts',(16.442038790653,14.048614225378,5.67179151136174));
#129154=CARTESIAN_POINT('Ctrl Pts',(16.4424774909826,14.0474886042698,5.66543654796761));
#129155=CARTESIAN_POINT('Ctrl Pts',(16.4439142669754,14.0440324656431,5.64471824224573));
#129156=CARTESIAN_POINT('Ctrl Pts',(16.4449233431192,14.0419626826163,5.63031403658809));
#129157=CARTESIAN_POINT('Ctrl Pts',(16.4486344742756,14.0356099088061,5.57769211828947));
#129158=CARTESIAN_POINT('Ctrl Pts',(16.4513896445024,14.0332831717413,5.53927576511434));
#129159=CARTESIAN_POINT('Ctrl Pts',(16.4541432617404,14.0332503521631,5.50082517101239));
#129160=CARTESIAN_POINT('Origin',(16.125,15.,5.5));
#129161=CARTESIAN_POINT('',(16.911384655308,14.033250032487,5.49974937350518));
#129162=CARTESIAN_POINT('',(16.8550925403241,14.0332500296882,5.49976041261023));
#129163=CARTESIAN_POINT('',(16.125,14.03325,5.5));
#129164=CARTESIAN_POINT('Ctrl Pts',(16.9113846553004,14.033250032487,5.49974937361882));
#129165=CARTESIAN_POINT('Ctrl Pts',(16.910722591978,14.0332474586815,5.50967740409213));
#129166=CARTESIAN_POINT('Ctrl Pts',(16.9100652231276,14.0333978184175,5.5196051809349));
#129167=CARTESIAN_POINT('Ctrl Pts',(16.908823664226,14.0339746734881,5.5384819026576));
#129168=CARTESIAN_POINT('Ctrl Pts',(16.9082386691869,14.0343726731809,5.54743061083325));
#129169=CARTESIAN_POINT('Ctrl Pts',(16.9068951742441,14.0355799149497,5.56809866600091));
#129170=CARTESIAN_POINT('Ctrl Pts',(16.9061394777521,14.036478505235,5.5798115085104));
#129171=CARTESIAN_POINT('Ctrl Pts',(16.9036296233975,14.0402011406127,5.61896435540944));
#129172=CARTESIAN_POINT('Ctrl Pts',(16.901904477747,14.0439860138778,5.64630047089543));
#129173=CARTESIAN_POINT('Ctrl Pts',(16.8974906322489,14.0568296250312,5.71672920919216));
#129174=CARTESIAN_POINT('Ctrl Pts',(16.8948465495084,14.0676708796551,5.75943127139042));
#129175=CARTESIAN_POINT('Ctrl Pts',(16.8890682674937,14.0975656420813,5.85059168347836));
#129176=CARTESIAN_POINT('Ctrl Pts',(16.8859409490176,14.1176953015698,5.89854672736554));
#129177=CARTESIAN_POINT('Ctrl Pts',(16.8819682217545,14.1464272611037,5.95401591983493));
#129178=CARTESIAN_POINT('Ctrl Pts',(16.8812902124078,14.1514326801779,5.96330374323185));
#129179=CARTESIAN_POINT('Ctrl Pts',(16.8802253161108,14.1594291590603,5.97757721348987));
#129180=CARTESIAN_POINT('Ctrl Pts',(16.879844470719,14.1623150406497,5.98262121606706));
#129181=CARTESIAN_POINT('Ctrl Pts',(16.879123258347,14.1678242279252,5.99205199962114));
#129182=CARTESIAN_POINT('Ctrl Pts',(16.8787835116746,14.1704371221735,5.9964444710351));
#129183=CARTESIAN_POINT('Ctrl Pts',(16.8779493048055,14.1768974477284,6.0071113500585));
#129184=CARTESIAN_POINT('Ctrl Pts',(16.8774526251604,14.1807818848317,6.0133628391683));
#129185=CARTESIAN_POINT('Ctrl Pts',(16.8755515649647,14.1958065530678,6.03693824574563));
#129186=CARTESIAN_POINT('Ctrl Pts',(16.8741218860787,14.2074273600083,6.05394788509376));
#129187=CARTESIAN_POINT('Ctrl Pts',(16.8700335599523,14.2417646883502,6.10091388255471));
#129188=CARTESIAN_POINT('Ctrl Pts',(16.8673386323229,14.2656976179819,6.12993497786153));
#129189=CARTESIAN_POINT('Ctrl Pts',(16.8602082266237,14.3334494297738,6.20296833316082));
#129190=CARTESIAN_POINT('Ctrl Pts',(16.8558064878986,14.3799265831757,6.24428844486873));
#129191=CARTESIAN_POINT('Ctrl Pts',(16.8504771195553,14.4431241602897,6.29041562587712));
#129192=CARTESIAN_POINT('Ctrl Pts',(16.849386414791,14.4564366207541,6.29962895636266));
#129193=CARTESIAN_POINT('Ctrl Pts',(16.8476576294941,14.478138894016,6.31385615695651));
#129194=CARTESIAN_POINT('Ctrl Pts',(16.8470118332279,14.4863837594538,6.31908438348582));
#129195=CARTESIAN_POINT('Ctrl Pts',(16.8457789939215,14.5023836374572,6.32889360377174));
#129196=CARTESIAN_POINT('Ctrl Pts',(16.8451913415545,14.510126203826,6.33349284546529));
#129197=CARTESIAN_POINT('Ctrl Pts',(16.8438223172555,14.5284283177165,6.34402152846769));
#129198=CARTESIAN_POINT('Ctrl Pts',(16.8430441167207,14.5390373842813,6.34986215334015));
#129199=CARTESIAN_POINT('Ctrl Pts',(16.8403441665956,14.5765263065262,6.36959237410414));
#129200=CARTESIAN_POINT('Ctrl Pts',(16.8384581922771,14.6039470660083,6.38241894544169));
#129201=CARTESIAN_POINT('Ctrl Pts',(16.8333947240324,14.6801690559781,6.41380284982873));
#129202=CARTESIAN_POINT('Ctrl Pts',(16.8302832731761,14.7299403522012,6.42972868612837));
#129203=CARTESIAN_POINT('Ctrl Pts',(16.8247147870982,14.819658492454,6.45061984351347));
#129204=CARTESIAN_POINT('Ctrl Pts',(16.8222788972086,14.8590827936255,6.45725798414191));
#129205=CARTESIAN_POINT('Ctrl Pts',(16.8190621143444,14.9094068158703,6.46255502989904));
#129206=CARTESIAN_POINT('Ctrl Pts',(16.8183769500227,14.9200307357841,6.46349582533969));
#129207=CARTESIAN_POINT('Ctrl Pts',(16.8173032070364,14.936488176329,6.46467915180172));
#129208=CARTESIAN_POINT('Ctrl Pts',(16.8169208292091,14.9423123203824,6.46504494458908));
#129209=CARTESIAN_POINT('Ctrl Pts',(16.8161986025968,14.9532355788995,6.46563176163025));
#129210=CARTESIAN_POINT('Ctrl Pts',(16.8158594038163,14.958333685168,6.46586516840361));
#129211=CARTESIAN_POINT('Ctrl Pts',(16.8150291884122,14.9707377684582,6.46633468153167));
#129212=CARTESIAN_POINT('Ctrl Pts',(16.8145360044032,14.978044920341,6.46652830351683));
#129213=CARTESIAN_POINT('Ctrl Pts',(16.8126667326163,15.0055368568391,6.46694486690711));
#129214=CARTESIAN_POINT('Ctrl Pts',(16.8112663728499,15.0257235704931,6.46661843878813));
#129215=CARTESIAN_POINT('Ctrl Pts',(16.8073003940887,15.0821330983503,6.46393812402135));
#129216=CARTESIAN_POINT('Ctrl Pts',(16.8047006255862,15.1182553128496,6.46017603440518));
#129217=CARTESIAN_POINT('Ctrl Pts',(16.797520420676,15.2172740764911,6.44419026845684));
#129218=CARTESIAN_POINT('Ctrl Pts',(16.7929727018695,15.2793090980343,6.42773493158762));
#129219=CARTESIAN_POINT('Ctrl Pts',(16.7875152258932,15.3543498916327,6.3996116407535));
#129220=CARTESIAN_POINT('Ctrl Pts',(16.7864301411606,15.3692881794249,6.39358337175345));
#129221=CARTESIAN_POINT('Ctrl Pts',(16.7847079960367,15.3930133570444,6.38331254069949));
#129222=CARTESIAN_POINT('Ctrl Pts',(16.7840633258956,15.4018982705841,6.37930559823286));
#129223=CARTESIAN_POINT('Ctrl Pts',(16.7828312746443,15.4188782708008,6.37133675834002));
#129224=CARTESIAN_POINT('Ctrl Pts',(16.7822433039227,15.4269814876039,6.36739470278409));
#129225=CARTESIAN_POINT('Ctrl Pts',(16.7808714812237,15.445877599647,6.35787313357056));
#129226=CARTESIAN_POINT('Ctrl Pts',(16.7800908408755,15.4566229172235,6.35220225272463));
#129227=CARTESIAN_POINT('Ctrl Pts',(16.7773691929045,15.4940131424312,6.33155910860444));
#129228=CARTESIAN_POINT('Ctrl Pts',(16.7754647837142,15.5200535215782,6.31552690515192));
#129229=CARTESIAN_POINT('Ctrl Pts',(16.7703198165967,15.5892428407727,6.26826515838282));
#129230=CARTESIAN_POINT('Ctrl Pts',(16.7671483833251,15.6306385652376,6.23466564678162));
#129231=CARTESIAN_POINT('Ctrl Pts',(16.7613904788051,15.6993397794273,6.16879686047644));
#129232=CARTESIAN_POINT('Ctrl Pts',(16.7588265489346,15.7276954720618,6.13782746089455));
#129233=CARTESIAN_POINT('Ctrl Pts',(16.7555740984933,15.7594917242494,6.09821095266105));
#129234=CARTESIAN_POINT('Ctrl Pts',(16.7550016647922,15.7649406602564,6.09122736417949));
#129235=CARTESIAN_POINT('Ctrl Pts',(16.7540704140971,15.7735534701889,6.07987042712077));
#129236=CARTESIAN_POINT('Ctrl Pts',(16.7537155401315,15.7767781464483,6.07554356157806));
#129237=CARTESIAN_POINT('Ctrl Pts',(16.7530040964841,15.7831248005238,6.0668771352577));
#129238=CARTESIAN_POINT('Ctrl Pts',(16.7526475803723,15.7862473360622,6.06253823203378));
#129239=CARTESIAN_POINT('Ctrl Pts',(16.751710399795,15.7943096013112,6.05113709303652));
#129240=CARTESIAN_POINT('Ctrl Pts',(16.7511261850026,15.7991910527928,6.04403445361888));
#129241=CARTESIAN_POINT('Ctrl Pts',(16.7480641970405,15.8240649718226,6.0067849656158));
#129242=CARTESIAN_POINT('Ctrl Pts',(16.7455082066664,15.8424471174724,5.9756011215326));
#129243=CARTESIAN_POINT('Ctrl Pts',(16.7369345298998,15.8975883232977,5.86878676568718));
#129244=CARTESIAN_POINT('Ctrl Pts',(16.7308865213051,15.9262454603174,5.78938371741908));
#129245=CARTESIAN_POINT('Ctrl Pts',(16.7241710170971,15.9474549918226,5.69275706396799));
#129246=CARTESIAN_POINT('Ctrl Pts',(16.7231726720834,15.9503052055342,5.67817492650931));
#129247=CARTESIAN_POINT('Ctrl Pts',(16.7215531045044,15.954424851388,5.65417185932061));
#129248=CARTESIAN_POINT('Ctrl Pts',(16.7209258393961,15.9558933917605,5.64478809852231));
#129249=CARTESIAN_POINT('Ctrl Pts',(16.7197041340052,15.9585015896906,5.62634700166048));
#129250=CARTESIAN_POINT('Ctrl Pts',(16.7191094309115,15.9596517159774,5.6172921804736));
#129251=CARTESIAN_POINT('Ctrl Pts',(16.7176847048384,15.9621154734428,5.59542174078066));
#129252=CARTESIAN_POINT('Ctrl Pts',(16.7168586575583,15.963301541918,5.58259332227013));
#129253=CARTESIAN_POINT('Ctrl Pts',(16.7136804158573,15.9669085881357,5.53272525118239));
#129254=CARTESIAN_POINT('Ctrl Pts',(16.7113847200973,15.967452350495,5.49558023103665));
#129255=CARTESIAN_POINT('Ctrl Pts',(16.7066924784334,15.9641469321776,5.41866437599519));
#129256=CARTESIAN_POINT('Ctrl Pts',(16.7043057034882,15.9599734353505,5.3789798938508));
#129257=CARTESIAN_POINT('Ctrl Pts',(16.6992901692353,15.946190672637,5.29702625274794));
#129258=CARTESIAN_POINT('Ctrl Pts',(16.6966634366622,15.936167777227,5.25491990815527));
#129259=CARTESIAN_POINT('Ctrl Pts',(16.6932293609409,15.9201576196384,5.20329717744535));
#129260=CARTESIAN_POINT('Ctrl Pts',(16.6925346250582,15.9167797964256,5.19301890619807));
#129261=CARTESIAN_POINT('Ctrl Pts',(16.6914490538474,15.9113049731542,5.17725669058079));
#129262=CARTESIAN_POINT('Ctrl Pts',(16.691064635239,15.909329199215,5.17173120609542));
#129263=CARTESIAN_POINT('Ctrl Pts',(16.6903410072991,15.9055443871085,5.16144294438672));
#129264=CARTESIAN_POINT('Ctrl Pts',(16.6900024871061,15.9037478135518,5.15667595237395));
#129265=CARTESIAN_POINT('Ctrl Pts',(16.6891773534538,15.8993049996095,5.14516401496963));
#129266=CARTESIAN_POINT('Ctrl Pts',(16.6886886391605,15.8966204877207,5.13843430488806));
#129267=CARTESIAN_POINT('Ctrl Pts',(16.6868591227057,15.8863663849603,5.11354528287289));
#129268=CARTESIAN_POINT('Ctrl Pts',(16.6854953014026,15.8783190947426,5.09558923301205));
#129269=CARTESIAN_POINT('Ctrl Pts',(16.6816779497534,15.8545668166931,5.04664890168829));
#129270=CARTESIAN_POINT('Ctrl Pts',(16.6791928053261,15.837731393548,5.01624638270794));
#129271=CARTESIAN_POINT('Ctrl Pts',(16.6719404923326,15.7839566058063,4.93039481894949));
#129272=CARTESIAN_POINT('Ctrl Pts',(16.6672034656906,15.7428760795483,4.87776546378233));
#129273=CARTESIAN_POINT('Ctrl Pts',(16.6615859365329,15.6856637005044,4.81829292537741));
#129274=CARTESIAN_POINT('Ctrl Pts',(16.6605132186048,15.6743390377175,4.8070886361339));
#129275=CARTESIAN_POINT('Ctrl Pts',(16.6588056894579,15.655672637336,4.78951196712998));
#129276=CARTESIAN_POINT('Ctrl Pts',(16.6581634997823,15.6485030753689,4.78296190831898));
#129277=CARTESIAN_POINT('Ctrl Pts',(16.6569331410993,15.6344828706865,4.77053548728371));
#129278=CARTESIAN_POINT('Ctrl Pts',(16.656344426411,15.6276462738187,4.76464488001068));
#129279=CARTESIAN_POINT('Ctrl Pts',(16.6549662139003,15.6113458091015,4.75099290076047));
#129280=CARTESIAN_POINT('Ctrl Pts',(16.6541800195706,15.6018149326939,4.74331371020866));
#129281=CARTESIAN_POINT('Ctrl Pts',(16.6514080857931,15.5674193807995,4.71666171008277));
#129282=CARTESIAN_POINT('Ctrl Pts',(16.6494608937632,15.5417818957345,4.69871585199138));
#129283=CARTESIAN_POINT('Ctrl Pts',(16.6441196988179,15.4681169165145,4.65230649772788));
#129284=CARTESIAN_POINT('Ctrl Pts',(16.6408026374728,15.4184317689345,4.62671160424633));
#129285=CARTESIAN_POINT('Ctrl Pts',(16.6350836845776,15.3311617802197,4.59092217403918));
#129286=CARTESIAN_POINT('Ctrl Pts',(16.6327189763895,15.2946684535178,4.57844670472949));
#129287=CARTESIAN_POINT('Ctrl Pts',(16.6296873015446,15.249037595778,4.56583539152958));
#129288=CARTESIAN_POINT('Ctrl Pts',(16.6291176473684,15.2405112397574,4.56360394578876));
#129289=CARTESIAN_POINT('Ctrl Pts',(16.6281898135247,15.2267263023727,4.56019695364344));
#129290=CARTESIAN_POINT('Ctrl Pts',(16.6278355249798,15.2214861144497,4.55894820555222));
#129291=CARTESIAN_POINT('Ctrl Pts',(16.6271240585719,15.2110169650254,4.55654566888808));
#129292=CARTESIAN_POINT('Ctrl Pts',(16.6267669193632,15.2057883137802,4.55539140341949));
#129293=CARTESIAN_POINT('Ctrl Pts',(16.6258262241626,15.192078412871,4.55248406344509));
#129294=CARTESIAN_POINT('Ctrl Pts',(16.625239071707,15.1835829077889,4.5508014590996));
#129295=CARTESIAN_POINT('Ctrl Pts',(16.6221123506709,15.1386083147418,4.54252020987332));
#129296=CARTESIAN_POINT('Ctrl Pts',(16.6194907027615,15.1017977471797,4.53791034808294));
#129297=CARTESIAN_POINT('Ctrl Pts',(16.6109699957622,14.9826570388743,4.52990433464539));
#129298=CARTESIAN_POINT('Ctrl Pts',(16.6050481110505,14.9001097649352,4.53490254373228));
#129299=CARTESIAN_POINT('Ctrl Pts',(16.5984173802141,14.8042454493938,4.55315412532811));
#129300=CARTESIAN_POINT('Ctrl Pts',(16.5973943424893,14.7893708661188,4.5563515663927));
#129301=CARTESIAN_POINT('Ctrl Pts',(16.5957455680379,14.7652732534682,4.56212982900395));
#129302=CARTESIAN_POINT('Ctrl Pts',(16.5951133555927,14.756002666161,4.56449884273853));
#129303=CARTESIAN_POINT('Ctrl Pts',(16.5938891134411,14.7379984196507,4.56938551773038));
#129304=CARTESIAN_POINT('Ctrl Pts',(16.5932967230474,14.729262114151,4.57188947367142));
#129305=CARTESIAN_POINT('Ctrl Pts',(16.5918891745671,14.7084565118162,4.5781714563502));
#129306=CARTESIAN_POINT('Ctrl Pts',(16.5910777428068,14.6964233240763,4.58206389402215));
#129307=CARTESIAN_POINT('Ctrl Pts',(16.588059211781,14.6515723725843,4.59755055430368));
#129308=CARTESIAN_POINT('Ctrl Pts',(16.5859010752542,14.6193106210243,4.61067847553064));
#129309=CARTESIAN_POINT('Ctrl Pts',(16.5793696922586,14.5226075670663,4.65625822629943));
#129310=CARTESIAN_POINT('Ctrl Pts',(16.5751347381663,14.4610394559672,4.6941936334867));
#129311=CARTESIAN_POINT('Ctrl Pts',(16.5693999989503,14.3882122331714,4.75117644735603));
#129312=CARTESIAN_POINT('Ctrl Pts',(16.5681173765514,14.3725624515576,4.76423986104643));
#129313=CARTESIAN_POINT('Ctrl Pts',(16.5663198529068,14.3517137826407,4.7827920595763));
#129314=CARTESIAN_POINT('Ctrl Pts',(16.5658308832474,14.3461480410818,4.78786247339973));
#129315=CARTESIAN_POINT('Ctrl Pts',(16.5650037989226,14.3369221373835,4.79646664092949));
#129316=CARTESIAN_POINT('Ctrl Pts',(16.5646681892916,14.3332294985236,4.79996533190271));
#129317=CARTESIAN_POINT('Ctrl Pts',(16.5639507345624,14.3254471500835,4.80745637165969));
#129318=CARTESIAN_POINT('Ctrl Pts',(16.5635683839398,14.3213650110284,4.81145604917722));
#129319=CARTESIAN_POINT('Ctrl Pts',(16.5624845850809,14.309969797889,4.8228208453607));
#129320=CARTESIAN_POINT('Ctrl Pts',(16.5617774719141,14.3027397517412,4.83026765593785));
#129321=CARTESIAN_POINT('Ctrl Pts',(16.5585435256585,14.2705308679322,4.86452909227338));
#129322=CARTESIAN_POINT('Ctrl Pts',(16.5559443718893,14.2469709234164,4.89263253700157));
#129323=CARTESIAN_POINT('Ctrl Pts',(16.5476205321475,14.1773065216971,4.9860332539458));
#129324=CARTESIAN_POINT('Ctrl Pts',(16.5418885724131,14.137658548171,5.05575003399312));
#129325=CARTESIAN_POINT('Ctrl Pts',(16.5354367067997,14.1012612721259,5.14348682852336));
#129326=CARTESIAN_POINT('Ctrl Pts',(16.5344228548407,14.0958096300957,5.15754889386116));
#129327=CARTESIAN_POINT('Ctrl Pts',(16.5327849463205,14.087449077433,5.18070794742554));
#129328=CARTESIAN_POINT('Ctrl Pts',(16.5321545763732,14.084342171256,5.18973019376714));
#129329=CARTESIAN_POINT('Ctrl Pts',(16.5309313227458,14.0785336025763,5.20744560154263));
#129330=CARTESIAN_POINT('Ctrl Pts',(16.5303381142771,14.0758201505584,5.21613381187037));
#129331=CARTESIAN_POINT('Ctrl Pts',(16.5289244020121,14.0696066304717,5.23706312416377));
#129332=CARTESIAN_POINT('Ctrl Pts',(16.5281077138256,14.0662248220311,5.24933774989583));
#129333=CARTESIAN_POINT('Ctrl Pts',(16.5260929010747,14.0584149444219,5.28004041956747));
#129334=CARTESIAN_POINT('Ctrl Pts',(16.5249038099647,14.0542843225235,5.29853893911191));
#129335=CARTESIAN_POINT('Ctrl Pts',(16.5199014228883,14.0390423622615,5.37766950115862));
#129336=CARTESIAN_POINT('Ctrl Pts',(16.5162320247279,14.0331991100086,5.4391667218192));
#129337=CARTESIAN_POINT('Ctrl Pts',(16.5125067604658,14.0332503338485,5.50080342759133));
#129338=CARTESIAN_POINT('Ctrl Pts',(16.4541432558754,14.033250352233,5.50082525291021));
#129339=CARTESIAN_POINT('Ctrl Pts',(16.4577492683692,14.0332073689333,5.45047209538164));
#129340=CARTESIAN_POINT('Ctrl Pts',(16.4613404233998,14.0370984091453,5.40018751979066));
#129341=CARTESIAN_POINT('Ctrl Pts',(16.4662074935876,14.047961835396,5.33081651676039));
#129342=CARTESIAN_POINT('Ctrl Pts',(16.467567718699,14.0516370512099,5.31130043020353));
#129343=CARTESIAN_POINT('Ctrl Pts',(16.469589386071,14.0580738138264,5.28209728475257));
#129344=CARTESIAN_POINT('Ctrl Pts',(16.4702640356312,14.0603896333483,5.27231841289181));
#129345=CARTESIAN_POINT('Ctrl Pts',(16.4715763064844,14.0652240576706,5.25323624215563));
#129346=CARTESIAN_POINT('Ctrl Pts',(16.4722142356759,14.0677301369894,5.24393100865256));
#129347=CARTESIAN_POINT('Ctrl Pts',(16.4734168511111,14.0727507660036,5.22634081656036));
#129348=CARTESIAN_POINT('Ctrl Pts',(16.4739823312114,14.0752382786214,5.2180491934416));
#129349=CARTESIAN_POINT('Ctrl Pts',(16.4752640657037,14.0811649915053,5.19921651630696));
#129350=CARTESIAN_POINT('Ctrl Pts',(16.4759779790741,14.0846748682881,5.18869886563752));
#129351=CARTESIAN_POINT('Ctrl Pts',(16.4782442391774,14.0964791419248,5.15525372626674));
#129352=CARTESIAN_POINT('Ctrl Pts',(16.4797745564303,14.1054604406175,5.13257782352961));
#129353=CARTESIAN_POINT('Ctrl Pts',(16.4860452502861,14.1462851837861,5.03990462906871));
#129354=CARTESIAN_POINT('Ctrl Pts',(16.4905558747543,14.1855604851074,4.97349795682848));
#129355=CARTESIAN_POINT('Ctrl Pts',(16.4970038522702,14.2495245613705,4.88992069758252));
#129356=CARTESIAN_POINT('Ctrl Pts',(16.4987685818631,14.2677452146626,4.86816713698991));
#129357=CARTESIAN_POINT('Ctrl Pts',(16.5011027970571,14.2922777440739,4.8413662981037));
#129358=CARTESIAN_POINT('Ctrl Pts',(16.5016195100263,14.2977340629855,4.83555159070076));
#129359=CARTESIAN_POINT('Ctrl Pts',(16.5024752131884,14.3067977113262,4.82612896656773));
#129360=CARTESIAN_POINT('Ctrl Pts',(16.5028111621358,14.3103629289267,4.82248078178033));
#129361=CARTESIAN_POINT('Ctrl Pts',(16.5035001287505,14.3176838336843,4.81510716595803));
#129362=CARTESIAN_POINT('Ctrl Pts',(16.5038532788591,14.3214415166913,4.81138405012056));
#129363=CARTESIAN_POINT('Ctrl Pts',(16.5048045640416,14.3315822756947,4.80150017449722));
#129364=CARTESIAN_POINT('Ctrl Pts',(16.5054066243292,14.338019756029,4.79539627912919));
#129365=CARTESIAN_POINT('Ctrl Pts',(16.5093524567836,14.3803912764152,4.75631362258508));
#129366=CARTESIAN_POINT('Ctrl Pts',(16.5128376484093,14.4186902908159,4.72600870603662));
#129367=CARTESIAN_POINT('Ctrl Pts',(16.5196142636065,14.4971245794882,4.67306242555056));
#129368=CARTESIAN_POINT('Ctrl Pts',(16.5228963967761,14.5369225140144,4.65013573330969));
#129369=CARTESIAN_POINT('Ctrl Pts',(16.5282825965558,14.6062192200502,4.61653415054145));
#129370=CARTESIAN_POINT('Ctrl Pts',(16.5304243453575,14.6348804745803,4.60430848344764));
#129371=CARTESIAN_POINT('Ctrl Pts',(16.5333289622871,14.6753303280665,4.58931948725682));
#129372=CARTESIAN_POINT('Ctrl Pts',(16.5341297289252,14.6866529407139,4.58536180141236));
#129373=CARTESIAN_POINT('Ctrl Pts',(16.5355032886334,14.7063640294383,4.57888104168893));
#129374=CARTESIAN_POINT('Ctrl Pts',(16.536079196528,14.7147183361072,4.57625945243649));
#129375=CARTESIAN_POINT('Ctrl Pts',(16.5372610234662,14.7320421497631,4.57108067199679));
#129376=CARTESIAN_POINT('Ctrl Pts',(16.5378663925751,14.7410153825975,4.56853904791834));
#129377=CARTESIAN_POINT('Ctrl Pts',(16.5394369651613,14.7645430871475,4.5622412329812));
#129378=CARTESIAN_POINT('Ctrl Pts',(16.5403955446741,14.7791511530601,4.55869383939881));
#129379=CARTESIAN_POINT('Ctrl Pts',(16.5459681657394,14.8653699496281,4.5398744242856));
#129380=CARTESIAN_POINT('Ctrl Pts',(16.5503267443039,14.938445219751,4.53243687462884));
#129381=CARTESIAN_POINT('Ctrl Pts',(16.5566491452149,15.0432028731231,4.53370092938054));
#129382=CARTESIAN_POINT('Ctrl Pts',(16.5585634799895,15.0747019441898,4.53562468080008));
#129383=CARTESIAN_POINT('Ctrl Pts',(16.5616784295267,15.1244061029229,4.54111012605176));
#129384=CARTESIAN_POINT('Ctrl Pts',(16.5628455441274,15.1427005859471,4.54366161135976));
#129385=CARTESIAN_POINT('Ctrl Pts',(16.5644868413208,15.1677674237073,4.54789284924952));
#129386=CARTESIAN_POINT('Ctrl Pts',(16.5649394006561,15.1746125074586,4.54912440328838));
#129387=CARTESIAN_POINT('Ctrl Pts',(16.5657190650942,15.1862783014608,4.55135349786119));
#129388=CARTESIAN_POINT('Ctrl Pts',(16.5660441801748,15.1911057060802,4.55231418727267));
#129389=CARTESIAN_POINT('Ctrl Pts',(16.5667487021835,15.2014830338668,4.55446186980962));
#129390=CARTESIAN_POINT('Ctrl Pts',(16.5671287004404,15.2070299042807,4.55566087479577));
#129391=CARTESIAN_POINT('Ctrl Pts',(16.568213684381,15.2227346182274,4.55920059952101));
#129392=CARTESIAN_POINT('Ctrl Pts',(16.5689244241698,15.2328652924451,4.56165680231362));
#129393=CARTESIAN_POINT('Ctrl Pts',(16.5732292155071,15.2934037810622,4.57737517335253));
#129394=CARTESIAN_POINT('Ctrl Pts',(16.5769711597976,15.3427078305578,4.59453169463096));
#129395=CARTESIAN_POINT('Ctrl Pts',(16.5838758107612,15.4309279975056,4.63347207096091));
#129396=CARTESIAN_POINT('Ctrl Pts',(16.5870341162533,15.4701960469196,4.65413600602973));
#129397=CARTESIAN_POINT('Ctrl Pts',(16.5920375085859,15.5313702352451,4.69190876932637));
#129398=CARTESIAN_POINT('Ctrl Pts',(16.5939263652396,15.5542014486246,4.70739242595949));
#129399=CARTESIAN_POINT('Ctrl Pts',(16.5965547092106,15.5855928009859,4.73070199922148));
#129400=CARTESIAN_POINT('Ctrl Pts',(16.597323051384,15.5947209651479,4.73773670201446));
#129401=CARTESIAN_POINT('Ctrl Pts',(16.5986595797358,15.610506368952,4.75035808568265));
#129402=CARTESIAN_POINT('Ctrl Pts',(16.5992304183465,15.6172179687675,4.75587432952845));
#129403=CARTESIAN_POINT('Ctrl Pts',(16.60041901472,15.6311230113808,4.76762042777011));
#129404=CARTESIAN_POINT('Ctrl Pts',(16.6010359956504,15.6383006916517,4.77386755285905));
#129405=CARTESIAN_POINT('Ctrl Pts',(16.6026774925372,15.6572764877867,4.7908820496721));
#129406=CARTESIAN_POINT('Ctrl Pts',(16.6036941867412,15.6689022290665,4.80183776799269));
#129407=CARTESIAN_POINT('Ctrl Pts',(16.6086619625971,15.7249339115653,4.85732528196518));
#129408=CARTESIAN_POINT('Ctrl Pts',(16.6124368613394,15.7651934791043,4.90582840789248));
#129409=CARTESIAN_POINT('Ctrl Pts',(16.6184807699982,15.8214823708443,4.98894437616548));
#129410=CARTESIAN_POINT('Ctrl Pts',(16.620740226256,15.8406803762178,5.02118134671776));
#129411=CARTESIAN_POINT('Ctrl Pts',(16.6243356693383,15.8673882376748,5.07261027315677));
#129412=CARTESIAN_POINT('Ctrl Pts',(16.6256243779527,15.8762398014624,5.09106477887754));
#129413=CARTESIAN_POINT('Ctrl Pts',(16.6274083620437,15.8874074814116,5.11637848808386));
#129414=CARTESIAN_POINT('Ctrl Pts',(16.6278767966389,15.8902425342599,5.12300434328766));
#129415=CARTESIAN_POINT('Ctrl Pts',(16.6286748033118,15.8949031256783,5.13424248769473));
#129416=CARTESIAN_POINT('Ctrl Pts',(16.6290021405767,15.8967677814178,5.13883839157188));
#129417=CARTESIAN_POINT('Ctrl Pts',(16.6297005939926,15.9006454065563,5.14861095413516));
#129418=CARTESIAN_POINT('Ctrl Pts',(16.6300721736769,15.9026492319637,5.15379085765597));
#129419=CARTESIAN_POINT('Ctrl Pts',(16.6311283539098,15.9081823120758,5.16846853409687));
#129420=CARTESIAN_POINT('Ctrl Pts',(16.6318184044622,15.9116069314338,5.1780046461681));
#129421=CARTESIAN_POINT('Ctrl Pts',(16.6373711950775,15.9377111408106,5.25445041226836));
#129422=CARTESIAN_POINT('Ctrl Pts',(16.6425040130643,15.9531427938087,5.32360587469783));
#129423=CARTESIAN_POINT('Ctrl Pts',(16.6498830525655,15.9645314738898,5.42667248032859));
#129424=CARTESIAN_POINT('Ctrl Pts',(16.6522104045477,15.9664746773638,5.45968972349377));
#129425=CARTESIAN_POINT('Ctrl Pts',(16.656081946325,15.9668953071581,5.51573187300437));
#129426=CARTESIAN_POINT('Ctrl Pts',(16.6576478452531,15.9662478696983,5.5387198678485));
#129427=CARTESIAN_POINT('Ctrl Pts',(16.6599144857269,15.9640912692188,5.57246123581872));
#129428=CARTESIAN_POINT('Ctrl Pts',(16.6606342214679,15.9632199882089,5.58324587890658));
#129429=CARTESIAN_POINT('Ctrl Pts',(16.6619168971444,15.9613303452022,5.60258505868069));
#129430=CARTESIAN_POINT('Ctrl Pts',(16.662481810538,15.9603783508253,5.61114476189332));
#129431=CARTESIAN_POINT('Ctrl Pts',(16.6636895443819,15.9580846168396,5.62952884858735));
#129432=CARTESIAN_POINT('Ctrl Pts',(16.6643311561,15.9567058547271,5.63934767635601));
#129433=CARTESIAN_POINT('Ctrl Pts',(16.6660922396773,15.952478037983,5.66642428671286));
#129434=CARTESIAN_POINT('Ctrl Pts',(16.6672018960184,15.9493112665748,5.68362906504903));
#129435=CARTESIAN_POINT('Ctrl Pts',(16.6737376463509,15.9276825066201,5.7855217632913));
#129436=CARTESIAN_POINT('Ctrl Pts',(16.6788044644982,15.8983684825073,5.86749295277333));
#129437=CARTESIAN_POINT('Ctrl Pts',(16.6859044763998,15.8450205182713,5.97054059516908));
#129438=CARTESIAN_POINT('Ctrl Pts',(16.6877291085472,15.8303377741881,5.99599090598995));
#129439=CARTESIAN_POINT('Ctrl Pts',(16.6901318688781,15.8101855391817,6.02751279173809));
#129440=CARTESIAN_POINT('Ctrl Pts',(16.6906533250202,15.8057655100517,6.03423991427185));
#129441=CARTESIAN_POINT('Ctrl Pts',(16.691514800342,15.7983995220895,6.04515130221034));
#129442=CARTESIAN_POINT('Ctrl Pts',(16.6918516960913,15.7955033100058,6.04936892968048));
#129443=CARTESIAN_POINT('Ctrl Pts',(16.6924971185142,15.7899287159527,6.05735045108545));
#129444=CARTESIAN_POINT('Ctrl Pts',(16.6928051985276,15.7872565774454,6.06111850861464));
#129445=CARTESIAN_POINT('Ctrl Pts',(16.6936577687543,15.7798283365891,6.07143577102364));
#129446=CARTESIAN_POINT('Ctrl Pts',(16.6942057304948,15.775016947922,6.07794445658906));
#129447=CARTESIAN_POINT('Ctrl Pts',(16.6966282195673,15.753561397556,6.10621906632008));
#129448=CARTESIAN_POINT('Ctrl Pts',(16.6985476910468,15.7360791119222,6.12733054324082));
#129449=CARTESIAN_POINT('Ctrl Pts',(16.70514896621,15.673694523376,6.1964630963521));
#129450=CARTESIAN_POINT('Ctrl Pts',(16.7099086123336,15.6247975800173,6.24064446529119));
#129451=CARTESIAN_POINT('Ctrl Pts',(16.7168700271584,15.5447763909791,6.29934166706548));
#129452=CARTESIAN_POINT('Ctrl Pts',(16.7191804824277,15.5167425028217,6.31774447987447));
#129453=CARTESIAN_POINT('Ctrl Pts',(16.7222662663603,15.4772128518769,6.34084720070379));
#129454=CARTESIAN_POINT('Ctrl Pts',(16.7230861742912,15.4665018983319,6.34683653855195));
#129455=CARTESIAN_POINT('Ctrl Pts',(16.7244818609436,15.4479181233561,6.35676855704967));
#129456=CARTESIAN_POINT('Ctrl Pts',(16.7250610327956,15.4401003698626,6.36081047772485));
#129457=CARTESIAN_POINT('Ctrl Pts',(16.7262404048705,15.4239687150931,6.3688736131134));
#129458=CARTESIAN_POINT('Ctrl Pts',(16.7268401737788,15.4156501884027,6.37288358755015));
#129459=CARTESIAN_POINT('Ctrl Pts',(16.7283763261889,15.3940588710247,6.38291309378859));
#129460=CARTESIAN_POINT('Ctrl Pts',(16.7293066400723,15.3807048661396,6.38875292684243));
#129461=CARTESIAN_POINT('Ctrl Pts',(16.735064754792,15.2964549908939,6.42334859678867));
#129462=CARTESIAN_POINT('Ctrl Pts',(16.7396073113771,15.2224884595989,6.44390575556967));
#129463=CARTESIAN_POINT('Ctrl Pts',(16.7460384618295,15.117273962186,6.46007752162148));
#129464=CARTESIAN_POINT('Ctrl Pts',(16.747859590196,15.0874868486499,6.46324859714241));
#129465=CARTESIAN_POINT('Ctrl Pts',(16.7508420704627,15.0397522827032,6.46609786774926));
#129466=CARTESIAN_POINT('Ctrl Pts',(16.7519732958886,15.0218770042431,6.46666780273942));
#129467=CARTESIAN_POINT('Ctrl Pts',(16.7535722616981,14.9971220061422,6.46677016558036));
#129468=CARTESIAN_POINT('Ctrl Pts',(16.7540198116915,14.9902466301316,6.46672524592449));
#129469=CARTESIAN_POINT('Ctrl Pts',(16.7547937816012,14.978461471832,6.46652251925225));
#129470=CARTESIAN_POINT('Ctrl Pts',(16.755118292027,14.9735514166529,6.46640062070721));
#129471=CARTESIAN_POINT('Ctrl Pts',(16.7558251568151,14.9629271825906,6.46605582950888));
#129472=CARTESIAN_POINT('Ctrl Pts',(16.7562081510912,14.9572139922257,6.46581965865952));
#129473=CARTESIAN_POINT('Ctrl Pts',(16.7573101208438,14.94088906367,6.46499969341926));
#129474=CARTESIAN_POINT('Ctrl Pts',(16.7580351190431,14.9302847408845,6.46429159052797));
#129475=CARTESIAN_POINT('Ctrl Pts',(16.7619433771386,14.8737309851228,6.45957753629581));
#129476=CARTESIAN_POINT('Ctrl Pts',(16.7652411643744,14.8281040344634,6.45246206643116));
#129477=CARTESIAN_POINT('Ctrl Pts',(16.7719939355626,14.7362112822387,6.43131216820889));
#129478=CARTESIAN_POINT('Ctrl Pts',(16.775439147838,14.6901288540215,6.41701005926373));
#129479=CARTESIAN_POINT('Ctrl Pts',(16.7808134647503,14.618425303569,6.38873001568306));
#129480=CARTESIAN_POINT('Ctrl Pts',(16.7827957364795,14.5920351733759,6.37692945754169));
#129481=CARTESIAN_POINT('Ctrl Pts',(16.7855268129005,14.5557508971591,6.35871141400187));
#129482=CARTESIAN_POINT('Ctrl Pts',(16.7863076776659,14.545386713048,6.35326979170319));
#129483=CARTESIAN_POINT('Ctrl Pts',(16.7876584290128,14.5274848150553,6.34345175481248));
#129484=CARTESIAN_POINT('Ctrl Pts',(16.7882311453952,14.5199028969711,6.33915924747966));
#129485=CARTESIAN_POINT('Ctrl Pts',(16.789416683242,14.5042321558482,6.33000532742448));
#129486=CARTESIAN_POINT('Ctrl Pts',(16.7900288199479,14.4961543773629,6.32512677667975));
#129487=CARTESIAN_POINT('Ctrl Pts',(16.7916407548668,14.4749327864901,6.31188219004696));
#129488=CARTESIAN_POINT('Ctrl Pts',(16.792633239925,14.4619172714429,6.30331518643864));
#129489=CARTESIAN_POINT('Ctrl Pts',(16.7979392777867,14.3927704155012,6.25536671072528));
#129490=CARTESIAN_POINT('Ctrl Pts',(16.8020357742926,14.3407424019931,6.21041331131239));
#129491=CARTESIAN_POINT('Ctrl Pts',(16.8082183176407,14.2706765056683,6.1354913980108));
#129492=CARTESIAN_POINT('Ctrl Pts',(16.8102760115387,14.2487761335198,6.10944605594021));
#129493=CARTESIAN_POINT('Ctrl Pts',(16.813592405134,14.2166513186919,6.06687219596239));
#129494=CARTESIAN_POINT('Ctrl Pts',(16.8148121208184,14.2054740671771,6.05109679229484));
#129495=CARTESIAN_POINT('Ctrl Pts',(16.8165152777005,14.1908670148169,6.02911182208111));
#129496=CARTESIAN_POINT('Ctrl Pts',(16.8169749074968,14.1870208319777,6.02318292522592));
#129497=CARTESIAN_POINT('Ctrl Pts',(16.817762690725,14.1805981417413,6.01304048949698));
#129498=CARTESIAN_POINT('Ctrl Pts',(16.8180887402015,14.1779883166802,6.00884844567653));
#129499=CARTESIAN_POINT('Ctrl Pts',(16.8187903230788,14.1724778450051,5.99984418787184));
#129500=CARTESIAN_POINT('Ctrl Pts',(16.8191663831388,14.1695869901407,5.99502662392762));
#129501=CARTESIAN_POINT('Ctrl Pts',(16.8202292218785,14.1615874275188,5.98142821056715));
#129502=CARTESIAN_POINT('Ctrl Pts',(16.8209214125889,14.1565750524341,5.97259189779269));
#129503=CARTESIAN_POINT('Ctrl Pts',(16.825476207258,14.1248085285235,5.91447526346422));
#129504=CARTESIAN_POINT('Ctrl Pts',(16.8295118649565,14.1022478816308,5.86302902330676));
#129505=CARTESIAN_POINT('Ctrl Pts',(16.8380189995739,14.0641375266948,5.75042456357647));
#129506=CARTESIAN_POINT('Ctrl Pts',(16.8424598712464,14.0498443458301,5.68909703755364));
#129507=CARTESIAN_POINT('Ctrl Pts',(16.8476617311138,14.0397718628649,5.6129703879532));
#129508=CARTESIAN_POINT('Ctrl Pts',(16.8485982476018,14.0382408361698,5.59909454462267));
#129509=CARTESIAN_POINT('Ctrl Pts',(16.8501309220511,14.036207816555,5.57611319701687));
#129510=CARTESIAN_POINT('Ctrl Pts',(16.8507322783809,14.0355332103842,5.56702546427246));
#129511=CARTESIAN_POINT('Ctrl Pts',(16.8519049668469,14.034461402571,5.54917079393646));
#129512=CARTESIAN_POINT('Ctrl Pts',(16.8524765293193,14.0340548834672,5.54040532443724));
#129513=CARTESIAN_POINT('Ctrl Pts',(16.8537324010243,14.0334200021052,5.5210142334101));
#129514=CARTESIAN_POINT('Ctrl Pts',(16.8544149537548,14.0332473959202,5.51038783667619));
#129515=CARTESIAN_POINT('Ctrl Pts',(16.8550925403141,14.0332500296882,5.49976041276753));
#129516=CARTESIAN_POINT('Origin',(16.125,15.,5.5));
#129517=CARTESIAN_POINT('',(17.3122359168897,14.0332501543841,5.49945364696662));
#129518=CARTESIAN_POINT('',(17.2535750170786,14.0332500522588,5.49945804013099));
#129519=CARTESIAN_POINT('',(16.125,14.03325,5.5));
#129520=CARTESIAN_POINT('Ctrl Pts',(17.3128750435716,14.0332501300013,5.49949864428434));
#129521=CARTESIAN_POINT('Ctrl Pts',(17.3076106834502,14.0332113526949,5.57427181392873));
#129522=CARTESIAN_POINT('Ctrl Pts',(17.3021747516393,14.0418471203054,5.64880226167124));
#129523=CARTESIAN_POINT('Ctrl Pts',(17.2947357824472,14.0662164561492,5.752284734281));
#129524=CARTESIAN_POINT('Ctrl Pts',(17.292566487215,14.0749393927244,5.78259958989893));
#129525=CARTESIAN_POINT('Ctrl Pts',(17.2896163549051,14.0890942041165,5.82404740441688));
#129526=CARTESIAN_POINT('Ctrl Pts',(17.2887969957306,14.0932801184978,5.83558183642833));
#129527=CARTESIAN_POINT('Ctrl Pts',(17.2873870493272,14.1009255159992,5.85546046865153));
#129528=CARTESIAN_POINT('Ctrl Pts',(17.2867932766066,14.1042843680011,5.86384143294114));
#129529=CARTESIAN_POINT('Ctrl Pts',(17.2855696212882,14.1114939264757,5.88112541471665));
#129530=CARTESIAN_POINT('Ctrl Pts',(17.2849403999434,14.1153622147692,5.89002003078127));
#129531=CARTESIAN_POINT('Ctrl Pts',(17.2832930384043,14.1259106864368,5.91331010174951));
#129532=CARTESIAN_POINT('Ctrl Pts',(17.2822823863766,14.1328127302932,5.92760221236292));
#129533=CARTESIAN_POINT('Ctrl Pts',(17.2770426837281,14.1707931681929,6.00154239473592));
#129534=CARTESIAN_POINT('Ctrl Pts',(17.2730195250341,14.2076813252928,6.05799718054965));
#129535=CARTESIAN_POINT('Ctrl Pts',(17.2668946188679,14.271808630087,6.13680625079424));
#129536=CARTESIAN_POINT('Ctrl Pts',(17.264817290618,14.2948858242393,6.16226776039735));
#129537=CARTESIAN_POINT('Ctrl Pts',(17.2614681373421,14.3331437458408,6.2002072822624));
#129538=CARTESIAN_POINT('Ctrl Pts',(17.2602355043746,14.3474336337868,6.21354364003395));
#129539=CARTESIAN_POINT('Ctrl Pts',(17.2585086883526,14.3675485593439,6.23120653248025));
#129540=CARTESIAN_POINT('Ctrl Pts',(17.2580386158929,14.3730335603861,6.23591500458463));
#129541=CARTESIAN_POINT('Ctrl Pts',(17.2572301017247,14.3824714092226,6.24383461351135));
#129542=CARTESIAN_POINT('Ctrl Pts',(17.256893818727,14.3863977191633,6.2470767915406));
#129543=CARTESIAN_POINT('Ctrl Pts',(17.2561645479275,14.3949106209618,6.25399399429277));
#129544=CARTESIAN_POINT('Ctrl Pts',(17.2557709260442,14.3995051728477,6.25765827276294));
#129545=CARTESIAN_POINT('Ctrl Pts',(17.2546424361792,14.412684643902,6.26797407318739));
#129546=CARTESIAN_POINT('Ctrl Pts',(17.2539013435198,14.4213483563214,6.27452292179586));
#129547=CARTESIAN_POINT('Ctrl Pts',(17.2501645016946,14.4651609191952,6.30649516958091));
#129548=CARTESIAN_POINT('Ctrl Pts',(17.2470692405103,14.5018802939441,6.32967670803815));
#129549=CARTESIAN_POINT('Ctrl Pts',(17.2411030261171,14.5751993051432,6.36933819492763));
#129550=CARTESIAN_POINT('Ctrl Pts',(17.238238922729,14.6115185882246,6.38616422425089));
#129551=CARTESIAN_POINT('Ctrl Pts',(17.2328290006973,14.6831020515089,6.41407801536702));
#129552=CARTESIAN_POINT('Ctrl Pts',(17.2302799768547,14.7181672845786,6.42549111755068));
#129553=CARTESIAN_POINT('Ctrl Pts',(17.2269254773766,14.7662332839478,6.43814920446232));
#129554=CARTESIAN_POINT('Ctrl Pts',(17.2260656255764,14.7787287429741,6.44117472596737));
#129555=CARTESIAN_POINT('Ctrl Pts',(17.2246089260312,14.8001885322323,6.44591974111596));
#129556=CARTESIAN_POINT('Ctrl Pts',(17.2240082858064,14.8091233887306,6.44776310755111));
#129557=CARTESIAN_POINT('Ctrl Pts',(17.2227898466543,14.8274182022474,6.45126832472021));
#129558=CARTESIAN_POINT('Ctrl Pts',(17.2221724508821,14.8367792711836,6.45291915010783));
#129559=CARTESIAN_POINT('Ctrl Pts',(17.2205982784343,14.860867425825,6.45680171060259));
#129560=CARTESIAN_POINT('Ctrl Pts',(17.2196477654434,14.8756247882248,6.45883170082973));
#129561=CARTESIAN_POINT('Ctrl Pts',(17.2134058935599,14.9737615870231,6.47002715409928));
#129562=CARTESIAN_POINT('Ctrl Pts',(17.2084648675997,15.0579785886101,6.46864859581226));
#129563=CARTESIAN_POINT('Ctrl Pts',(17.2011657626691,15.1768430759656,6.4511295454358));
#129564=CARTESIAN_POINT('Ctrl Pts',(17.1989333516914,15.2123931904438,6.44382702920944));
#129565=CARTESIAN_POINT('Ctrl Pts',(17.1960568648701,15.2557806244191,6.43233909494369));
#129566=CARTESIAN_POINT('Ctrl Pts',(17.1954991694994,15.2640859761082,6.43002069908999));
#129567=CARTESIAN_POINT('Ctrl Pts',(17.1945860234339,15.2774889558539,6.42608532474093));
#129568=CARTESIAN_POINT('Ctrl Pts',(17.1942342422719,15.2826063337724,6.42453653602264));
#129569=CARTESIAN_POINT('Ctrl Pts',(17.1935224857099,15.2928613489043,6.4213397324722));
#129570=CARTESIAN_POINT('Ctrl Pts',(17.1931624852142,15.2979985474341,6.41969099952346));
#129571=CARTESIAN_POINT('Ctrl Pts',(17.1922057324492,15.3115280410132,6.41522358844941));
#129572=CARTESIAN_POINT('Ctrl Pts',(17.1916051700539,15.3198956787063,6.41233254820179));
#129573=CARTESIAN_POINT('Ctrl Pts',(17.1882035275343,15.3666586414219,6.39545343426489));
#129574=CARTESIAN_POINT('Ctrl Pts',(17.1853033238585,15.4041733134573,6.37915794720899));
#129575=CARTESIAN_POINT('Ctrl Pts',(17.1785224898527,15.4886232866842,6.33592505357763));
#129576=CARTESIAN_POINT('Ctrl Pts',(17.1746423695747,15.5345623865423,6.30732108265115));
#129577=CARTESIAN_POINT('Ctrl Pts',(17.1687135845517,15.6025548972457,6.25662474166392));
#129578=CARTESIAN_POINT('Ctrl Pts',(17.1665966495201,15.6263451525073,6.23705189223996));
#129579=CARTESIAN_POINT('Ctrl Pts',(17.1637032393467,15.658186280762,6.20819818247666));
#129580=CARTESIAN_POINT('Ctrl Pts',(17.1628902218705,15.6670547550369,6.19985128583535));
#129581=CARTESIAN_POINT('Ctrl Pts',(17.1614875324569,15.6822100559904,6.18503741976923));
#129582=CARTESIAN_POINT('Ctrl Pts',(17.1608947683197,15.6885683233384,6.17864607875259));
#129583=CARTESIAN_POINT('Ctrl Pts',(17.1596698938386,15.7016045052249,6.16517023077048));
#129584=CARTESIAN_POINT('Ctrl Pts',(17.1590384893874,15.7082666993586,6.15807188922337));
#129585=CARTESIAN_POINT('Ctrl Pts',(17.1573776708703,15.7256248830882,6.13900830488633));
#129586=CARTESIAN_POINT('Ctrl Pts',(17.1563559789697,15.7361323448849,6.12687502850902));
#129587=CARTESIAN_POINT('Ctrl Pts',(17.1512494606944,15.7876478712169,6.06430597951119));
#129588=CARTESIAN_POINT('Ctrl Pts',(17.1473541269949,15.8237974445655,6.01008739774125));
#129589=CARTESIAN_POINT('Ctrl Pts',(17.1412872704953,15.8709397613192,5.92112050145835));
#129590=CARTESIAN_POINT('Ctrl Pts',(17.1391323573883,15.8858860921251,5.88869534450003));
#129591=CARTESIAN_POINT('Ctrl Pts',(17.1356754834809,15.9063556902626,5.83693385263708));
#129592=CARTESIAN_POINT('Ctrl Pts',(17.1344158063256,15.9131272896578,5.81812496121841));
#129593=CARTESIAN_POINT('Ctrl Pts',(17.132657236626,15.9215646913578,5.7921936920799));
#129594=CARTESIAN_POINT('Ctrl Pts',(17.1321836248819,15.9237402850596,5.78524114725821));
#129595=CARTESIAN_POINT('Ctrl Pts',(17.1313710570111,15.9273049834889,5.77338076043736));
#129596=CARTESIAN_POINT('Ctrl Pts',(17.1310343185989,15.9287341835196,5.76848535864741));
#129597=CARTESIAN_POINT('Ctrl Pts',(17.1303065686542,15.9317190609568,5.75795223002339));
#129598=CARTESIAN_POINT('Ctrl Pts',(17.1299149568862,15.9332623469274,5.7523116110255));
#129599=CARTESIAN_POINT('Ctrl Pts',(17.1287978733808,15.9374902848146,5.73628905782922));
#129600=CARTESIAN_POINT('Ctrl Pts',(17.1280663602916,15.9400534183356,5.72587629572563));
#129601=CARTESIAN_POINT('Ctrl Pts',(17.1244682549607,15.9516954195802,5.67494445831862));
#129602=CARTESIAN_POINT('Ctrl Pts',(17.1215100353092,15.9583298238891,5.63391454531794));
#129603=CARTESIAN_POINT('Ctrl Pts',(17.115635500724,15.9661932762804,5.55218743701533));
#129604=CARTESIAN_POINT('Ctrl Pts',(17.1127255665204,15.9675325326763,5.51157898045148));
#129605=CARTESIAN_POINT('Ctrl Pts',(17.1071807503692,15.9651736725518,5.43296475202831));
#129606=CARTESIAN_POINT('Ctrl Pts',(17.1045445952136,15.9617868950551,5.39502131441314));
#129607=CARTESIAN_POINT('Ctrl Pts',(17.1010989475308,15.9542573127376,5.34454329609833));
#129608=CARTESIAN_POINT('Ctrl Pts',(17.1002310685472,15.9520856128918,5.33175369613272));
#129609=CARTESIAN_POINT('Ctrl Pts',(17.0987650248699,15.9479455349259,5.31003051203689));
#129610=CARTESIAN_POINT('Ctrl Pts',(17.0981629449963,15.9461066260117,5.30107437242908));
#129611=CARTESIAN_POINT('Ctrl Pts',(17.0970185088022,15.9423456152242,5.28399067956057));
#129612=CARTESIAN_POINT('Ctrl Pts',(17.0964755492781,15.9404447164484,5.27585935788927));
#129613=CARTESIAN_POINT('Ctrl Pts',(17.0950495759109,15.935144879374,5.25444430357452));
#129614=CARTESIAN_POINT('Ctrl Pts',(17.0941721933513,15.9315682237453,5.2412062221827));
#129615=CARTESIAN_POINT('Ctrl Pts',(17.0905003492009,15.91527749382,5.18563355136984));
#129616=CARTESIAN_POINT('Ctrl Pts',(17.0877885121062,15.8999491875991,5.14411906482836));
#129617=CARTESIAN_POINT('Ctrl Pts',(17.0821444258943,15.861761526449,5.05912480948116));
#129618=CARTESIAN_POINT('Ctrl Pts',(17.0792283585936,15.8383265517629,5.01604527397734));
#129619=CARTESIAN_POINT('Ctrl Pts',(17.0743944948884,15.7953849086198,4.9496600774261));
#129620=CARTESIAN_POINT('Ctrl Pts',(17.0725268748431,15.7778707715684,4.92517141896538));
#129621=CARTESIAN_POINT('Ctrl Pts',(17.0700655254145,15.7541339990509,4.89505731972667));
#129622=CARTESIAN_POINT('Ctrl Pts',(17.0695308173356,15.7489401261655,4.88863888619985));
#129623=CARTESIAN_POINT('Ctrl Pts',(17.0686457272327,15.7402966441488,4.87823297799517));
#129624=CARTESIAN_POINT('Ctrl Pts',(17.0682985983077,15.7368953493077,4.87420563027202));
#129625=CARTESIAN_POINT('Ctrl Pts',(17.0676305838473,15.7303326208582,4.86656263840618));
#129626=CARTESIAN_POINT('Ctrl Pts',(17.0673101426296,15.7271768718056,4.86294237086507));
#129627=CARTESIAN_POINT('Ctrl Pts',(17.0664151386439,15.7183380351217,4.85295372399721));
#129628=CARTESIAN_POINT('Ctrl Pts',(17.0658366980359,15.7125975323553,4.84663703752501));
#129629=CARTESIAN_POINT('Ctrl Pts',(17.0631093057454,15.68536797257,4.81746014045381));
#129630=CARTESIAN_POINT('Ctrl Pts',(17.0609020262016,15.662859529037,4.79558052407562));
#129631=CARTESIAN_POINT('Ctrl Pts',(17.0542895561488,15.5931180161702,4.73409399612881));
#129632=CARTESIAN_POINT('Ctrl Pts',(17.0498407625908,15.5431131286031,4.69785903847948));
#129633=CARTESIAN_POINT('Ctrl Pts',(17.0432294507842,15.4617877911234,4.65004200277396));
#129634=CARTESIAN_POINT('Ctrl Pts',(17.0409745388417,15.4327503914839,4.63489650243903));
#129635=CARTESIAN_POINT('Ctrl Pts',(17.0379321855195,15.3917147310829,4.61607737208906));
#129636=CARTESIAN_POINT('Ctrl Pts',(17.0371028766634,15.380332729201,4.61112054711191));
#129637=CARTESIAN_POINT('Ctrl Pts',(17.0356815125061,15.3604923986584,4.60293105101111));
#129638=CARTESIAN_POINT('Ctrl Pts',(17.0350861242755,15.3520785333719,4.59959554403789));
#129639=CARTESIAN_POINT('Ctrl Pts',(17.0338641645262,15.3346031637319,4.59295021016647));
#129640=CARTESIAN_POINT('Ctrl Pts',(17.0332381866449,15.3255364459781,4.58965686050631));
#129641=CARTESIAN_POINT('Ctrl Pts',(17.0316107951971,15.301678406688,4.58139282308706));
#129642=CARTESIAN_POINT('Ctrl Pts',(17.0306165280843,15.2868130629751,4.57664345139428));
#129643=CARTESIAN_POINT('Ctrl Pts',(17.0252282402437,15.2048354727992,4.55262317490542));
#129644=CARTESIAN_POINT('Ctrl Pts',(17.0210600363142,15.1359024171776,4.54030632174868));
#129645=CARTESIAN_POINT('Ctrl Pts',(17.0148619787201,15.0333907916218,4.53326595077989));
#129646=CARTESIAN_POINT('Ctrl Pts',(17.0128668623069,15.0004505509173,4.53268970821658));
#129647=CARTESIAN_POINT('Ctrl Pts',(17.0100005204936,14.9544088050621,4.53423614589188));
#129648=CARTESIAN_POINT('Ctrl Pts',(17.0091743169722,14.9412812215649,4.5349453634108));
#129649=CARTESIAN_POINT('Ctrl Pts',(17.0076907795106,14.9180612685299,4.53667533108472));
#129650=CARTESIAN_POINT('Ctrl Pts',(17.0070381170956,14.9079626660079,4.53758767493448));
#129651=CARTESIAN_POINT('Ctrl Pts',(17.0060081867569,14.8922467127321,4.5392571143912));
#129652=CARTESIAN_POINT('Ctrl Pts',(17.0056364732037,14.8866182064168,4.53990509419112));
#129653=CARTESIAN_POINT('Ctrl Pts',(17.0049244580443,14.87592746963,4.54123117809075));
#129654=CARTESIAN_POINT('Ctrl Pts',(17.0045846462763,14.8708643861681,4.54189998691578));
#129655=CARTESIAN_POINT('Ctrl Pts',(17.0037304878003,14.8582299611661,4.54367089424771));
#129656=CARTESIAN_POINT('Ctrl Pts',(17.0032135765452,14.8506660527944,4.54482280928426));
#129657=CARTESIAN_POINT('Ctrl Pts',(17.0012376811162,14.8220326331237,4.54953182639755));
#129658=CARTESIAN_POINT('Ctrl Pts',(16.9997518880061,14.8010706912037,4.55369713058502));
#129659=CARTESIAN_POINT('Ctrl Pts',(16.99324707997,14.7110706753485,4.57470319094223));
#129660=CARTESIAN_POINT('Ctrl Pts',(16.9880862093617,14.6438658312652,4.5984325584684));
#129661=CARTESIAN_POINT('Ctrl Pts',(16.9806629179709,14.5486802568075,4.64436282493202));
#129662=CARTESIAN_POINT('Ctrl Pts',(16.9782724990335,14.5183237146337,4.66107633665176));
#129663=CARTESIAN_POINT('Ctrl Pts',(16.9750854505441,14.478208719315,4.68605967825578));
#129664=CARTESIAN_POINT('Ctrl Pts',(16.9742413867559,14.4676223504203,4.69294420798522));
#129665=CARTESIAN_POINT('Ctrl Pts',(16.9728029987107,14.4496564267965,4.70513520800126));
#129666=CARTESIAN_POINT('Ctrl Pts',(16.9722051209408,14.4422114618579,4.71034181939273));
#129667=CARTESIAN_POINT('Ctrl Pts',(16.9709851476126,14.4270733780262,4.72124952347356));
#129668=CARTESIAN_POINT('Ctrl Pts',(16.9703635507454,14.4193893316038,4.72696152667446));
#129669=CARTESIAN_POINT('Ctrl Pts',(16.9687632474545,14.3996950927668,4.74206075417177));
#129670=CARTESIAN_POINT('Ctrl Pts',(16.9677912330976,14.3878195447154,4.7516197411115));
#129671=CARTESIAN_POINT('Ctrl Pts',(16.9616381637684,14.3133669924242,4.81450753277526));
#129672=CARTESIAN_POINT('Ctrl Pts',(16.9567892777506,14.2575852392825,4.87535155868957));
#129673=CARTESIAN_POINT('Ctrl Pts',(16.9495429910546,14.1887513448055,4.97287445489697));
#129674=CARTESIAN_POINT('Ctrl Pts',(16.94725878971,14.1690980507912,5.00443256765029));
#129675=CARTESIAN_POINT('Ctrl Pts',(16.9443235885123,14.1471620137522,5.04464519534949));
#129676=CARTESIAN_POINT('Ctrl Pts',(16.9437633048511,14.1431155309344,5.05230632890165));
#129677=CARTESIAN_POINT('Ctrl Pts',(16.9428469831884,14.136735442915,5.06478907783135));
#129678=CARTESIAN_POINT('Ctrl Pts',(16.9424946624713,14.1343378904047,5.06957770599404));
#129679=CARTESIAN_POINT('Ctrl Pts',(16.9417829951092,14.1296090252159,5.07922200078097));
#129680=CARTESIAN_POINT('Ctrl Pts',(16.9414236371304,14.1272782657519,5.08407771788205));
#129681=CARTESIAN_POINT('Ctrl Pts',(16.9404704892153,14.1212425002425,5.09692627131019));
#129682=CARTESIAN_POINT('Ctrl Pts',(16.9398729376423,14.1176060557816,5.10495052449272));
#129683=CARTESIAN_POINT('Ctrl Pts',(16.9366430152249,14.098707023119,5.14821674510514));
#129684=CARTESIAN_POINT('Ctrl Pts',(16.9339231324468,14.0854463455459,5.18429201661173));
#129685=CARTESIAN_POINT('Ctrl Pts',(16.9271907373145,14.0582424424118,5.27456406461322));
#129686=CARTESIAN_POINT('Ctrl Pts',(16.9231709938523,14.046786314049,5.32937400048957));
#129687=CARTESIAN_POINT('Ctrl Pts',(16.9177667114474,14.0375857271319,5.40608111272542));
#129688=CARTESIAN_POINT('Ctrl Pts',(16.9162886353816,14.0357451571529,5.42737289805189));
#129689=CARTESIAN_POINT('Ctrl Pts',(16.9136686245222,14.0337084919509,5.46570695274326));
#129690=CARTESIAN_POINT('Ctrl Pts',(16.9125198714081,14.0332544456984,5.48272613773083));
#129691=CARTESIAN_POINT('Ctrl Pts',(16.9113846553004,14.033250032487,5.49974937361882));
#129692=CARTESIAN_POINT('Ctrl Pts',(16.8550925403141,14.0332500296882,5.49976041276753));
#129693=CARTESIAN_POINT('Ctrl Pts',(16.8569805886081,14.0332573685012,5.47014782776616));
#129694=CARTESIAN_POINT('Ctrl Pts',(16.8588280516786,14.0346252816896,5.44054947718285));
#129695=CARTESIAN_POINT('Ctrl Pts',(16.8637501480891,14.0419916165554,5.36082074904889));
#129696=CARTESIAN_POINT('Ctrl Pts',(16.8667628118452,14.0505586046603,5.3110233457765));
#129697=CARTESIAN_POINT('Ctrl Pts',(16.8723921692601,14.0735129401352,5.22060420950517));
#129698=CARTESIAN_POINT('Ctrl Pts',(16.8749953183793,14.0867991173928,5.17983806412932));
#129699=CARTESIAN_POINT('Ctrl Pts',(16.8783947714423,14.1067118030943,5.13019538297171));
#129700=CARTESIAN_POINT('Ctrl Pts',(16.8790796408903,14.1108446832636,5.1203658889598));
#129701=CARTESIAN_POINT('Ctrl Pts',(16.8801458722479,14.11744523418,5.10536671543337));
#129702=CARTESIAN_POINT('Ctrl Pts',(16.8805209256628,14.1197978251529,5.10014693777188));
#129703=CARTESIAN_POINT('Ctrl Pts',(16.8812228141034,14.1242538791875,5.09049004290508));
#129704=CARTESIAN_POINT('Ctrl Pts',(16.8815489394985,14.1263449934759,5.08604758909313));
#129705=CARTESIAN_POINT('Ctrl Pts',(16.8823356528223,14.1314396533196,5.07543483463591));
#129706=CARTESIAN_POINT('Ctrl Pts',(16.8827980701513,14.1344751799524,5.06928032931161));
#129707=CARTESIAN_POINT('Ctrl Pts',(16.8844711952187,14.1456131576357,5.04729141749724));
#129708=CARTESIAN_POINT('Ctrl Pts',(16.8857007876877,14.1540862865985,5.03164987789483));
#129709=CARTESIAN_POINT('Ctrl Pts',(16.889022006378,14.1778402634125,4.99054907604134));
#129710=CARTESIAN_POINT('Ctrl Pts',(16.8911377941257,14.1938704809174,4.96554523949328));
#129711=CARTESIAN_POINT('Ctrl Pts',(16.8987730088496,14.2555397068338,4.87845514331493));
#129712=CARTESIAN_POINT('Ctrl Pts',(16.9042842671423,14.3074177316254,4.82112367767922));
#129713=CARTESIAN_POINT('Ctrl Pts',(16.9104951272084,14.3764956421193,4.76104265722603));
#129714=CARTESIAN_POINT('Ctrl Pts',(16.9114687486816,14.3876448496,4.75177754202202));
#129715=CARTESIAN_POINT('Ctrl Pts',(16.9130453599745,14.4062191116181,4.73703552244383));
#129716=CARTESIAN_POINT('Ctrl Pts',(16.9136541672156,14.4135213064361,4.73140824278354));
#129717=CARTESIAN_POINT('Ctrl Pts',(16.9148368582036,14.4279566474442,4.72060949418074));
#129718=CARTESIAN_POINT('Ctrl Pts',(16.9154110348513,14.435082178889,4.7154294030732));
#129719=CARTESIAN_POINT('Ctrl Pts',(16.9167796953597,14.4523423689923,4.7032387368818));
#129720=CARTESIAN_POINT('Ctrl Pts',(16.9175705947952,14.462542348759,4.69632302128274));
#129721=CARTESIAN_POINT('Ctrl Pts',(16.9205173765212,14.5013543797885,4.6710774603318));
#129722=CARTESIAN_POINT('Ctrl Pts',(16.92262638522,14.5307952347298,4.65406426684295));
#129723=CARTESIAN_POINT('Ctrl Pts',(16.9288675434884,14.6217415775555,4.60772062321625));
#129724=CARTESIAN_POINT('Ctrl Pts',(16.9328769183196,14.6855020724685,4.58330366859324));
#129725=CARTESIAN_POINT('Ctrl Pts',(16.938600237111,14.775375818592,4.55937759750302));
#129726=CARTESIAN_POINT('Ctrl Pts',(16.940157356991,14.7996931065315,4.55390092408));
#129727=CARTESIAN_POINT('Ctrl Pts',(16.9422644203817,14.8319285034046,4.5479393786893));
#129728=CARTESIAN_POINT('Ctrl Pts',(16.9427744219838,14.8396813554126,4.5466032424631));
#129729=CARTESIAN_POINT('Ctrl Pts',(16.9435891334133,14.851969906475,4.54463953860423));
#129730=CARTESIAN_POINT('Ctrl Pts',(16.9438905229242,14.8564954254587,4.54394929278589));
#129731=CARTESIAN_POINT('Ctrl Pts',(16.9445359851929,14.8661392116224,4.54254840694741));
#129732=CARTESIAN_POINT('Ctrl Pts',(16.9448805494108,14.8712585760792,4.5418466165919));
#129733=CARTESIAN_POINT('Ctrl Pts',(16.9457837526175,14.8846098799488,4.54012527556997));
#129734=CARTESIAN_POINT('Ctrl Pts',(16.9463456845636,14.8928495801515,4.53917059645901));
#129735=CARTESIAN_POINT('Ctrl Pts',(16.9491748155504,14.9340511344386,4.53493339244573));
#129736=CARTESIAN_POINT('Ctrl Pts',(16.9515084332927,14.9671514448371,4.53324079484158));
#129737=CARTESIAN_POINT('Ctrl Pts',(16.9577024681769,15.054138598902,4.53326507157288));
#129738=CARTESIAN_POINT('Ctrl Pts',(16.9615882129949,15.1079153544375,4.53778266070494));
#129739=CARTESIAN_POINT('Ctrl Pts',(16.9680464825794,15.1982324962835,4.55304040153624));
#129740=CARTESIAN_POINT('Ctrl Pts',(16.9706598635109,15.2350324653195,4.56149643402058));
#129741=CARTESIAN_POINT('Ctrl Pts',(16.9740803609126,15.2836457980712,4.57570704711354));
#129742=CARTESIAN_POINT('Ctrl Pts',(16.9749449031465,15.2959701717125,4.5795793972008));
#129743=CARTESIAN_POINT('Ctrl Pts',(16.9763336690487,15.3158185339383,4.58625572938594));
#129744=CARTESIAN_POINT('Ctrl Pts',(16.9768626799689,15.3233913550519,4.58890836003187));
#129745=CARTESIAN_POINT('Ctrl Pts',(16.9779717440913,15.3392884347996,4.59470002315309));
#129746=CARTESIAN_POINT('Ctrl Pts',(16.9785510449438,15.3476041934152,4.59786030825321));
#129747=CARTESIAN_POINT('Ctrl Pts',(16.9799560227229,15.3677919797368,4.60585298370008));
#129748=CARTESIAN_POINT('Ctrl Pts',(16.9807776011295,15.3796139929807,4.61080763171321));
#129749=CARTESIAN_POINT('Ctrl Pts',(16.9840709228368,15.4270052987942,4.63178700740235));
#129750=CARTESIAN_POINT('Ctrl Pts',(16.9864789946547,15.461689886295,4.64972342345273));
#129751=CARTESIAN_POINT('Ctrl Pts',(16.9911994745563,15.5283350591226,4.68947163753116));
#129752=CARTESIAN_POINT('Ctrl Pts',(16.9935085441428,15.56025869538,4.71120065477955));
#129753=CARTESIAN_POINT('Ctrl Pts',(16.9984234901247,15.6247292664395,4.76097601471548));
#129754=CARTESIAN_POINT('Ctrl Pts',(17.0010285414683,15.6568765219826,4.78939773572276));
#129755=CARTESIAN_POINT('Ctrl Pts',(17.0044302026669,15.6945317017549,4.82743400426612));
#129756=CARTESIAN_POINT('Ctrl Pts',(17.0051152062007,15.7019085964831,4.83513640228213));
#129757=CARTESIAN_POINT('Ctrl Pts',(17.0061816031185,15.713047791645,4.84715913427062));
#129758=CARTESIAN_POINT('Ctrl Pts',(17.0065566849855,15.7169018677013,4.85139375793849));
#129759=CARTESIAN_POINT('Ctrl Pts',(17.0072585948304,15.7239905936182,4.85932278607112));
#129760=CARTESIAN_POINT('Ctrl Pts',(17.0075847126636,15.7272350577276,4.8630079759129));
#129761=CARTESIAN_POINT('Ctrl Pts',(17.008371363781,15.734946043608,4.87190211154157));
#129762=CARTESIAN_POINT('Ctrl Pts',(17.0088337256631,15.7393853666401,4.87713410956155));
#129763=CARTESIAN_POINT('Ctrl Pts',(17.0105063972969,15.7551275584549,4.89609263799861));
#129764=CARTESIAN_POINT('Ctrl Pts',(17.0117355789586,15.7661062963535,4.91008239176833));
#129765=CARTESIAN_POINT('Ctrl Pts',(17.0150552848717,15.79435967144,4.9482041347071));
#129766=CARTESIAN_POINT('Ctrl Pts',(17.017169947176,15.8109193513682,4.97284197203264));
#129767=CARTESIAN_POINT('Ctrl Pts',(17.0248063663458,15.8663189015304,5.06406909866737));
#129768=CARTESIAN_POINT('Ctrl Pts',(17.0303200594861,15.8983072586581,5.13449707694267));
#129769=CARTESIAN_POINT('Ctrl Pts',(17.0365327385846,15.9259692603401,5.22179786480939));
#129770=CARTESIAN_POINT('Ctrl Pts',(17.0375060265478,15.9300349488594,5.23570748953081));
#129771=CARTESIAN_POINT('Ctrl Pts',(17.0390822427881,15.9361729904792,5.25860685255865));
#129772=CARTESIAN_POINT('Ctrl Pts',(17.0396909828186,15.9384319932439,5.2675437167275));
#129773=CARTESIAN_POINT('Ctrl Pts',(17.0408736396669,15.9425994079716,5.28508251958931));
#129774=CARTESIAN_POINT('Ctrl Pts',(17.0414478480907,15.9445187181497,5.29368091031825));
#129775=CARTESIAN_POINT('Ctrl Pts',(17.0428167427146,15.948840701846,5.31436920294445));
#129776=CARTESIAN_POINT('Ctrl Pts',(17.0436078412074,15.9511302568103,5.32648133621391));
#129777=CARTESIAN_POINT('Ctrl Pts',(17.0465566649586,15.9588639238478,5.37216415515685));
#129778=CARTESIAN_POINT('Ctrl Pts',(17.0486674264615,15.9627674321898,5.40597210521097));
#129779=CARTESIAN_POINT('Ctrl Pts',(17.054919583033,15.9691224912061,5.50803105509186));
#129780=CARTESIAN_POINT('Ctrl Pts',(17.0589375661397,15.9661395241976,5.57639694824305));
#129781=CARTESIAN_POINT('Ctrl Pts',(17.0646617781144,15.952299510654,5.66835712668768));
#129782=CARTESIAN_POINT('Ctrl Pts',(17.066209142905,15.9476763059727,5.69268598518938));
#129783=CARTESIAN_POINT('Ctrl Pts',(17.0683050445963,15.9403638423426,5.7244617613827));
#129784=CARTESIAN_POINT('Ctrl Pts',(17.068814180564,15.9385094738968,5.73209307664392));
#129785=CARTESIAN_POINT('Ctrl Pts',(17.0696278592342,15.9354279575539,5.74413322881435));
#129786=CARTESIAN_POINT('Ctrl Pts',(17.0699290965608,15.9342620750389,5.74855757929147));
#129787=CARTESIAN_POINT('Ctrl Pts',(17.0705746396514,15.9317118231857,5.75796390667448));
#129788=CARTESIAN_POINT('Ctrl Pts',(17.0709194412268,15.9303188111271,5.76294334937198));
#129789=CARTESIAN_POINT('Ctrl Pts',(17.0718239802219,15.9265828187025,5.77589656159812));
#129790=CARTESIAN_POINT('Ctrl Pts',(17.0723870275845,15.9241768881022,5.78385154717093));
#129791=CARTESIAN_POINT('Ctrl Pts',(17.0752364134043,15.9115875727676,5.82361921480091));
#129792=CARTESIAN_POINT('Ctrl Pts',(17.0775902755841,15.8998635936921,5.8549174300905));
#129793=CARTESIAN_POINT('Ctrl Pts',(17.0839033999428,15.864512540436,5.9362061688339));
#129794=CARTESIAN_POINT('Ctrl Pts',(17.0878888324592,15.8381760337433,5.98489102557268));
#129795=CARTESIAN_POINT('Ctrl Pts',(17.0923404979088,15.8034426860291,6.03772580694495));
#129796=CARTESIAN_POINT('Ctrl Pts',(17.0929001330538,15.798978371731,6.04433699068287));
#129797=CARTESIAN_POINT('Ctrl Pts',(17.0955457325953,15.7774028353802,6.07545071491485));
#129798=CARTESIAN_POINT('Ctrl Pts',(17.0976003791149,15.759242097443,6.09920817909452));
#129799=CARTESIAN_POINT('Ctrl Pts',(17.1004313352177,15.7322004709816,6.13137567991266));
#129800=CARTESIAN_POINT('Ctrl Pts',(17.1012417902442,15.7242184665974,6.14051574064338));
#129801=CARTESIAN_POINT('Ctrl Pts',(17.1026265289631,15.7101689767015,6.15600505699528));
#129802=CARTESIAN_POINT('Ctrl Pts',(17.1032040678017,15.7041833272325,6.1624261924069));
#129803=CARTESIAN_POINT('Ctrl Pts',(17.10438452871,15.6916930222926,6.17546457898329));
#129804=CARTESIAN_POINT('Ctrl Pts',(17.1049869621035,15.685178879644,6.18207151176312));
#129805=CARTESIAN_POINT('Ctrl Pts',(17.106539523719,15.668035486275,6.19896560579679));
#129806=CARTESIAN_POINT('Ctrl Pts',(17.1074833201627,15.6572632483098,6.20910463825069));
#129807=CARTESIAN_POINT('Ctrl Pts',(17.109544581392,15.6330015702537,6.23091208992195));
#129808=CARTESIAN_POINT('Ctrl Pts',(17.1106574651702,15.6194133045659,6.24246258027983));
#129809=CARTESIAN_POINT('Ctrl Pts',(17.1142102854606,15.5746067486109,6.27846287129403));
#129810=CARTESIAN_POINT('Ctrl Pts',(17.1166030389666,15.5422012277256,6.301370983305));
#129811=CARTESIAN_POINT('Ctrl Pts',(17.1226151839751,15.4572745987172,6.3538911921325));
#129812=CARTESIAN_POINT('Ctrl Pts',(17.1262112402832,15.4032300651862,6.38070081854876));
#129813=CARTESIAN_POINT('Ctrl Pts',(17.1306838806059,15.3377283540409,6.40589453769879));
#129814=CARTESIAN_POINT('Ctrl Pts',(17.1313270108584,15.3283500470545,6.40933579206176));
#129815=CARTESIAN_POINT('Ctrl Pts',(17.1323380250233,15.3137051481468,6.41445347857233));
#129816=CARTESIAN_POINT('Ctrl Pts',(17.1327004490219,15.3084743815264,6.41623121359989));
#129817=CARTESIAN_POINT('Ctrl Pts',(17.1333939607351,15.2985085135548,6.41952321471357));
#129818=CARTESIAN_POINT('Ctrl Pts',(17.1337245759304,15.2937765165227,6.42104594287271));
#129819=CARTESIAN_POINT('Ctrl Pts',(17.1345440398682,15.282090371369,6.42470726102692));
#129820=CARTESIAN_POINT('Ctrl Pts',(17.1350351327719,15.2751235088988,6.42680394003697));
#129821=CARTESIAN_POINT('Ctrl Pts',(17.1369613969367,15.2479127128858,6.43465920116543));
#129822=CARTESIAN_POINT('Ctrl Pts',(17.1384233045867,15.2275078076048,6.43983434383364));
#129823=CARTESIAN_POINT('Ctrl Pts',(17.142674254307,15.1684627538008,6.45277407304656));
#129824=CARTESIAN_POINT('Ctrl Pts',(17.1455033208931,15.1294952536638,6.45884768982404));
#129825=CARTESIAN_POINT('Ctrl Pts',(17.1526266015848,15.0304146237354,6.46813965270383));
#129826=CARTESIAN_POINT('Ctrl Pts',(17.1568864661465,14.9701604162608,6.46815859511631));
#129827=CARTESIAN_POINT('Ctrl Pts',(17.162073669323,14.8943261133081,6.46109082360551));
#129828=CARTESIAN_POINT('Ctrl Pts',(17.1631538058722,14.8784034487245,6.45920637590301));
#129829=CARTESIAN_POINT('Ctrl Pts',(17.1648565480208,14.8531043456944,6.45557207273387));
#129830=CARTESIAN_POINT('Ctrl Pts',(17.1654868782415,14.8436947717267,6.45407809215954));
#129831=CARTESIAN_POINT('Ctrl Pts',(17.1666835173301,14.8257534473216,6.45095694212353));
#129832=CARTESIAN_POINT('Ctrl Pts',(17.1672504980261,14.8172185860916,6.4493534271853));
#129833=CARTESIAN_POINT('Ctrl Pts',(17.1685599681171,14.7974363666491,6.44536010222345));
#129834=CARTESIAN_POINT('Ctrl Pts',(17.1692996979501,14.786207598781,6.44288417926362));
#129835=CARTESIAN_POINT('Ctrl Pts',(17.1717818011826,14.7483876693906,6.43383456042668));
#129836=CARTESIAN_POINT('Ctrl Pts',(17.1734952829874,14.7220314533522,6.42633117010752));
#129837=CARTESIAN_POINT('Ctrl Pts',(17.1778861455186,14.6544382398202,6.40394251541647));
#129838=CARTESIAN_POINT('Ctrl Pts',(17.1805187632866,14.6138318129792,6.38735528813823));
#129839=CARTESIAN_POINT('Ctrl Pts',(17.1863435116237,14.5269524741419,6.34476881263823));
#129840=CARTESIAN_POINT('Ctrl Pts',(17.1895279123647,14.4814151126276,6.31760426058058));
#129841=CARTESIAN_POINT('Ctrl Pts',(17.1935559668098,14.4298787200643,6.28081703817897));
#129842=CARTESIAN_POINT('Ctrl Pts',(17.194223835475,14.4215201473601,6.27464479639575));
#129843=CARTESIAN_POINT('Ctrl Pts',(17.1952690618377,14.4087584399973,6.26489940848967));
#129844=CARTESIAN_POINT('Ctrl Pts',(17.1956404890185,14.4042842788252,6.2614200306366));
#129845=CARTESIAN_POINT('Ctrl Pts',(17.1963397375666,14.3959806083238,6.25484461031386));
#129846=CARTESIAN_POINT('Ctrl Pts',(17.1966669155138,14.3921437666636,6.25175834317565));
#129847=CARTESIAN_POINT('Ctrl Pts',(17.1974619511648,14.3829342474817,6.24423382258601));
#129848=CARTESIAN_POINT('Ctrl Pts',(17.1979317448755,14.3775857492722,6.2397665977753));
#129849=CARTESIAN_POINT('Ctrl Pts',(17.1996662916528,14.3581616088595,6.22318321552687));
#129850=CARTESIAN_POINT('Ctrl Pts',(17.2009517063024,14.344388431949,6.21072065884791));
#129851=CARTESIAN_POINT('Ctrl Pts',(17.2044823381726,14.3080082914622,6.17584468015182));
#129852=CARTESIAN_POINT('Ctrl Pts',(17.2067550478549,14.2861356708602,6.15269906940836));
#129853=CARTESIAN_POINT('Ctrl Pts',(17.214233822534,14.21822033755,6.07332586059523));
#129854=CARTESIAN_POINT('Ctrl Pts',(17.219419526279,14.1773577328399,6.01297674458097));
#129855=CARTESIAN_POINT('Ctrl Pts',(17.2253832805294,14.1366301730942,5.93523126106986));
#129856=CARTESIAN_POINT('Ctrl Pts',(17.2263991898725,14.1299352931855,5.92168846039345));
#129857=CARTESIAN_POINT('Ctrl Pts',(17.2280259072467,14.1196182694233,5.89952573834837));
#129858=CARTESIAN_POINT('Ctrl Pts',(17.2286432664246,14.1157991604781,5.89100088589861));
#129859=CARTESIAN_POINT('Ctrl Pts',(17.2298308590498,14.1086432600245,5.87438652095032));
#129860=CARTESIAN_POINT('Ctrl Pts',(17.2304015434043,14.1052915802733,5.86630445928171));
#129861=CARTESIAN_POINT('Ctrl Pts',(17.2317433350006,14.0976221251964,5.84707717181626));
#129862=CARTESIAN_POINT('Ctrl Pts',(17.2325112330752,14.0934003435546,5.83589503574992));
#129863=CARTESIAN_POINT('Ctrl Pts',(17.2352356753645,14.0790436680399,5.79562428986589));
#129864=CARTESIAN_POINT('Ctrl Pts',(17.2371545689029,14.0700923216056,5.76613204447125));
#129865=CARTESIAN_POINT('Ctrl Pts',(17.2439463334806,14.043049831694,5.65883260937626));
#129866=CARTESIAN_POINT('Ctrl Pts',(17.2486080869679,14.033205421626,5.57929423180456));
#129867=CARTESIAN_POINT('Ctrl Pts',(17.2535748249259,14.0332501517357,5.49945835346593));
#129868=CARTESIAN_POINT('Origin',(16.125,15.,5.5));
#129869=CARTESIAN_POINT('',(17.7122358268452,14.0332503676593,5.5008431306014));
#129870=CARTESIAN_POINT('',(17.654370605628,14.0332503772168,5.50085402224954));
#129871=CARTESIAN_POINT('',(16.125,14.03325,5.5));
#129872=CARTESIAN_POINT('Ctrl Pts',(17.7122358268452,14.0332503676593,5.50084313060139));
#129873=CARTESIAN_POINT('Ctrl Pts',(17.7087976196952,14.0332959166321,5.55307045170094));
#129874=CARTESIAN_POINT('Ctrl Pts',(17.7053594125452,14.0375775866098,5.60511395562003));
#129875=CARTESIAN_POINT('Ctrl Pts',(17.7019212053952,14.0459839817697,5.65639373216326));
#129876=CARTESIAN_POINT('Ctrl Pts',(17.7001166244923,14.0503961708862,5.68330848785335));
#129877=CARTESIAN_POINT('Ctrl Pts',(17.6983120435895,14.0559438391561,5.71001327697186));
#129878=CARTESIAN_POINT('Ctrl Pts',(17.6965074626866,14.0626057458369,5.7364266794632));
#129879=CARTESIAN_POINT('Ctrl Pts',(17.6938358502455,14.0724684417909,5.77553070333594));
#129880=CARTESIAN_POINT('Ctrl Pts',(17.6911642378045,14.0848048701166,5.81410643268523));
#129881=CARTESIAN_POINT('Ctrl Pts',(17.6884926253634,14.0995398785608,5.85181974389983));
#129882=CARTESIAN_POINT('Ctrl Pts',(17.6858250159401,14.1142528087655,5.88947654727291));
#129883=CARTESIAN_POINT('Ctrl Pts',(17.6831574065167,14.1313570047041,5.92627294634419));
#129884=CARTESIAN_POINT('Ctrl Pts',(17.6804897970933,14.1507273254122,5.961889041544));
#129885=CARTESIAN_POINT('Ctrl Pts',(17.6778248925357,14.1700780052703,5.99746902322807));
#129886=CARTESIAN_POINT('Ctrl Pts',(17.6751599879781,14.1916899873374,6.03187055612003));
#129887=CARTESIAN_POINT('Ctrl Pts',(17.6724950834204,14.2153909552819,6.06479572364407));
#129888=CARTESIAN_POINT('Ctrl Pts',(17.6698315903055,14.2390793702223,6.09770345264968));
#129889=CARTESIAN_POINT('Ctrl Pts',(17.6671680971905,14.264854239059,6.1291358905146));
#129890=CARTESIAN_POINT('Ctrl Pts',(17.6645046040756,14.2925001081522,6.15882430551352));
#129891=CARTESIAN_POINT('Ctrl Pts',(17.6618391798863,14.3201660209349,6.18853424507983));
#129892=CARTESIAN_POINT('Ctrl Pts',(17.659173755697,14.3497052514647,6.21649720022547));
#129893=CARTESIAN_POINT('Ctrl Pts',(17.6565083315077,14.3808637634722,6.24247955063976));
#129894=CARTESIAN_POINT('Ctrl Pts',(17.6538420766206,14.4120319862438,6.26846999863179));
#129895=CARTESIAN_POINT('Ctrl Pts',(17.6511758217336,14.4448200291885,6.2924782572714));
#129896=CARTESIAN_POINT('Ctrl Pts',(17.6485095668466,14.4789420220101,6.31431206921736));
#129897=CARTESIAN_POINT('Ctrl Pts',(17.645837912486,14.5131331158004,6.3361900971493));
#129898=CARTESIAN_POINT('Ctrl Pts',(17.6431662581255,14.5486630462699,6.3558845898121));
#129899=CARTESIAN_POINT('Ctrl Pts',(17.640494603765,14.5852199411891,6.37324857017508));
#129900=CARTESIAN_POINT('Ctrl Pts',(17.6381867010175,14.6167995345197,6.38824840644879));
#129901=CARTESIAN_POINT('Ctrl Pts',(17.6358787982699,14.6491448829356,6.40150982190342));
#129902=CARTESIAN_POINT('Ctrl Pts',(17.6335708955224,14.6820450946975,6.41296782018541));
#129903=CARTESIAN_POINT('Ctrl Pts',(17.6308993644067,14.7201289955596,6.42623111690236));
#129904=CARTESIAN_POINT('Ctrl Pts',(17.6282278332909,14.7591318060258,6.43713787356378));
#129905=CARTESIAN_POINT('Ctrl Pts',(17.6255563021752,14.7987331433189,6.44556713928822));
#129906=CARTESIAN_POINT('Ctrl Pts',(17.6228887738615,14.8382751452319,6.45398377529558));
#129907=CARTESIAN_POINT('Ctrl Pts',(17.6202212455479,14.8784133342073,6.45993013643737));
#129908=CARTESIAN_POINT('Ctrl Pts',(17.6175537172342,14.9188117202061,6.46333484610706));
#129909=CARTESIAN_POINT('Ctrl Pts',(17.6148888933841,14.9591691484524,6.46673610392459));
#129910=CARTESIAN_POINT('Ctrl Pts',(17.6122240695341,14.9997856714742,6.4676007574624));
#129911=CARTESIAN_POINT('Ctrl Pts',(17.609559245684,15.040317720132,6.46590892114286));
#129912=CARTESIAN_POINT('Ctrl Pts',(17.606895832688,15.0808283096587,6.46421798054259));
#129913=CARTESIAN_POINT('Ctrl Pts',(17.6042324196919,15.1212539297447,6.45997325441683));
#129914=CARTESIAN_POINT('Ctrl Pts',(17.6015690066959,15.1612516684648,6.4532069355168));
#129915=CARTESIAN_POINT('Ctrl Pts',(17.5989036609282,15.2012784325346,6.44643570646987));
#129916=CARTESIAN_POINT('Ctrl Pts',(17.5962383151606,15.2408761153243,6.43713931740122));
#129917=CARTESIAN_POINT('Ctrl Pts',(17.593572969393,15.2797099169859,6.42540149386077));
#129918=CARTESIAN_POINT('Ctrl Pts',(17.5909067921151,15.3185558336613,6.41366000846162));
#129919=CARTESIAN_POINT('Ctrl Pts',(17.5882406148373,15.3566368413702,6.39947576590505));
#129920=CARTESIAN_POINT('Ctrl Pts',(17.5855744375595,15.393635185694,6.38298182488861));
#129921=CARTESIAN_POINT('Ctrl Pts',(17.5829028583062,15.4307084928317,6.3664544652895));
#129922=CARTESIAN_POINT('Ctrl Pts',(17.5802312790529,15.4666942304483,6.34760832401572));
#129923=CARTESIAN_POINT('Ctrl Pts',(17.5775596997995,15.5012981683483,6.32662307547673));
#129924=CARTESIAN_POINT('Ctrl Pts',(17.5752512426524,15.5311987253555,6.30849015019922));
#129925=CARTESIAN_POINT('Ctrl Pts',(17.5729427855053,15.5600678254938,6.28876097242699));
#129926=CARTESIAN_POINT('Ctrl Pts',(17.5706343283582,15.5877350985541,6.26757606556457));
#129927=CARTESIAN_POINT('Ctrl Pts',(17.5679629006329,15.619752639113,6.24306014694741));
#129928=CARTESIAN_POINT('Ctrl Pts',(17.5652914729076,15.65030732673,6.21648107266194));
#129929=CARTESIAN_POINT('Ctrl Pts',(17.5626200451824,15.6791219749082,6.1880399012389));
#129930=CARTESIAN_POINT('Ctrl Pts',(17.5599526226303,15.7078934223451,6.15964137061709));
#129931=CARTESIAN_POINT('Ctrl Pts',(17.5572852000783,15.734929573689,6.12938666818248));
#129932=CARTESIAN_POINT('Ctrl Pts',(17.5546177775262,15.7599860639873,6.09751715041915));
#129933=CARTESIAN_POINT('Ctrl Pts',(17.5519530615594,15.78501712992,6.06567997007675));
#129934=CARTESIAN_POINT('Ctrl Pts',(17.5492883455926,15.8080721472486,6.03223167286745));
#129935=CARTESIAN_POINT('Ctrl Pts',(17.5466236296258,15.8289455889551,5.99744826168351));
#129936=CARTESIAN_POINT('Ctrl Pts',(17.5439603263891,15.8498079643637,5.96268329132948));
#129937=CARTESIAN_POINT('Ctrl Pts',(17.5412970231525,15.8684907536195,5.92658510943038));
#129938=CARTESIAN_POINT('Ctrl Pts',(17.5386337199158,15.8848322879557,5.88945780861491));
#129939=CARTESIAN_POINT('Ctrl Pts',(17.5359684857979,15.9011856698206,5.85230359069643));
#129940=CARTESIAN_POINT('Ctrl Pts',(17.5333032516801,15.9151941608265,5.81411929606249));
#129941=CARTESIAN_POINT('Ctrl Pts',(17.5306380175622,15.9267435947425,5.77523057988494));
#129942=CARTESIAN_POINT('Ctrl Pts',(17.5279719531495,15.9382966266297,5.73632974878616));
#129943=CARTESIAN_POINT('Ctrl Pts',(17.5253058887367,15.9473889337335,5.69672462802192));
#129944=CARTESIAN_POINT('Ctrl Pts',(17.522639824324,15.9539569277647,5.65675376381363));
#129945=CARTESIAN_POINT('Ctrl Pts',(17.5199683583395,15.9605382288602,5.61670191675729));
#129946=CARTESIAN_POINT('Ctrl Pts',(17.5172968923551,15.9645849334581,5.57628342960348));
#129947=CARTESIAN_POINT('Ctrl Pts',(17.5146254263706,15.966085324279,5.53584283349242));
#129948=CARTESIAN_POINT('Ctrl Pts',(17.5123162046451,15.9673822657713,5.5008858833844));
#129949=CARTESIAN_POINT('Ctrl Pts',(17.5100069829195,15.9667774868603,5.4659126948984));
#129950=CARTESIAN_POINT('Ctrl Pts',(17.507697761194,15.9642947089741,5.43114307046806));
#129951=CARTESIAN_POINT('Ctrl Pts',(17.5050262537061,15.9614224167033,5.39091856063004));
#129952=CARTESIAN_POINT('Ctrl Pts',(17.5023547462182,15.956022332195,5.35078154256967));
#129953=CARTESIAN_POINT('Ctrl Pts',(17.4996832387303,15.9481099992535,5.31107411025631));
#129954=CARTESIAN_POINT('Ctrl Pts',(17.4970157351346,15.9402095248333,5.27142618901659));
#129955=CARTESIAN_POINT('Ctrl Pts',(17.4943482315389,15.9298043571631,5.23220714982284));
#129956=CARTESIAN_POINT('Ctrl Pts',(17.4916807279432,15.9169617461634,5.19375382684363));
#129957=CARTESIAN_POINT('Ctrl Pts',(17.4890159298416,15.9041321606786,5.15533950483774));
#129958=CARTESIAN_POINT('Ctrl Pts',(17.4863511317399,15.8888702055026,5.11768991576088));
#129959=CARTESIAN_POINT('Ctrl Pts',(17.4836863336383,15.8712934238896,5.08112850182088));
#129960=CARTESIAN_POINT('Ctrl Pts',(17.4810229473632,15.8537259545644,5.04458645834481));
#129961=CARTESIAN_POINT('Ctrl Pts',(17.4783595610881,15.8338463402288,5.00913197494729));
#129962=CARTESIAN_POINT('Ctrl Pts',(17.475696174813,15.811819701173,4.97506730404046));
#129963=CARTESIAN_POINT('Ctrl Pts',(17.4730308570369,15.7897770882886,4.94097792926422));
#129964=CARTESIAN_POINT('Ctrl Pts',(17.4703655392608,15.7655846503951,4.90828087799683));
#129965=CARTESIAN_POINT('Ctrl Pts',(17.4677002214847,15.7394516367196,4.87725058052796));
#129966=CARTESIAN_POINT('Ctrl Pts',(17.4650340729418,15.7133104775087,4.84621061106385));
#129967=CARTESIAN_POINT('Ctrl Pts',(17.4623679243989,15.6852279349662,4.81683886146808));
#129968=CARTESIAN_POINT('Ctrl Pts',(17.459701775856,15.6554518354536,4.78937460367608));
#129969=CARTESIAN_POINT('Ctrl Pts',(17.4570302261723,15.6256154148804,4.76185470820196));
#129970=CARTESIAN_POINT('Ctrl Pts',(17.4543586764885,15.5940790345019,4.73625040050669));
#129971=CARTESIAN_POINT('Ctrl Pts',(17.4516871268047,15.561124040503,4.7127609170845));
#129972=CARTESIAN_POINT('Ctrl Pts',(17.4493784825464,15.5326456789959,4.69246226369885));
#129973=CARTESIAN_POINT('Ctrl Pts',(17.4470698382881,15.5031086477845,4.67374233222166));
#129974=CARTESIAN_POINT('Ctrl Pts',(17.4447611940298,15.4727094250297,4.65670209179192));
#129975=CARTESIAN_POINT('Ctrl Pts',(17.4420897043288,15.4375324114138,4.63698366759239));
#129976=CARTESIAN_POINT('Ctrl Pts',(17.4394182146278,15.4010385654625,4.61942467951124));
#129977=CARTESIAN_POINT('Ctrl Pts',(17.4367467249268,15.3635221663353,4.60420024721878));
#129978=CARTESIAN_POINT('Ctrl Pts',(17.4340792392166,15.3260619962548,4.58899863308942));
#129979=CARTESIAN_POINT('Ctrl Pts',(17.4314117535064,15.2875828395704,4.57612487716833));
#129980=CARTESIAN_POINT('Ctrl Pts',(17.4287442677963,15.2484030134787,4.56570801919597));
#129981=CARTESIAN_POINT('Ctrl Pts',(17.4260794876373,15.2092629263167,4.55530172673215));
#129982=CARTESIAN_POINT('Ctrl Pts',(17.4234147074784,15.1694241382623,4.54734755368335));
#129983=CARTESIAN_POINT('Ctrl Pts',(17.4207499273195,15.1292214351756,4.54192516827173));
#129984=CARTESIAN_POINT('Ctrl Pts',(17.4180865590031,15.0890400321146,4.53650565572536));
#129985=CARTESIAN_POINT('Ctrl Pts',(17.4154231906867,15.0484956747044,4.53361535292633));
#129986=CARTESIAN_POINT('Ctrl Pts',(17.4127598223703,15.0079316105748,4.53328253762866));
#129987=CARTESIAN_POINT('Ctrl Pts',(17.4100945224049,14.9673381267315,4.53294948095155));
#129988=CARTESIAN_POINT('Ctrl Pts',(17.4074292224396,14.9267254937623,4.53517763170673));
#129989=CARTESIAN_POINT('Ctrl Pts',(17.4047639224742,14.8864379853199,4.5399431103722));
#129990=CARTESIAN_POINT('Ctrl Pts',(17.4020977916883,14.8461379185584,4.54471007452049));
#129991=CARTESIAN_POINT('Ctrl Pts',(17.3994316609024,14.8061637568535,4.55201584731124));
#129992=CARTESIAN_POINT('Ctrl Pts',(17.3967655301166,14.7668516193589,4.56178499526791));
#129993=CARTESIAN_POINT('Ctrl Pts',(17.3940939978403,14.7274598368098,4.57157393518635));
#129994=CARTESIAN_POINT('Ctrl Pts',(17.3914224655641,14.6887333202173,4.58383605050688));
#129995=CARTESIAN_POINT('Ctrl Pts',(17.3887509332878,14.6509931797788,4.59844589627739));
#129996=CARTESIAN_POINT('Ctrl Pts',(17.3864421644805,14.6183777179312,4.6110718924128));
#129997=CARTESIAN_POINT('Ctrl Pts',(17.3841333956731,14.5864988586795,4.62545041278623));
#129998=CARTESIAN_POINT('Ctrl Pts',(17.3818246268657,14.5555490039028,4.64147284575955));
#129999=CARTESIAN_POINT('Ctrl Pts',(17.3791531481338,14.5197368955058,4.66001241922649));
#130000=CARTESIAN_POINT('Ctrl Pts',(17.3764816694018,14.4850043907671,4.68083925012965));
#130001=CARTESIAN_POINT('Ctrl Pts',(17.3738101906699,14.4516595701061,4.70380383356625));
#130002=CARTESIAN_POINT('Ctrl Pts',(17.3711427162105,14.4183647299116,4.72673399544748));
#130003=CARTESIAN_POINT('Ctrl Pts',(17.3684752417512,14.3864539404335,4.75179524771507));
#130004=CARTESIAN_POINT('Ctrl Pts',(17.3658077672919,14.3562100113391,4.77879266989304));
#130005=CARTESIAN_POINT('Ctrl Pts',(17.363142998639,14.3259967607829,4.80576270669245));
#130006=CARTESIAN_POINT('Ctrl Pts',(17.3604782299861,14.2974474614101,4.83466464131405));
#130007=CARTESIAN_POINT('Ctrl Pts',(17.3578134613331,14.2708127406299,4.86526265016752));
#130008=CARTESIAN_POINT('Ctrl Pts',(17.3551501047518,14.2441921336945,4.89584444501406));
#130009=CARTESIAN_POINT('Ctrl Pts',(17.3524867481704,14.219484480074,4.92812009391392));
#130010=CARTESIAN_POINT('Ctrl Pts',(17.349823391589,14.1969021358283,4.96181844786091));
#130011=CARTESIAN_POINT('Ctrl Pts',(17.3471581036054,14.174303415409,4.99554123904472));
#130012=CARTESIAN_POINT('Ctrl Pts',(17.3444928156218,14.1538334176651,5.03068831470276));
#130013=CARTESIAN_POINT('Ctrl Pts',(17.3418275276382,14.135661498133,5.06695898959753));
#130014=CARTESIAN_POINT('Ctrl Pts',(17.3391614089887,14.1174839151253,5.10324096864127));
#130015=CARTESIAN_POINT('Ctrl Pts',(17.3364952903393,14.1016060760367,5.14064670903404));
#130016=CARTESIAN_POINT('Ctrl Pts',(17.3338291716898,14.0881497917777,5.17885398918091));
#130017=CARTESIAN_POINT('Ctrl Pts',(17.3311576516337,14.0746662458428,5.21713867513091));
#130018=CARTESIAN_POINT('Ctrl Pts',(17.3284861315776,14.0636142227846,5.25622758181451));
#130019=CARTESIAN_POINT('Ctrl Pts',(17.3258146115215,14.0550655082373,5.29578352471683));
#130020=CARTESIAN_POINT('Ctrl Pts',(17.3235057609149,14.0476773156149,5.32996959139418));
#130021=CARTESIAN_POINT('Ctrl Pts',(17.3211969103082,14.0421580952794,5.36450406953048));
#130022=CARTESIAN_POINT('Ctrl Pts',(17.3188880597015,14.0385229231138,5.39916650793299));
#130023=CARTESIAN_POINT('Ctrl Pts',(17.3166706787643,14.0350317654615,5.43245572549052));
#130024=CARTESIAN_POINT('Ctrl Pts',(17.314453297827,14.0332691004685,5.46592930822326));
#130025=CARTESIAN_POINT('Ctrl Pts',(17.3122359168897,14.0332501543841,5.49945364696662));
#130026=CARTESIAN_POINT('Ctrl Pts',(17.2535748450812,14.0332501519173,5.49945802948715));
#130027=CARTESIAN_POINT('Ctrl Pts',(17.2543247186306,14.0332569092666,5.48740448371654));
#130028=CARTESIAN_POINT('Ctrl Pts',(17.2550815808894,14.033489093376,5.47535260252305));
#130029=CARTESIAN_POINT('Ctrl Pts',(17.2563749225964,14.0342612417695,5.45502252247803));
#130030=CARTESIAN_POINT('Ctrl Pts',(17.2569064296428,14.0346825426573,5.4467410188117));
#130031=CARTESIAN_POINT('Ctrl Pts',(17.2577766650328,14.0355383683539,5.4333224954904));
#130032=CARTESIAN_POINT('Ctrl Pts',(17.2581122261669,14.0359075574332,5.42818156267272));
#130033=CARTESIAN_POINT('Ctrl Pts',(17.2587475267943,14.0366793379702,5.41851693893325));
#130034=CARTESIAN_POINT('Ctrl Pts',(17.2590467783054,14.0370727373995,5.4139926012123));
#130035=CARTESIAN_POINT('Ctrl Pts',(17.2596966591357,14.0379907536201,5.40423224631418));
#130036=CARTESIAN_POINT('Ctrl Pts',(17.2600478721077,14.0385262668562,5.39899747504598));
#130037=CARTESIAN_POINT('Ctrl Pts',(17.2609882981898,14.0400649873054,5.38507942314247));
#130038=CARTESIAN_POINT('Ctrl Pts',(17.2615812900937,14.0411432500638,5.37640514692402));
#130039=CARTESIAN_POINT('Ctrl Pts',(17.2650899701888,14.0481586513915,5.32560569562272));
#130040=CARTESIAN_POINT('Ctrl Pts',(17.2681139638864,14.0567530995382,5.28389840008284));
#130041=CARTESIAN_POINT('Ctrl Pts',(17.2728344407192,14.0743035346338,5.22028233959132));
#130042=CARTESIAN_POINT('Ctrl Pts',(17.2745170884469,14.0813636659866,5.19790197784353));
#130043=CARTESIAN_POINT('Ctrl Pts',(17.2801887364239,14.1079999099434,5.12307314134545));
#130044=CARTESIAN_POINT('Ctrl Pts',(17.2841245219664,14.1313146654974,5.07206824675988));
#130045=CARTESIAN_POINT('Ctrl Pts',(17.288848539852,14.165713509303,5.01136755965406));
#130046=CARTESIAN_POINT('Ctrl Pts',(17.2897731553977,14.1727663841989,4.99952004229735));
#130047=CARTESIAN_POINT('Ctrl Pts',(17.2912917530246,14.1848801836336,4.9801272614319));
#130048=CARTESIAN_POINT('Ctrl Pts',(17.2918907397198,14.1897981504352,4.97249554343377));
#130049=CARTESIAN_POINT('Ctrl Pts',(17.2930625396891,14.1996926542071,4.95760611543204));
#130050=CARTESIAN_POINT('Ctrl Pts',(17.2936355339779,14.2046622110789,4.95034485027512));
#130051=CARTESIAN_POINT('Ctrl Pts',(17.2948991109822,14.2159089136869,4.93438370532776));
#130052=CARTESIAN_POINT('Ctrl Pts',(17.2955878557477,14.222233179841,4.92571835106705));
#130053=CARTESIAN_POINT('Ctrl Pts',(17.2980893158884,14.2458956577073,4.89440469950239));
#130054=CARTESIAN_POINT('Ctrl Pts',(17.2998695798597,14.2640902908091,4.87242040683532));
#130055=CARTESIAN_POINT('Ctrl Pts',(17.306033034434,14.3313142839145,4.79814587828379));
#130056=CARTESIAN_POINT('Ctrl Pts',(17.3102464203683,14.3851508415495,4.75053374347122));
#130057=CARTESIAN_POINT('Ctrl Pts',(17.3163390737033,14.4664145230372,4.69336508121755));
#130058=CARTESIAN_POINT('Ctrl Pts',(17.3180646058462,14.4897503101519,4.67840501264147));
#130059=CARTESIAN_POINT('Ctrl Pts',(17.3203539007209,14.5205407997681,4.66048394963582));
#130060=CARTESIAN_POINT('Ctrl Pts',(17.3208673639943,14.5274361509142,4.65658330445516));
#130061=CARTESIAN_POINT('Ctrl Pts',(17.3217191201378,14.5388396574904,4.65031616741772));
#130062=CARTESIAN_POINT('Ctrl Pts',(17.3220544277231,14.543320138849,4.64789966581242));
#130063=CARTESIAN_POINT('Ctrl Pts',(17.322699950325,14.5519240376989,4.64334659261929));
#130064=CARTESIAN_POINT('Ctrl Pts',(17.3230097547151,14.5560441410294,4.64120414448304));
#130065=CARTESIAN_POINT('Ctrl Pts',(17.3238729909078,14.5675035250802,4.63534977886605));
#130066=CARTESIAN_POINT('Ctrl Pts',(17.3244300347971,14.5748747948989,4.63170180539624));
#130067=CARTESIAN_POINT('Ctrl Pts',(17.3269903693181,14.6086881961767,4.61550162918485));
#130068=CARTESIAN_POINT('Ctrl Pts',(17.3290450071617,14.6356434328545,4.60406123260561));
#130069=CARTESIAN_POINT('Ctrl Pts',(17.3356706448702,14.7230975461629,4.57154341720252));
#130070=CARTESIAN_POINT('Ctrl Pts',(17.3403033159443,14.7851969536707,4.55524219321351));
#130071=CARTESIAN_POINT('Ctrl Pts',(17.3471188038722,14.8811975021898,4.54000481284117));
#130072=CARTESIAN_POINT('Ctrl Pts',(17.3494039966905,14.9141906918192,4.53649495359746));
#130073=CARTESIAN_POINT('Ctrl Pts',(17.3524628050184,14.9595146006904,4.53402066352866));
#130074=CARTESIAN_POINT('Ctrl Pts',(17.3532799664084,14.9717388478542,4.53358576358348));
#130075=CARTESIAN_POINT('Ctrl Pts',(17.3546724677809,14.992760900117,4.53323711037753));
#130076=CARTESIAN_POINT('Ctrl Pts',(17.3552511607009,15.0015550704157,4.53321125389845));
#130077=CARTESIAN_POINT('Ctrl Pts',(17.3564308241142,15.0195943127416,4.5334043668191));
#130078=CARTESIAN_POINT('Ctrl Pts',(17.3570313468656,15.0288383612637,4.53363598280809));
#130079=CARTESIAN_POINT('Ctrl Pts',(17.3585721514065,15.052701092411,4.53457660767245));
#130080=CARTESIAN_POINT('Ctrl Pts',(17.3595062896233,15.0673098426854,4.53548501714557));
#130081=CARTESIAN_POINT('Ctrl Pts',(17.365240279008,15.1576935768077,4.54316900210194));
#130082=CARTESIAN_POINT('Ctrl Pts',(17.3697588957289,15.2324679043734,4.55853704378782));
#130083=CARTESIAN_POINT('Ctrl Pts',(17.3761754626059,15.3332796845443,4.59201382937322));
#130084=CARTESIAN_POINT('Ctrl Pts',(17.3780084369784,15.3614260895656,4.60284606015946));
#130085=CARTESIAN_POINT('Ctrl Pts',(17.3810078208716,15.4054584835517,4.62220078124195));
#130086=CARTESIAN_POINT('Ctrl Pts',(17.3821436838015,15.4216926694521,4.62988319636871));
#130087=CARTESIAN_POINT('Ctrl Pts',(17.3837481257597,15.4438421035046,4.64113029723895));
#130088=CARTESIAN_POINT('Ctrl Pts',(17.3841963320234,15.4499481767441,4.64431336880373));
#130089=CARTESIAN_POINT('Ctrl Pts',(17.3849710463743,15.4603517326595,4.64987884160691));
#130090=CARTESIAN_POINT('Ctrl Pts',(17.3852956344526,15.4646659447153,4.65222924066097));
#130091=CARTESIAN_POINT('Ctrl Pts',(17.3860021857633,15.4739575250388,4.65738356375072));
#130092=CARTESIAN_POINT('Ctrl Pts',(17.386384782454,15.478928012001,4.66019874404365));
#130093=CARTESIAN_POINT('Ctrl Pts',(17.387484479889,15.4930501913619,4.66836339641623));
#130094=CARTESIAN_POINT('Ctrl Pts',(17.3882075669692,15.502138950625,4.67381939996979));
#130095=CARTESIAN_POINT('Ctrl Pts',(17.3918081718366,15.5465199913123,4.70146427338571));
#130096=CARTESIAN_POINT('Ctrl Pts',(17.3947789304895,15.58043867426,4.72576892131138));
#130097=CARTESIAN_POINT('Ctrl Pts',(17.4013641814037,15.6516085659239,4.78407786977893));
#130098=CARTESIAN_POINT('Ctrl Pts',(17.4049723311714,15.6879904429575,4.81896540390468));
#130099=CARTESIAN_POINT('Ctrl Pts',(17.4106325598203,15.7418935243969,4.8794042834374));
#130100=CARTESIAN_POINT('Ctrl Pts',(17.4127396245306,15.7611970837907,4.90323842277798));
#130101=CARTESIAN_POINT('Ctrl Pts',(17.4156066956423,15.7863979188752,4.93757110732959));
#130102=CARTESIAN_POINT('Ctrl Pts',(17.4164032909988,15.7932801822665,4.94732059932046));
#130103=CARTESIAN_POINT('Ctrl Pts',(17.4177720556238,15.8048911089773,4.9644326763853));
#130104=CARTESIAN_POINT('Ctrl Pts',(17.4183472795598,15.8097034617819,4.97173645991493));
#130105=CARTESIAN_POINT('Ctrl Pts',(17.4195297898079,15.8194526393979,4.98697923258663));
#130106=CARTESIAN_POINT('Ctrl Pts',(17.4201364989245,15.8243747739359,4.99492656173603));
#130107=CARTESIAN_POINT('Ctrl Pts',(17.4217152577608,15.8369645600532,5.01592865626018));
#130108=CARTESIAN_POINT('Ctrl Pts',(17.4226805492907,15.8444423507405,5.02909459981354));
#130109=CARTESIAN_POINT('Ctrl Pts',(17.4282058164764,15.8858677349724,5.10619383633156));
#130110=CARTESIAN_POINT('Ctrl Pts',(17.432517540193,15.912858330038,5.17360203602639));
#130111=CARTESIAN_POINT('Ctrl Pts',(17.4388135335007,15.9405570262538,5.27421311593733));
#130112=CARTESIAN_POINT('Ctrl Pts',(17.4407524753761,15.9475070326552,5.30543019800855));
#130113=CARTESIAN_POINT('Ctrl Pts',(17.443902198176,15.9560387204902,5.35528562815933));
#130114=CARTESIAN_POINT('Ctrl Pts',(17.4450785629847,15.9586484157231,5.37372490594616));
#130115=CARTESIAN_POINT('Ctrl Pts',(17.4467307551215,15.9615015170068,5.39915830271393));
#130116=CARTESIAN_POINT('Ctrl Pts',(17.447184582137,15.9622040380042,5.40609793651254));
#130117=CARTESIAN_POINT('Ctrl Pts',(17.4479656952311,15.9632743754465,5.4179494274931));
#130118=CARTESIAN_POINT('Ctrl Pts',(17.4482909708854,15.9636798529462,5.42285754211342));
#130119=CARTESIAN_POINT('Ctrl Pts',(17.4489949317035,15.9644710497425,5.4334173962096));
#130120=CARTESIAN_POINT('Ctrl Pts',(17.449374196241,15.9648446082729,5.43906949119331));
#130121=CARTESIAN_POINT('Ctrl Pts',(17.4504550506527,15.9657616477409,5.45508192825005));
#130122=CARTESIAN_POINT('Ctrl Pts',(17.4511623302768,15.9661880372743,5.46544787575962));
#130123=CARTESIAN_POINT('Ctrl Pts',(17.4555514392557,15.9677834103671,5.52920830409514));
#130124=CARTESIAN_POINT('Ctrl Pts',(17.4593888343635,15.9646927261921,5.58261315710402));
#130125=CARTESIAN_POINT('Ctrl Pts',(17.4663269727654,15.9511106693,5.67857121028968));
#130126=CARTESIAN_POINT('Ctrl Pts',(17.4694258533113,15.9421095332945,5.72119994474269));
#130127=CARTESIAN_POINT('Ctrl Pts',(17.474351203117,15.9228414270807,5.78933302169659));
#130128=CARTESIAN_POINT('Ctrl Pts',(17.4762196120331,15.9143085705217,5.81526175722135));
#130129=CARTESIAN_POINT('Ctrl Pts',(17.4788253529677,15.9006418498044,5.85154182627666));
#130130=CARTESIAN_POINT('Ctrl Pts',(17.479590859813,15.8964030207263,5.86221408137099));
#130131=CARTESIAN_POINT('Ctrl Pts',(17.480924177662,15.8886270661105,5.88081868121039));
#130132=CARTESIAN_POINT('Ctrl Pts',(17.4814946012313,15.885171388768,5.88878342462708));
#130133=CARTESIAN_POINT('Ctrl Pts',(17.4826839592794,15.8776967484638,5.90539470777142));
#130134=CARTESIAN_POINT('Ctrl Pts',(17.4833020952871,15.8736562043767,5.91403055250293));
#130135=CARTESIAN_POINT('Ctrl Pts',(17.4849506705226,15.8624655915626,5.93705464785389));
#130136=CARTESIAN_POINT('Ctrl Pts',(17.4859731639266,15.8550833538701,5.95132711630148));
#130137=CARTESIAN_POINT('Ctrl Pts',(17.4902776954715,15.8221811756167,6.01123049800135));
#130138=CARTESIAN_POINT('Ctrl Pts',(17.493445343203,15.7933377245919,6.05493651589568));
#130139=CARTESIAN_POINT('Ctrl Pts',(17.4993161377708,15.7332430423628,6.13166533256069));
#130140=CARTESIAN_POINT('Ctrl Pts',(17.5020184159081,15.7029301948823,6.16523314486186));
#130141=CARTESIAN_POINT('Ctrl Pts',(17.5062097999904,15.6540619704933,6.21226516050319));
#130142=CARTESIAN_POINT('Ctrl Pts',(17.5076312694427,15.6371944093681,6.22739386612571));
#130143=CARTESIAN_POINT('Ctrl Pts',(17.5095698968696,15.6140924768739,6.24669374511524));
#130144=CARTESIAN_POINT('Ctrl Pts',(17.5100538705391,15.6083174555036,6.25140600494245));
#130145=CARTESIAN_POINT('Ctrl Pts',(17.5108701863821,15.5985772398406,6.25916787747479));
#130146=CARTESIAN_POINT('Ctrl Pts',(17.5112000395516,15.5946416795074,6.26225445238271));
#130147=CARTESIAN_POINT('Ctrl Pts',(17.5118941843601,15.5863645099912,6.26864294309396));
#130148=CARTESIAN_POINT('Ctrl Pts',(17.5122588203172,15.582018663705,6.27193884739973));
#130149=CARTESIAN_POINT('Ctrl Pts',(17.5132750763057,15.5699062613803,6.28096450903728));
#130150=CARTESIAN_POINT('Ctrl Pts',(17.5139315421207,15.5620816558534,6.28661483981535));
#130151=CARTESIAN_POINT('Ctrl Pts',(17.5189325533948,15.5023774749667,6.32838299748462));
#130152=CARTESIAN_POINT('Ctrl Pts',(17.523501858163,15.4471553896278,6.35944899401651));
#130153=CARTESIAN_POINT('Ctrl Pts',(17.5315640670774,15.3438536024578,6.40489528995907));
#130154=CARTESIAN_POINT('Ctrl Pts',(17.5350680773101,15.2969285134284,6.42136062366709));
#130155=CARTESIAN_POINT('Ctrl Pts',(17.5396775990968,15.2317886964276,6.43871968290166));
#130156=CARTESIAN_POINT('Ctrl Pts',(17.540877289752,15.2145132795484,6.4428174611121));
#130157=CARTESIAN_POINT('Ctrl Pts',(17.5427208828995,15.1874734168911,6.44844960478174));
#130158=CARTESIAN_POINT('Ctrl Pts',(17.5433748886528,15.1777824787674,6.45031380985332));
#130159=CARTESIAN_POINT('Ctrl Pts',(17.5445913458023,15.1595784924271,6.45352741008591));
#130160=CARTESIAN_POINT('Ctrl Pts',(17.5451548372646,15.1510727303776,6.45491196195982));
#130161=CARTESIAN_POINT('Ctrl Pts',(17.5464223225942,15.1317819692474,6.45778786196739));
#130162=CARTESIAN_POINT('Ctrl Pts',(17.5471241504801,15.1209879019671,6.45921114403649));
#130163=CARTESIAN_POINT('Ctrl Pts',(17.549317642329,15.0869263807489,6.4631182810499));
#130164=CARTESIAN_POINT('Ctrl Pts',(17.5507891959852,15.0635906654162,6.46494008961774));
#130165=CARTESIAN_POINT('Ctrl Pts',(17.5571157939137,14.9617290484488,6.46918052216765));
#130166=CARTESIAN_POINT('Ctrl Pts',(17.5617210334738,14.883147257417,6.46287090851723));
#130167=CARTESIAN_POINT('Ctrl Pts',(17.5682810597497,14.7782206204251,6.44140048680865));
#130168=CARTESIAN_POINT('Ctrl Pts',(17.5700571487987,14.7505148751223,6.43443985104588));
#130169=CARTESIAN_POINT('Ctrl Pts',(17.5724043745192,14.7155065406645,6.42397665060791));
#130170=CARTESIAN_POINT('Ctrl Pts',(17.5729220113832,14.7078814923477,6.42159435046795));
#130171=CARTESIAN_POINT('Ctrl Pts',(17.5737788423868,14.6954345783482,6.41753556752393));
#130172=CARTESIAN_POINT('Ctrl Pts',(17.5741149794583,14.6905947169296,6.41591483373247));
#130173=CARTESIAN_POINT('Ctrl Pts',(17.5748038979303,14.6807686339591,6.41253758476846));
#130174=CARTESIAN_POINT('Ctrl Pts',(17.5751568066441,14.6757835911033,6.4107783625274));
#130175=CARTESIAN_POINT('Ctrl Pts',(17.5761066583923,14.6624886528917,6.40596359918072));
#130176=CARTESIAN_POINT('Ctrl Pts',(17.5767075064352,14.6542060932035,6.40283470970285));
#130177=CARTESIAN_POINT('Ctrl Pts',(17.5806300311369,14.6008800162927,6.38184839362959));
#130178=CARTESIAN_POINT('Ctrl Pts',(17.5840914117939,14.5571940102271,6.36074114409454));
#130179=CARTESIAN_POINT('Ctrl Pts',(17.5910606773516,14.4729855407954,6.31194254903599));
#130180=CARTESIAN_POINT('Ctrl Pts',(17.5945580840589,14.4326087417535,6.28425943123633));
#130181=CARTESIAN_POINT('Ctrl Pts',(17.5999988500447,14.3717973896715,6.23540119820824));
#130182=CARTESIAN_POINT('Ctrl Pts',(17.6019971815238,14.3499317188028,6.21614590805787));
#130183=CARTESIAN_POINT('Ctrl Pts',(17.6047458632091,14.3205190879945,6.18778555181103));
#130184=CARTESIAN_POINT('Ctrl Pts',(17.6055288379672,14.3122200995737,6.17948664738948));
#130185=CARTESIAN_POINT('Ctrl Pts',(17.6068820224609,14.2980234200164,6.16476343726271));
#130186=CARTESIAN_POINT('Ctrl Pts',(17.6074550915398,14.2920578707101,6.15840678628417));
#130187=CARTESIAN_POINT('Ctrl Pts',(17.6086402517664,14.279823319005,6.14501157071517));
#130188=CARTESIAN_POINT('Ctrl Pts',(17.6092516726875,14.2735696094926,6.13796024649898));
#130189=CARTESIAN_POINT('Ctrl Pts',(17.6108591205679,14.2572933458136,6.11905834358368));
#130190=CARTESIAN_POINT('Ctrl Pts',(17.6118479114037,14.2474511012525,6.10705568425469));
#130191=CARTESIAN_POINT('Ctrl Pts',(17.617900139376,14.1884068283506,6.03140676819867));
#130192=CARTESIAN_POINT('Ctrl Pts',(17.6226489626738,14.14702138127,5.96206570421902));
#130193=CARTESIAN_POINT('Ctrl Pts',(17.6291128673259,14.1041879164194,5.86443256604884));
#130194=CARTESIAN_POINT('Ctrl Pts',(17.6307133812222,14.0946523389052,5.84005268703975));
#130195=CARTESIAN_POINT('Ctrl Pts',(17.6333773049893,14.0807674273744,5.79981019181811));
#130196=CARTESIAN_POINT('Ctrl Pts',(17.6344179423211,14.0758127903135,5.78417002629577));
#130197=CARTESIAN_POINT('Ctrl Pts',(17.6359095793583,14.0694085299031,5.76201047148965));
#130198=CARTESIAN_POINT('Ctrl Pts',(17.636343790383,14.0676246171125,5.75558973129185));
#130199=CARTESIAN_POINT('Ctrl Pts',(17.6371028621737,14.0646476253452,5.74442869572332));
#130200=CARTESIAN_POINT('Ctrl Pts',(17.6374260274492,14.0634238817683,5.73969694483293));
#130201=CARTESIAN_POINT('Ctrl Pts',(17.6381403118093,14.0608151650847,5.7292849480221));
#130202=CARTESIAN_POINT('Ctrl Pts',(17.6385322127395,14.0594458173628,5.72360135686545));
#130203=CARTESIAN_POINT('Ctrl Pts',(17.6397095731124,14.0555130697071,5.70660252963761));
#130204=CARTESIAN_POINT('Ctrl Pts',(17.6405025074394,14.0531018178137,5.69525360683657));
#130205=CARTESIAN_POINT('Ctrl Pts',(17.6455439360664,14.0392124345504,5.62355697933958));
#130206=CARTESIAN_POINT('Ctrl Pts',(17.6499852011548,14.0333046373484,5.56227671970015));
#130207=CARTESIAN_POINT('Ctrl Pts',(17.6543706060827,14.033250377214,5.50085401588055));
#130208=CARTESIAN_POINT('Origin',(16.125,15.,5.5));
#130209=CARTESIAN_POINT('',(18.1122363826056,14.0332503335345,5.49919695023161));
#130210=CARTESIAN_POINT('',(18.0542644868187,14.0332501467026,5.49946741256401));
#130211=CARTESIAN_POINT('',(16.125,14.03325,5.5));
#130212=CARTESIAN_POINT('Ctrl Pts',(18.1116014980396,14.0336172045748,5.49916088635316));
#130213=CARTESIAN_POINT('Ctrl Pts',(18.1088658687755,14.0336893782224,5.53997545647357));
#130214=CARTESIAN_POINT('Ctrl Pts',(18.1061935292842,14.0363249574671,5.58078098174216));
#130215=CARTESIAN_POINT('Ctrl Pts',(18.1035215018489,14.0413803580352,5.6212698696751));
#130216=CARTESIAN_POINT('Ctrl Pts',(18.1008461429723,14.0464420615965,5.66180923851073));
#130217=CARTESIAN_POINT('Ctrl Pts',(18.0982503860392,14.0540669973466,5.70201867661375));
#130218=CARTESIAN_POINT('Ctrl Pts',(18.0957117391143,14.0641887759179,5.74155657413911));
#130219=CARTESIAN_POINT('Ctrl Pts',(18.0931714984445,14.0743169088717,5.78111929328233));
#130220=CARTESIAN_POINT('Ctrl Pts',(18.0906756150031,14.0869242328612,5.82001513743482));
#130221=CARTESIAN_POINT('Ctrl Pts',(18.0881817228849,14.1019116579752,5.85791351849397));
#130222=CARTESIAN_POINT('Ctrl Pts',(18.0856819955985,14.1169341504223,5.89590057356776));
#130223=CARTESIAN_POINT('Ctrl Pts',(18.0831837022177,14.1343484255732,5.93288515096058));
#130224=CARTESIAN_POINT('Ctrl Pts',(18.0806279241079,14.1540096713151,5.96854122302932));
#130225=CARTESIAN_POINT('Ctrl Pts',(18.0787455098085,14.1684908228622,5.99480308812046));
#130226=CARTESIAN_POINT('Ctrl Pts',(18.0768314636631,14.184190028169,6.02034430119852));
#130227=CARTESIAN_POINT('Ctrl Pts',(18.0748600895335,14.2010311060696,6.04503941695895));
#130228=CARTESIAN_POINT('Ctrl Pts',(18.0748590319094,14.2010401411531,6.04505266566168));
#130229=CARTESIAN_POINT('Ctrl Pts',(18.0748579742688,14.2010491765653,6.04506591412149));
#130230=CARTESIAN_POINT('Ctrl Pts',(18.0748569166117,14.2010582123061,6.04507916233835));
#130231=CARTESIAN_POINT('Ctrl Pts',(18.0724065240528,14.2219923238445,6.07577278846326));
#130232=CARTESIAN_POINT('Ctrl Pts',(18.0698604177907,14.244781920386,6.1052840748042));
#130233=CARTESIAN_POINT('Ctrl Pts',(18.0672739372776,14.2692511598286,6.13340288117519));
#130234=CARTESIAN_POINT('Ctrl Pts',(18.0670480255632,14.271388383675,6.1358588701997));
#130235=CARTESIAN_POINT('Ctrl Pts',(18.0668218058398,14.2735383898142,6.13830422664061));
#130236=CARTESIAN_POINT('Ctrl Pts',(18.0665953149815,14.2757010429266,6.14073880552423));
#130237=CARTESIAN_POINT('Ctrl Pts',(18.0637799385348,14.3025837289705,6.17100164305548));
#130238=CARTESIAN_POINT('Ctrl Pts',(18.0609233217478,14.3314258555293,6.1996013612969));
#130239=CARTESIAN_POINT('Ctrl Pts',(18.0580817228216,14.361975897788,6.22630679014228));
#130240=CARTESIAN_POINT('Ctrl Pts',(18.0552430158035,14.39249484913,6.25298504075157));
#130241=CARTESIAN_POINT('Ctrl Pts',(18.0524196050428,14.4247180905576,6.27777315290609));
#130242=CARTESIAN_POINT('Ctrl Pts',(18.0496459487321,14.4583756431876,6.30047312464432));
#130243=CARTESIAN_POINT('Ctrl Pts',(18.046873781404,14.4920151274242,6.32316091035027));
#130244=CARTESIAN_POINT('Ctrl Pts',(18.0441514015046,14.5270873595618,6.34376286150736));
#130245=CARTESIAN_POINT('Ctrl Pts',(18.041488724339,14.5633047650662,6.36211106595343));
#130246=CARTESIAN_POINT('Ctrl Pts',(18.0388241827983,14.5995475295694,6.38047211759518));
#130247=CARTESIAN_POINT('Ctrl Pts',(18.0362193552178,14.6369370964161,6.39657613249006));
#130248=CARTESIAN_POINT('Ctrl Pts',(18.0336595581491,14.6751671758804,6.41028521668761));
#130249=CARTESIAN_POINT('Ctrl Pts',(18.0310989935289,14.7134087185792,6.4239984115344));
#130250=CARTESIAN_POINT('Ctrl Pts',(18.0285832355814,14.7524913169899,6.4353149186364));
#130251=CARTESIAN_POINT('Ctrl Pts',(18.026075344813,14.792089783369,6.44413046985751));
#130252=CARTESIAN_POINT('Ctrl Pts',(18.0235624718859,14.8317669157916,6.4529635339926));
#130253=CARTESIAN_POINT('Ctrl Pts',(18.0210570003867,14.8719619543096,6.45928512125692));
#130254=CARTESIAN_POINT('Ctrl Pts',(18.0185049586738,14.9123287521555,6.46303089420097));
#130255=CARTESIAN_POINT('Ctrl Pts',(18.0163245790278,14.9468168030184,6.4662311581483));
#130256=CARTESIAN_POINT('Ctrl Pts',(18.0141096076922,14.9814297928223,6.46755158034023));
#130257=CARTESIAN_POINT('Ctrl Pts',(18.0118220857894,15.0159418679715,6.46698121831073));
#130258=CARTESIAN_POINT('Ctrl Pts',(18.0118211641835,15.0159557723331,6.46698098852101));
#130259=CARTESIAN_POINT('Ctrl Pts',(18.0118202425658,15.0159696766789,6.46698075842474));
#130260=CARTESIAN_POINT('Ctrl Pts',(18.0118193209363,15.0159835810087,6.46698052802191));
#130261=CARTESIAN_POINT('Ctrl Pts',(18.0093419444725,15.0533589702906,6.46636119609794));
#130262=CARTESIAN_POINT('Ctrl Pts',(18.0067725382995,15.0907651161667,6.46351754675653));
#130263=CARTESIAN_POINT('Ctrl Pts',(18.0041666197859,15.1279257633553,6.45848168359273));
#130264=CARTESIAN_POINT('Ctrl Pts',(18.0039548448629,15.1309456940077,6.45807243459736));
#130265=CARTESIAN_POINT('Ctrl Pts',(18.0037428288012,15.1339639811941,6.45764872549634));
#130266=CARTESIAN_POINT('Ctrl Pts',(18.0035306013974,15.1369804652223,6.45721058335147));
#130267=CARTESIAN_POINT('Ctrl Pts',(18.0007110077786,15.1770566239422,6.45138954999749));
#130268=CARTESIAN_POINT('Ctrl Pts',(17.9978547419002,15.2168191808931,6.44301782903751));
#130269=CARTESIAN_POINT('Ctrl Pts',(17.9950167387749,15.2559371188899,6.43217817789313));
#130270=CARTESIAN_POINT('Ctrl Pts',(17.9921815149166,15.2950167485457,6.4213491420591));
#130271=CARTESIAN_POINT('Ctrl Pts',(17.9893648137686,15.33345317573,6.40805728346844));
#130272=CARTESIAN_POINT('Ctrl Pts',(17.986599669708,15.3709325477281,6.39241895397032));
#130273=CARTESIAN_POINT('Ctrl Pts',(17.98383590699,15.4083931967048,6.37678843668359));
#130274=CARTESIAN_POINT('Ctrl Pts',(17.9811237283587,15.4448977780505,6.35881384072439));
#130275=CARTESIAN_POINT('Ctrl Pts',(17.978471672925,15.4801476626227,6.3386428554526));
#130276=CARTESIAN_POINT('Ctrl Pts',(17.9758176195666,15.5154241026782,6.31845667437889));
#130277=CARTESIAN_POINT('Ctrl Pts',(17.9732237007733,15.5494438505318,6.29607069449121));
#130278=CARTESIAN_POINT('Ctrl Pts',(17.9706740015162,15.581922932576,6.27166493845294));
#130279=CARTESIAN_POINT('Ctrl Pts',(17.9681234609455,15.6144127316072,6.2472511293493));
#130280=CARTESIAN_POINT('Ctrl Pts',(17.9656169089056,15.6453605939784,6.22081599670884));
#130281=CARTESIAN_POINT('Ctrl Pts',(17.9631164361356,15.6745002420025,6.19257410705889));
#130282=CARTESIAN_POINT('Ctrl Pts',(17.9606108920038,15.7036989899298,6.16427493830445));
#130283=CARTESIAN_POINT('Ctrl Pts',(17.9581109411544,15.7310816816463,6.13416136866688));
#130284=CARTESIAN_POINT('Ctrl Pts',(17.9555620680015,15.7564040080915,6.10248778276124));
#130285=CARTESIAN_POINT('Ctrl Pts',(17.9533945604248,15.7779375765114,6.07555323823291));
#130286=CARTESIAN_POINT('Ctrl Pts',(17.9511910843983,15.7979812735429,6.0474911579514));
#130287=CARTESIAN_POINT('Ctrl Pts',(17.9489142448659,15.8164036574049,6.01848213947661));
#130288=CARTESIAN_POINT('Ctrl Pts',(17.9489132820208,15.8164114479853,6.0184698719496));
#130289=CARTESIAN_POINT('Ctrl Pts',(17.9489123191626,15.8164192382764,6.01845760425303));
#130290=CARTESIAN_POINT('Ctrl Pts',(17.9489113562913,15.8164270282781,6.01844533638694));
#130291=CARTESIAN_POINT('Ctrl Pts',(17.9464450745537,15.8363802024246,5.98702263882757));
#130292=CARTESIAN_POINT('Ctrl Pts',(17.9438855878723,15.8545098229505,5.95435673608956));
#130293=CARTESIAN_POINT('Ctrl Pts',(17.9412885873555,15.870690772421,5.92069341892059));
#130294=CARTESIAN_POINT('Ctrl Pts',(17.9410745755695,15.8720242006868,5.91791931603396));
#130295=CARTESIAN_POINT('Ctrl Pts',(17.9408603090284,15.8733443984736,5.91513846888866));
#130296=CARTESIAN_POINT('Ctrl Pts',(17.9406458188985,15.8746512977548,5.91235103064029));
#130297=CARTESIAN_POINT('Ctrl Pts',(17.9378328046746,15.891791136628,5.87579408770548));
#130298=CARTESIAN_POINT('Ctrl Pts',(17.9349819647332,15.9066436051444,5.83809783774839));
#130299=CARTESIAN_POINT('Ctrl Pts',(17.9321487179927,15.9190952188582,5.79958219943527));
#130300=CARTESIAN_POINT('Ctrl Pts',(17.9293183943032,15.9315339862841,5.76110629757619));
#130301=CARTESIAN_POINT('Ctrl Pts',(17.9265059236572,15.9415771629589,5.72181272334531));
#130302=CARTESIAN_POINT('Ctrl Pts',(17.9237448700913,15.9491487441809,5.68202569232012));
#130303=CARTESIAN_POINT('Ctrl Pts',(17.920985318238,15.9567162072869,5.64226030110872));
#130304=CARTESIAN_POINT('Ctrl Pts',(17.9182772075239,15.9618148199288,5.60200199529049));
#130305=CARTESIAN_POINT('Ctrl Pts',(17.9156296451895,15.9644031220143,5.56157960489602));
#130306=CARTESIAN_POINT('Ctrl Pts',(17.9129801843571,15.966993280104,5.52112822865665));
#130307=CARTESIAN_POINT('Ctrl Pts',(17.9103912828771,15.9670693890494,5.4805125711672));
#130308=CARTESIAN_POINT('Ctrl Pts',(17.9078476039144,15.9646250281175,5.44006701231661));
#130309=CARTESIAN_POINT('Ctrl Pts',(17.9053031489214,15.9621799214554,5.39960911425793));
#130310=CARTESIAN_POINT('Ctrl Pts',(17.9028036904404,15.9572124955404,5.35932151722426));
#130311=CARTESIAN_POINT('Ctrl Pts',(17.9003118363484,15.949754806761,5.31954275906698));
#130312=CARTESIAN_POINT('Ctrl Pts',(17.8978149108835,15.9422819402388,5.27968304395688));
#130313=CARTESIAN_POINT('Ctrl Pts',(17.8953251213505,15.932308143317,5.24033448709196));
#130314=CARTESIAN_POINT('Ctrl Pts',(17.8927882747748,15.9199105622351,5.20183911645171));
#130315=CARTESIAN_POINT('Ctrl Pts',(17.8905719613089,15.9090794279603,5.16820767451102));
#130316=CARTESIAN_POINT('Ctrl Pts',(17.8883191088923,15.8963987108305,5.13522773161351));
#130317=CARTESIAN_POINT('Ctrl Pts',(17.8859891485143,15.8819531603237,5.10312470204307));
#130318=CARTESIAN_POINT('Ctrl Pts',(17.8859881712975,15.881947101665,5.10311123759953));
#130319=CARTESIAN_POINT('Ctrl Pts',(17.8859871940672,15.881941042696,5.10309777330959));
#130320=CARTESIAN_POINT('Ctrl Pts',(17.8859862168232,15.8819349834168,5.10308430917325));
#130321=CARTESIAN_POINT('Ctrl Pts',(17.8835206934754,15.8666478131493,5.06911516255648));
#130322=CARTESIAN_POINT('Ctrl Pts',(17.8809616614798,15.8493173518981,5.0359889359937));
#130323=CARTESIAN_POINT('Ctrl Pts',(17.8783646711916,15.8300807044715,5.00394517438977));
#130324=CARTESIAN_POINT('Ctrl Pts',(17.8781482371223,15.8284775156175,5.00127463620797));
#130325=CARTESIAN_POINT('Ctrl Pts',(17.8779315394092,15.8268611136928,4.99861163024406));
#130326=CARTESIAN_POINT('Ctrl Pts',(17.8777146102079,15.8252315927147,4.99595630226268));
#130327=CARTESIAN_POINT('Ctrl Pts',(17.8748989717401,15.8040811808644,4.96149140051695));
#130328=CARTESIAN_POINT('Ctrl Pts',(17.872044972252,15.7807158849934,4.92831692112204));
#130329=CARTESIAN_POINT('Ctrl Pts',(17.8692081040133,15.7553417304167,4.89670397818174));
#130330=CARTESIAN_POINT('Ctrl Pts',(17.8663741108469,15.7299932917073,4.86512307391465));
#130331=CARTESIAN_POINT('Ctrl Pts',(17.8635575134749,15.7026402592037,4.83510028959648));
#130332=CARTESIAN_POINT('Ctrl Pts',(17.8607919502432,15.6735127620098,4.80687764311701));
#130333=CARTESIAN_POINT('Ctrl Pts',(17.8580278519906,15.6444006942861,4.7786699467885));
#130334=CARTESIAN_POINT('Ctrl Pts',(17.8553148149984,15.6135160758515,4.75226043225306));
#130335=CARTESIAN_POINT('Ctrl Pts',(17.8526619882167,15.5811117946709,4.72786472603724));
#130336=CARTESIAN_POINT('Ctrl Pts',(17.8500072446075,15.54868409944,4.7034513924503));
#130337=CARTESIAN_POINT('Ctrl Pts',(17.8474127222728,15.5147344984511,4.68105491162952));
#130338=CARTESIAN_POINT('Ctrl Pts',(17.8448630843471,15.4795397257855,4.66086466929473));
#130339=CARTESIAN_POINT('Ctrl Pts',(17.8423126543957,15.4443340201285,4.64066815501296));
#130340=CARTESIAN_POINT('Ctrl Pts',(17.8398068819401,15.4078822766436,4.62267956406072));
#130341=CARTESIAN_POINT('Ctrl Pts',(17.8373083419198,15.3704858537613,4.60705842571141));
#130342=CARTESIAN_POINT('Ctrl Pts',(17.8348047545454,15.3330138855656,4.59140573076653));
#130343=CARTESIAN_POINT('Ctrl Pts',(17.8323079267811,15.294593333726,4.57813063592173));
#130344=CARTESIAN_POINT('Ctrl Pts',(17.8297636306789,15.2555532947734,4.56735689974287));
#130345=CARTESIAN_POINT('Ctrl Pts',(17.8275707465065,15.2219053701346,4.55807120554918));
#130346=CARTESIAN_POINT('Ctrl Pts',(17.8253419942227,15.1877977496348,4.55064338818002));
#130347=CARTESIAN_POINT('Ctrl Pts',(17.8230384246179,15.1534565324485,4.54512473143032));
#130348=CARTESIAN_POINT('Ctrl Pts',(17.8230374665369,15.1534422495422,4.54512243615765));
#130349=CARTESIAN_POINT('Ctrl Pts',(17.8230365084429,15.1534279665951,4.54512014121477));
#130350=CARTESIAN_POINT('Ctrl Pts',(17.823035550336,15.1534136836072,4.54511784660166));
#130351=CARTESIAN_POINT('Ctrl Pts',(17.8205667211352,15.116609588965,4.53920513712671));
#130352=CARTESIAN_POINT('Ctrl Pts',(17.8180048593831,15.0793856105227,4.53546526148694));
#130353=CARTESIAN_POINT('Ctrl Pts',(17.815405549373,15.0420177039287,4.53391545663618));
#130354=CARTESIAN_POINT('Ctrl Pts',(17.8151910551426,15.0389341162328,4.53378756723577));
#130355=CARTESIAN_POINT('Ctrl Pts',(17.8149763059084,15.0358495741346,4.53367457686729));
#130356=CARTESIAN_POINT('Ctrl Pts',(17.8147613329042,15.0327642462848,4.53357648715621));
#130357=CARTESIAN_POINT('Ctrl Pts',(17.8119454617059,14.9923504005498,4.53229163749196));
#130358=CARTESIAN_POINT('Ctrl Pts',(17.8090918310268,14.9517965738512,4.53356564647681));
#130359=CARTESIAN_POINT('Ctrl Pts',(17.8062557657168,14.9114423675895,4.53737558507123));
#130360=CARTESIAN_POINT('Ctrl Pts',(17.803422565318,14.8711289259787,4.54118167497597));
#130361=CARTESIAN_POINT('Ctrl Pts',(17.8006071922017,14.8310145990644,4.54751827374003));
#130362=CARTESIAN_POINT('Ctrl Pts',(17.7978431046286,14.7914279990699,4.55632633642105));
#130363=CARTESIAN_POINT('Ctrl Pts',(17.7950804715473,14.7518622299594,4.56512976420715));
#130364=CARTESIAN_POINT('Ctrl Pts',(17.7923691501625,14.7128236115966,4.57640200068218));
#130365=CARTESIAN_POINT('Ctrl Pts',(17.7897181174785,14.6746312654799,4.5900504708212));
#130366=CARTESIAN_POINT('Ctrl Pts',(17.7870651525617,14.6364110824744,4.60370888878966));
#130367=CARTESIAN_POINT('Ctrl Pts',(17.7844724874549,14.5990384927188,4.61974711801268));
#130368=CARTESIAN_POINT('Ctrl Pts',(17.7819246340463,14.5628238351016,4.6380382139017));
#130369=CARTESIAN_POINT('Ctrl Pts',(17.7793759806,14.5265978059157,4.65633505327878));
#130370=CARTESIAN_POINT('Ctrl Pts',(17.7768719111538,14.491530648528,4.67688642475008));
#130371=CARTESIAN_POINT('Ctrl Pts',(17.7743748836567,14.4579213097127,4.6995283670398));
#130372=CARTESIAN_POINT('Ctrl Pts',(17.7718727953186,14.4242438532984,4.72221619879956));
#130373=CARTESIAN_POINT('Ctrl Pts',(17.7693772739804,14.3920305644859,4.74700346924696));
#130374=CARTESIAN_POINT('Ctrl Pts',(17.7668340263732,14.3615657555603,4.77368333767468));
#130375=CARTESIAN_POINT('Ctrl Pts',(17.764640735305,14.3352929722413,4.79669199674406));
#130376=CARTESIAN_POINT('Ctrl Pts',(17.7624113416266,14.3103206576772,4.82110770405281));
#130377=CARTESIAN_POINT('Ctrl Pts',(17.7601068293578,14.2868162319021,4.84676948192799));
#130378=CARTESIAN_POINT('Ctrl Pts',(17.76010586425,14.2868063884718,4.84678022883692));
#130379=CARTESIAN_POINT('Ctrl Pts',(17.7601048991289,14.2867965452982,4.84679097596449));
#130380=CARTESIAN_POINT('Ctrl Pts',(17.7601039339947,14.2867867023815,4.84680172331068));
#130381=CARTESIAN_POINT('Ctrl Pts',(17.7576574878544,14.2618366328468,4.87404436308077));
#130382=CARTESIAN_POINT('Ctrl Pts',(17.7551188439162,14.2384353630941,4.90281317730129));
#130383=CARTESIAN_POINT('Ctrl Pts',(17.7525424071133,14.2167495663272,4.93289180029561));
#130384=CARTESIAN_POINT('Ctrl Pts',(17.7523372409479,14.2150226884312,4.93528701361191));
#130385=CARTESIAN_POINT('Ctrl Pts',(17.7521318351298,14.2133066900175,4.93769050538471));
#130386=CARTESIAN_POINT('Ctrl Pts',(17.7519262171315,14.2116016555307,4.94010215220752));
#130387=CARTESIAN_POINT('Ctrl Pts',(17.7491428756289,14.1885215103621,4.97274733281705));
#130388=CARTESIAN_POINT('Ctrl Pts',(17.7463212722676,14.1674496164549,5.00689228645096));
#130389=CARTESIAN_POINT('Ctrl Pts',(17.7435155809644,14.1485526504879,5.04224773268058));
#130390=CARTESIAN_POINT('Ctrl Pts',(17.740712090522,14.1296705078165,5.07757544513362));
#130391=CARTESIAN_POINT('Ctrl Pts',(17.7379247838215,14.1129596062418,5.11411163420977));
#130392=CARTESIAN_POINT('Ctrl Pts',(17.7351870199387,14.0985500750757,5.15155536242206));
#130393=CARTESIAN_POINT('Ctrl Pts',(17.7324507313258,14.0841483086208,5.18897891372959));
#130394=CARTESIAN_POINT('Ctrl Pts',(17.7297640154077,14.0720453839529,5.22730897157081));
#130395=CARTESIAN_POINT('Ctrl Pts',(17.7271367399864,14.0623374688623,5.26623394088526));
#130396=CARTESIAN_POINT('Ctrl Pts',(17.7245073209853,14.0526216331362,5.30519066887156));
#130397=CARTESIAN_POINT('Ctrl Pts',(17.7219373687409,14.0453048495426,5.34474322479761));
#130398=CARTESIAN_POINT('Ctrl Pts',(17.7194132115611,14.0404490318487,5.38456887519119));
#130399=CARTESIAN_POINT('Ctrl Pts',(17.716966696999,14.0357425782276,5.423169495792));
#130400=CARTESIAN_POINT('Ctrl Pts',(17.7145628866741,14.0333481032163,5.46202654932006));
#130401=CARTESIAN_POINT('Ctrl Pts',(17.7121702600549,14.0332882759794,5.5008377736384));
#130402=CARTESIAN_POINT('Ctrl Pts',(17.6543706060827,14.033250377214,5.50085401588055));
#130403=CARTESIAN_POINT('Ctrl Pts',(17.6580115786231,14.0332053278599,5.44985795470837));
#130404=CARTESIAN_POINT('Ctrl Pts',(17.6616032851967,14.0371953487123,5.39893238786557));
#130405=CARTESIAN_POINT('Ctrl Pts',(17.6661790796772,14.0477171410936,5.33259644850869));
#130406=CARTESIAN_POINT('Ctrl Pts',(17.6672679536018,14.0506478613156,5.31670471445997));
#130407=CARTESIAN_POINT('Ctrl Pts',(17.6689809790593,14.0559428155606,5.29154659700883));
#130408=CARTESIAN_POINT('Ctrl Pts',(17.669613021814,14.0580484002325,5.28222951675262));
#130409=CARTESIAN_POINT('Ctrl Pts',(17.6708108916401,14.0623293641528,5.26451198174632));
#130410=CARTESIAN_POINT('Ctrl Pts',(17.6713774194988,14.0644804217476,5.25610667322801));
#130411=CARTESIAN_POINT('Ctrl Pts',(17.6726829194021,14.0697299905992,5.23668615780269));
#130412=CARTESIAN_POINT('Ctrl Pts',(17.6734191856156,14.0729115258471,5.2256946070088));
#130413=CARTESIAN_POINT('Ctrl Pts',(17.6758736512411,14.0842552382558,5.18895925274585));
#130414=CARTESIAN_POINT('Ctrl Pts',(17.6775638706208,14.0933009978729,5.16350048160501));
#130415=CARTESIAN_POINT('Ctrl Pts',(17.6818686155903,14.119393435123,5.09879415316991));
#130416=CARTESIAN_POINT('Ctrl Pts',(17.6844408186437,14.1379994756611,5.06023935469139));
#130417=CARTESIAN_POINT('Ctrl Pts',(17.690296652061,14.1859945388744,4.97562147997777));
#130418=CARTESIAN_POINT('Ctrl Pts',(17.6935702910173,14.2168514121737,4.93056640225068));
#130419=CARTESIAN_POINT('Ctrl Pts',(17.697698802244,14.2579118665586,4.88030748678154));
#130420=CARTESIAN_POINT('Ctrl Pts',(17.6983669334397,14.2646173592589,4.87236478751426));
#130421=CARTESIAN_POINT('Ctrl Pts',(17.6994124619425,14.2751752687108,4.86026036363062));
#130422=CARTESIAN_POINT('Ctrl Pts',(17.6997839218796,14.2789386394842,4.85602158116335));
#130423=CARTESIAN_POINT('Ctrl Pts',(17.7004831499036,14.2860400500654,4.84816336917266));
#130424=CARTESIAN_POINT('Ctrl Pts',(17.70081027332,14.2893687961256,4.84453597262604));
#130425=CARTESIAN_POINT('Ctrl Pts',(17.7016050430806,14.297473697085,4.83583821566285));
#130426=CARTESIAN_POINT('Ctrl Pts',(17.7020746228493,14.3022771489473,4.83079382977349));
#130427=CARTESIAN_POINT('Ctrl Pts',(17.7038074811637,14.3200713914113,4.81250689341262));
#130428=CARTESIAN_POINT('Ctrl Pts',(17.7050913746803,14.333387349295,4.79958786553665));
#130429=CARTESIAN_POINT('Ctrl Pts',(17.7086161400394,14.3704922149092,4.76560594466785));
#130430=CARTESIAN_POINT('Ctrl Pts',(17.7108844139193,14.3949609245833,4.7453198049455));
#130431=CARTESIAN_POINT('Ctrl Pts',(17.7183690740793,14.4786318883733,4.68263961848548));
#130432=CARTESIAN_POINT('Ctrl Pts',(17.7235653945706,14.5416333941749,4.64571302630296));
#130433=CARTESIAN_POINT('Ctrl Pts',(17.729537574548,14.6219856202463,4.61009080760766));
#130434=CARTESIAN_POINT('Ctrl Pts',(17.7305524166336,14.6359217801681,4.60429897020812));
#130435=CARTESIAN_POINT('Ctrl Pts',(17.7321778766288,14.6586924988455,4.59545484336193));
#130436=CARTESIAN_POINT('Ctrl Pts',(17.7327950267675,14.6674452645428,4.59220040267388));
#130437=CARTESIAN_POINT('Ctrl Pts',(17.7339824999806,14.6844890955603,4.58614279051585));
#130438=CARTESIAN_POINT('Ctrl Pts',(17.7345532700782,14.6927737388548,4.58332439605747));
#130439=CARTESIAN_POINT('Ctrl Pts',(17.7358957042201,14.7124696402621,4.57692097069132));
#130440=CARTESIAN_POINT('Ctrl Pts',(17.7366641504585,14.7239115617762,4.5734344079247));
#130441=CARTESIAN_POINT('Ctrl Pts',(17.7393935801319,14.7651088767559,4.56171177196163));
#130442=CARTESIAN_POINT('Ctrl Pts',(17.7413167216283,14.7951915373875,4.55468925577576));
#130443=CARTESIAN_POINT('Ctrl Pts',(17.7463446052182,14.8757702247164,4.53990712662917));
#130444=CARTESIAN_POINT('Ctrl Pts',(17.7493892273225,14.9266299750044,4.53468742770296));
#130445=CARTESIAN_POINT('Ctrl Pts',(17.7549337463581,15.0183906809525,4.53256689340583));
#130446=CARTESIAN_POINT('Ctrl Pts',(17.7574155375176,15.0591311931225,4.53420092219245));
#130447=CARTESIAN_POINT('Ctrl Pts',(17.7606764942316,15.1101487158995,4.5394874352612));
#130448=CARTESIAN_POINT('Ctrl Pts',(17.7613551030031,15.120635806784,4.54074815227532));
#130449=CARTESIAN_POINT('Ctrl Pts',(17.7624136300875,15.1367517353785,4.54295398741473));
#130450=CARTESIAN_POINT('Ctrl Pts',(17.7627873817123,15.1423967156238,4.54377759973275));
#130451=CARTESIAN_POINT('Ctrl Pts',(17.7634884725191,15.1528934855495,4.54540410270926));
#130452=CARTESIAN_POINT('Ctrl Pts',(17.7638151279656,15.1577469403971,4.54619412687196));
#130453=CARTESIAN_POINT('Ctrl Pts',(17.7646053537182,15.16940183953,4.54818264645704));
#130454=CARTESIAN_POINT('Ctrl Pts',(17.765070795136,15.1761967571458,4.54941704529846));
#130455=CARTESIAN_POINT('Ctrl Pts',(17.7667677982586,15.2007408557987,4.55414804159278));
#130456=CARTESIAN_POINT('Ctrl Pts',(17.7680189063515,15.2184032547852,4.55806967188822));
#130457=CARTESIAN_POINT('Ctrl Pts',(17.7714198517377,15.2655213676021,4.56992785198217));
#130458=CARTESIAN_POINT('Ctrl Pts',(17.7735950741786,15.2947285186452,4.57876674661313));
#130459=CARTESIAN_POINT('Ctrl Pts',(17.7811626291963,15.394380518069,4.61414889493831));
#130460=CARTESIAN_POINT('Ctrl Pts',(17.7865415504299,15.4621248191605,4.64752556447274));
#130461=CARTESIAN_POINT('Ctrl Pts',(17.7926525082424,15.5376947484774,4.69644085618685));
#130462=CARTESIAN_POINT('Ctrl Pts',(17.793643411322,15.5498875094492,4.70473481959738));
#130463=CARTESIAN_POINT('Ctrl Pts',(17.795240653009,15.5694301527178,4.71869288783753));
#130464=CARTESIAN_POINT('Ctrl Pts',(17.7958531007874,15.5768962618671,4.7241893172971));
#130465=CARTESIAN_POINT('Ctrl Pts',(17.7970380765168,15.5912824493956,4.73510273395075));
#130466=CARTESIAN_POINT('Ctrl Pts',(17.797610961855,15.5982099825225,4.74050833597131));
#130467=CARTESIAN_POINT('Ctrl Pts',(17.7989688216112,15.6145554668192,4.75362524662387));
#130468=CARTESIAN_POINT('Ctrl Pts',(17.7997503683703,15.6239035044796,4.7614215462063));
#130469=CARTESIAN_POINT('Ctrl Pts',(17.8026020408453,15.6577473610206,4.79074867648136));
#130470=CARTESIAN_POINT('Ctrl Pts',(17.8046294022459,15.6812976802206,4.81333937561477));
#130471=CARTESIAN_POINT('Ctrl Pts',(17.8103987448658,15.7458968658224,4.8819087227117));
#130472=CARTESIAN_POINT('Ctrl Pts',(17.8140431190923,15.783748718739,4.93066998390617));
#130473=CARTESIAN_POINT('Ctrl Pts',(17.8197536055054,15.8338638310769,5.00979080711079));
#130474=CARTESIAN_POINT('Ctrl Pts',(17.8217374707134,15.8496631023992,5.03771638027573));
#130475=CARTESIAN_POINT('Ctrl Pts',(17.8243325212409,15.8678155763205,5.07388689022333));
#130476=CARTESIAN_POINT('Ctrl Pts',(17.8248765231526,15.8714885644254,5.08145020911602));
#130477=CARTESIAN_POINT('Ctrl Pts',(17.8257656235734,15.8772691371133,5.09375945900256));
#130478=CARTESIAN_POINT('Ctrl Pts',(17.8261072007205,15.8794380314579,5.09847632467666));
#130479=CARTESIAN_POINT('Ctrl Pts',(17.8267943576951,15.8836953580494,5.1079350533619));
#130480=CARTESIAN_POINT('Ctrl Pts',(17.8271399195935,15.8857838666308,5.11267668981902));
#130481=CARTESIAN_POINT('Ctrl Pts',(17.8280496370066,15.8911483488441,5.12512625262244));
#130482=CARTESIAN_POINT('Ctrl Pts',(17.8286171765238,15.8943623758075,5.13286019648734));
#130483=CARTESIAN_POINT('Ctrl Pts',(17.8315568780144,15.9103550484467,5.17280012892302));
#130484=CARTESIAN_POINT('Ctrl Pts',(17.8340017071513,15.921494975487,5.20563184071929));
#130485=CARTESIAN_POINT('Ctrl Pts',(17.8418093038422,15.9510672660986,5.3110951678131));
#130486=CARTESIAN_POINT('Ctrl Pts',(17.8472138362182,15.9628425058149,5.38532108675831));
#130487=CARTESIAN_POINT('Ctrl Pts',(17.8538390623054,15.9668062015164,5.48143769786327));
#130488=CARTESIAN_POINT('Ctrl Pts',(17.855285833799,15.9669805777599,5.50273319879022));
#130489=CARTESIAN_POINT('Ctrl Pts',(17.8574160014287,15.9661901780335,5.53453708969768));
#130490=CARTESIAN_POINT('Ctrl Pts',(17.8581152511595,15.9657570567328,5.54505100174174));
#130491=CARTESIAN_POINT('Ctrl Pts',(17.8593757071274,15.9646588094596,5.56413037953826));
#130492=CARTESIAN_POINT('Ctrl Pts',(17.8599386086797,15.9640510076316,5.57269791483708));
#130493=CARTESIAN_POINT('Ctrl Pts',(17.8611577557631,15.962477800191,5.5913489456024));
#130494=CARTESIAN_POINT('Ctrl Pts',(17.8618125682031,15.9614679260809,5.6014277344616));
#130495=CARTESIAN_POINT('Ctrl Pts',(17.863691000132,15.9580931089762,5.6304963702171));
#130496=CARTESIAN_POINT('Ctrl Pts',(17.8649021777186,15.955322469334,5.64943481144132));
#130497=CARTESIAN_POINT('Ctrl Pts',(17.8687284953191,15.9446744232055,5.70967295325515));
#130498=CARTESIAN_POINT('Ctrl Pts',(17.8712831119922,15.9346652906083,5.7505468834835));
#130499=CARTESIAN_POINT('Ctrl Pts',(17.8771298191637,15.9055236214757,5.84299519021532));
#130500=CARTESIAN_POINT('Ctrl Pts',(17.8803963691972,15.8845932497051,5.89384340318341));
#130501=CARTESIAN_POINT('Ctrl Pts',(17.8849663129955,15.8509738216589,5.95912194267895));
#130502=CARTESIAN_POINT('Ctrl Pts',(17.8861369572696,15.842011792829,5.97535822906351));
#130503=CARTESIAN_POINT('Ctrl Pts',(17.8877936426604,15.8289576550394,5.99747947368217));
#130504=CARTESIAN_POINT('Ctrl Pts',(17.8882582010315,15.8252581573867,6.00359267958698));
#130505=CARTESIAN_POINT('Ctrl Pts',(17.8890515430426,15.8188829220634,6.01386846878965));
#130506=CARTESIAN_POINT('Ctrl Pts',(17.8893781393811,15.8162423926746,6.01805250572704));
#130507=CARTESIAN_POINT('Ctrl Pts',(17.8900774441743,15.8105571822718,6.02690959357493));
#130508=CARTESIAN_POINT('Ctrl Pts',(17.8904506344504,15.8075041429159,6.03157663696451));
#130509=CARTESIAN_POINT('Ctrl Pts',(17.891516327873,15.7987273185627,6.04474327616203));
#130510=CARTESIAN_POINT('Ctrl Pts',(17.8922144326168,15.7929087105019,6.05317838262196));
#130511=CARTESIAN_POINT('Ctrl Pts',(17.8954404229621,15.7656607638038,6.09136582416341));
#130512=CARTESIAN_POINT('Ctrl Pts',(17.8980414806253,15.7426851363144,6.11997440359137));
#130513=CARTESIAN_POINT('Ctrl Pts',(17.9062791616073,15.6655148338207,6.20560287283945));
#130514=CARTESIAN_POINT('Ctrl Pts',(17.9119253599867,15.6059495699985,6.25737353337065));
#130515=CARTESIAN_POINT('Ctrl Pts',(17.9183626049519,15.5275801394844,6.31025782333974));
#130516=CARTESIAN_POINT('Ctrl Pts',(17.9194340767841,15.5141776415332,6.31882839896031));
#130517=CARTESIAN_POINT('Ctrl Pts',(17.9211267538669,15.4924382626409,6.33198584526223));
#130518=CARTESIAN_POINT('Ctrl Pts',(17.9217555171401,15.4842351005887,6.3367868709464));
#130519=CARTESIAN_POINT('Ctrl Pts',(17.9229512914854,15.4683942502812,6.34574699965837));
#130520=CARTESIAN_POINT('Ctrl Pts',(17.9235189444294,15.4607686785824,6.34992552266441));
#130521=CARTESIAN_POINT('Ctrl Pts',(17.9248330694812,15.442875853715,6.35941850816268));
#130522=CARTESIAN_POINT('Ctrl Pts',(17.9255767240289,15.4325674633394,6.36465287936762));
#130523=CARTESIAN_POINT('Ctrl Pts',(17.9280897440018,15.3971416346311,6.38184915926701));
#130524=CARTESIAN_POINT('Ctrl Pts',(17.9298292038722,15.3716018682482,6.39291190815713));
#130525=CARTESIAN_POINT('Ctrl Pts',(17.9343188705862,15.3035698191934,6.41895491018199));
#130526=CARTESIAN_POINT('Ctrl Pts',(17.937021449321,15.2604463229174,6.43209481573727));
#130527=CARTESIAN_POINT('Ctrl Pts',(17.9428039886906,15.1668658533833,6.4536045624667));
#130528=CARTESIAN_POINT('Ctrl Pts',(17.9458777623418,15.1163480766884,6.4610763861211));
#130529=CARTESIAN_POINT('Ctrl Pts',(17.9497843096605,15.055072894217,6.46523645738158));
#130530=CARTESIAN_POINT('Ctrl Pts',(17.9504549526995,15.0446520395152,6.4657746202088));
#130531=CARTESIAN_POINT('Ctrl Pts',(17.9515038550019,15.0285472907884,6.46634512041499));
#130532=CARTESIAN_POINT('Ctrl Pts',(17.9518761349435,15.0228680701773,6.46649619090531));
#130533=CARTESIAN_POINT('Ctrl Pts',(17.9525772418382,15.0122490788378,6.46668501768854));
#130534=CARTESIAN_POINT('Ctrl Pts',(17.9529054264019,15.0073098410021,6.46673498188979));
#130535=CARTESIAN_POINT('Ctrl Pts',(17.9537030219731,14.9953781813697,6.46676423970374));
#130536=CARTESIAN_POINT('Ctrl Pts',(17.9541743767159,14.9883860522446,6.46670552167659));
#130537=CARTESIAN_POINT('Ctrl Pts',(17.9559149629149,14.9627592710454,6.46621225703878));
#130538=CARTESIAN_POINT('Ctrl Pts',(17.9572048927681,14.9441386915784,6.46531466938631));
#130539=CARTESIAN_POINT('Ctrl Pts',(17.960752642355,14.8936380092983,6.46141437290753));
#130540=CARTESIAN_POINT('Ctrl Pts',(17.9630380382578,14.8618625687701,6.4573653012614));
#130541=CARTESIAN_POINT('Ctrl Pts',(17.970463928082,14.7596968017413,6.43915396490156));
#130542=CARTESIAN_POINT('Ctrl Pts',(17.9755830178685,14.6906549627653,6.41872997247535));
#130543=CARTESIAN_POINT('Ctrl Pts',(17.9814919137304,14.6105259787636,6.38495515043246));
#130544=CARTESIAN_POINT('Ctrl Pts',(17.9825121388226,14.5966888272792,6.37873532585098));
#130545=CARTESIAN_POINT('Ctrl Pts',(17.9841449370835,14.5745517127815,6.36815152473711));
#130546=CARTESIAN_POINT('Ctrl Pts',(17.9847641080932,14.5661592685921,6.36398816258358));
#130547=CARTESIAN_POINT('Ctrl Pts',(17.9859547903937,14.5500309856751,6.35569289597671));
#130548=CARTESIAN_POINT('Ctrl Pts',(17.9865267589366,14.5422882810484,6.35157644207727));
#130549=CARTESIAN_POINT('Ctrl Pts',(17.9878710868155,14.5241104634479,6.34159253811574));
#130550=CARTESIAN_POINT('Ctrl Pts',(17.9886402366176,14.5137260751381,6.3356354116798));
#130551=CARTESIAN_POINT('Ctrl Pts',(17.9913669829866,14.4770128624685,6.31365823603719));
#130552=CARTESIAN_POINT('Ctrl Pts',(17.9932869518528,14.4513414938149,6.29657352718076));
#130553=CARTESIAN_POINT('Ctrl Pts',(17.9982959936048,14.3856432203931,6.24816471367412));
#130554=CARTESIAN_POINT('Ctrl Pts',(18.0013257193629,14.3471955686309,6.21486448611302));
#130555=CARTESIAN_POINT('Ctrl Pts',(18.0068795629692,14.2826349551585,6.14937532031835));
#130556=CARTESIAN_POINT('Ctrl Pts',(18.0093867889278,14.2556343426971,6.11823942649461));
#130557=CARTESIAN_POINT('Ctrl Pts',(18.0126766367787,14.2242945267007,6.07706027901792));
#130558=CARTESIAN_POINT('Ctrl Pts',(18.0133564858849,14.2180247176223,6.06853512044301));
#130559=CARTESIAN_POINT('Ctrl Pts',(18.0144165957525,14.2085894660936,6.05525447456439));
#130560=CARTESIAN_POINT('Ctrl Pts',(18.0147906644586,14.2053239244271,6.05057069996892));
#130561=CARTESIAN_POINT('Ctrl Pts',(18.0154901102102,14.1993402768648,6.04182419855143));
#130562=CARTESIAN_POINT('Ctrl Pts',(18.0158147731818,14.1966112122535,6.03776938015437));
#130563=CARTESIAN_POINT('Ctrl Pts',(18.0165979786235,14.1901419401326,6.0279982474826));
#130564=CARTESIAN_POINT('Ctrl Pts',(18.0170583404214,14.1864314394967,6.02226278562051));
#130565=CARTESIAN_POINT('Ctrl Pts',(18.0187284688762,14.1732882583315,6.00146689548224));
#130566=CARTESIAN_POINT('Ctrl Pts',(18.0199572759245,14.1642110047314,5.98618722333599));
#130567=CARTESIAN_POINT('Ctrl Pts',(18.0232779348797,14.1411125904707,5.94474561044486));
#130568=CARTESIAN_POINT('Ctrl Pts',(18.0253942376146,14.1278665469322,5.91817376006185));
#130569=CARTESIAN_POINT('Ctrl Pts',(18.030008532074,14.10179961599,5.85923626695958));
#130570=CARTESIAN_POINT('Ctrl Pts',(18.032506000554,14.0894604934114,5.82669949922358));
#130571=CARTESIAN_POINT('Ctrl Pts',(18.0381744012657,14.0652153082359,5.75062782529277));
#130572=CARTESIAN_POINT('Ctrl Pts',(18.0413173170397,14.0545475253697,5.70677847415103));
#130573=CARTESIAN_POINT('Ctrl Pts',(18.0452697394032,14.0447346602697,5.64917142230363));
#130574=CARTESIAN_POINT('Ctrl Pts',(18.0461648294619,14.0427647067609,5.6359581039228));
#130575=CARTESIAN_POINT('Ctrl Pts',(18.0475864180532,14.0400460673616,5.61471258456415));
#130576=CARTESIAN_POINT('Ctrl Pts',(18.0481182525748,14.0391230005478,5.60670486581259));
#130577=CARTESIAN_POINT('Ctrl Pts',(18.0491809742467,14.0374691850684,5.59058840811177));
#130578=CARTESIAN_POINT('Ctrl Pts',(18.0497117561455,14.0367404989088,5.58248011649193));
#130579=CARTESIAN_POINT('Ctrl Pts',(18.0507941390795,14.0354560278096,5.56583101652093));
#130580=CARTESIAN_POINT('Ctrl Pts',(18.0513453645958,14.0349110656988,5.55729008100414));
#130581=CARTESIAN_POINT('Ctrl Pts',(18.0529443477483,14.033651848075,5.53234690915795));
#130582=CARTESIAN_POINT('Ctrl Pts',(18.053982926214,14.0332418710457,5.51593207069491));
#130583=CARTESIAN_POINT('Ctrl Pts',(18.0550108970343,14.0332501220858,5.49951414732463));
#130584=CARTESIAN_POINT('Origin',(13.2437274406976,15.,5.5));
#130585=CARTESIAN_POINT('',(14.3005175290658,14.3042076641721,5.74898599439144));
#130586=CARTESIAN_POINT('',(14.2215869807902,14.3043221293274,5.74892323211324));
#130587=CARTESIAN_POINT('',(13.2437274406976,14.3042076641721,5.74898599439144));
#130588=CARTESIAN_POINT('',(14.2111241293531,15.1353891683142,6.22635393211075));
#130589=CARTESIAN_POINT('Ctrl Pts',(14.3005175290658,14.3042076641721,5.74898599439144));
#130590=CARTESIAN_POINT('Ctrl Pts',(14.2989144299391,14.310124946029,5.76552186170024));
#130591=CARTESIAN_POINT('Ctrl Pts',(14.2973221359364,14.3166336622363,5.78185228783364));
#130592=CARTESIAN_POINT('Ctrl Pts',(14.2949908712359,14.327164580291,5.8057553425873));
#130593=CARTESIAN_POINT('Ctrl Pts',(14.2942349309219,14.3307405840018,5.81350547873262));
#130594=CARTESIAN_POINT('Ctrl Pts',(14.2930767780573,14.3364790020146,5.82539617763793));
#130595=CARTESIAN_POINT('Ctrl Pts',(14.29266952052,14.3385475893906,5.82958079351132));
#130596=CARTESIAN_POINT('Ctrl Pts',(14.2918147405124,14.3429990359836,5.83837502079495));
#130597=CARTESIAN_POINT('Ctrl Pts',(14.2913678469936,14.3453910720543,5.842979703518));
#130598=CARTESIAN_POINT('Ctrl Pts',(14.2901888210751,14.3518693914283,5.85513578615727));
#130599=CARTESIAN_POINT('Ctrl Pts',(14.2894615431732,14.35603928679,5.86264215447201));
#130600=CARTESIAN_POINT('Ctrl Pts',(14.2858238669878,14.3777300403012,5.90013383873696));
#130601=CARTESIAN_POINT('Ctrl Pts',(14.2830113999811,14.3972205376587,5.92893426075455));
#130602=CARTESIAN_POINT('Ctrl Pts',(14.2760109154024,14.4508371041792,5.99724846229244));
#130603=CARTESIAN_POINT('Ctrl Pts',(14.2718496518594,14.4872475473401,6.0347149362366));
#130604=CARTESIAN_POINT('Ctrl Pts',(14.2664203483292,14.5374462877555,6.07648898730475));
#130605=CARTESIAN_POINT('Ctrl Pts',(14.2653130928246,14.5478238941084,6.08466418975156));
#130606=CARTESIAN_POINT('Ctrl Pts',(14.263514522439,14.5648616265861,6.09736106981975));
#130607=CARTESIAN_POINT('Ctrl Pts',(14.2628300919144,14.5713865962394,6.10205995638556));
#130608=CARTESIAN_POINT('Ctrl Pts',(14.2613774595412,14.5853120572962,6.11174712042919));
#130609=CARTESIAN_POINT('Ctrl Pts',(14.2606084378468,14.592728781948,6.11670963095666));
#130610=CARTESIAN_POINT('Ctrl Pts',(14.2586925803046,14.6113032768607,6.12865658437628));
#130611=CARTESIAN_POINT('Ctrl Pts',(14.2575401565641,14.6225607862165,6.13547921693106));
#130612=CARTESIAN_POINT('Ctrl Pts',(14.2526482115671,14.6706594508275,6.1629005437584));
#130613=CARTESIAN_POINT('Ctrl Pts',(14.2488148988832,14.7090419758722,6.18062071603704));
#130614=CARTESIAN_POINT('Ctrl Pts',(14.2408477729093,14.7906608743542,6.21013179820528));
#130615=CARTESIAN_POINT('Ctrl Pts',(14.2367251712402,14.8338921033393,6.22146994500351));
#130616=CARTESIAN_POINT('Ctrl Pts',(14.2319785368801,14.886342120804,6.23025777311806));
#130617=CARTESIAN_POINT('Ctrl Pts',(14.2312189746746,14.8948237283986,6.23152751170346));
#130618=CARTESIAN_POINT('Ctrl Pts',(14.230011268403,14.9084733731188,6.23332859796016));
#130619=CARTESIAN_POINT('Ctrl Pts',(14.229558538495,14.9136279980075,6.23395356793651));
#130620=CARTESIAN_POINT('Ctrl Pts',(14.2286433800297,14.924131127763,6.23511482116643));
#130621=CARTESIAN_POINT('Ctrl Pts',(14.2281811636339,14.9294796988879,6.23564718368991));
#130622=CARTESIAN_POINT('Ctrl Pts',(14.2272289140466,14.9405795405494,6.23662981240413));
#130623=CARTESIAN_POINT('Ctrl Pts',(14.2267393538851,14.9463312415515,6.23707119196986));
#130624=CARTESIAN_POINT('Ctrl Pts',(14.225483544493,14.9611861936966,6.23803632629154));
#130625=CARTESIAN_POINT('Ctrl Pts',(14.224721774194,14.9702953122305,6.23845905905128));
#130626=CARTESIAN_POINT('Ctrl Pts',(14.2196286246053,15.0316935426315,6.24017036159618));
#130627=CARTESIAN_POINT('Ctrl Pts',(14.2154840848789,15.083988662881,6.23607315801718));
#130628=CARTESIAN_POINT('Ctrl Pts',(14.2112487597337,15.1354171833248,6.2264868797579));
#130629=CARTESIAN_POINT('',(14.2104374411951,14.3543584447163,5.86069344365419));
#130630=CARTESIAN_POINT('Origin',(14.211,15.,5.5));
#130631=CARTESIAN_POINT('Ctrl Pts',(14.210553733114,14.3548588757739,5.86043574993653));
#130632=CARTESIAN_POINT('Ctrl Pts',(14.2112419750398,14.3509984596515,5.85352602137142));
#130633=CARTESIAN_POINT('Ctrl Pts',(14.2119342498727,14.3472494500005,5.84655498469671));
#130634=CARTESIAN_POINT('Ctrl Pts',(14.2137122629482,14.3379642055853,5.82860430238041));
#130635=CARTESIAN_POINT('Ctrl Pts',(14.2148034098591,14.3325889791096,5.81754475279969));
#130636=CARTESIAN_POINT('Ctrl Pts',(14.2177517409103,14.3189282362072,5.78755701600778));
#130637=CARTESIAN_POINT('Ctrl Pts',(14.2196239758872,14.3111569531308,5.76840805509445));
#130638=CARTESIAN_POINT('Ctrl Pts',(14.2215130984838,14.3041985386328,5.74896049156307));
#130639=CARTESIAN_POINT('Origin',(13.2437274406976,15.,5.5));
#130640=CARTESIAN_POINT('',(14.7015708502323,14.3042076642092,5.74898599449524));
#130641=CARTESIAN_POINT('',(14.6223301870619,14.3039706980243,5.74911183878948));
#130642=CARTESIAN_POINT('',(13.2437274406976,14.3042076641721,5.74898599439144));
#130643=CARTESIAN_POINT('Ctrl Pts',(14.7015708502323,14.3042076642463,5.74898599459905));
#130644=CARTESIAN_POINT('Ctrl Pts',(14.701267806545,14.3053884691484,5.75228575851628));
#130645=CARTESIAN_POINT('Ctrl Pts',(14.700963995868,14.3065927345564,5.75557708635813));
#130646=CARTESIAN_POINT('Ctrl Pts',(14.699411568657,14.312849886356,5.77230843738443));
#130647=CARTESIAN_POINT('Ctrl Pts',(14.6981511326319,14.3182698787912,5.78560662306213));
#130648=CARTESIAN_POINT('Ctrl Pts',(14.6953173478509,14.3311929782285,5.81484656144697));
#130649=CARTESIAN_POINT('Ctrl Pts',(14.6937386979415,14.3388856121142,5.83069450392347));
#130650=CARTESIAN_POINT('Ctrl Pts',(14.6879994437572,14.3686134650661,5.88674695541637));
#130651=CARTESIAN_POINT('Ctrl Pts',(14.683760741336,14.393810839229,5.92515436181349));
#130652=CARTESIAN_POINT('Ctrl Pts',(14.6774540830455,14.4368037430779,5.97902419704531));
#130653=CARTESIAN_POINT('Ctrl Pts',(14.6753575046946,14.4520473638091,5.9963893161148));
#130654=CARTESIAN_POINT('Ctrl Pts',(14.6726381683769,14.4732803807093,6.01840480435905));
#130655=CARTESIAN_POINT('Ctrl Pts',(14.6719769805336,14.4785618480709,6.02371687581842));
#130656=CARTESIAN_POINT('Ctrl Pts',(14.6708846891836,14.4874967262137,6.03243433077191));
#130657=CARTESIAN_POINT('Ctrl Pts',(14.6704504500508,14.4911053891,6.03588450647049));
#130658=CARTESIAN_POINT('Ctrl Pts',(14.6695259293109,14.4989133875257,6.04319956691947));
#130659=CARTESIAN_POINT('Ctrl Pts',(14.6690364567184,14.5031229749826,6.04705282319242));
#130660=CARTESIAN_POINT('Ctrl Pts',(14.6675936522134,14.5157444538783,6.05834001663442));
#130661=CARTESIAN_POINT('Ctrl Pts',(14.6666496488284,14.5242820147883,6.06563190129867));
#130662=CARTESIAN_POINT('Ctrl Pts',(14.6643956685121,14.5452626249511,6.08274005164855));
#130663=CARTESIAN_POINT('Ctrl Pts',(14.6630954446102,14.5578619550194,6.09235637360294));
#130664=CARTESIAN_POINT('Ctrl Pts',(14.6592979196196,14.595831125286,6.11944893541082));
#130665=CARTESIAN_POINT('Ctrl Pts',(14.6568315289693,14.62199520517,6.13575308447036));
#130666=CARTESIAN_POINT('Ctrl Pts',(14.651533144489,14.6798446657623,6.16696465836887));
#130667=CARTESIAN_POINT('Ctrl Pts',(14.6487024788669,14.7117220691834,6.18134916359588));
#130668=CARTESIAN_POINT('Ctrl Pts',(14.6446807964519,14.7571488775215,6.19808753652944));
#130669=CARTESIAN_POINT('Ctrl Pts',(14.6435510954004,14.7699277282347,6.20240271915735));
#130670=CARTESIAN_POINT('Ctrl Pts',(14.6417264575681,14.7905417391893,6.20874082345869));
#130671=CARTESIAN_POINT('Ctrl Pts',(14.6410388148323,14.7983048935685,6.2109890230949));
#130672=CARTESIAN_POINT('Ctrl Pts',(14.639587463633,14.8146663435325,6.21543775926846));
#130673=CARTESIAN_POINT('Ctrl Pts',(14.6388230311735,14.8232704705992,6.21761160113773));
#130674=CARTESIAN_POINT('Ctrl Pts',(14.6369362113905,14.8444605089657,6.22256109948304));
#130675=CARTESIAN_POINT('Ctrl Pts',(14.6358086117844,14.8570833776075,6.22516333971602));
#130676=CARTESIAN_POINT('Ctrl Pts',(14.6308007329605,14.9129187302258,6.23515958043277));
#130677=CARTESIAN_POINT('Ctrl Pts',(14.626817120478,14.9566643240459,6.23902870969415));
#130678=CARTESIAN_POINT('Ctrl Pts',(14.6188072372161,15.0438864757312,6.23897124817574));
#130679=CARTESIAN_POINT('Ctrl Pts',(14.6147977956115,15.087202768997,6.2351196229914));
#130680=CARTESIAN_POINT('Ctrl Pts',(14.6101461821876,15.1384849684717,6.22596030866754));
#130681=CARTESIAN_POINT('Ctrl Pts',(14.6093764317879,15.1470091997274,6.22428224605358));
#130682=CARTESIAN_POINT('Ctrl Pts',(14.6081570612918,15.1605950959485,6.22135799160512));
#130683=CARTESIAN_POINT('Ctrl Pts',(14.6077026917716,15.1656763226698,6.22020795544054));
#130684=CARTESIAN_POINT('Ctrl Pts',(14.6067904429232,15.1759222450937,6.21777480900454));
#130685=CARTESIAN_POINT('Ctrl Pts',(14.6063327045588,15.1810860681342,6.21648946553497));
#130686=CARTESIAN_POINT('Ctrl Pts',(14.6050881905973,15.1951750241103,6.2128204814137));
#130687=CARTESIAN_POINT('Ctrl Pts',(14.6043072683205,15.2040704470951,6.21032500006579));
#130688=CARTESIAN_POINT('Ctrl Pts',(14.6008266032506,15.2438522987441,6.19835568056725));
#130689=CARTESIAN_POINT('Ctrl Pts',(14.5982072210285,15.2741478773704,6.18702845060417));
#130690=CARTESIAN_POINT('Ctrl Pts',(14.5912731272345,15.352531799387,6.15170689407542));
#130691=CARTESIAN_POINT('Ctrl Pts',(14.5869924055877,15.3989031539572,6.12440053168542));
#130692=CARTESIAN_POINT('Ctrl Pts',(14.5814475175013,15.4523326473204,6.08453858548331));
#130693=CARTESIAN_POINT('Ctrl Pts',(14.5803567326554,15.4625500410934,6.07648729333851));
#130694=CARTESIAN_POINT('Ctrl Pts',(14.5785099034493,15.4793196965112,6.06253993614659));
#130695=CARTESIAN_POINT('Ctrl Pts',(14.5777596592846,15.4859888059428,6.0567884854284));
#130696=CARTESIAN_POINT('Ctrl Pts',(14.5762222352992,15.4993538943086,6.04483933894811));
#130697=CARTESIAN_POINT('Ctrl Pts',(14.57543483262,15.5060410232793,6.03863409054969));
#130698=CARTESIAN_POINT('Ctrl Pts',(14.5734005193417,15.5229035765834,6.02239546219996));
#130699=CARTESIAN_POINT('Ctrl Pts',(14.5721463754687,15.5329054375387,6.01218834660953));
#130700=CARTESIAN_POINT('Ctrl Pts',(14.5693299168533,15.5544796238679,5.9888551105171));
#130701=CARTESIAN_POINT('Ctrl Pts',(14.5677624109683,15.5658940131104,5.97559524729847));
#130702=CARTESIAN_POINT('Ctrl Pts',(14.5621063476228,15.604989822456,5.92677657142481));
#130703=CARTESIAN_POINT('Ctrl Pts',(14.557942324498,15.6298764863027,5.88910912300637));
#130704=CARTESIAN_POINT('Ctrl Pts',(14.5515937631531,15.6626598713458,5.82801341353703));
#130705=CARTESIAN_POINT('Ctrl Pts',(14.5493866804984,15.673083052649,5.80605617346355));
#130706=CARTESIAN_POINT('Ctrl Pts',(14.5465681749533,15.6852535609962,5.77677351284916));
#130707=CARTESIAN_POINT('Ctrl Pts',(14.5459135432988,15.6879972592758,5.7698810940452));
#130708=CARTESIAN_POINT('Ctrl Pts',(14.5448287443299,15.692409325123,5.75829274207759));
#130709=CARTESIAN_POINT('Ctrl Pts',(14.5443955369173,15.6941347552552,5.75361932627306));
#130710=CARTESIAN_POINT('Ctrl Pts',(14.5434693003087,15.6977461192832,5.74352472138963));
#130711=CARTESIAN_POINT('Ctrl Pts',(14.5429771317728,15.6996163813272,5.7380984305573));
#130712=CARTESIAN_POINT('Ctrl Pts',(14.5415165932995,15.7050138167016,5.72182558751973));
#130713=CARTESIAN_POINT('Ctrl Pts',(14.5405579002258,15.7083535273689,5.71091798445137));
#130714=CARTESIAN_POINT('Ctrl Pts',(14.5382593569631,15.7158264147139,5.68432700761366));
#130715=CARTESIAN_POINT('Ctrl Pts',(14.536929787555,15.7196986050995,5.66857609485616));
#130716=CARTESIAN_POINT('Ctrl Pts',(14.5331479054982,15.7293040133022,5.62309632964483));
#130717=CARTESIAN_POINT('Ctrl Pts',(14.5307237780026,15.7337334187486,5.59312600285986));
#130718=CARTESIAN_POINT('Ctrl Pts',(14.5254769870785,15.7392795147375,5.52827263108273));
#130719=CARTESIAN_POINT('Ctrl Pts',(14.5226550617432,15.7397903361777,5.49341529172412));
#130720=CARTESIAN_POINT('Ctrl Pts',(14.5186430831266,15.7370883270293,5.44519572933336));
#130721=CARTESIAN_POINT('Ctrl Pts',(14.5175138901773,15.7359660948069,5.43176092730023));
#130722=CARTESIAN_POINT('Ctrl Pts',(14.5156898996518,15.7335845841976,5.41033423059805));
#130723=CARTESIAN_POINT('Ctrl Pts',(14.5150023882257,15.7325603545599,5.40231884333171));
#130724=CARTESIAN_POINT('Ctrl Pts',(14.5135511865942,15.7301359609925,5.38553941311485));
#130725=CARTESIAN_POINT('Ctrl Pts',(14.512786770935,15.7287089420086,5.37678064127879));
#130726=CARTESIAN_POINT('Ctrl Pts',(14.5108997330682,15.7248231477976,5.35536754042156));
#130727=CARTESIAN_POINT('Ctrl Pts',(14.5097718935652,15.7221904173392,5.34274829258643));
#130728=CARTESIAN_POINT('Ctrl Pts',(14.5047524470521,15.7091275725118,5.28741574677365));
#130729=CARTESIAN_POINT('Ctrl Pts',(14.5007568151518,15.6952294455235,5.24562106055232));
#130730=CARTESIAN_POINT('Ctrl Pts',(14.4927490618646,15.6604595581773,5.16565844288695));
#130731=CARTESIAN_POINT('Ctrl Pts',(14.4887542532177,15.6397661571429,5.12758756581377));
#130732=CARTESIAN_POINT('Ctrl Pts',(14.4841152135233,15.611052223549,5.0842935642736));
#130733=CARTESIAN_POINT('Ctrl Pts',(14.4833443905735,15.6061165815586,5.07712960526417));
#130734=CARTESIAN_POINT('Ctrl Pts',(14.4821237836821,15.5980233966744,5.06581550691226));
#130735=CARTESIAN_POINT('Ctrl Pts',(14.4816692331542,15.5949466107293,5.06160897199963));
#130736=CARTESIAN_POINT('Ctrl Pts',(14.4807571432415,15.5886412558044,5.05317705768354));
#130737=CARTESIAN_POINT('Ctrl Pts',(14.4802997386425,15.5854110859988,5.04895328875033));
#130738=CARTESIAN_POINT('Ctrl Pts',(14.479057029991,15.5764559025559,5.0375017866286));
#130739=CARTESIAN_POINT('Ctrl Pts',(14.4782775529401,15.5706405294859,5.0303454298236));
#130740=CARTESIAN_POINT('Ctrl Pts',(14.4748114202874,15.5439558195449,4.99873513288063));
#130741=CARTESIAN_POINT('Ctrl Pts',(14.4722043739278,15.5216357405264,4.97554685669194));
#130742=CARTESIAN_POINT('Ctrl Pts',(14.4652595821577,15.4580068373192,4.91753882279555));
#130743=CARTESIAN_POINT('Ctrl Pts',(14.4609570448515,15.4142852308484,4.88567253461053));
#130744=CARTESIAN_POINT('Ctrl Pts',(14.455390681674,15.356231974462,4.85239820087444));
#130745=CARTESIAN_POINT('Ctrl Pts',(14.4543026260153,15.3448091395608,4.84624475101794));
#130746=CARTESIAN_POINT('Ctrl Pts',(14.4524590325502,15.3253759946238,4.83642716293709));
#130747=CARTESIAN_POINT('Ctrl Pts',(14.4517092484074,15.3174511469462,4.83259966805812));
#130748=CARTESIAN_POINT('Ctrl Pts',(14.4501716300559,15.3011696218219,4.82509170375196));
#130749=CARTESIAN_POINT('Ctrl Pts',(14.4493835582933,15.2928093376706,4.82142279370527));
#130750=CARTESIAN_POINT('Ctrl Pts',(14.4473449115132,15.2711571624565,4.81239535879327));
#130751=CARTESIAN_POINT('Ctrl Pts',(14.4460870403816,15.2577741557115,4.80726717132763));
#130752=CARTESIAN_POINT('Ctrl Pts',(14.4432602946794,15.227675073818,4.79672655537037));
#130753=CARTESIAN_POINT('Ctrl Pts',(14.4416861638558,15.2108983797514,4.79151481985206));
#130754=CARTESIAN_POINT('Ctrl Pts',(14.4359805401268,15.1500270897019,4.77495853504284));
#130755=CARTESIAN_POINT('Ctrl Pts',(14.4317720309761,15.1050931814404,4.76709615589753));
#130756=CARTESIAN_POINT('Ctrl Pts',(14.4254612377103,15.0363682778015,4.76152348289476));
#130757=CARTESIAN_POINT('Ctrl Pts',(14.423332631217,15.0129299258302,4.76074139673383));
#130758=CARTESIAN_POINT('Ctrl Pts',(14.4205794390972,14.9819697409277,4.7611816868809));
#130759=CARTESIAN_POINT('Ctrl Pts',(14.4199152893824,14.9744494679774,4.76140351050627));
#130760=CARTESIAN_POINT('Ctrl Pts',(14.4188238039256,14.9619891331639,4.76196160721052));
#130761=CARTESIAN_POINT('Ctrl Pts',(14.4183932385791,14.9570469051014,4.76223273741448));
#130762=CARTESIAN_POINT('Ctrl Pts',(14.4174750117101,14.9464449131299,4.76292127211181));
#130763=CARTESIAN_POINT('Ctrl Pts',(14.4169881692252,14.9407866108438,4.7633542374187));
#130764=CARTESIAN_POINT('Ctrl Pts',(14.4155632739837,14.9241334372702,4.76482164944413));
#130765=CARTESIAN_POINT('Ctrl Pts',(14.4146341952418,14.913155518348,4.76603745478489));
#130766=CARTESIAN_POINT('Ctrl Pts',(14.4124251720849,14.8868716735825,4.7695464557907));
#130767=CARTESIAN_POINT('Ctrl Pts',(14.4111544559741,14.8716021425636,4.77207523691253));
#130768=CARTESIAN_POINT('Ctrl Pts',(14.4050685100603,14.7983287413865,4.78658781886045));
#130769=CARTESIAN_POINT('Ctrl Pts',(14.4003940549879,14.7418306091224,4.8050345773885));
#130770=CARTESIAN_POINT('Ctrl Pts',(14.3941061036381,14.6726119777229,4.83725463359074));
#130771=CARTESIAN_POINT('Ctrl Pts',(14.3926821566971,14.6573418624367,4.84501935091343));
#130772=CARTESIAN_POINT('Ctrl Pts',(14.3904211205612,14.6338393552793,4.85801705124607));
#130773=CARTESIAN_POINT('Ctrl Pts',(14.3895962993838,14.6254167217405,4.86289477075438));
#130774=CARTESIAN_POINT('Ctrl Pts',(14.3880262539937,14.6096860749912,4.87242447266838));
#130775=CARTESIAN_POINT('Ctrl Pts',(14.3872823913848,14.6023586867983,4.87704143415004));
#130776=CARTESIAN_POINT('Ctrl Pts',(14.3855498704174,14.5855929893541,4.88802175376457));
#130777=CARTESIAN_POINT('Ctrl Pts',(14.3845579872634,14.5762174699572,4.89447635884686));
#130778=CARTESIAN_POINT('Ctrl Pts',(14.3809651740239,14.5430783396257,4.91843773119462));
#130779=CARTESIAN_POINT('Ctrl Pts',(14.3783205146754,14.5202224587935,4.93714557179297));
#130780=CARTESIAN_POINT('Ctrl Pts',(14.372655517622,14.4744377065392,4.9794399971453));
#130781=CARTESIAN_POINT('Ctrl Pts',(14.3696320534765,14.451838430233,5.00329374460986));
#130782=CARTESIAN_POINT('Ctrl Pts',(14.3638252711711,14.4115032183826,5.05198533481528));
#130783=CARTESIAN_POINT('Ctrl Pts',(14.3610463160058,14.3935668338413,5.07657957406272));
#130784=CARTESIAN_POINT('Ctrl Pts',(14.357654334462,14.3730477032107,5.10870574949459));
#130785=CARTESIAN_POINT('Ctrl Pts',(14.3569736187382,14.3690016131414,5.11526447580852));
#130786=CARTESIAN_POINT('Ctrl Pts',(14.3558632174351,14.3625122745119,5.12616157653991));
#130787=CARTESIAN_POINT('Ctrl Pts',(14.3554300567931,14.3600090464157,5.13046332624843));
#130788=CARTESIAN_POINT('Ctrl Pts',(14.3545163845745,14.3547869204473,5.13964971806609));
#130789=CARTESIAN_POINT('Ctrl Pts',(14.3540365641347,14.3520796497563,5.14454048084657));
#130790=CARTESIAN_POINT('Ctrl Pts',(14.3526542387923,14.3443910913841,5.15880985265868));
#130791=CARTESIAN_POINT('Ctrl Pts',(14.3517599418001,14.3395558549154,5.16826618446797));
#130792=CARTESIAN_POINT('Ctrl Pts',(14.3468403861918,14.313840845554,5.22135021339282));
#130793=CARTESIAN_POINT('Ctrl Pts',(14.3429902757745,14.2970768897113,5.26684676113759));
#130794=CARTESIAN_POINT('Ctrl Pts',(14.3360614301468,14.2754051121965,5.35001730955931));
#130795=CARTESIAN_POINT('Ctrl Pts',(14.3330136320369,14.2687191110345,5.38703878684167));
#130796=CARTESIAN_POINT('Ctrl Pts',(14.328878994262,14.2636493618928,5.43633933637818));
#130797=CARTESIAN_POINT('Ctrl Pts',(14.3278703137976,14.2627129722432,5.44830137806929));
#130798=CARTESIAN_POINT('Ctrl Pts',(14.3261122505771,14.2615990058168,5.46899715270202));
#130799=CARTESIAN_POINT('Ctrl Pts',(14.3253672087991,14.2612843243115,5.47772128158993));
#130800=CARTESIAN_POINT('Ctrl Pts',(14.3238068640553,14.2609512530727,5.49588156880129));
#130801=CARTESIAN_POINT('Ctrl Pts',(14.3229908963015,14.2609589130649,5.50531653813821));
#130802=CARTESIAN_POINT('Ctrl Pts',(14.3207746599572,14.2614667867423,5.53075971845945));
#130803=CARTESIAN_POINT('Ctrl Pts',(14.3193643716485,14.2623067408155,5.54675507378159));
#130804=CARTESIAN_POINT('Ctrl Pts',(14.3153935712907,14.2660927965288,5.59121109885985));
#130805=CARTESIAN_POINT('Ctrl Pts',(14.3128030662614,14.2701726250593,5.6195444446003));
#130806=CARTESIAN_POINT('Ctrl Pts',(14.3069704640862,14.2829054103019,5.68202472040388));
#130807=CARTESIAN_POINT('Ctrl Pts',(14.3037235300448,14.2923738286286,5.71591629464904));
#130808=CARTESIAN_POINT('Ctrl Pts',(14.3005175290658,14.3042076641721,5.74898599439144));
#130809=CARTESIAN_POINT('',(14.2442422781566,14.2606640288133,5.50021908758302));
#130810=CARTESIAN_POINT('Ctrl Pts',(14.2215869807902,14.3043221293274,5.74892323211324));
#130811=CARTESIAN_POINT('Ctrl Pts',(14.2248697646003,14.2919680803988,5.7146519512802));
#130812=CARTESIAN_POINT('Ctrl Pts',(14.2281873301198,14.2821560247849,5.67953294869403));
#130813=CARTESIAN_POINT('Ctrl Pts',(14.2314770181605,14.2749982774291,5.6439414857939));
#130814=CARTESIAN_POINT('Ctrl Pts',(14.234766709764,14.2678405223213,5.60834998434789));
#130815=CARTESIAN_POINT('Ctrl Pts',(14.2379949555046,14.2632814103378,5.57229160377229));
#130816=CARTESIAN_POINT('Ctrl Pts',(14.2411291090077,14.2614900739362,5.53615063568822));
#130817=CARTESIAN_POINT('Ctrl Pts',(14.2421667238184,14.2608970215604,5.52418555365778));
#130818=CARTESIAN_POINT('Ctrl Pts',(14.2432044289964,14.2606238001271,5.51220407947721));
#130819=CARTESIAN_POINT('Ctrl Pts',(14.2442421952123,14.2606640265644,5.50022005200379));
#130820=CARTESIAN_POINT('Ctrl Pts',(14.2442423611009,14.2606640310621,5.50021812316224));
#130821=CARTESIAN_POINT('Ctrl Pts',(14.2467604292871,14.2607084642982,5.47077714598032));
#130822=CARTESIAN_POINT('Ctrl Pts',(14.2492104808063,14.2625220578675,5.4412707827379));
#130823=CARTESIAN_POINT('Ctrl Pts',(14.2516428117451,14.2661106683047,5.41193170632528));
#130824=CARTESIAN_POINT('Ctrl Pts',(14.2519183407403,14.266517178049,5.40860824153004));
#130825=CARTESIAN_POINT('Ctrl Pts',(14.2521936423477,14.2669464382962,5.40528697174121));
#130826=CARTESIAN_POINT('Ctrl Pts',(14.2524687896758,14.2673984361738,5.40196827146818));
#130827=CARTESIAN_POINT('Ctrl Pts',(14.2551687278868,14.2718337557873,5.36940286100478));
#130828=CARTESIAN_POINT('Ctrl Pts',(14.257854511435,14.2784609639366,5.33708066115314));
#130829=CARTESIAN_POINT('Ctrl Pts',(14.2605672626014,14.2872101843153,5.30531268485562));
#130830=CARTESIAN_POINT('Ctrl Pts',(14.263277356756,14.2959508352457,5.27357582379153));
#130831=CARTESIAN_POINT('Ctrl Pts',(14.2660147514805,14.3068088742505,5.24239213419929));
#130832=CARTESIAN_POINT('Ctrl Pts',(14.2688013850528,14.3196770880376,5.21205406993458));
#130833=CARTESIAN_POINT('Ctrl Pts',(14.2716167631207,14.3326780391594,5.18140306450668));
#130834=CARTESIAN_POINT('Ctrl Pts',(14.2744826125123,14.3477306509699,5.15161525159242));
#130835=CARTESIAN_POINT('Ctrl Pts',(14.2773975710157,14.3646909466205,5.12297374166932));
#130836=CARTESIAN_POINT('Ctrl Pts',(14.2802840518035,14.3814855484971,5.09461204525697));
#130837=CARTESIAN_POINT('Ctrl Pts',(14.2832186288134,14.400150649726,5.06737434612188));
#130838=CARTESIAN_POINT('Ctrl Pts',(14.2861755727077,14.4205162102673,5.04151752419138));
#130839=CARTESIAN_POINT('Ctrl Pts',(14.2891762759477,14.4411831575227,5.01527805123663));
#130840=CARTESIAN_POINT('Ctrl Pts',(14.2921998140541,14.4636015705217,4.9904607738186));
#130841=CARTESIAN_POINT('Ctrl Pts',(14.2951957160754,14.4875607689585,4.96731456331708));
#130842=CARTESIAN_POINT('Ctrl Pts',(14.297962320326,14.509686198884,4.94593989755595));
#130843=CARTESIAN_POINT('Ctrl Pts',(14.3007048100857,14.5331262564948,4.92598991755922));
#130844=CARTESIAN_POINT('Ctrl Pts',(14.3033699190066,14.5576837540332,4.90764441773356));
#130845=CARTESIAN_POINT('Ctrl Pts',(14.3035908047853,14.559719093724,4.90612393202917));
#130846=CARTESIAN_POINT('Ctrl Pts',(14.3038111590203,14.5617621182262,4.90461443947957));
#130847=CARTESIAN_POINT('Ctrl Pts',(14.3040309513857,14.5638127205748,4.90311602720806));
#130848=CARTESIAN_POINT('Ctrl Pts',(14.3040321491743,14.5638238956124,4.90310786140567));
#130849=CARTESIAN_POINT('Ctrl Pts',(14.3040333469478,14.5638350708957,4.90309969591605));
#130850=CARTESIAN_POINT('Ctrl Pts',(14.3040345447063,14.5638462464246,4.90309153073925));
#130851=CARTESIAN_POINT('Ctrl Pts',(14.306629244969,14.5880557571609,4.88540333561519));
#130852=CARTESIAN_POINT('Ctrl Pts',(14.3091535475,14.6134222131576,4.86918317244379));
#130853=CARTESIAN_POINT('Ctrl Pts',(14.3116484096287,14.6397327828386,4.85456421835864));
#130854=CARTESIAN_POINT('Ctrl Pts',(14.3119018982887,14.6424060492192,4.8530788701146));
#130855=CARTESIAN_POINT('Ctrl Pts',(14.3121550830228,14.6450890177863,4.85161004932618));
#130856=CARTESIAN_POINT('Ctrl Pts',(14.3124080067914,14.6477814354157,4.85015789303608));
#130857=CARTESIAN_POINT('Ctrl Pts',(14.3151471500034,14.6769400926496,4.83443116214175));
#130858=CARTESIAN_POINT('Ctrl Pts',(14.3178565197513,14.7072125808724,4.82065887681126));
#130859=CARTESIAN_POINT('Ctrl Pts',(14.3205827364436,14.7382976380876,4.8089675697619));
#130860=CARTESIAN_POINT('Ctrl Pts',(14.3233062437292,14.7693518019183,4.79728788193015));
#130861=CARTESIAN_POINT('Ctrl Pts',(14.3260470428033,14.8012165799276,4.78768458369584));
#130862=CARTESIAN_POINT('Ctrl Pts',(14.3288339245698,14.8335851856984,4.78024081182856));
#130863=CARTESIAN_POINT('Ctrl Pts',(14.3316195658775,14.8659393839971,4.77280035323145));
#130864=CARTESIAN_POINT('Ctrl Pts',(14.3344514718522,14.8987968133817,4.76751722030853));
#130865=CARTESIAN_POINT('Ctrl Pts',(14.3373355482926,14.9318482118683,4.76443694336892));
#130866=CARTESIAN_POINT('Ctrl Pts',(14.3402220634959,14.9649275584783,4.76135406176011));
#130867=CARTESIAN_POINT('Ctrl Pts',(14.3431608765856,14.9982011697976,4.76047767289296));
#130868=CARTESIAN_POINT('Ctrl Pts',(14.3461330712643,15.0313574370878,4.7618186309569));
#130869=CARTESIAN_POINT('Ctrl Pts',(14.3491067426328,15.0645301775666,4.76316025525552));
#130870=CARTESIAN_POINT('Ctrl Pts',(14.3521136607897,15.0975855176736,4.76672157718414));
#130871=CARTESIAN_POINT('Ctrl Pts',(14.3551109360268,15.1302095814376,4.7724783327648));
#130872=CARTESIAN_POINT('Ctrl Pts',(14.3581140312821,15.1628969936191,4.77824626663885));
#130873=CARTESIAN_POINT('Ctrl Pts',(14.3611069637679,15.1951515006022,4.78621869460513));
#130874=CARTESIAN_POINT('Ctrl Pts',(14.3640272845584,15.2266545773731,4.79633101960155));
#130875=CARTESIAN_POINT('Ctrl Pts',(14.3650241516788,15.2374083211149,4.79978291582225));
#130876=CARTESIAN_POINT('Ctrl Pts',(14.366012429098,15.2480744791746,4.8034837759039));
#130877=CARTESIAN_POINT('Ctrl Pts',(14.3669893251901,15.2586403193246,4.80742974171195));
#130878=CARTESIAN_POINT('Ctrl Pts',(14.366990579758,15.2586538883866,4.80743480927438));
#130879=CARTESIAN_POINT('Ctrl Pts',(14.366991834309,15.2586674573113,4.80743987725041));
#130880=CARTESIAN_POINT('Ctrl Pts',(14.3669930888434,15.2586810260987,4.80744494564005));
#130881=CARTESIAN_POINT('Ctrl Pts',(14.3695787610439,15.2866471297844,4.81789120778495));
#130882=CARTESIAN_POINT('Ctrl Pts',(14.372093138749,15.3140323479414,4.83009815532248));
#130883=CARTESIAN_POINT('Ctrl Pts',(14.3745772892216,15.340609796519,4.84396317939131));
#130884=CARTESIAN_POINT('Ctrl Pts',(14.374832750069,15.343342923039,4.84538900718936));
#130885=CARTESIAN_POINT('Ctrl Pts',(14.3750878912543,15.3460674842986,4.84683233036716));
#130886=CARTESIAN_POINT('Ctrl Pts',(14.375342757439,15.348783218757,4.84829300993393));
#130887=CARTESIAN_POINT('Ctrl Pts',(14.3780727997337,15.3778732682692,4.86393932645365));
#130888=CARTESIAN_POINT('Ctrl Pts',(14.3807721227504,15.4059536841026,4.88158174700822));
#130889=CARTESIAN_POINT('Ctrl Pts',(14.3834877411975,15.432753730036,4.90104012195106));
#130890=CARTESIAN_POINT('Ctrl Pts',(14.3862005110504,15.4595256636047,4.92047808570009));
#130891=CARTESIAN_POINT('Ctrl Pts',(14.3889300205994,15.4850200982898,4.94172766113073));
#130892=CARTESIAN_POINT('Ctrl Pts',(14.3917055192335,15.5089994042371,4.96458005592421));
#130893=CARTESIAN_POINT('Ctrl Pts',(14.3944796550394,15.5329669358409,4.98742122971137));
#130894=CARTESIAN_POINT('Ctrl Pts',(14.3972999585682,15.555420971719,5.01186336788663));
#130895=CARTESIAN_POINT('Ctrl Pts',(14.4001728576909,15.576153906496,5.03767480536044));
#130896=CARTESIAN_POINT('Ctrl Pts',(14.4030480836802,15.5969036336391,5.06350714846636));
#130897=CARTESIAN_POINT('Ctrl Pts',(14.4059760321815,15.615929524449,5.09071092442181));
#130898=CARTESIAN_POINT('Ctrl Pts',(14.4089383556134,15.6330516845592,5.11903341319642));
#130899=CARTESIAN_POINT('Ctrl Pts',(14.4119020789529,15.6501819361021,5.14736928635192));
#130900=CARTESIAN_POINT('Ctrl Pts',(14.4149000481656,15.6654065699473,5.17682504842975));
#130901=CARTESIAN_POINT('Ctrl Pts',(14.4178899265822,15.6785738204058,5.20712690092421));
#130902=CARTESIAN_POINT('Ctrl Pts',(14.4208856284582,15.6917667170405,5.23748777307884));
#130903=CARTESIAN_POINT('Ctrl Pts',(14.4238727389467,15.7028938078213,5.26869835220417));
#130904=CARTESIAN_POINT('Ctrl Pts',(14.4267892002207,15.7118343797676,5.30045907912811));
#130905=CARTESIAN_POINT('Ctrl Pts',(14.4278482484995,15.7150809503346,5.3119922832492));
#130906=CARTESIAN_POINT('Ctrl Pts',(14.4288978335193,15.7180395400288,5.32359777545549));
#130907=CARTESIAN_POINT('Ctrl Pts',(14.4299345986302,15.7207056368008,5.33526029301637));
#130908=CARTESIAN_POINT('Ctrl Pts',(14.4299358766582,15.7207089233179,5.33527466948756));
#130909=CARTESIAN_POINT('Ctrl Pts',(14.4299371546687,15.7207122093985,5.33528904607521));
#130910=CARTESIAN_POINT('Ctrl Pts',(14.4299384326618,15.7207154950427,5.33530342277929));
#130911=CARTESIAN_POINT('Ctrl Pts',(14.4325273633362,15.7273714814289,5.36442743691014));
#130912=CARTESIAN_POINT('Ctrl Pts',(14.4350448117096,15.7322344141166,5.39403323947481));
#130913=CARTESIAN_POINT('Ctrl Pts',(14.4375316836577,15.7352656946264,5.42387472832081));
#130914=CARTESIAN_POINT('Ctrl Pts',(14.4377898328919,15.7355803560801,5.42697241797076));
#130915=CARTESIAN_POINT('Ctrl Pts',(14.4380476526519,15.7358753014408,5.43007260585816));
#130916=CARTESIAN_POINT('Ctrl Pts',(14.4383051886924,15.7361505028073,5.4331749885224));
#130917=CARTESIAN_POINT('Ctrl Pts',(14.4410405763686,15.7390735205912,5.46612656798922));
#130918=CARTESIAN_POINT('Ctrl Pts',(14.4437447966235,15.7397669865307,5.4993309370506));
#130919=CARTESIAN_POINT('Ctrl Pts',(14.4464648946848,15.7382331285503,5.53246191912244));
#130920=CARTESIAN_POINT('Ctrl Pts',(14.4491821912515,15.7367008503272,5.56555877879707));
#130921=CARTESIAN_POINT('Ctrl Pts',(14.4519158152569,15.732946388313,5.59858226648247));
#130922=CARTESIAN_POINT('Ctrl Pts',(14.454695072665,15.7270141370407,5.63121826876531));
#130923=CARTESIAN_POINT('Ctrl Pts',(14.457473005414,15.7210847132182,5.66383871596583));
#130924=CARTESIAN_POINT('Ctrl Pts',(14.460296753895,15.7129798930243,5.69607201826397));
#130925=CARTESIAN_POINT('Ctrl Pts',(14.4631727829094,15.7027796686425,5.727616673456));
#130926=CARTESIAN_POINT('Ctrl Pts',(14.4660511555404,15.6925711323083,5.75918703373707));
#130927=CARTESIAN_POINT('Ctrl Pts',(14.468981936248,15.6802638759292,5.79006762672038));
#130928=CARTESIAN_POINT('Ctrl Pts',(14.4719467740945,15.6659706856688,5.819968566145));
#130929=CARTESIAN_POINT('Ctrl Pts',(14.4749130271505,15.6516706728234,5.84988377821943));
#130930=CARTESIAN_POINT('Ctrl Pts',(14.4779132075223,15.6353826794534,5.87881839691178));
#130931=CARTESIAN_POINT('Ctrl Pts',(14.4809049351614,15.6172525632722,5.90649442785779));
#130932=CARTESIAN_POINT('Ctrl Pts',(14.4839024479596,15.5990873885497,5.93422397645728));
#130933=CARTESIAN_POINT('Ctrl Pts',(14.4868910033293,15.5790724690893,5.96068990556623));
#130934=CARTESIAN_POINT('Ctrl Pts',(14.4898084895584,15.5573923142399,5.98562596341381));
#130935=CARTESIAN_POINT('Ctrl Pts',(14.4908357699898,15.5497584825504,5.99440623596856));
#130936=CARTESIAN_POINT('Ctrl Pts',(14.4918541001814,15.5419185708745,6.00299696561843));
#130937=CARTESIAN_POINT('Ctrl Pts',(14.4928604199827,15.5338819616943,6.0113870284288));
#130938=CARTESIAN_POINT('Ctrl Pts',(14.4928616695749,15.5338719822782,6.01139744674406));
#130939=CARTESIAN_POINT('Ctrl Pts',(14.4928629191505,15.5338620025394,6.01140786477173));
#130940=CARTESIAN_POINT('Ctrl Pts',(14.4928641687095,15.5338520224779,6.01141828251177));
#130941=CARTESIAN_POINT('Ctrl Pts',(14.4954536365896,15.5131702878352,6.0330070207212));
#130942=CARTESIAN_POINT('Ctrl Pts',(14.4979719606962,15.4910984741824,6.05336125999676));
#130943=CARTESIAN_POINT('Ctrl Pts',(14.500460108996,15.467821300313,6.07231315241162));
#130944=CARTESIAN_POINT('Ctrl Pts',(14.5007162406014,15.4654251328845,6.074264072552));
#130945=CARTESIAN_POINT('Ctrl Pts',(14.5009720524405,15.46301623774,6.07620012694115));
#130946=CARTESIAN_POINT('Ctrl Pts',(14.5012275892028,15.4605948474988,6.07812112976851));
#130947=CARTESIAN_POINT('Ctrl Pts',(14.5039623658394,15.4346809187121,6.0986798689671));
#130948=CARTESIAN_POINT('Ctrl Pts',(14.5066664734542,15.4073303639171,6.11751573878081));
#130949=CARTESIAN_POINT('Ctrl Pts',(14.5093868373066,15.3788167160486,6.13445131519405));
#130950=CARTESIAN_POINT('Ctrl Pts',(14.5121044090448,15.3503323338847,6.15136950934962));
#130951=CARTESIAN_POINT('Ctrl Pts',(14.5148386837705,15.3206876622895,6.16639169543563));
#130952=CARTESIAN_POINT('Ctrl Pts',(14.5176188159135,15.2901693561779,6.17938224246889));
#130953=CARTESIAN_POINT('Ctrl Pts',(14.5203976335316,15.2596654799822,6.1923666472051));
#130954=CARTESIAN_POINT('Ctrl Pts',(14.5232224896802,15.228288993506,6.20332158140069));
#130955=CARTESIAN_POINT('Ctrl Pts',(14.5260996919465,15.1963356147579,6.21214804855116));
#130956=CARTESIAN_POINT('Ctrl Pts',(14.5289792573594,15.1643559915855,6.22098176518695));
#130957=CARTESIAN_POINT('Ctrl Pts',(14.53191129621,15.1317985810812,6.22768360115573));
#130958=CARTESIAN_POINT('Ctrl Pts',(14.534877310697,15.0989674590039,6.23218832584451));
#130959=CARTESIAN_POINT('Ctrl Pts',(14.5378447518066,15.0661205454935,6.23669521725968));
#130960=CARTESIAN_POINT('Ctrl Pts',(14.540846037674,15.0329995778638,6.23900275407254));
#130961=CARTESIAN_POINT('Ctrl Pts',(14.5438386677894,14.9999169121041,6.23907987489896));
#130962=CARTESIAN_POINT('Ctrl Pts',(14.5468371037384,14.9667700645224,6.23915714534316));
#130963=CARTESIAN_POINT('Ctrl Pts',(14.5498263765233,14.9336615313222,6.23699483779894));
#130964=CARTESIAN_POINT('Ctrl Pts',(14.5527443018251,14.9009151441113,6.23260066238511));
#130965=CARTESIAN_POINT('Ctrl Pts',(14.5537731552654,14.8893688467756,6.23105128670754));
#130966=CARTESIAN_POINT('Ctrl Pts',(14.5547929997385,14.8778676704415,6.22922482656027));
#130967=CARTESIAN_POINT('Ctrl Pts',(14.5558007613404,14.8664261254646,6.22712301133068));
#130968=CARTESIAN_POINT('Ctrl Pts',(14.5558020208007,14.8664118262776,6.22712038456576));
#130969=CARTESIAN_POINT('Ctrl Pts',(14.5558032802441,14.8663975271542,6.22711775736648));
#130970=CARTESIAN_POINT('Ctrl Pts',(14.5558045396706,14.8663832280945,6.2271151297328));
#130971=CARTESIAN_POINT('Ctrl Pts',(14.5583928450922,14.8369965725034,6.2217149588477));
#130972=CARTESIAN_POINT('Ctrl Pts',(14.5609098652777,14.8078758271027,6.21447688966069));
#130973=CARTESIAN_POINT('Ctrl Pts',(14.5633965756876,14.7792625071587,6.20546269975056));
#130974=CARTESIAN_POINT('Ctrl Pts',(14.5636531362126,14.776310394859,6.20453268180936));
#130975=CARTESIAN_POINT('Ctrl Pts',(14.5639093741022,14.7733637133995,6.20358379273608));
#130976=CARTESIAN_POINT('Ctrl Pts',(14.5641653343571,14.7704227475361,6.20261612504836));
#130977=CARTESIAN_POINT('Ctrl Pts',(14.5668990455627,14.7390125923053,6.19228122362686));
#130978=CARTESIAN_POINT('Ctrl Pts',(14.5696019248745,14.7082504869431,6.17980028029817));
#130979=CARTESIAN_POINT('Ctrl Pts',(14.5723209571294,14.6784349284052,6.16530399818331));
#130980=CARTESIAN_POINT('Ctrl Pts',(14.5750371794267,14.6486501824671,6.15082269711056));
#130981=CARTESIAN_POINT('Ctrl Pts',(14.5777700016255,14.6198099352693,6.13433078180673));
#130982=CARTESIAN_POINT('Ctrl Pts',(14.5805486486701,14.5921850016099,6.11599291589402));
#130983=CARTESIAN_POINT('Ctrl Pts',(14.5833259653237,14.5645732945172,6.09766382998459));
#130984=CARTESIAN_POINT('Ctrl Pts',(14.5861492876469,14.5381756402627,6.07749086301158));
#130985=CARTESIAN_POINT('Ctrl Pts',(14.5890250021544,14.5132372397542,6.05566640702311));
#130986=CARTESIAN_POINT('Ctrl Pts',(14.5919030643459,14.488278479964,6.0338241339238));
#130987=CARTESIAN_POINT('Ctrl Pts',(14.594833646003,14.4647813168602,6.01032776578187));
#130988=CARTESIAN_POINT('Ctrl Pts',(14.5977983330731,14.4429673372083,5.98539524459405));
#130989=CARTESIAN_POINT('Ctrl Pts',(14.6007644363182,14.4211429374295,5.96045081361087));
#130990=CARTESIAN_POINT('Ctrl Pts',(14.6037645148987,14.4010033938592,5.93406872166128));
#130991=CARTESIAN_POINT('Ctrl Pts',(14.6067561477313,14.3827462972326,5.90649259827256));
#130992=CARTESIAN_POINT('Ctrl Pts',(14.6097535849123,14.3644537782952,5.87886297185255));
#130993=CARTESIAN_POINT('Ctrl Pts',(14.6127420715505,14.3480513587491,5.85003428955134));
#130994=CARTESIAN_POINT('Ctrl Pts',(14.6156594784949,14.3337105588627,5.82028104282061));
#130995=CARTESIAN_POINT('Ctrl Pts',(14.6166958198584,14.3286163212775,5.80971188984606));
#130996=CARTESIAN_POINT('Ctrl Pts',(14.6177230509408,14.3237819537905,5.79902636994269));
#130997=CARTESIAN_POINT('Ctrl Pts',(14.6187380291237,14.319214131938,5.78823783860755));
#130998=CARTESIAN_POINT('Ctrl Pts',(14.6187392905008,14.3192084552189,5.78822443102196));
#130999=CARTESIAN_POINT('Ctrl Pts',(14.6187405518606,14.3192027789012,5.78821102325586));
#131000=CARTESIAN_POINT('Ctrl Pts',(14.6187418132029,14.3191971029851,5.78819761530927));
#131001=CARTESIAN_POINT('Ctrl Pts',(14.6199525060722,14.3137491045748,5.77532806779205));
#131002=CARTESIAN_POINT('Ctrl Pts',(14.6211471738604,14.3086710787256,5.76229203155521));
#131003=CARTESIAN_POINT('Ctrl Pts',(14.6223301869987,14.3039706982751,5.74911183949278));
#131004=CARTESIAN_POINT('Origin',(13.2437274406976,15.,5.5));
#131005=CARTESIAN_POINT('',(15.1006177988695,14.3042076755364,5.74898602614905));
#131006=CARTESIAN_POINT('',(15.0214324762185,14.3044236561645,5.74887185968306));
#131007=CARTESIAN_POINT('',(13.2437274406976,14.3042076641721,5.74898599439144));
#131008=CARTESIAN_POINT('Ctrl Pts',(15.1006178015771,14.3042076756101,5.74898602635499));
#131009=CARTESIAN_POINT('Ctrl Pts',(15.0992510192417,14.3099072116453,5.76491339980638));
#131010=CARTESIAN_POINT('Ctrl Pts',(15.0978904180461,14.3161552982477,5.78064972156567));
#131011=CARTESIAN_POINT('Ctrl Pts',(15.093390819992,14.3385505614446,5.83184683983702));
#131012=CARTESIAN_POINT('Ctrl Pts',(15.0902464920784,14.3569524182242,5.8662334633876));
#131013=CARTESIAN_POINT('Ctrl Pts',(15.0858797728196,14.3853466982996,5.91049808107278));
#131014=CARTESIAN_POINT('Ctrl Pts',(15.0847366692995,14.3930338554862,5.92178123176599));
#131015=CARTESIAN_POINT('Ctrl Pts',(15.0828203115642,14.4063039757117,5.9401444676008));
#131016=CARTESIAN_POINT('Ctrl Pts',(15.082053692695,14.4117121382454,5.94734717856612));
#131017=CARTESIAN_POINT('Ctrl Pts',(15.0805099531525,14.4227906268988,5.96155336360282));
#131018=CARTESIAN_POINT('Ctrl Pts',(15.0797329617558,14.4284600943739,5.9685555340117));
#131019=CARTESIAN_POINT('Ctrl Pts',(15.0777644185759,14.4430479769367,5.98591377213543));
#131020=CARTESIAN_POINT('Ctrl Pts',(15.0765665553399,14.4521278952372,5.99612886703441));
#131021=CARTESIAN_POINT('Ctrl Pts',(15.0716718426609,14.4900118650182,6.03644038352152));
#131022=CARTESIAN_POINT('Ctrl Pts',(15.0678855158728,14.5210490774347,6.06432354481301));
#131023=CARTESIAN_POINT('Ctrl Pts',(15.0612003791751,14.5791218903357,6.10823837756831));
#131024=CARTESIAN_POINT('Ctrl Pts',(15.0583260855716,14.6051452695217,6.12544557981788));
#131025=CARTESIAN_POINT('Ctrl Pts',(15.053961666409,14.6467939978574,6.14934620534783));
#131026=CARTESIAN_POINT('Ctrl Pts',(15.0524437184848,14.6616940170464,6.1572321888255));
#131027=CARTESIAN_POINT('Ctrl Pts',(15.0504128388405,14.6823065920435,6.16725458701378));
#131028=CARTESIAN_POINT('Ctrl Pts',(15.0498786775349,14.6877938167225,6.16983960168206));
#131029=CARTESIAN_POINT('Ctrl Pts',(15.048915078788,14.697820390212,6.17441310211501));
#131030=CARTESIAN_POINT('Ctrl Pts',(15.0484844380467,14.702349016998,6.17642401488885));
#131031=CARTESIAN_POINT('Ctrl Pts',(15.04755263282,14.7122550908629,6.18070399108053));
#131032=CARTESIAN_POINT('Ctrl Pts',(15.0470524775739,14.7176397343954,6.18295515495054));
#131033=CARTESIAN_POINT('Ctrl Pts',(15.0455391195859,14.7341209558929,6.1896172177964));
#131034=CARTESIAN_POINT('Ctrl Pts',(15.0445366597996,14.7452989279717,6.19382345416604));
#131035=CARTESIAN_POINT('Ctrl Pts',(15.0427771264441,14.7652920474885,6.20079841242744));
#131036=CARTESIAN_POINT('Ctrl Pts',(15.0420161564255,14.7740658742122,6.20367607948708));
#131037=CARTESIAN_POINT('Ctrl Pts',(15.0382466569616,14.8180405759767,6.21719168559805));
#131038=CARTESIAN_POINT('Ctrl Pts',(15.0353073111224,14.853948845698,6.22535684117382));
#131039=CARTESIAN_POINT('Ctrl Pts',(15.0292970284429,14.9276752155475,6.23642185235241));
#131040=CARTESIAN_POINT('Ctrl Pts',(15.0262329249709,14.9654027549854,6.23915523361877));
#131041=CARTESIAN_POINT('Ctrl Pts',(15.0220803935836,15.0151755727269,6.23894169353115));
#131042=CARTESIAN_POINT('Ctrl Pts',(15.0210710440379,15.0271768690993,6.23859766360036));
#131043=CARTESIAN_POINT('Ctrl Pts',(15.0193116929085,15.0478880541387,6.23749851625121));
#131044=CARTESIAN_POINT('Ctrl Pts',(15.0185660325591,15.0566030089313,6.2368808673125));
#131045=CARTESIAN_POINT('Ctrl Pts',(15.0170042035901,15.074712021765,6.23527430959483));
#131046=CARTESIAN_POINT('Ctrl Pts',(15.0161873673796,15.0841021043392,6.23425950078802));
#131047=CARTESIAN_POINT('Ctrl Pts',(15.0139680421021,15.1093804572255,6.2310363763011));
#131048=CARTESIAN_POINT('Ctrl Pts',(15.0125555061944,15.1252195258054,6.22849039262709));
#131049=CARTESIAN_POINT('Ctrl Pts',(15.0092925418075,15.1612085404964,6.22149719907432));
#131050=CARTESIAN_POINT('Ctrl Pts',(15.0074337210017,15.1812796098589,6.21671748540461));
#131051=CARTESIAN_POINT('Ctrl Pts',(15.0011466615815,15.2477916384619,6.19790580054746));
#131052=CARTESIAN_POINT('Ctrl Pts',(14.9966477496338,15.293045151734,6.18014518120771));
#131053=CARTESIAN_POINT('Ctrl Pts',(14.9907704098767,15.3506817466176,6.15069703538824));
#131054=CARTESIAN_POINT('Ctrl Pts',(14.9893100632424,15.3648863762643,6.14283929197273));
#131055=CARTESIAN_POINT('Ctrl Pts',(14.9873428381708,15.3839576946009,6.13145329586703));
#131056=CARTESIAN_POINT('Ctrl Pts',(14.9868162700791,15.3890562119405,6.12832479442541));
#131057=CARTESIAN_POINT('Ctrl Pts',(14.9858615664064,15.398295630209,6.12249979814702));
#131058=CARTESIAN_POINT('Ctrl Pts',(14.9854323194997,15.4024484581214,6.11982308186187));
#131059=CARTESIAN_POINT('Ctrl Pts',(14.984496571616,15.4115006876899,6.11385909198455));
#131060=CARTESIAN_POINT('Ctrl Pts',(14.9839911754329,15.4163880697629,6.11055448848179));
#131061=CARTESIAN_POINT('Ctrl Pts',(14.982442271807,15.431343765723,6.10017906118955));
#131062=CARTESIAN_POINT('Ctrl Pts',(14.9814102569868,15.4412761239467,6.09291465206659));
#131063=CARTESIAN_POINT('Ctrl Pts',(14.9795878417004,15.4586660316979,6.07951665669839));
#131064=CARTESIAN_POINT('Ctrl Pts',(14.9787935703072,15.4661931091757,6.07347893334562));
#131065=CARTESIAN_POINT('Ctrl Pts',(14.9747267846272,15.5043410016406,6.04163158898095));
#131066=CARTESIAN_POINT('Ctrl Pts',(14.971533592717,15.532946586586,6.01351039144344));
#131067=CARTESIAN_POINT('Ctrl Pts',(14.9655705428336,15.5812245369672,5.95764662982539));
#131068=CARTESIAN_POINT('Ctrl Pts',(14.9628201953718,15.6015336224318,5.93060333829186));
#131069=CARTESIAN_POINT('Ctrl Pts',(14.9590079457786,15.6263988334279,5.89228452967835));
#131070=CARTESIAN_POINT('Ctrl Pts',(14.9580070100405,15.632634900863,5.88214617647201));
#131071=CARTESIAN_POINT('Ctrl Pts',(14.9562572898702,15.643012038641,5.86432484568326));
#131072=CARTESIAN_POINT('Ctrl Pts',(14.9555127098893,15.647266975387,5.85671070026271));
#131073=CARTESIAN_POINT('Ctrl Pts',(14.9539483345668,15.6558656316758,5.84066293815921));
#131074=CARTESIAN_POINT('Ctrl Pts',(14.953127808438,15.6601836813751,5.83221747811366));
#131075=CARTESIAN_POINT('Ctrl Pts',(14.9508851247262,15.6714602597545,5.8090736727205));
#131076=CARTESIAN_POINT('Ctrl Pts',(14.9494525407782,15.6780976678559,5.79422589767985));
#131077=CARTESIAN_POINT('Ctrl Pts',(14.9461312656242,15.6921881055925,5.75969085902998));
#131078=CARTESIAN_POINT('Ctrl Pts',(14.9442337026044,15.6993003008116,5.73988048365984));
#131079=CARTESIAN_POINT('Ctrl Pts',(14.9390407927451,15.7162696363072,5.68540785215006));
#131080=CARTESIAN_POINT('Ctrl Pts',(14.9357166858559,15.7244533880979,5.65028415998758));
#131081=CARTESIAN_POINT('Ctrl Pts',(14.9300516487741,15.7340472126008,5.58922461006446));
#131082=CARTESIAN_POINT('Ctrl Pts',(14.9277039454842,15.7367145526301,5.56354777485325));
#131083=CARTESIAN_POINT('Ctrl Pts',(14.924738245076,15.7384195392994,5.53024193681021));
#131084=CARTESIAN_POINT('Ctrl Pts',(14.9240716807826,15.7386899669246,5.52269664285404));
#131085=CARTESIAN_POINT('Ctrl Pts',(14.9229775170635,15.7389462435518,5.51019679462352));
#131086=CARTESIAN_POINT('Ctrl Pts',(14.9225466509125,15.7389979899954,5.50524434465818));
#131087=CARTESIAN_POINT('Ctrl Pts',(14.9216294637016,15.739002173277,5.49463281922514));
#131088=CARTESIAN_POINT('Ctrl Pts',(14.9211439399876,15.7389394133532,5.48897418326743));
#131089=CARTESIAN_POINT('Ctrl Pts',(14.9197266671525,15.7385640535688,5.47235172032866));
#131090=CARTESIAN_POINT('Ctrl Pts',(14.9188037579985,15.7380723662661,5.46139288454181));
#131091=CARTESIAN_POINT('Ctrl Pts',(14.9172097835843,15.7367896290749,5.44230559996862));
#131092=CARTESIAN_POINT('Ctrl Pts',(14.9165348536471,15.7361075475423,5.43417225694721));
#131093=CARTESIAN_POINT('Ctrl Pts',(14.9134330119992,15.732332784988,5.39663871326985));
#131094=CARTESIAN_POINT('Ctrl Pts',(14.9110545810954,15.7276123261766,5.36742765655907));
#131095=CARTESIAN_POINT('Ctrl Pts',(14.9051455899846,15.7115780966835,5.29579546764514));
#131096=CARTESIAN_POINT('Ctrl Pts',(14.9016211370708,15.6982155625316,5.25395679469438));
#131097=CARTESIAN_POINT('Ctrl Pts',(14.8968449257441,15.6759171420462,5.20092713878095));
#131098=CARTESIAN_POINT('Ctrl Pts',(14.895698249951,15.6702591044545,5.18845346430624));
#131099=CARTESIAN_POINT('Ctrl Pts',(14.8937776356104,15.6603076549552,5.16804207528852));
#131100=CARTESIAN_POINT('Ctrl Pts',(14.8930103972369,15.6562094111272,5.16001256416301));
#131101=CARTESIAN_POINT('Ctrl Pts',(14.891466742981,15.6477273766923,5.14411901902167));
#131102=CARTESIAN_POINT('Ctrl Pts',(14.8906904739429,15.6433447131643,5.13625614568605));
#131103=CARTESIAN_POINT('Ctrl Pts',(14.8887265447247,15.631971503005,5.1167004122829));
#131104=CARTESIAN_POINT('Ctrl Pts',(14.8875326364623,15.6247995277899,5.10511767440195));
#131105=CARTESIAN_POINT('Ctrl Pts',(14.8829024114174,15.5960280780468,5.06139939738936));
#131106=CARTESIAN_POINT('Ctrl Pts',(14.8793905681541,15.5722390326687,5.03078628246848));
#131107=CARTESIAN_POINT('Ctrl Pts',(14.8714493562617,15.5139144050625,4.96679721108965));
#131108=CARTESIAN_POINT('Ctrl Pts',(14.8670153539851,15.4782980048915,4.93462846425949));
#131109=CARTESIAN_POINT('Ctrl Pts',(14.8620152896383,15.4332247839639,4.90124747843356));
#131110=CARTESIAN_POINT('Ctrl Pts',(14.8612894015299,15.4265511590456,4.89647500314726));
#131111=CARTESIAN_POINT('Ctrl Pts',(14.8601659878828,15.4160034152996,4.88919444258697));
#131112=CARTESIAN_POINT('Ctrl Pts',(14.8597638784543,15.4121832036215,4.88661000914633));
#131113=CARTESIAN_POINT('Ctrl Pts',(14.8589076036269,15.4039478996683,4.88115038249094));
#131114=CARTESIAN_POINT('Ctrl Pts',(14.8584541901416,15.3995257025552,4.87828626110608));
#131115=CARTESIAN_POINT('Ctrl Pts',(14.857235676925,15.3874850252007,4.87066942366231));
#131116=CARTESIAN_POINT('Ctrl Pts',(14.8564760283747,15.3798096278646,4.86600765919918));
#131117=CARTESIAN_POINT('Ctrl Pts',(14.8532053519795,15.346111501072,4.84637234661793));
#131118=CARTESIAN_POINT('Ctrl Pts',(14.8507639365229,15.3192719560999,4.8328507165758));
#131119=CARTESIAN_POINT('Ctrl Pts',(14.8436848422111,15.238730209886,4.79825214950862));
#131120=CARTESIAN_POINT('Ctrl Pts',(14.8391010405225,15.1833068241211,4.78178001955737));
#131121=CARTESIAN_POINT('Ctrl Pts',(14.8332617275527,15.1142502652122,4.76977855293323));
#131122=CARTESIAN_POINT('Ctrl Pts',(14.8322146395045,15.1019137678445,4.76795489789314));
#131123=CARTESIAN_POINT('Ctrl Pts',(14.8304190098092,15.0808828638724,4.76538786728927));
#131124=CARTESIAN_POINT('Ctrl Pts',(14.8296755231385,15.0722103624063,4.76448475684657));
#131125=CARTESIAN_POINT('Ctrl Pts',(14.8281321975413,15.0542953182335,4.7629390618583));
#131126=CARTESIAN_POINT('Ctrl Pts',(14.8273318797121,15.0450526610542,4.762316430449));
#131127=CARTESIAN_POINT('Ctrl Pts',(14.8252163923668,15.0207618563589,4.76113826802042));
#131128=CARTESIAN_POINT('Ctrl Pts',(14.8238927955329,15.0057050106242,4.76086868905633));
#131129=CARTESIAN_POINT('Ctrl Pts',(14.8216616481105,14.9805807351554,4.76118653886527));
#131130=CARTESIAN_POINT('Ctrl Pts',(14.8207616595112,14.9705140477882,4.76151980568802));
#131131=CARTESIAN_POINT('Ctrl Pts',(14.8170055679276,14.9287816844488,4.76375601331087));
#131132=CARTESIAN_POINT('Ctrl Pts',(14.8141056028554,14.8972509648339,4.76749095783466));
#131133=CARTESIAN_POINT('Ctrl Pts',(14.8074490882703,14.8260082037432,4.78062071078683));
#131134=CARTESIAN_POINT('Ctrl Pts',(14.8036925335516,14.7866306668265,4.79130130157021));
#131135=CARTESIAN_POINT('Ctrl Pts',(14.7992634750848,14.7400177224675,4.80818471390117));
#131136=CARTESIAN_POINT('Ctrl Pts',(14.7984796360593,14.7317587105458,4.81134492898591));
#131137=CARTESIAN_POINT('Ctrl Pts',(14.7972435464586,14.7186978911827,4.81661315076737));
#131138=CARTESIAN_POINT('Ctrl Pts',(14.7967863301209,14.7138586603227,4.81862521212996));
#131139=CARTESIAN_POINT('Ctrl Pts',(14.7958741744206,14.7041819487624,4.82276988969222));
#131140=CARTESIAN_POINT('Ctrl Pts',(14.7954193076996,14.6993451344094,4.82490326694368));
#131141=CARTESIAN_POINT('Ctrl Pts',(14.7941920506198,14.6862763713661,4.83083583997955));
#131142=CARTESIAN_POINT('Ctrl Pts',(14.7934252455913,14.6780904203679,4.83473506488145));
#131143=CARTESIAN_POINT('Ctrl Pts',(14.7900854204252,14.6424452533595,4.85252607832617));
#131144=CARTESIAN_POINT('Ctrl Pts',(14.7875854670921,14.6157942225327,4.86797603600287));
#131145=CARTESIAN_POINT('Ctrl Pts',(14.7805574299694,14.5433417190661,4.91625987728089));
#131146=CARTESIAN_POINT('Ctrl Pts',(14.7760759011876,14.5002268733635,4.95272007232085));
#131147=CARTESIAN_POINT('Ctrl Pts',(14.7703358473794,14.4529976668205,5.00293896231947));
#131148=CARTESIAN_POINT('Ctrl Pts',(14.7692734165035,14.4445646180919,5.01238055271503));
#131149=CARTESIAN_POINT('Ctrl Pts',(14.7674598890912,14.4307200842893,5.02870612011047));
#131150=CARTESIAN_POINT('Ctrl Pts',(14.7667141064142,14.4251807116233,5.03547840158619));
#131151=CARTESIAN_POINT('Ctrl Pts',(14.7651733044624,14.4140597555829,5.04957814663552));
#131152=CARTESIAN_POINT('Ctrl Pts',(14.7643779002494,14.4084923603415,5.05691478079476));
#131153=CARTESIAN_POINT('Ctrl Pts',(14.762293224762,14.3943593622559,5.07628023475415));
#131154=CARTESIAN_POINT('Ctrl Pts',(14.760995986419,14.3860150780933,5.08846449791527));
#131155=CARTESIAN_POINT('Ctrl Pts',(14.7561136104232,14.3562991326642,5.13477266536349));
#131156=CARTESIAN_POINT('Ctrl Pts',(14.7524493425166,14.3373649994363,5.17037038815118));
#131157=CARTESIAN_POINT('Ctrl Pts',(14.7447968048354,14.3043652520063,5.24688155283492));
#131158=CARTESIAN_POINT('Ctrl Pts',(14.7408178834751,14.2907947303222,5.28785574283835));
#131159=CARTESIAN_POINT('Ctrl Pts',(14.736192517651,14.2788643549322,5.33825866313483));
#131160=CARTESIAN_POINT('Ctrl Pts',(14.7354205617058,14.2770078333285,5.34677067440099));
#131161=CARTESIAN_POINT('Ctrl Pts',(14.7341985789747,14.2742812896801,5.36042729313339));
#131162=CARTESIAN_POINT('Ctrl Pts',(14.7337437689779,14.2733145257646,5.36555144270778));
#131163=CARTESIAN_POINT('Ctrl Pts',(14.7328315984357,14.2714720138729,5.37591849172053));
#131164=CARTESIAN_POINT('Ctrl Pts',(14.7323743675612,14.270598430403,5.38116144121119));
#131165=CARTESIAN_POINT('Ctrl Pts',(14.7311327947591,14.2683660998827,5.39551253755506));
#131166=CARTESIAN_POINT('Ctrl Pts',(14.7303542612193,14.2671208402391,5.40463776989514));
#131167=CARTESIAN_POINT('Ctrl Pts',(14.7268976941268,14.2623081944379,5.44560789898914));
#131168=CARTESIAN_POINT('Ctrl Pts',(14.7242987576568,14.2606431863995,5.47764505514616));
#131169=CARTESIAN_POINT('Ctrl Pts',(14.7173492325736,14.2617732229955,5.56379314414781));
#131170=CARTESIAN_POINT('Ctrl Pts',(14.713034583888,14.2684215434994,5.61764566060312));
#131171=CARTESIAN_POINT('Ctrl Pts',(14.7074566166424,14.2838714680731,5.68288972529384));
#131172=CARTESIAN_POINT('Ctrl Pts',(14.7063703933084,14.2871863070076,5.69541065369431));
#131173=CARTESIAN_POINT('Ctrl Pts',(14.7045289722822,14.2933021330107,5.71627876396466));
#131174=CARTESIAN_POINT('Ctrl Pts',(14.7037794966573,14.2959264866741,5.72467499328519));
#131175=CARTESIAN_POINT('Ctrl Pts',(14.7025423363583,14.3004750904483,5.73836441285612));
#131176=CARTESIAN_POINT('Ctrl Pts',(14.7020575832709,14.3023111167124,5.74368608509744));
#131177=CARTESIAN_POINT('Ctrl Pts',(14.7015708502323,14.3042076642463,5.74898599459905));
#131178=CARTESIAN_POINT('',(14.643302331303,14.2612458317818,5.50031209173545));
#131179=CARTESIAN_POINT('Ctrl Pts',(14.6223301870619,14.3039706980243,5.74911183878948));
#131180=CARTESIAN_POINT('Ctrl Pts',(14.6250909116188,14.2930017110506,5.71835404013125));
#131181=CARTESIAN_POINT('Ctrl Pts',(14.6277888702942,14.2840924867556,5.68681257433633));
#131182=CARTESIAN_POINT('Ctrl Pts',(14.6304768935317,14.2773101411995,5.65476687587751));
#131183=CARTESIAN_POINT('Ctrl Pts',(14.6307891739804,14.2765222038469,5.65104397461897));
#131184=CARTESIAN_POINT('Ctrl Pts',(14.6311013203347,14.2757629754969,5.64731432574451));
#131185=CARTESIAN_POINT('Ctrl Pts',(14.6314134154308,14.2750325620636,5.64357841300164));
#131186=CARTESIAN_POINT('Ctrl Pts',(14.6343937879807,14.2680574311685,5.60790206970437));
#131187=CARTESIAN_POINT('Ctrl Pts',(14.6373704162079,14.2637087182105,5.57164788306008));
#131188=CARTESIAN_POINT('Ctrl Pts',(14.6403957909006,14.2620332555201,5.53519586439941));
#131189=CARTESIAN_POINT('Ctrl Pts',(14.6413595316584,14.2614995326438,5.52358398168926));
#131190=CARTESIAN_POINT('Ctrl Pts',(14.6423280172788,14.2612367984457,5.51195198761351));
#131191=CARTESIAN_POINT('Ctrl Pts',(14.643302331268,14.2612458317815,5.50031209215397));
#131192=CARTESIAN_POINT('Ctrl Pts',(14.6433023313447,14.2612458317821,5.50031209123629));
#131193=CARTESIAN_POINT('Ctrl Pts',(14.6461222215263,14.2612719763879,5.46662353982884));
#131194=CARTESIAN_POINT('Ctrl Pts',(14.6489879456295,14.2635801106923,5.4329480764385));
#131195=CARTESIAN_POINT('Ctrl Pts',(14.651906822104,14.268136916162,5.3996050731548));
#131196=CARTESIAN_POINT('Ctrl Pts',(14.6548299420279,14.272700346295,5.36621359596372));
#131197=CARTESIAN_POINT('Ctrl Pts',(14.6578064047676,14.2795188773573,5.3331554877905));
#131198=CARTESIAN_POINT('Ctrl Pts',(14.6608172228768,14.2885259866646,5.30074347405539));
#131199=CARTESIAN_POINT('Ctrl Pts',(14.6638305628729,14.2975406404034,5.26830431174162));
#131200=CARTESIAN_POINT('Ctrl Pts',(14.666878138236,14.3087477111867,5.23651223112942));
#131201=CARTESIAN_POINT('Ctrl Pts',(14.669915552554,14.3220470860818,5.20567390799831));
#131202=CARTESIAN_POINT('Ctrl Pts',(14.6729599034648,14.3353768329773,5.17476515888329));
#131203=CARTESIAN_POINT('Ctrl Pts',(14.6759935383719,14.3508090333046,5.14481454070596));
#131204=CARTESIAN_POINT('Ctrl Pts',(14.6789512632767,14.3682037596851,5.11612483749924));
#131205=CARTESIAN_POINT('Ctrl Pts',(14.6798666873083,14.3735874755691,5.10724529507469));
#131206=CARTESIAN_POINT('Ctrl Pts',(14.6807747262521,14.3791588651593,5.09848649185438));
#131207=CARTESIAN_POINT('Ctrl Pts',(14.6816732068274,14.384912854012,5.08985725627272));
#131208=CARTESIAN_POINT('Ctrl Pts',(14.6816744645226,14.3849209084587,5.08984517704912));
#131209=CARTESIAN_POINT('Ctrl Pts',(14.6816757222009,14.3849289632781,5.0898330980551));
#131210=CARTESIAN_POINT('Ctrl Pts',(14.6816769798624,14.3849370184703,5.08982101929069));
#131211=CARTESIAN_POINT('Ctrl Pts',(14.6842658152184,14.4015182417089,5.06495746740496));
#131212=CARTESIAN_POINT('Ctrl Pts',(14.6867833984792,14.4196830520397,5.04106536422739));
#131213=CARTESIAN_POINT('Ctrl Pts',(14.6892706941656,14.4392791137363,5.01834216308987));
#131214=CARTESIAN_POINT('Ctrl Pts',(14.6895272679287,14.4413005200847,5.01599818072507));
#131215=CARTESIAN_POINT('Ctrl Pts',(14.6897835194112,14.4433371121714,5.01366664954593));
#131216=CARTESIAN_POINT('Ctrl Pts',(14.6900394935768,14.4453886924276,5.01134779444572));
#131217=CARTESIAN_POINT('Ctrl Pts',(14.6927738171437,14.4673037330717,4.98657771605502));
#131218=CARTESIAN_POINT('Ctrl Pts',(14.6954773345768,14.4909342492166,4.96325204878176));
#131219=CARTESIAN_POINT('Ctrl Pts',(14.6981970141438,14.5160420502934,4.94159332122161));
#131220=CARTESIAN_POINT('Ctrl Pts',(14.7009138917455,14.5411239839168,4.91995690768748));
#131221=CARTESIAN_POINT('Ctrl Pts',(14.7036473786631,14.5676796812181,4.89998369340697));
#131222=CARTESIAN_POINT('Ctrl Pts',(14.7064266813217,14.5954507124083,4.88185734650776));
#131223=CARTESIAN_POINT('Ctrl Pts',(14.7092046604926,14.6232085191957,4.86373963126901));
#131224=CARTESIAN_POINT('Ctrl Pts',(14.7120286365145,14.6521802637181,4.84746681569434));
#131225=CARTESIAN_POINT('Ctrl Pts',(14.7149049737545,14.6820921812796,4.83318807667209));
#131226=CARTESIAN_POINT('Ctrl Pts',(14.717783664302,14.7120285716119,4.81889765533942));
#131227=CARTESIAN_POINT('Ctrl Pts',(14.7207148433939,14.7429066065502,4.80660450113035));
#131228=CARTESIAN_POINT('Ctrl Pts',(14.7236800711917,14.7744383906408,4.79642600147313));
#131229=CARTESIAN_POINT('Ctrl Pts',(14.7266467191728,14.8059852767468,4.78624262686631));
#131230=CARTESIAN_POINT('Ctrl Pts',(14.729647285496,14.8381866381599,4.77817604580261));
#131231=CARTESIAN_POINT('Ctrl Pts',(14.7326393224649,14.870740464133,4.77231145050326));
#131232=CARTESIAN_POINT('Ctrl Pts',(14.7356371621703,14.9033574247787,4.76643548144697));
#131233=CARTESIAN_POINT('Ctrl Pts',(14.7386259667064,14.9363284394209,4.76277051413231));
#131234=CARTESIAN_POINT('Ctrl Pts',(14.7415435871632,14.9693334407004,4.76136558621512));
#131235=CARTESIAN_POINT('Ctrl Pts',(14.7425759365491,14.9810116878562,4.7608684768433));
#131236=CARTESIAN_POINT('Ctrl Pts',(14.7435992340124,14.992694024955,4.7606539473331));
#131237=CARTESIAN_POINT('Ctrl Pts',(14.7446103736317,15.004365714554,4.76072284074558));
#131238=CARTESIAN_POINT('Ctrl Pts',(14.7446116328997,15.0043802504156,4.76072292654508));
#131239=CARTESIAN_POINT('Ctrl Pts',(14.7446128921509,15.0043947862905,4.76072301278323));
#131240=CARTESIAN_POINT('Ctrl Pts',(14.7446141513852,15.0044093221786,4.76072309946007));
#131241=CARTESIAN_POINT('Ctrl Pts',(14.7472028424028,15.0342917063171,4.76090128674805));
#131242=CARTESIAN_POINT('Ctrl Pts',(14.749720259795,15.0642334838074,4.76293605499652));
#131243=CARTESIAN_POINT('Ctrl Pts',(14.7522073680622,15.0939860074293,4.76680875635777));
#131244=CARTESIAN_POINT('Ctrl Pts',(14.7524640214252,15.0970562739498,4.76720839389724));
#131245=CARTESIAN_POINT('Ctrl Pts',(14.7527203520295,15.1001244899583,4.76762757411392));
#131246=CARTESIAN_POINT('Ctrl Pts',(14.7529764048909,15.1031903586769,4.76806625561962));
#131247=CARTESIAN_POINT('Ctrl Pts',(14.7557106121156,15.1359286001261,4.772750624838));
#131248=CARTESIAN_POINT('Ctrl Pts',(14.7584139868398,15.1684037434545,4.77966192216373));
#131249=CARTESIAN_POINT('Ctrl Pts',(14.76113350607,15.2002989631679,4.78872357659478));
#131250=CARTESIAN_POINT('Ctrl Pts',(14.7638502211033,15.2321612945413,4.797775887219));
#131251=CARTESIAN_POINT('Ctrl Pts',(14.7665835278909,15.2634448910942,4.80897355353244));
#131252=CARTESIAN_POINT('Ctrl Pts',(14.7693626433398,15.2938542563831,4.82220172931195));
#131253=CARTESIAN_POINT('Ctrl Pts',(14.7721404332908,15.3242491179393,4.83542359591917));
#131254=CARTESIAN_POINT('Ctrl Pts',(14.7749642129968,15.3537706252292,4.85067372086793));
#131255=CARTESIAN_POINT('Ctrl Pts',(14.7778403583777,15.3821436590195,4.86780548236156));
#131256=CARTESIAN_POINT('Ctrl Pts',(14.7807188549676,15.4105398873713,4.88495124883253));
#131257=CARTESIAN_POINT('Ctrl Pts',(14.7836498445575,15.4377857881248,4.90398163250348));
#131258=CARTESIAN_POINT('Ctrl Pts',(14.7866148992793,15.4636250257334,4.92472072884242));
#131259=CARTESIAN_POINT('Ctrl Pts',(14.7895813727922,15.4894766275264,4.9454697489265));
#131260=CARTESIAN_POINT('Ctrl Pts',(14.7925817811825,15.5139201802209,4.96792926253701));
#131261=CARTESIAN_POINT('Ctrl Pts',(14.795573687835,15.536718479835,4.99189387462251));
#131262=CARTESIAN_POINT('Ctrl Pts',(14.7985713967506,15.5595609926378,5.01590496174929));
#131263=CARTESIAN_POINT('Ctrl Pts',(14.8015600984603,15.5807515967063,5.0414274316669));
#131264=CARTESIAN_POINT('Ctrl Pts',(14.8044776515932,15.600073358392,5.06822093313735));
#131265=CARTESIAN_POINT('Ctrl Pts',(14.8055108580628,15.6069158624593,5.07770943867687));
#131266=CARTESIAN_POINT('Ctrl Pts',(14.8065350015697,15.6135242123974,5.08735700333458));
#131267=CARTESIAN_POINT('Ctrl Pts',(14.8075469683162,15.6198895788537,5.09715175176511));
#131268=CARTESIAN_POINT('Ctrl Pts',(14.8075482276661,15.6198975002832,5.09716394091554));
#131269=CARTESIAN_POINT('Ctrl Pts',(14.807549486999,15.6199054213535,5.09717613031826));
#131270=CARTESIAN_POINT('Ctrl Pts',(14.8075507463151,15.6199133420647,5.09718831997327));
#131271=CARTESIAN_POINT('Ctrl Pts',(14.8101395146416,15.6361958990002,5.12224651832175));
#131272=CARTESIAN_POINT('Ctrl Pts',(14.8126570102922,15.6509602865276,5.14837519478572));
#131273=CARTESIAN_POINT('Ctrl Pts',(14.8151441952392,15.6640853653416,5.17535639746759));
#131274=CARTESIAN_POINT('Ctrl Pts',(14.8154008763878,15.6654398927999,5.17814089730997));
#131275=CARTESIAN_POINT('Ctrl Pts',(14.8156572347108,15.6667769658503,5.18093443154027));
#131276=CARTESIAN_POINT('Ctrl Pts',(14.8159133152318,15.6680964558547,5.18373672943679));
#131277=CARTESIAN_POINT('Ctrl Pts',(14.8186476274682,15.682185374649,5.21365840172559));
#131278=CARTESIAN_POINT('Ctrl Pts',(14.8213511049492,15.6942694172094,5.24458482483895));
#131279=CARTESIAN_POINT('Ctrl Pts',(14.8240707235769,15.7042383377209,5.27620924200535));
#131280=CARTESIAN_POINT('Ctrl Pts',(14.8267875391592,15.7141969835058,5.30780106464581));
#131281=CARTESIAN_POINT('Ctrl Pts',(14.8295209432087,15.7220453368245,5.34008912491049));
#131282=CARTESIAN_POINT('Ctrl Pts',(14.8323001516207,15.7277168506456,5.37276343803394));
#131283=CARTESIAN_POINT('Ctrl Pts',(14.8350780355032,15.7333856615076,5.40542217906488));
#131284=CARTESIAN_POINT('Ctrl Pts',(14.8379019049028,15.7368799939699,5.43846666805591));
#131285=CARTESIAN_POINT('Ctrl Pts',(14.8407781342237,15.7381710464651,5.47158647040787));
#131286=CARTESIAN_POINT('Ctrl Pts',(14.8436567153987,15.7394631546366,5.50473335437838));
#131287=CARTESIAN_POINT('Ctrl Pts',(14.8465877838303,15.738548472643,5.5379556420415));
#131288=CARTESIAN_POINT('Ctrl Pts',(14.8495529094249,15.7354329855916,5.5709424875009));
#131289=CARTESIAN_POINT('Ctrl Pts',(14.852519454302,15.7323160072859,5.60394512239376));
#131290=CARTESIAN_POINT('Ctrl Pts',(14.855519926056,15.7269959735091,5.63671213662848));
#131291=CARTESIAN_POINT('Ctrl Pts',(14.8585118853793,15.7195140212916,5.66893244798056));
#131292=CARTESIAN_POINT('Ctrl Pts',(14.8615096464463,15.7120175607319,5.70121523811967));
#131293=CARTESIAN_POINT('Ctrl Pts',(14.8644983894872,15.7023502733526,5.73294922160899));
#131294=CARTESIAN_POINT('Ctrl Pts',(14.8674159709196,15.6905936409715,5.76382102498956));
#131295=CARTESIAN_POINT('Ctrl Pts',(14.8684485235098,15.6864328860796,5.77474677334788));
#131296=CARTESIAN_POINT('Ctrl Pts',(14.8694720231491,15.6820108469657,5.78556452871274));
#131297=CARTESIAN_POINT('Ctrl Pts',(14.8704833620264,15.6773325782012,5.79626041244684));
#131298=CARTESIAN_POINT('Ctrl Pts',(14.8704846209158,15.6773267548089,5.79627372641619));
#131299=CARTESIAN_POINT('Ctrl Pts',(14.8704858797884,15.6773209310087,5.7962870402244));
#131300=CARTESIAN_POINT('Ctrl Pts',(14.8704871386441,15.6773151068005,5.79630035387143));
#131301=CARTESIAN_POINT('Ctrl Pts',(14.8730759013494,15.6653379653543,5.82367908580836));
#131302=CARTESIAN_POINT('Ctrl Pts',(14.8755933965129,15.6516319005856,5.85037835679467));
#131303=CARTESIAN_POINT('Ctrl Pts',(14.8780805875388,15.6363123514682,5.87617713629024));
#131304=CARTESIAN_POINT('Ctrl Pts',(14.8783372320461,15.6347315809945,5.87883922174531));
#131305=CARTESIAN_POINT('Ctrl Pts',(14.8785935538916,15.6331336718161,5.88149169853617));
#131306=CARTESIAN_POINT('Ctrl Pts',(14.8788495980807,15.6315187792568,5.88413431046347));
#131307=CARTESIAN_POINT('Ctrl Pts',(14.8815838816912,15.6142734190979,5.91235463644495));
#131308=CARTESIAN_POINT('Ctrl Pts',(14.8842873387627,15.5950864649871,5.93945286103092));
#131309=CARTESIAN_POINT('Ctrl Pts',(14.8870069435193,15.5741535137537,5.96516823149236));
#131310=CARTESIAN_POINT('Ctrl Pts',(14.8897237451682,15.5532421381983,5.99085709701695));
#131311=CARTESIAN_POINT('Ctrl Pts',(14.8924571417644,15.5305888881882,6.01516617657772));
#131312=CARTESIAN_POINT('Ctrl Pts',(14.8952363470137,15.5064160849056,6.0378694409836));
#131313=CARTESIAN_POINT('Ctrl Pts',(14.8980142277164,15.4822548021852,6.06056188519767));
#131314=CARTESIAN_POINT('Ctrl Pts',(14.9008380981967,15.4565756861741,6.08165020872348));
#131315=CARTESIAN_POINT('Ctrl Pts',(14.9037143306719,15.4296221887639,6.10093966148744));
#131316=CARTESIAN_POINT('Ctrl Pts',(14.9065929151896,15.4026466500983,6.120244888225));
#131317=CARTESIAN_POINT('Ctrl Pts',(14.9095239890321,15.3743947243384,6.13774836173002));
#131318=CARTESIAN_POINT('Ctrl Pts',(14.9124891202093,15.3451293350402,6.1532841613303));
#131319=CARTESIAN_POINT('Ctrl Pts',(14.9154556707582,15.3158499367599,6.1688273977269));
#131320=CARTESIAN_POINT('Ctrl Pts',(14.9184561483448,15.2855559865514,6.18240098230982));
#131321=CARTESIAN_POINT('Ctrl Pts',(14.9214481122626,15.2545299341904,6.19386822545329));
#131322=CARTESIAN_POINT('Ctrl Pts',(14.924445878342,15.2234437146039,6.2053577064308));
#131323=CARTESIAN_POINT('Ctrl Pts',(14.9274346251376,15.1916222515561,6.21473224791747));
#131324=CARTESIAN_POINT('Ctrl Pts',(14.9303522083298,15.1593720926524,6.22188759901106));
#131325=CARTESIAN_POINT('Ctrl Pts',(14.9313849042293,15.1479569573624,6.22442027802899));
#131326=CARTESIAN_POINT('Ctrl Pts',(14.9324085444352,15.1364883406239,6.22667526330663));
#131327=CARTESIAN_POINT('Ctrl Pts',(14.9334200198331,15.124980619804,6.22864914415783));
#131328=CARTESIAN_POINT('Ctrl Pts',(14.9334212789608,15.1249662945023,6.2286516013289));
#131329=CARTESIAN_POINT('Ctrl Pts',(14.9334225380716,15.1249519691109,6.22865405807048));
#131330=CARTESIAN_POINT('Ctrl Pts',(14.9334237971656,15.1249376436298,6.22865651438255));
#131331=CARTESIAN_POINT('Ctrl Pts',(14.9360125426822,15.0954839052033,6.23370678617647));
#131332=CARTESIAN_POINT('Ctrl Pts',(14.9385300175094,15.065647035084,6.2369393898572));
#131333=CARTESIAN_POINT('Ctrl Pts',(14.9410171849092,15.0356751200762,6.23832921061113));
#131334=CARTESIAN_POINT('Ctrl Pts',(14.9412738427776,15.0325822330357,6.23847263016231));
#131335=CARTESIAN_POINT('Ctrl Pts',(14.9415301779094,15.0294879476791,6.23859644903481));
#131336=CARTESIAN_POINT('Ctrl Pts',(14.9417862353182,15.0263925634539,6.23870065608836));
#131337=CARTESIAN_POINT('Ctrl Pts',(14.9445205074269,14.9933389494504,6.23981341607999));
#131338=CARTESIAN_POINT('Ctrl Pts',(14.9472239489535,14.9601549780845,6.23868746473644));
#131339=CARTESIAN_POINT('Ctrl Pts',(14.9499435353598,14.9271659939967,6.23534279795633));
#131340=CARTESIAN_POINT('Ctrl Pts',(14.9526603183903,14.8942110152714,6.23200157889094));
#131341=CARTESIAN_POINT('Ctrl Pts',(14.9553936935767,14.8614507279703,6.2264467753758));
#131342=CARTESIAN_POINT('Ctrl Pts',(14.958172876127,14.8291961681283,6.21873979836838));
#131343=CARTESIAN_POINT('Ctrl Pts',(14.9609507338853,14.7969569835211,6.21103649515415));
#131344=CARTESIAN_POINT('Ctrl Pts',(14.9637745801328,14.7652230567194,6.20118338718233));
#131345=CARTESIAN_POINT('Ctrl Pts',(14.9666507887204,14.7342909163415,6.18927673425501));
#131346=CARTESIAN_POINT('Ctrl Pts',(14.9695293490742,14.7033334839295,6.17736034571067));
#131347=CARTESIAN_POINT('Ctrl Pts',(14.9724603990982,14.673179142556,6.1633871523955));
#131348=CARTESIAN_POINT('Ctrl Pts',(14.9754255084587,14.6441110472132,6.14748553004897));
#131349=CARTESIAN_POINT('Ctrl Pts',(14.9783920370114,14.6150290389907,6.13157629669957));
#131350=CARTESIAN_POINT('Ctrl Pts',(14.981392494618,14.5870343302754,6.11373663792384));
#131351=CARTESIAN_POINT('Ctrl Pts',(14.9843844420708,14.5603963968804,6.09412731152478));
#131352=CARTESIAN_POINT('Ctrl Pts',(14.9873821915862,14.5337068065101,6.07447995820843));
#131353=CARTESIAN_POINT('Ctrl Pts',(14.9903709253773,14.50837944566,6.05305558592979));
#131354=CARTESIAN_POINT('Ctrl Pts',(14.9932885001231,14.4846699455329,6.03005291635318));
#131355=CARTESIAN_POINT('Ctrl Pts',(14.9943212873573,14.4762770606222,6.02191024116567));
#131356=CARTESIAN_POINT('Ctrl Pts',(14.9953450178091,14.4680867496832,6.01357016871636));
#131357=CARTESIAN_POINT('Ctrl Pts',(14.9963565815236,14.4601097698342,6.00504283513605));
#131358=CARTESIAN_POINT('Ctrl Pts',(14.9963578406379,14.4600998407223,6.00503222098741));
#131359=CARTESIAN_POINT('Ctrl Pts',(14.9963590997355,14.4600899119181,6.00502160652613));
#131360=CARTESIAN_POINT('Ctrl Pts',(14.9963603588163,14.4600799834219,6.00501099175224));
#131361=CARTESIAN_POINT('Ctrl Pts',(14.9989264199637,14.4398452791334,5.98337762402734));
#131362=CARTESIAN_POINT('Ctrl Pts',(15.0014230133456,14.4208889613002,5.96044138623255));
#131363=CARTESIAN_POINT('Ctrl Pts',(15.0038897946441,14.4033688781723,5.93639150010391));
#131364=CARTESIAN_POINT('Ctrl Pts',(15.0041351714271,14.401626112554,5.9339991989736));
#131365=CARTESIAN_POINT('Ctrl Pts',(15.0043802532264,14.3998975597837,5.93159592106345));
#131366=CARTESIAN_POINT('Ctrl Pts',(15.0046250790734,14.3981833754518,5.92918188070301));
#131367=CARTESIAN_POINT('Ctrl Pts',(15.007427460399,14.3785620886504,5.90154974255911));
#131368=CARTESIAN_POINT('Ctrl Pts',(15.0101972648971,14.3608230937688,5.87250150924527));
#131369=CARTESIAN_POINT('Ctrl Pts',(15.0129847378888,14.3451451873103,5.84234467510009));
#131370=CARTESIAN_POINT('Ctrl Pts',(15.0157722078083,14.3294672981314,5.81218787419279));
#131371=CARTESIAN_POINT('Ctrl Pts',(15.0185779004322,14.315850069152,5.78092297439461));
#131372=CARTESIAN_POINT('Ctrl Pts',(15.0214324762185,14.3044236561645,5.74887185968306));
#131373=CARTESIAN_POINT('Origin',(13.2437274406976,15.,5.5));
#131374=CARTESIAN_POINT('',(15.5006844331709,14.3042076643853,5.74898599498742));
#131375=CARTESIAN_POINT('',(15.4218039449815,14.3042130191175,5.74898305899437));
#131376=CARTESIAN_POINT('',(13.2437274406976,14.3042076641721,5.74898599439144));
#131377=CARTESIAN_POINT('Ctrl Pts',(15.5006844331709,14.3042076645986,5.7489859955834));
#131378=CARTESIAN_POINT('Ctrl Pts',(15.4981861316207,14.3133756656007,5.77460601012787));
#131379=CARTESIAN_POINT('Ctrl Pts',(15.4956999505869,14.323953135999,5.7997040624191));
#131380=CARTESIAN_POINT('Ctrl Pts',(15.4924749873236,14.3397861202763,5.83214063832067));
#131381=CARTESIAN_POINT('Ctrl Pts',(15.4916880923997,14.3438229318855,5.84004624332186));
#131382=CARTESIAN_POINT('Ctrl Pts',(15.4904483724183,14.3504715583388,5.85250721549171));
#131383=CARTESIAN_POINT('Ctrl Pts',(15.4899905344219,14.3529910127437,5.85711050041579));
#131384=CARTESIAN_POINT('Ctrl Pts',(15.4890783641418,14.3581429899698,5.86629010920502));
#131385=CARTESIAN_POINT('Ctrl Pts',(15.4886240901128,14.360775939403,5.87086583989662));
#131386=CARTESIAN_POINT('Ctrl Pts',(15.4874003930892,14.368045271583,5.88319155650544));
#131387=CARTESIAN_POINT('Ctrl Pts',(15.4866365007217,14.372775230978,5.89088573748443));
#131388=CARTESIAN_POINT('Ctrl Pts',(15.4825581322327,14.3990044101059,5.93184981887718));
#131389=CARTESIAN_POINT('Ctrl Pts',(15.4793696563172,14.4230140590203,5.96344157916389));
#131390=CARTESIAN_POINT('Ctrl Pts',(15.4735867795493,14.4709293648759,6.01695517899527));
#131391=CARTESIAN_POINT('Ctrl Pts',(15.4709993584947,14.4939590227313,6.0395189884298));
#131392=CARTESIAN_POINT('Ctrl Pts',(15.467533367178,14.5260966204892,6.06713308338228));
#131393=CARTESIAN_POINT('Ctrl Pts',(15.4666976704082,14.5339427815203,6.07359829222213));
#131394=CARTESIAN_POINT('Ctrl Pts',(15.4646029116109,14.5538117770367,6.0892934278339));
#131395=CARTESIAN_POINT('Ctrl Pts',(15.4633378551875,14.5659893106941,6.09831875484494));
#131396=CARTESIAN_POINT('Ctrl Pts',(15.4612753539412,14.5860579269549,6.11225738392157));
#131397=CARTESIAN_POINT('Ctrl Pts',(15.4604868749982,14.5937796895815,6.11740763434963));
#131398=CARTESIAN_POINT('Ctrl Pts',(15.4589479082104,14.6089318202291,6.12710648327711));
#131399=CARTESIAN_POINT('Ctrl Pts',(15.4581981909701,14.6163496904144,6.13167182019241));
#131400=CARTESIAN_POINT('Ctrl Pts',(15.4563685962439,14.634527890282,6.14242130606061));
#131401=CARTESIAN_POINT('Ctrl Pts',(15.4552840565502,14.6453662676324,6.14846732575677));
#131402=CARTESIAN_POINT('Ctrl Pts',(15.4490720261915,14.7077482062829,6.18123447541211));
#131403=CARTESIAN_POINT('Ctrl Pts',(15.4437471548227,14.7621377636819,6.20207567475584));
#131404=CARTESIAN_POINT('Ctrl Pts',(15.4356778200098,14.8472672358452,6.22365820597087));
#131405=CARTESIAN_POINT('Ctrl Pts',(15.4329504935942,14.8765639018257,6.22922725943238));
#131406=CARTESIAN_POINT('Ctrl Pts',(15.4294875498167,14.9149986421132,6.23414978055329));
#131407=CARTESIAN_POINT('Ctrl Pts',(15.4286937201891,14.9238982713221,6.23512562207877));
#131408=CARTESIAN_POINT('Ctrl Pts',(15.4274457571045,14.9380549873666,6.23641802796965));
#131409=CARTESIAN_POINT('Ctrl Pts',(15.426986503302,14.9433011584626,6.236840514129));
#131410=CARTESIAN_POINT('Ctrl Pts',(15.426130337972,14.9531561764013,6.23752827819928));
#131411=CARTESIAN_POINT('Ctrl Pts',(15.4257327269203,14.9577638128169,6.23780648757034));
#131412=CARTESIAN_POINT('Ctrl Pts',(15.4246327235724,14.9705883729491,6.23846029568647));
#131413=CARTESIAN_POINT('Ctrl Pts',(15.4239351666281,14.9788097560181,6.23874193292489));
#131414=CARTESIAN_POINT('Ctrl Pts',(15.4192332868046,15.0347087120355,6.23972279956432));
#131415=CARTESIAN_POINT('Ctrl Pts',(15.4154228796418,15.0823597885935,6.23594351438948));
#131416=CARTESIAN_POINT('Ctrl Pts',(15.4084553561543,15.1675531638058,6.22080152425317));
#131417=CARTESIAN_POINT('Ctrl Pts',(15.4053197640139,15.2051861723463,6.21100421524594));
#131418=CARTESIAN_POINT('Ctrl Pts',(15.4009634553932,15.2547582025784,6.19383371255165));
#131419=CARTESIAN_POINT('Ctrl Pts',(15.3998215222683,15.2675170219097,6.18901491840268));
#131420=CARTESIAN_POINT('Ctrl Pts',(15.3979065588366,15.2884666321186,6.18043300737628));
#131421=CARTESIAN_POINT('Ctrl Pts',(15.3971401426835,15.2967353261543,6.17686793870034));
#131422=CARTESIAN_POINT('Ctrl Pts',(15.3955963724329,15.3131453657191,6.16943423457033));
#131423=CARTESIAN_POINT('Ctrl Pts',(15.3948191418274,15.3212851642268,6.16556595619604));
#131424=CARTESIAN_POINT('Ctrl Pts',(15.3928490714833,15.3415982260221,6.15545312448036));
#131425=CARTESIAN_POINT('Ctrl Pts',(15.391649899273,15.3536720440601,6.14901785601911));
#131426=CARTESIAN_POINT('Ctrl Pts',(15.3864062106976,15.4051746547766,6.11970338634263));
#131427=CARTESIAN_POINT('Ctrl Pts',(15.3822515733105,15.4426115822421,6.09354219936424));
#131428=CARTESIAN_POINT('Ctrl Pts',(15.3754570238094,15.4990455022024,6.04578299395352));
#131429=CARTESIAN_POINT('Ctrl Pts',(15.3728451000567,15.5196245068181,6.02622808863488));
#131430=CARTESIAN_POINT('Ctrl Pts',(15.3692426747452,15.5467720482305,5.99728204945637));
#131431=CARTESIAN_POINT('Ctrl Pts',(15.3682216878176,15.5543246964849,5.98884892663414));
#131432=CARTESIAN_POINT('Ctrl Pts',(15.3664214347519,15.5674204115569,5.97353254885324));
#131433=CARTESIAN_POINT('Ctrl Pts',(15.3656385026394,15.5730393481342,5.96671717902119));
#131434=CARTESIAN_POINT('Ctrl Pts',(15.3644034907934,15.5817944342483,5.95570130261518));
#131435=CARTESIAN_POINT('Ctrl Pts',(15.3639464592728,15.5850102212622,5.95156559618653));
#131436=CARTESIAN_POINT('Ctrl Pts',(15.3630343140923,15.5913833571592,5.9431869679682));
#131437=CARTESIAN_POINT('Ctrl Pts',(15.3625792773048,15.5945396805755,5.9389436608149));
#131438=CARTESIAN_POINT('Ctrl Pts',(15.3613509784014,15.6029887759995,5.92732647113087));
#131439=CARTESIAN_POINT('Ctrl Pts',(15.3605833178554,15.6081919191402,5.91988806795778));
#131440=CARTESIAN_POINT('Ctrl Pts',(15.3572242820411,15.6305500836759,5.88663687319953));
#131441=CARTESIAN_POINT('Ctrl Pts',(15.3547070761151,15.6462105001422,5.85985270889106));
#131442=CARTESIAN_POINT('Ctrl Pts',(15.3491478058262,15.6771699870741,5.79832311926794));
#131443=CARTESIAN_POINT('Ctrl Pts',(15.3461200694798,15.6915684577631,5.76322768508735));
#131444=CARTESIAN_POINT('Ctrl Pts',(15.3411306073947,15.7103716762329,5.70502521312085));
#131445=CARTESIAN_POINT('Ctrl Pts',(15.3392112253379,15.7164783274423,5.68254277834742));
#131446=CARTESIAN_POINT('Ctrl Pts',(15.3363677894907,15.7238127940514,5.64942930716048));
#131447=CARTESIAN_POINT('Ctrl Pts',(15.3354699313882,15.7258879153481,5.63899924116567));
#131448=CARTESIAN_POINT('Ctrl Pts',(15.333839906966,15.729219075678,5.62013799352749));
#131449=CARTESIAN_POINT('Ctrl Pts',(15.3331103914427,15.7305556783495,5.61172280685354));
#131450=CARTESIAN_POINT('Ctrl Pts',(15.3314975702183,15.733171771607,5.59318880634765));
#131451=CARTESIAN_POINT('Ctrl Pts',(15.3306124500743,15.7343878500848,5.58306300722543));
#131452=CARTESIAN_POINT('Ctrl Pts',(15.32793810052,15.737405704941,5.55262637472144));
#131453=CARTESIAN_POINT('Ctrl Pts',(15.3261303316822,15.73857669323,5.53226462500212));
#131454=CARTESIAN_POINT('Ctrl Pts',(15.3193640188557,15.7397887294718,5.45689514901511));
#131455=CARTESIAN_POINT('Ctrl Pts',(15.3142708877315,15.7345318580043,5.40198522419863));
#131456=CARTESIAN_POINT('Ctrl Pts',(15.3078648334357,15.7201306655421,5.33338267580967));
#131457=CARTESIAN_POINT('Ctrl Pts',(15.306491227146,15.7165716565863,5.31868637282943));
#131458=CARTESIAN_POINT('Ctrl Pts',(15.3041567068893,15.709684120363,5.29363263191981));
#131459=CARTESIAN_POINT('Ctrl Pts',(15.3031886952572,15.706573243469,5.28322054967123));
#131460=CARTESIAN_POINT('Ctrl Pts',(15.3017352799149,15.7015005157098,5.26751381355664));
#131461=CARTESIAN_POINT('Ctrl Pts',(15.3012417667802,15.69970594552,5.26216729266063));
#131462=CARTESIAN_POINT('Ctrl Pts',(15.3003207992447,15.696218298093,5.25215795151998));
#131463=CARTESIAN_POINT('Ctrl Pts',(15.2998926874294,15.6945392948091,5.24749104989162));
#131464=CARTESIAN_POINT('Ctrl Pts',(15.2988154875267,15.6901702798967,5.23572046527283));
#131465=CARTESIAN_POINT('Ctrl Pts',(15.2981699036334,15.687417486591,5.22864064195116));
#131466=CARTESIAN_POINT('Ctrl Pts',(15.2952657675121,15.6744431463359,5.19673765738197));
#131467=CARTESIAN_POINT('Ctrl Pts',(15.2930671921494,15.662981628611,5.17243725069471));
#131468=CARTESIAN_POINT('Ctrl Pts',(15.2883146328304,15.6351257756688,5.12086244949662));
#131469=CARTESIAN_POINT('Ctrl Pts',(15.285773677615,15.6182436975709,5.09391523288703));
#131470=CARTESIAN_POINT('Ctrl Pts',(15.2805032809056,15.5801223248354,5.04098028397749));
#131471=CARTESIAN_POINT('Ctrl Pts',(15.2777768154182,15.5587451870643,5.01518625713211));
#131472=CARTESIAN_POINT('Ctrl Pts',(15.2740035976647,15.5276184484873,4.98243138155775));
#131473=CARTESIAN_POINT('Ctrl Pts',(15.2730169406041,15.5193400941577,4.97412516970498));
#131474=CARTESIAN_POINT('Ctrl Pts',(15.2712834629087,15.5045826920972,4.96000650581688));
#131475=CARTESIAN_POINT('Ctrl Pts',(15.2705406162339,15.4981918959925,4.95410487465395));
#131476=CARTESIAN_POINT('Ctrl Pts',(15.2689713617391,15.484562719481,4.9419575785705));
#131477=CARTESIAN_POINT('Ctrl Pts',(15.268144110608,15.4773043849164,4.93573687113212));
#131478=CARTESIAN_POINT('Ctrl Pts',(15.2658586113336,15.4570647386553,4.91906058006096));
#131479=CARTESIAN_POINT('Ctrl Pts',(15.2643892260522,15.4438480076003,4.90890133232782));
#131480=CARTESIAN_POINT('Ctrl Pts',(15.2575325826782,15.3813012542295,4.86410470847991));
#131481=CARTESIAN_POINT('Ctrl Pts',(15.2519536994261,15.3281984521128,4.83514144674961));
#131482=CARTESIAN_POINT('Ctrl Pts',(15.2450221703642,15.2577225678547,4.80722152460192));
#131483=CARTESIAN_POINT('Ctrl Pts',(15.2436077959801,15.2430833708254,4.80195023186749));
#131484=CARTESIAN_POINT('Ctrl Pts',(15.2412130693636,15.2177471847386,4.79372102658508));
#131485=CARTESIAN_POINT('Ctrl Pts',(15.2402251711931,15.2071300646936,4.7905347082374));
#131486=CARTESIAN_POINT('Ctrl Pts',(15.2387485403647,15.1909688463192,4.78607832230386));
#131487=CARTESIAN_POINT('Ctrl Pts',(15.2382513241704,15.1854757189655,4.7846315450095));
#131488=CARTESIAN_POINT('Ctrl Pts',(15.2373278766807,15.1751699984046,4.78204392526856));
#131489=CARTESIAN_POINT('Ctrl Pts',(15.2369009265237,15.1703620395085,4.78088788677452));
#131490=CARTESIAN_POINT('Ctrl Pts',(15.2358329177675,15.1582333990356,4.77810012079674));
#131491=CARTESIAN_POINT('Ctrl Pts',(15.235195231477,15.1508987734924,4.77653139792875));
#131492=CARTESIAN_POINT('Ctrl Pts',(15.2324538033784,15.1190208130612,4.77021930481038));
#131493=CARTESIAN_POINT('Ctrl Pts',(15.2304017081464,15.0942666982995,4.76661065474652));
#131494=CARTESIAN_POINT('Ctrl Pts',(15.2247654725293,15.0251803396307,4.76009634469771));
#131495=CARTESIAN_POINT('Ctrl Pts',(15.2212347128843,14.9807009808366,4.75991952041867));
#131496=CARTESIAN_POINT('Ctrl Pts',(15.2162066937237,14.919151407828,4.76523009136065));
#131497=CARTESIAN_POINT('Ctrl Pts',(15.2147814187573,14.9018879048862,4.76733550905956));
#131498=CARTESIAN_POINT('Ctrl Pts',(15.2121603215073,14.8706624072444,4.77226707599984));
#131499=CARTESIAN_POINT('Ctrl Pts',(15.2109704525231,14.8566771217979,4.77489178694993));
#131500=CARTESIAN_POINT('Ctrl Pts',(15.2089982188837,14.8338749631326,4.77985662623833));
#131501=CARTESIAN_POINT('Ctrl Pts',(15.2082233541159,14.8250097866401,4.78195932132144));
#131502=CARTESIAN_POINT('Ctrl Pts',(15.2066885427285,14.8076493294858,4.7864175569321));
#131503=CARTESIAN_POINT('Ctrl Pts',(15.2059290575557,14.7991528282493,4.78876228837253));
#131504=CARTESIAN_POINT('Ctrl Pts',(15.2040324513256,14.778181147762,4.79495545918812));
#131505=CARTESIAN_POINT('Ctrl Pts',(15.2028897871548,14.7657626925221,4.79898342085638));
#131506=CARTESIAN_POINT('Ctrl Pts',(15.1970292133704,14.7032148559598,4.82111847343141));
#131507=CARTESIAN_POINT('Ctrl Pts',(15.1921511948226,14.6550518762363,4.84427891666842));
#131508=CARTESIAN_POINT('Ctrl Pts',(15.184262763908,14.5821777722817,4.88958696347024));
#131509=CARTESIAN_POINT('Ctrl Pts',(15.1812770768556,14.5557098490978,4.90857276570762));
#131510=CARTESIAN_POINT('Ctrl Pts',(15.1775375990922,14.5234239159424,4.93512654442446));
#131511=CARTESIAN_POINT('Ctrl Pts',(15.1767155536211,14.5163812516878,4.94114428040627));
#131512=CARTESIAN_POINT('Ctrl Pts',(15.1754340799272,14.5054699581362,4.9508284414386));
#131513=CARTESIAN_POINT('Ctrl Pts',(15.1749690821581,14.5015249425992,4.95440675797896));
#131514=CARTESIAN_POINT('Ctrl Pts',(15.1740559574324,14.493801619868,4.96156589058948));
#131515=CARTESIAN_POINT('Ctrl Pts',(15.1736077399166,14.4900218082253,4.96514456300887));
#131516=CARTESIAN_POINT('Ctrl Pts',(15.1724208269508,14.4800518053797,4.97478581602349));
#131517=CARTESIAN_POINT('Ctrl Pts',(15.1716871019361,14.4739296117049,4.98091808818721));
#131518=CARTESIAN_POINT('Ctrl Pts',(15.1669246907344,14.4345650743947,5.02175949748127));
#131519=CARTESIAN_POINT('Ctrl Pts',(15.1630883000331,14.4046634511938,5.05953834011732));
#131520=CARTESIAN_POINT('Ctrl Pts',(15.1564619839311,14.3601271268223,5.12871404094873));
#131521=CARTESIAN_POINT('Ctrl Pts',(15.1536987860371,14.343634509876,5.15871634376645));
#131522=CARTESIAN_POINT('Ctrl Pts',(15.1495995528462,14.3228219722918,5.20371045200673));
#131523=CARTESIAN_POINT('Ctrl Pts',(15.1483161873207,14.3168025245518,5.21786754736671));
#131524=CARTESIAN_POINT('Ctrl Pts',(15.1462316606304,14.3078509964003,5.24089060716967));
#131525=CARTESIAN_POINT('Ctrl Pts',(15.145439837054,14.3046373909379,5.24964276344141));
#131526=CARTESIAN_POINT('Ctrl Pts',(15.1438909747184,14.2987179708466,5.26675818771838));
#131527=CARTESIAN_POINT('Ctrl Pts',(15.1431346724125,14.295994096024,5.27511358406749));
#131528=CARTESIAN_POINT('Ctrl Pts',(15.1413035450768,14.2898016665464,5.29532491788782));
#131529=CARTESIAN_POINT('Ctrl Pts',(15.1402242320716,14.2864802519917,5.3072226904373));
#131530=CARTESIAN_POINT('Ctrl Pts',(15.1339829113367,14.2691561771627,5.3758799476414));
#131531=CARTESIAN_POINT('Ctrl Pts',(15.1286201460481,14.2616328904203,5.43404843570366));
#131532=CARTESIAN_POINT('Ctrl Pts',(15.1205345037587,14.2607373493634,5.52204944684244));
#131533=CARTESIAN_POINT('Ctrl Pts',(15.1178278533825,14.2622115112062,5.55161352494177));
#131534=CARTESIAN_POINT('Ctrl Pts',(15.114387174355,14.2664323502094,5.58988419383587));
#131535=CARTESIAN_POINT('Ctrl Pts',(15.1135957134548,14.2675715227852,5.59873810271899));
#131536=CARTESIAN_POINT('Ctrl Pts',(15.1123505665385,14.2696361944341,5.61277123840683));
#131537=CARTESIAN_POINT('Ctrl Pts',(15.1118917969224,14.2704569974679,5.61796462862891));
#131538=CARTESIAN_POINT('Ctrl Pts',(15.1110358145192,14.2721029791986,5.62770381912303));
#131539=CARTESIAN_POINT('Ctrl Pts',(15.1106379106869,14.2729154816681,5.63225144677907));
#131540=CARTESIAN_POINT('Ctrl Pts',(15.1095358525569,14.2752969886803,5.64489493903591));
#131541=CARTESIAN_POINT('Ctrl Pts',(15.1088365642261,14.2769589960563,5.65297294696688));
#131542=CARTESIAN_POINT('Ctrl Pts',(15.105572575207,14.2854161614428,5.69085398919124));
#131543=CARTESIAN_POINT('Ctrl Pts',(15.1030853361234,14.2939179596096,5.72023137888309));
#131544=CARTESIAN_POINT('Ctrl Pts',(15.1006178015771,14.3042076756101,5.74898602635499));
#131545=CARTESIAN_POINT('',(15.043709765672,14.2610104882535,5.49935386504384));
#131546=CARTESIAN_POINT('Ctrl Pts',(15.0212936472645,14.3041920192027,5.74894227013274));
#131547=CARTESIAN_POINT('Ctrl Pts',(15.0223182907216,14.3000436147494,5.73734724079242));
#131548=CARTESIAN_POINT('Ctrl Pts',(15.0233508648385,14.2961859397969,5.72565103150668));
#131549=CARTESIAN_POINT('Ctrl Pts',(15.0250923247468,14.2902294392276,5.7059493344584));
#131550=CARTESIAN_POINT('Ctrl Pts',(15.025795992383,14.287969522801,5.69799486144921));
#131551=CARTESIAN_POINT('Ctrl Pts',(15.0272756037324,14.2835264193999,5.68129488363134));
#131552=CARTESIAN_POINT('Ctrl Pts',(15.0280522266231,14.2813688318268,5.67254406693846));
#131553=CARTESIAN_POINT('Ctrl Pts',(15.0299512189619,14.2765178666212,5.651196858922));
#131554=CARTESIAN_POINT('Ctrl Pts',(15.03107861212,14.2739928573599,5.63856576440307));
#131555=CARTESIAN_POINT('Ctrl Pts',(15.0359616676643,14.264574940277,5.58408250794419));
#131556=CARTESIAN_POINT('Ctrl Pts',(15.0398126156169,14.2609631816662,5.54175221801516));
#131557=CARTESIAN_POINT('Ctrl Pts',(15.0437039207594,14.2610002829325,5.49935333612335));
#131558=CARTESIAN_POINT('Ctrl Pts',(15.043709765672,14.2610104882535,5.49935386504384));
#131559=CARTESIAN_POINT('Ctrl Pts',(15.046685545653,14.2609595334599,5.46642905352292));
#131560=CARTESIAN_POINT('Ctrl Pts',(15.0496697149401,14.2631076464298,5.43358447738546));
#131561=CARTESIAN_POINT('Ctrl Pts',(15.052610173577,14.2674364515606,5.40107731686082));
#131562=CARTESIAN_POINT('Ctrl Pts',(15.0535470231831,14.2688156375593,5.39072032011563));
#131563=CARTESIAN_POINT('Ctrl Pts',(15.0544794357131,14.2704163193918,5.38039720107147));
#131564=CARTESIAN_POINT('Ctrl Pts',(15.0554057261597,14.2722383764944,5.37011526689897));
#131565=CARTESIAN_POINT('Ctrl Pts',(15.0567161994914,14.2748161394955,5.35556885699023));
#131566=CARTESIAN_POINT('Ctrl Pts',(15.0580139727417,14.277836233072,5.34110642935388));
#131567=CARTESIAN_POINT('Ctrl Pts',(15.059293127905,14.2812964464757,5.32675188192325));
#131568=CARTESIAN_POINT('Ctrl Pts',(15.0592943869642,14.281299852328,5.32673775289072));
#131569=CARTESIAN_POINT('Ctrl Pts',(15.0592956460065,14.2813032586102,5.32672362394553));
#131570=CARTESIAN_POINT('Ctrl Pts',(15.059296905032,14.2813066653223,5.32670949508773));
#131571=CARTESIAN_POINT('Ctrl Pts',(15.0618856599462,14.2883114026749,5.29765833542018));
#131572=CARTESIAN_POINT('Ctrl Pts',(15.0644031451847,14.2971372223748,5.26897381748352));
#131573=CARTESIAN_POINT('Ctrl Pts',(15.0668903239177,14.3077091184231,5.24089375008832));
#131574=CARTESIAN_POINT('Ctrl Pts',(15.0671469791864,14.3088000463832,5.23799613073031));
#131575=CARTESIAN_POINT('Ctrl Pts',(15.0674033117378,14.3099095308069,5.23510497537456));
#131576=CARTESIAN_POINT('Ctrl Pts',(15.0676593665835,14.3110374635529,5.2322205634705));
#131577=CARTESIAN_POINT('Ctrl Pts',(15.0703936478333,14.3230820915351,5.2014193756733));
#131578=CARTESIAN_POINT('Ctrl Pts',(15.0730970996172,14.337234617664,5.17138346159711));
#131579=CARTESIAN_POINT('Ctrl Pts',(15.0758166969593,14.353348058333,5.14240376075178));
#131580=CARTESIAN_POINT('Ctrl Pts',(15.0785334910692,14.3694448900303,5.11345393080986));
#131581=CARTESIAN_POINT('Ctrl Pts',(15.0812668780129,14.3874980403923,5.0855580140648));
#131582=CARTESIAN_POINT('Ctrl Pts',(15.0840460724848,14.4073281408633,5.05897743470522));
#131583=CARTESIAN_POINT('Ctrl Pts',(15.0868239422916,14.4271487895874,5.03240952461625));
#131584=CARTESIAN_POINT('Ctrl Pts',(15.0896478007549,14.4487443984622,5.00715558422028));
#131585=CARTESIAN_POINT('Ctrl Pts',(15.0925240211446,14.4719093238968,4.98344993559047));
#131586=CARTESIAN_POINT('Ctrl Pts',(15.0954025934196,14.4950931912908,4.95972490285195));
#131587=CARTESIAN_POINT('Ctrl Pts',(15.0983336549516,14.5198488539283,4.93755064902295));
#131588=CARTESIAN_POINT('Ctrl Pts',(15.101298774781,14.5459464551747,4.91713651593686));
#131589=CARTESIAN_POINT('Ctrl Pts',(15.1042653138839,14.5720565482031,4.89671261149691));
#131590=CARTESIAN_POINT('Ctrl Pts',(15.1072657809954,14.5995099972452,4.87805058477965));
#131591=CARTESIAN_POINT('Ctrl Pts',(15.1102577363054,14.6280526088082,4.86133441152981));
#131592=CARTESIAN_POINT('Ctrl Pts',(15.1132554936804,14.6566505708263,4.84458582191203));
#131593=CARTESIAN_POINT('Ctrl Pts',(15.1162442336628,14.6863422917646,4.82979100185164));
#131594=CARTESIAN_POINT('Ctrl Pts',(15.1191618125078,14.7168441793445,4.81710620235439));
#131595=CARTESIAN_POINT('Ctrl Pts',(15.1201945367908,14.7276408164384,4.81261621213913));
#131596=CARTESIAN_POINT('Ctrl Pts',(15.1212182051605,14.7385386779047,4.80839029865132));
#131597=CARTESIAN_POINT('Ctrl Pts',(15.1222297082397,14.7495242032278,4.80443433472866));
#131598=CARTESIAN_POINT('Ctrl Pts',(15.1222309673336,14.7495378777366,4.80442941044312));
#131599=CARTESIAN_POINT('Ctrl Pts',(15.1222322264106,14.7495515524089,4.80442448656474));
#131600=CARTESIAN_POINT('Ctrl Pts',(15.1222334854708,14.7495652272445,4.80441956309354));
#131601=CARTESIAN_POINT('Ctrl Pts',(15.1248222384473,14.7776820501033,4.79429641640001));
#131602=CARTESIAN_POINT('Ctrl Pts',(15.1273397213037,14.80649396278,4.78589594207448));
#131603=CARTESIAN_POINT('Ctrl Pts',(15.1298268971727,14.8357610914496,4.77928625107586));
#131604=CARTESIAN_POINT('Ctrl Pts',(15.130083554543,14.8387812334403,4.77860418193421));
#131605=CARTESIAN_POINT('Ctrl Pts',(15.1303398891848,14.8418061797683,4.7779411668358));
#131606=CARTESIAN_POINT('Ctrl Pts',(15.1305959461108,14.8448356375512,4.77729726911286));
#131607=CARTESIAN_POINT('Ctrl Pts',(15.1333302264247,14.8771854236143,4.77042146655147));
#131608=CARTESIAN_POINT('Ctrl Pts',(15.1360336766783,14.9100550468417,4.76572709493435));
#131609=CARTESIAN_POINT('Ctrl Pts',(15.1387532720654,14.9431206775473,4.76325135956388));
#131610=CARTESIAN_POINT('Ctrl Pts',(15.1414700641897,14.9761522253698,4.76077817609391));
#131611=CARTESIAN_POINT('Ctrl Pts',(15.1442034487258,15.0093791747229,4.76051852538285));
#131612=CARTESIAN_POINT('Ctrl Pts',(15.1469826405762,15.0424845418505,4.76246633367419));
#131613=CARTESIAN_POINT('Ctrl Pts',(15.1497605077328,15.075574129401,4.76441321354837));
#131614=CARTESIAN_POINT('Ctrl Pts',(15.1525843633328,15.1085421829167,4.76856513821236));
#131615=CARTESIAN_POINT('Ctrl Pts',(15.1554605808695,15.1410799084982,4.77487918515324));
#131616=CARTESIAN_POINT('Ctrl Pts',(15.1583391502564,15.1736442398058,4.78119839501808));
#131617=CARTESIAN_POINT('Ctrl Pts',(15.1612702089108,15.205777528696,4.7896831650204));
#131618=CARTESIAN_POINT('Ctrl Pts',(15.1642353260955,15.2371785326199,4.8002566129381));
#131619=CARTESIAN_POINT('Ctrl Pts',(15.1672018625311,15.2685945666086,4.81083512182802));
#131620=CARTESIAN_POINT('Ctrl Pts',(15.17020232721,15.2992776274748,4.82350445858556));
#131621=CARTESIAN_POINT('Ctrl Pts',(15.1731942805184,15.3289342782322,4.83815346573462));
#131622=CARTESIAN_POINT('Ctrl Pts',(15.1761920358741,15.3586484396771,4.85283088049035));
#131623=CARTESIAN_POINT('Ctrl Pts',(15.1791807742738,15.3873321063918,4.8694961575027));
#131624=CARTESIAN_POINT('Ctrl Pts',(15.1820983521007,15.4146988337077,4.88799833915478));
#131625=CARTESIAN_POINT('Ctrl Pts',(15.1831310850357,15.4243858145872,4.89454754315068));
#131626=CARTESIAN_POINT('Ctrl Pts',(15.1841547619693,15.4339078788635,4.90132650367367));
#131627=CARTESIAN_POINT('Ctrl Pts',(15.1851662734444,15.4432526645573,4.90832712317662));
#131628=CARTESIAN_POINT('Ctrl Pts',(15.1851675325333,15.4432642965713,4.90833583726666));
#131629=CARTESIAN_POINT('Ctrl Pts',(15.1851687916053,15.4432759283351,4.9083445517171));
#131630=CARTESIAN_POINT('Ctrl Pts',(15.1851700506604,15.4432875598486,4.90835326652794));
#131631=CARTESIAN_POINT('Ctrl Pts',(15.1877588052003,15.4672032188393,4.92627186700164));
#131632=CARTESIAN_POINT('Ctrl Pts',(15.1902762897157,15.4900621955577,4.94571827013843));
#131633=CARTESIAN_POINT('Ctrl Pts',(15.1927634673064,15.5116757036713,4.96652956978407));
#131634=CARTESIAN_POINT('Ctrl Pts',(15.1930201247306,15.5139060499653,4.96867713439024));
#131635=CARTESIAN_POINT('Ctrl Pts',(15.1932764594274,15.5161231228628,4.9708391888316));
#131636=CARTESIAN_POINT('Ctrl Pts',(15.1935325164093,15.5183267084219,4.97301552329867));
#131637=CARTESIAN_POINT('Ctrl Pts',(15.196266798539,15.5418575044603,4.99625532092931));
#131638=CARTESIAN_POINT('Ctrl Pts',(15.1989702506808,15.5638520715764,5.02112879029918));
#131639=CARTESIAN_POINT('Ctrl Pts',(15.2016898479807,15.5841012741654,5.04738590659609));
#131640=CARTESIAN_POINT('Ctrl Pts',(15.2044066420413,15.6043296047826,5.07361595823274));
#131641=CARTESIAN_POINT('Ctrl Pts',(15.2071400285388,15.6228165004013,5.10122634451727));
#131642=CARTESIAN_POINT('Ctrl Pts',(15.2099192223221,15.6393927389725,5.12994896158249));
#131643=CARTESIAN_POINT('Ctrl Pts',(15.2126970914321,15.6559610766546,5.15865788831575));
#131644=CARTESIAN_POINT('Ctrl Pts',(15.2155209489576,15.6706208002561,5.1884777586313));
#131645=CARTESIAN_POINT('Ctrl Pts',(15.2183971683278,15.6832379692582,5.21912704786309));
#131646=CARTESIAN_POINT('Ctrl Pts',(15.2212757395646,15.695865455241,5.24980139882803));
#131647=CARTESIAN_POINT('Ctrl Pts',(15.2242067999771,15.7064471222298,5.28130646226646));
#131648=CARTESIAN_POINT('Ctrl Pts',(15.2271719187527,15.7148815470349,5.3133483479334));
#131649=CARTESIAN_POINT('Ctrl Pts',(15.2301384567909,15.7233200090017,5.3454055705418));
#131650=CARTESIAN_POINT('Ctrl Pts',(15.2331389229045,15.7296090546103,5.37800022275787));
#131651=CARTESIAN_POINT('Ctrl Pts',(15.2361308774017,15.7336801813444,5.41082608756029));
#131652=CARTESIAN_POINT('Ctrl Pts',(15.2391286339414,15.7377592028676,5.44371560876512));
#131653=CARTESIAN_POINT('Ctrl Pts',(15.2421173732762,15.7396112172276,5.47683743517485));
#131654=CARTESIAN_POINT('Ctrl Pts',(15.2450349517313,15.7392048101568,5.50986930580845));
#131655=CARTESIAN_POINT('Ctrl Pts',(15.2460676728476,15.7390609562141,5.52156143708696));
#131656=CARTESIAN_POINT('Ctrl Pts',(15.2470913381354,15.738634521863,5.53324215314183));
#131657=CARTESIAN_POINT('Ctrl Pts',(15.2481028382458,15.7379254733588,5.54489667652789));
#131658=CARTESIAN_POINT('Ctrl Pts',(15.2481040973284,15.7379245907582,5.54491118370096));
#131659=CARTESIAN_POINT('Ctrl Pts',(15.2481053563941,15.737923707719,5.54492569086321));
#131660=CARTESIAN_POINT('Ctrl Pts',(15.2481066154429,15.7379228242412,5.54494019801461));
#131661=CARTESIAN_POINT('Ctrl Pts',(15.2506953696104,15.7361062887758,5.57476862677589));
#131662=CARTESIAN_POINT('Ctrl Pts',(15.2532128538165,15.7324326186822,5.60455452190264));
#131663=CARTESIAN_POINT('Ctrl Pts',(15.2557000311894,15.7269340777126,5.63405062287497));
#131664=CARTESIAN_POINT('Ctrl Pts',(15.2559566880301,15.7263666721993,5.63709438492113));
#131665=CARTESIAN_POINT('Ctrl Pts',(15.2562130221458,15.7257798655446,5.64013502756024));
#131666=CARTESIAN_POINT('Ctrl Pts',(15.2564690785486,15.7251737153565,5.64317225673248));
#131667=CARTESIAN_POINT('Ctrl Pts',(15.2592033599,15.7187009806899,5.675605107434));
#131668=CARTESIAN_POINT('Ctrl Pts',(15.2619068113793,15.7100190027675,5.70765309131112));
#131669=CARTESIAN_POINT('Ctrl Pts',(15.2646264081145,15.699221622836,5.73900404841786));
#131670=CARTESIAN_POINT('Ctrl Pts',(15.2673432016053,15.6884353723836,5.77032269029389));
#131671=CARTESIAN_POINT('Ctrl Pts',(15.2700765876299,15.675538647215,5.80094576630405));
#131672=CARTESIAN_POINT('Ctrl Pts',(15.2728557810128,15.6606623359664,5.83058451380219));
#131673=CARTESIAN_POINT('Ctrl Pts',(15.2756336497183,15.6457931153766,5.86020913426015));
#131674=CARTESIAN_POINT('Ctrl Pts',(15.2784575069112,15.6289465071931,5.88885042484307));
#131675=CARTESIAN_POINT('Ctrl Pts',(15.281333725998,15.6102840096509,5.91624171263645));
#131676=CARTESIAN_POINT('Ctrl Pts',(15.2842122969514,15.5916062518994,5.94365539811724));
#131677=CARTESIAN_POINT('Ctrl Pts',(15.2871433571296,15.5711097293887,5.96981706546049));
#131678=CARTESIAN_POINT('Ctrl Pts',(15.2901084757038,15.5489841486601,5.9944804028846));
#131679=CARTESIAN_POINT('Ctrl Pts',(15.29307501354,15.5268479774629,6.01915554548136));
#131680=CARTESIAN_POINT('Ctrl Pts',(15.2960754794847,15.5030810452484,6.04233087613006));
#131681=CARTESIAN_POINT('Ctrl Pts',(15.2990674338381,15.4779014562307,6.06378080242425));
#131682=CARTESIAN_POINT('Ctrl Pts',(15.3020651902414,15.4526730385167,6.08527232478803));
#131683=CARTESIAN_POINT('Ctrl Pts',(15.3050539294653,15.4260260541295,6.10503145249076));
#131684=CARTESIAN_POINT('Ctrl Pts',(15.3079715078339,15.3982124013273,6.12285474959797));
#131685=CARTESIAN_POINT('Ctrl Pts',(15.3090042333416,15.3883672951876,6.12916360277261));
#131686=CARTESIAN_POINT('Ctrl Pts',(15.3100279029465,15.3783763441575,6.13523014918259));
#131687=CARTESIAN_POINT('Ctrl Pts',(15.3110394072595,15.3682518728438,6.14104623508441));
#131688=CARTESIAN_POINT('Ctrl Pts',(15.3110406663469,15.3682392702335,6.14105347475766));
#131689=CARTESIAN_POINT('Ctrl Pts',(15.3110419254175,15.3682266673911,6.14106071405862));
#131690=CARTESIAN_POINT('Ctrl Pts',(15.3110431844712,15.3682140643165,6.14106795298725));
#131691=CARTESIAN_POINT('Ctrl Pts',(15.3136319384367,15.3423007464737,6.15595199240796));
#131692=CARTESIAN_POINT('Ctrl Pts',(15.31614942238,15.3154018000945,6.1692614549191));
#131693=CARTESIAN_POINT('Ctrl Pts',(15.3186365994219,15.2877414922757,6.18088733164246));
#131694=CARTESIAN_POINT('Ctrl Pts',(15.3188932565782,15.284887165532,6.1820870309035));
#131695=CARTESIAN_POINT('Ctrl Pts',(15.3191495910078,15.282024776462,6.1832688099034));
#131696=CARTESIAN_POINT('Ctrl Pts',(15.3194056477232,15.2791546023593,6.18443255506905));
#131697=CARTESIAN_POINT('Ctrl Pts',(15.3221399290356,15.2485056760054,6.19685951545524));
#131698=CARTESIAN_POINT('Ctrl Pts',(15.3248433803914,15.2169634492227,6.20722956257817));
#131699=CARTESIAN_POINT('Ctrl Pts',(15.3275629769416,15.1848402558027,6.21544943543967));
#131700=CARTESIAN_POINT('Ctrl Pts',(15.330279770244,15.1527501736423,6.22366083559609));
#131701=CARTESIAN_POINT('Ctrl Pts',(15.3330131560189,15.1200806139098,6.2297269803529));
#131702=CARTESIAN_POINT('Ctrl Pts',(15.3357923491187,15.0871447382741,6.2335984180491));
#131703=CARTESIAN_POINT('Ctrl Pts',(15.3385702175381,15.0542245612634,6.2374680104551));
#131704=CARTESIAN_POINT('Ctrl Pts',(15.3413940744116,15.0210384430784,6.23914528121923));
#131705=CARTESIAN_POINT('Ctrl Pts',(15.3442702931754,14.9878979255697,6.23861849181247));
#131706=CARTESIAN_POINT('Ctrl Pts',(15.3471488638016,14.9547303093106,6.23809127165399));
#131707=CARTESIAN_POINT('Ctrl Pts',(15.350079923649,14.9216083960125,6.23535648147473));
#131708=CARTESIAN_POINT('Ctrl Pts',(15.3530450419179,14.8888422311719,6.23043713969165));
#131709=CARTESIAN_POINT('Ctrl Pts',(15.356011579446,14.8560603827466,6.22551544325663));
#131710=CARTESIAN_POINT('Ctrl Pts',(15.3590120451082,14.8236345843641,6.21840695804047));
#131711=CARTESIAN_POINT('Ctrl Pts',(15.3620039992297,14.7918731900644,6.20916981455404));
#131712=CARTESIAN_POINT('Ctrl Pts',(15.3650017553981,14.7600502035432,6.19991475824611));
#131713=CARTESIAN_POINT('Ctrl Pts',(15.3679904944384,14.7288942102524,6.18852226373755));
#131714=CARTESIAN_POINT('Ctrl Pts',(15.3709080726904,14.6987136396494,6.17509087119461));
#131715=CARTESIAN_POINT('Ctrl Pts',(15.3719407988323,14.6880307165027,6.17033660275556));
#131716=CARTESIAN_POINT('Ctrl Pts',(15.3729644690679,14.6774699890325,6.16532728193802));
#131717=CARTESIAN_POINT('Ctrl Pts',(15.3739759740021,14.6670450445103,6.16006871962322));
#131718=CARTESIAN_POINT('Ctrl Pts',(15.3739772330885,14.6670320679001,6.16006217394677));
#131719=CARTESIAN_POINT('Ctrl Pts',(15.373978492158,14.6670190914731,6.16005562787173));
#131720=CARTESIAN_POINT('Ctrl Pts',(15.3739797512106,14.6670061152295,6.16004908139809));
#131721=CARTESIAN_POINT('Ctrl Pts',(15.3765685213135,14.6403253309968,6.1465887105774));
#131722=CARTESIAN_POINT('Ctrl Pts',(15.3790860205765,14.6144177854373,6.13143927358467));
#131723=CARTESIAN_POINT('Ctrl Pts',(15.3815732127602,14.589497844783,6.11472815397399));
#131724=CARTESIAN_POINT('Ctrl Pts',(15.3818301718085,14.5869232933363,6.11300167967105));
#131725=CARTESIAN_POINT('Ctrl Pts',(15.3820868073725,14.5843593016485,6.11125857862862));
#131726=CARTESIAN_POINT('Ctrl Pts',(15.3823431646236,14.5818061179262,6.10949902060918));
#131727=CARTESIAN_POINT('Ctrl Pts',(15.3850775311863,14.5545732615545,6.09073116211081));
#131728=CARTESIAN_POINT('Ctrl Pts',(15.3877810720171,14.5285673908074,6.07008605612694));
#131729=CARTESIAN_POINT('Ctrl Pts',(15.3905007651949,14.5040381616394,6.04777332771944));
#131730=CARTESIAN_POINT('Ctrl Pts',(15.3932180794694,14.479530388077,6.02548011615447));
#131731=CARTESIAN_POINT('Ctrl Pts',(15.3959519991338,14.4564964272674,6.00152271037857));
#131732=CARTESIAN_POINT('Ctrl Pts',(15.398731750532,14.435149891367,5.97613562952543));
#131733=CARTESIAN_POINT('Ctrl Pts',(15.4015099804942,14.4138150390255,5.95076244373483));
#131734=CARTESIAN_POINT('Ctrl Pts',(15.4043342166437,14.3941655856131,5.92396141030448));
#131735=CARTESIAN_POINT('Ctrl Pts',(15.4072108249875,14.3763826913015,5.89598639120007));
#131736=CARTESIAN_POINT('Ctrl Pts',(15.4100893512336,14.358587940717,5.86799272049417));
#131737=CARTESIAN_POINT('Ctrl Pts',(15.4130203605021,14.3426621732482,5.83882357447615));
#131738=CARTESIAN_POINT('Ctrl Pts',(15.4159854127,14.3287566151184,5.80875056030614));
#131739=CARTESIAN_POINT('Ctrl Pts',(15.4179145687271,14.3197092225317,5.7891841133556));
#131740=CARTESIAN_POINT('Ctrl Pts',(15.4198576101616,14.311516429361,5.76923536980049));
#131741=CARTESIAN_POINT('Ctrl Pts',(15.4218039449478,14.3042130192439,5.74898305934474));
#131742=CARTESIAN_POINT('Origin',(13.2437274406976,15.,5.5));
#131743=CARTESIAN_POINT('',(15.901560926295,14.3042076642396,5.74898599458007));
#131744=CARTESIAN_POINT('',(15.8222092530609,14.3040405757782,5.74907393379149));
#131745=CARTESIAN_POINT('',(13.2437274406976,14.3042076641721,5.74898599439144));
#131746=CARTESIAN_POINT('Ctrl Pts',(15.901560926295,14.3042076642395,5.74898599457988));
#131747=CARTESIAN_POINT('Ctrl Pts',(15.9010190912704,14.306350730213,5.75497480082541));
#131748=CARTESIAN_POINT('Ctrl Pts',(15.9004756543572,14.3085674346765,5.76092615949075));
#131749=CARTESIAN_POINT('Ctrl Pts',(15.8993204802887,14.3134192632855,5.77345558730921));
#131750=CARTESIAN_POINT('Ctrl Pts',(15.8987090507264,14.3160688926906,5.78001660504494));
#131751=CARTESIAN_POINT('Ctrl Pts',(15.8969222802899,14.324044718264,5.79897754145352));
#131752=CARTESIAN_POINT('Ctrl Pts',(15.895738944638,14.3296165653406,5.81127015873152));
#131753=CARTESIAN_POINT('Ctrl Pts',(15.8899081820006,14.3584484064902,5.87050946718659));
#131754=CARTESIAN_POINT('Ctrl Pts',(15.8851092827127,14.3863156565981,5.91503639228237));
#131755=CARTESIAN_POINT('Ctrl Pts',(15.8773481532337,14.4384402854192,5.98145562301003));
#131756=CARTESIAN_POINT('Ctrl Pts',(15.8744072089615,14.4598552502085,6.00536411943401));
#131757=CARTESIAN_POINT('Ctrl Pts',(15.8707154059179,14.4893356864558,6.03425442147313));
#131758=CARTESIAN_POINT('Ctrl Pts',(15.8698980696092,14.4960342086426,6.04057777710842));
#131759=CARTESIAN_POINT('Ctrl Pts',(15.8686221836898,14.5067823201493,6.05035040832505));
#131760=CARTESIAN_POINT('Ctrl Pts',(15.8681581404396,14.5107536330575,6.05388378710459));
#131761=CARTESIAN_POINT('Ctrl Pts',(15.867245212566,14.5186953561192,6.06079766773829));
#131762=CARTESIAN_POINT('Ctrl Pts',(15.8667962564223,14.5226640760234,6.06417958535731));
#131763=CARTESIAN_POINT('Ctrl Pts',(15.8656048051966,14.5333567489225,6.07309765957925));
#131764=CARTESIAN_POINT('Ctrl Pts',(15.8648673489293,14.5401436239582,6.07855767678657));
#131765=CARTESIAN_POINT('Ctrl Pts',(15.8605185610571,14.5810764755566,6.11031246912124));
#131766=CARTESIAN_POINT('Ctrl Pts',(15.857060372767,14.6173778428562,6.13370312014058));
#131767=CARTESIAN_POINT('Ctrl Pts',(15.8511441067054,14.6824011018498,6.16796361242261));
#131768=CARTESIAN_POINT('Ctrl Pts',(15.8486984505258,14.710132281052,6.18045644194394));
#131769=CARTESIAN_POINT('Ctrl Pts',(15.8454071429745,14.7477255601951,6.19467603423283));
#131770=CARTESIAN_POINT('Ctrl Pts',(15.8446000858053,14.7569665060866,6.19796267237899));
#131771=CARTESIAN_POINT('Ctrl Pts',(15.842564223519,14.7802913079684,6.20573900734019));
#131772=CARTESIAN_POINT('Ctrl Pts',(15.841329533632,14.7944488959244,6.20999164788247));
#131773=CARTESIAN_POINT('Ctrl Pts',(15.8393035330068,14.8176218302293,6.21620113677814));
#131774=CARTESIAN_POINT('Ctrl Pts',(15.838520584489,14.8265634940413,6.21841883843111));
#131775=CARTESIAN_POINT('Ctrl Pts',(15.8369837408856,14.8440717595613,6.22241532247205));
#131776=CARTESIAN_POINT('Ctrl Pts',(15.8362304960068,14.852633132112,6.22421026383182));
#131777=CARTESIAN_POINT('Ctrl Pts',(15.8343761980905,14.8736469091048,6.22822789533029));
#131778=CARTESIAN_POINT('Ctrl Pts',(15.8332701611456,14.8861279062051,6.23028355744324));
#131779=CARTESIAN_POINT('Ctrl Pts',(15.8271812992151,14.9544922819002,6.23974836629611));
#131780=CARTESIAN_POINT('Ctrl Pts',(15.8220148474509,15.0110203090233,6.24106312870786));
#131781=CARTESIAN_POINT('Ctrl Pts',(15.8140122770399,15.0977367820379,6.23315265306898));
#131782=CARTESIAN_POINT('Ctrl Pts',(15.8111966503182,15.128138367114,6.22845469237488));
#131783=CARTESIAN_POINT('Ctrl Pts',(15.8076388507702,15.1670127164,6.21993739392308));
#131784=CARTESIAN_POINT('Ctrl Pts',(15.8068350942062,15.1758278124639,6.21783542815829));
#131785=CARTESIAN_POINT('Ctrl Pts',(15.8055753332943,15.1897200219132,6.21425152714977));
#131786=CARTESIAN_POINT('Ctrl Pts',(15.8051140520987,15.1948233720841,6.21287641978269));
#131787=CARTESIAN_POINT('Ctrl Pts',(15.8042570696595,15.204341415113,6.21020191288035));
#131788=CARTESIAN_POINT('Ctrl Pts',(15.8038606365126,15.2087595092214,6.20891582127889));
#131789=CARTESIAN_POINT('Ctrl Pts',(15.8027689692013,15.220959296157,6.20524055885781));
#131790=CARTESIAN_POINT('Ctrl Pts',(15.8020784453792,15.2287143004552,6.20276385968532));
#131791=CARTESIAN_POINT('Ctrl Pts',(15.7973192442402,15.282310802889,6.18466558542474));
#131792=CARTESIAN_POINT('Ctrl Pts',(15.7934517162254,15.3265679096676,6.1646963915172));
#131793=CARTESIAN_POINT('Ctrl Pts',(15.7867439009506,15.3987646129057,6.12315513103539));
#131794=CARTESIAN_POINT('Ctrl Pts',(15.7839294568019,15.427701106077,6.10366126042322));
#131795=CARTESIAN_POINT('Ctrl Pts',(15.7797768741851,15.4672646645769,6.07273126308239));
#131796=CARTESIAN_POINT('Ctrl Pts',(15.7784940641908,15.4790774543958,6.06288728274005));
#131797=CARTESIAN_POINT('Ctrl Pts',(15.7764102060157,15.4975455259033,6.04649459892924));
#131798=CARTESIAN_POINT('Ctrl Pts',(15.7756184840612,15.5043990884787,6.04017537883108));
#131799=CARTESIAN_POINT('Ctrl Pts',(15.7740696678275,15.5174783137206,6.02764991510521));
#131800=CARTESIAN_POINT('Ctrl Pts',(15.7733133078616,15.5237164035921,6.02145886911737));
#131801=CARTESIAN_POINT('Ctrl Pts',(15.7714817724414,15.5384553983814,6.0062997565654));
#131802=CARTESIAN_POINT('Ctrl Pts',(15.7704021037596,15.5468443575775,5.99722717935986));
#131803=CARTESIAN_POINT('Ctrl Pts',(15.7641627705108,15.5935830044438,5.9440658717889));
#131804=CARTESIAN_POINT('Ctrl Pts',(15.7588025787515,15.6268161495871,5.89577003024519));
#131805=CARTESIAN_POINT('Ctrl Pts',(15.7507180476973,15.6677859271082,5.81789665067658));
#131806=CARTESIAN_POINT('Ctrl Pts',(15.7480099981808,15.6799778555234,5.79090686942623));
#131807=CARTESIAN_POINT('Ctrl Pts',(15.7445678118916,15.6936997237978,5.75491447568632));
#131808=CARTESIAN_POINT('Ctrl Pts',(15.743776190196,15.6967287314128,5.74651530092497));
#131809=CARTESIAN_POINT('Ctrl Pts',(15.7425308521589,15.7012987426797,5.73308521615288));
#131810=CARTESIAN_POINT('Ctrl Pts',(15.742072049724,15.7029394151296,5.72808951879469));
#131811=CARTESIAN_POINT('Ctrl Pts',(15.7412160550945,15.7059210373339,5.71867287229715));
#131812=CARTESIAN_POINT('Ctrl Pts',(15.7408181712773,15.7072741113623,5.71425608763402));
#131813=CARTESIAN_POINT('Ctrl Pts',(15.7397162535129,15.7109266705092,5.7019213794533));
#131814=CARTESIAN_POINT('Ctrl Pts',(15.7390170834389,15.7131352992562,5.69397689857699));
#131815=CARTESIAN_POINT('Ctrl Pts',(15.73432834209,15.7271682758949,5.64001605048752));
#131816=CARTESIAN_POINT('Ctrl Pts',(15.7305310489525,15.7346659320182,5.5929818598551));
#131817=CARTESIAN_POINT('Ctrl Pts',(15.7235690116083,15.73999487045,5.50668397483167));
#131818=CARTESIAN_POINT('Ctrl Pts',(15.7204252805073,15.7393193074721,5.46769670588419));
#131819=CARTESIAN_POINT('Ctrl Pts',(15.7160592723548,15.734263861582,5.4153601122154));
#131820=CARTESIAN_POINT('Ctrl Pts',(15.7149162485942,15.7325753183973,5.40181301453608));
#131821=CARTESIAN_POINT('Ctrl Pts',(15.7129999858034,15.7291516524742,5.37941813497513));
#131822=CARTESIAN_POINT('Ctrl Pts',(15.7122333806722,15.7276279850374,5.37054105394538));
#131823=CARTESIAN_POINT('Ctrl Pts',(15.7106896388498,15.7242563918933,5.35284413076323));
#131824=CARTESIAN_POINT('Ctrl Pts',(15.7099126310405,15.7224086223868,5.34402584292082));
#131825=CARTESIAN_POINT('Ctrl Pts',(15.707943983482,15.7173532945442,5.32192128758176));
#131826=CARTESIAN_POINT('Ctrl Pts',(15.7067460308474,15.7139376416921,5.30868673148448));
#131827=CARTESIAN_POINT('Ctrl Pts',(15.7014591269118,15.6974073647799,5.25126728076949));
#131828=CARTESIAN_POINT('Ctrl Pts',(15.69725718942,15.6805447449814,5.20827688946693));
#131829=CARTESIAN_POINT('Ctrl Pts',(15.6894208780699,15.6421426175256,5.13215544570545));
#131830=CARTESIAN_POINT('Ctrl Pts',(15.6858099063898,15.6217346401265,5.09862314291903));
#131831=CARTESIAN_POINT('Ctrl Pts',(15.6815177101152,15.5935758700741,5.05969673935276));
#131832=CARTESIAN_POINT('Ctrl Pts',(15.6807333565859,15.5882617040098,5.05262156511884));
#131833=CARTESIAN_POINT('Ctrl Pts',(15.6794966561937,15.5795987355904,5.04150923696917));
#131834=CARTESIAN_POINT('Ctrl Pts',(15.6790393356279,15.5763320199259,5.0374095952544));
#131835=CARTESIAN_POINT('Ctrl Pts',(15.6781271835534,15.5696846613527,5.02924707667916));
#131836=CARTESIAN_POINT('Ctrl Pts',(15.6776724222115,15.5663035097473,5.02518501657882));
#131837=CARTESIAN_POINT('Ctrl Pts',(15.6764457854826,15.5570086501147,5.01425887489405));
#131838=CARTESIAN_POINT('Ctrl Pts',(15.6756794860002,15.5510115820901,5.00746641086904));
#131839=CARTESIAN_POINT('Ctrl Pts',(15.6716645065889,15.518660045634,4.97215483501962));
#131840=CARTESIAN_POINT('Ctrl Pts',(15.6685364360735,15.4902097312988,4.94563184997997));
#131841=CARTESIAN_POINT('Ctrl Pts',(15.6619999284044,15.4266539133024,4.89511954841005));
#131842=CARTESIAN_POINT('Ctrl Pts',(15.6586018071178,15.3913056073004,4.87167417419855));
#131843=CARTESIAN_POINT('Ctrl Pts',(15.6538154691473,15.3404796579314,4.84392296378181));
#131844=CARTESIAN_POINT('Ctrl Pts',(15.6525166773131,15.3265811729723,4.83689507318885));
#131845=CARTESIAN_POINT('Ctrl Pts',(15.6504135864206,15.3039914842732,4.82635487462265));
#131846=CARTESIAN_POINT('Ctrl Pts',(15.6496189427168,15.2954369557246,4.82255954814017));
#131847=CARTESIAN_POINT('Ctrl Pts',(15.6480687490371,15.2787290032232,4.81552349599436));
#131848=CARTESIAN_POINT('Ctrl Pts',(15.6473139943061,15.270585361286,4.8122635027787));
#131849=CARTESIAN_POINT('Ctrl Pts',(15.6454938928568,15.2509389101029,4.8048017541583));
#131850=CARTESIAN_POINT('Ctrl Pts',(15.6444241997129,15.2393863232312,4.80073961452834));
#131851=CARTESIAN_POINT('Ctrl Pts',(15.6381294417354,15.1714237059104,4.7787239738254));
#131852=CARTESIAN_POINT('Ctrl Pts',(15.6326973553008,15.1131315559367,4.76731763296795));
#131853=CARTESIAN_POINT('Ctrl Pts',(15.6245815824239,15.0250248309666,4.76084790327428));
#131854=CARTESIAN_POINT('Ctrl Pts',(15.621912349062,14.9958260197347,4.76043593965468));
#131855=CARTESIAN_POINT('Ctrl Pts',(15.6185120151877,14.9578077307438,4.76215202850299));
#131856=CARTESIAN_POINT('Ctrl Pts',(15.6177248847222,14.9489461998596,4.76271216757074));
#131857=CARTESIAN_POINT('Ctrl Pts',(15.616484884843,14.9348658291116,4.76385729725892));
#131858=CARTESIAN_POINT('Ctrl Pts',(15.6160269988506,14.9296397474941,4.76433840696036));
#131859=CARTESIAN_POINT('Ctrl Pts',(15.6151148265101,14.9191684264645,4.76541500398255));
#131860=CARTESIAN_POINT('Ctrl Pts',(15.6146605973175,14.9139235589778,4.76601109587703));
#131861=CARTESIAN_POINT('Ctrl Pts',(15.6134371707002,14.8997267705813,4.76777887313962));
#131862=CARTESIAN_POINT('Ctrl Pts',(15.6126734997449,14.8907888279233,4.76905852359377));
#131863=CARTESIAN_POINT('Ctrl Pts',(15.6087034449563,14.844048107674,4.77662701672887));
#131864=CARTESIAN_POINT('Ctrl Pts',(15.6056145689812,14.8067483662577,4.78568626445037));
#131865=CARTESIAN_POINT('Ctrl Pts',(15.5998676150899,14.738911608855,4.80786887622241));
#131866=CARTESIAN_POINT('Ctrl Pts',(15.5972155188678,14.7082337112476,4.82023173734152));
#131867=CARTESIAN_POINT('Ctrl Pts',(15.5932730728649,14.6648178000812,4.84120992372543));
#131868=CARTESIAN_POINT('Ctrl Pts',(15.5920227810439,14.6513562063296,4.84823399674612));
#131869=CARTESIAN_POINT('Ctrl Pts',(15.5896861642823,14.6268708246815,4.86198580402747));
#131870=CARTESIAN_POINT('Ctrl Pts',(15.5886038061238,14.6157885938362,4.86859755293151));
#131871=CARTESIAN_POINT('Ctrl Pts',(15.5867594510494,14.597384133368,4.88024176932054));
#131872=CARTESIAN_POINT('Ctrl Pts',(15.5860030170607,14.5899689897489,4.88512248649213));
#131873=CARTESIAN_POINT('Ctrl Pts',(15.5845485893017,14.5759765400734,4.89469811029625));
#131874=CARTESIAN_POINT('Ctrl Pts',(15.5838515498125,14.5693847607987,4.89936968382915));
#131875=CARTESIAN_POINT('Ctrl Pts',(15.5819814551295,14.5520117130343,4.9121148997504));
#131876=CARTESIAN_POINT('Ctrl Pts',(15.5808014029495,14.5413728983271,4.92037639269052));
#131877=CARTESIAN_POINT('Ctrl Pts',(15.5752414288283,14.4927873596902,4.96028040105452));
#131878=CARTESIAN_POINT('Ctrl Pts',(15.5707282547691,14.4578560089472,4.99538131067525));
#131879=CARTESIAN_POINT('Ctrl Pts',(15.5628121500631,14.4035241476881,5.06218069271082));
#131880=CARTESIAN_POINT('Ctrl Pts',(15.5594355344606,14.3825082743107,5.09235589864732));
#131881=CARTESIAN_POINT('Ctrl Pts',(15.5553877287887,14.3594366857689,5.13138924417488));
#131882=CARTESIAN_POINT('Ctrl Pts',(15.5546243149542,14.3551819463905,5.13888374911916));
#131883=CARTESIAN_POINT('Ctrl Pts',(15.5534124617848,14.3485734599106,5.15101367562257));
#131884=CARTESIAN_POINT('Ctrl Pts',(15.5529593695649,14.3461359610775,5.15560224076619));
#131885=CARTESIAN_POINT('Ctrl Pts',(15.5520470652589,14.3412931010373,5.16495566981849));
#131886=CARTESIAN_POINT('Ctrl Pts',(15.5515880253884,14.3388905716795,5.16972161546449));
#131887=CARTESIAN_POINT('Ctrl Pts',(15.5503355135044,14.332436059173,5.182878262787));
#131888=CARTESIAN_POINT('Ctrl Pts',(15.5495480222946,14.3284906143905,5.19132058498329));
#131889=CARTESIAN_POINT('Ctrl Pts',(15.5457817983754,14.310227132208,5.23240886148132));
#131890=CARTESIAN_POINT('Ctrl Pts',(15.5429020260804,14.2981223222434,5.26599135512854));
#131891=CARTESIAN_POINT('Ctrl Pts',(15.537254796242,14.2791807946754,5.33348518422662));
#131892=CARTESIAN_POINT('Ctrl Pts',(15.5344934406337,14.2722040533432,5.36725815972864));
#131893=CARTESIAN_POINT('Ctrl Pts',(15.5308147946604,14.2661962629926,5.41188048874733));
#131894=CARTESIAN_POINT('Ctrl Pts',(15.5299459220278,14.265009784337,5.42239627363822));
#131895=CARTESIAN_POINT('Ctrl Pts',(15.5277834975326,14.2626353941577,5.44845151526249));
#131896=CARTESIAN_POINT('Ctrl Pts',(15.5264838396102,14.261712521617,5.46400918246762));
#131897=CARTESIAN_POINT('Ctrl Pts',(15.5243797063117,14.2610234839208,5.48894002377559));
#131898=CARTESIAN_POINT('Ctrl Pts',(15.5235849042555,14.2609426892394,5.49830030569007));
#131899=CARTESIAN_POINT('Ctrl Pts',(15.5220346326109,14.2611305938584,5.51642945676641));
#131900=CARTESIAN_POINT('Ctrl Pts',(15.5212799615315,14.2613776184711,5.52519701311198));
#131901=CARTESIAN_POINT('Ctrl Pts',(15.5194604612362,14.2623430014501,5.5461838443705));
#131902=CARTESIAN_POINT('Ctrl Pts',(15.5183912932982,14.2632089988482,5.55839329141341));
#131903=CARTESIAN_POINT('Ctrl Pts',(15.5120936328619,14.2700347783098,5.62954040220463));
#131904=CARTESIAN_POINT('Ctrl Pts',(15.5066577747397,14.282760120173,5.68760036365243));
#131905=CARTESIAN_POINT('Ctrl Pts',(15.5010403239809,14.3029090446194,5.74533437517337));
#131906=CARTESIAN_POINT('Ctrl Pts',(15.5008623455759,14.3035547805997,5.74716150870291));
#131907=CARTESIAN_POINT('Ctrl Pts',(15.5006844331709,14.3042076645986,5.7489859955834));
#131908=CARTESIAN_POINT('',(15.4440687571878,14.2608033075753,5.50047868038583));
#131909=CARTESIAN_POINT('Ctrl Pts',(15.4218039449815,14.3042130191175,5.74898305899438));
#131910=CARTESIAN_POINT('Ctrl Pts',(15.424802386429,14.2929616929186,5.71778320195144));
#131911=CARTESIAN_POINT('Ctrl Pts',(15.4278094459352,14.2838229275677,5.68586179826189));
#131912=CARTESIAN_POINT('Ctrl Pts',(15.4307689392091,14.2768967474548,5.65352289190575));
#131913=CARTESIAN_POINT('Ctrl Pts',(15.4328487506394,14.2720293099464,5.63079642461635));
#131914=CARTESIAN_POINT('Ctrl Pts',(15.434904548357,14.2682540029085,5.6078641606579));
#131915=CARTESIAN_POINT('Ctrl Pts',(15.4369125409172,14.2655940059027,5.58483839126259));
#131916=CARTESIAN_POINT('Ctrl Pts',(15.4393520146978,14.2623624237341,5.55686480120453));
#131917=CARTESIAN_POINT('Ctrl Pts',(15.4417246722218,14.2607667042999,5.52869421490943));
#131918=CARTESIAN_POINT('Ctrl Pts',(15.4440687571363,14.2608033075744,5.5004786810059));
#131919=CARTESIAN_POINT('Ctrl Pts',(15.4440687571967,14.2608033075754,5.50047868027838));
#131920=CARTESIAN_POINT('Ctrl Pts',(15.4467761069373,14.2608455833229,5.46789056116125));
#131921=CARTESIAN_POINT('Ctrl Pts',(15.4494469348908,14.2630684344419,5.43522701256568));
#131922=CARTESIAN_POINT('Ctrl Pts',(15.4521278841484,14.2674494715339,5.40280611817825));
#131923=CARTESIAN_POINT('Ctrl Pts',(15.4548051655613,14.2718245148668,5.37042957927693));
#131924=CARTESIAN_POINT('Ctrl Pts',(15.4574930545461,14.2783512841037,5.33829519427106));
#131925=CARTESIAN_POINT('Ctrl Pts',(15.4602226997084,14.2869647716622,5.3067066159124));
#131926=CARTESIAN_POINT('Ctrl Pts',(15.4629502225471,14.2955715621569,5.27514259795625));
#131927=CARTESIAN_POINT('Ctrl Pts',(15.4657196952501,14.3062614877415,5.2441235989032));
#131928=CARTESIAN_POINT('Ctrl Pts',(15.4685412005376,14.3189337096865,5.21393790265118));
#131929=CARTESIAN_POINT('Ctrl Pts',(15.471364285272,14.3316130253987,5.18373530878646));
#131930=CARTESIAN_POINT('Ctrl Pts',(15.4742395361271,14.3462767111684,5.15436699216516));
#131931=CARTESIAN_POINT('Ctrl Pts',(15.4771535537219,14.3627913473154,5.12610630435767));
#131932=CARTESIAN_POINT('Ctrl Pts',(15.4800683726115,14.3793105246475,5.09783784544275));
#131933=CARTESIAN_POINT('Ctrl Pts',(15.4830218659706,14.3976817340025,5.07067768020242));
#131934=CARTESIAN_POINT('Ctrl Pts',(15.4859773680107,14.4177397040656,5.04488329105562));
#131935=CARTESIAN_POINT('Ctrl Pts',(15.4889386844745,14.4378371346109,5.01903815604416));
#131936=CARTESIAN_POINT('Ctrl Pts',(15.4919016374085,14.4596283158344,4.99456436472374));
#131937=CARTESIAN_POINT('Ctrl Pts',(15.4948095761129,14.4829120894533,4.97170310431067));
#131938=CARTESIAN_POINT('Ctrl Pts',(15.4965131315522,14.4965524042007,4.95831031014164));
#131939=CARTESIAN_POINT('Ctrl Pts',(15.4981974437974,14.5107042977867,4.94547060155898));
#131940=CARTESIAN_POINT('Ctrl Pts',(15.499849108333,14.5253208329636,4.93322896563607));
#131941=CARTESIAN_POINT('Ctrl Pts',(15.4998503674193,14.5253319753473,4.93321963367046));
#131942=CARTESIAN_POINT('Ctrl Pts',(15.4998516264888,14.5253431180245,4.93321030203082));
#131943=CARTESIAN_POINT('Ctrl Pts',(15.4998528855414,14.5253542609955,4.93320097071717));
#131944=CARTESIAN_POINT('Ctrl Pts',(15.5024416396342,14.5482654650402,4.91401473820545));
#131945=CARTESIAN_POINT('Ctrl Pts',(15.5049591237203,14.5724224611895,4.89620646031482));
#131946=CARTESIAN_POINT('Ctrl Pts',(15.50744630092,14.5976235007547,4.87992268447526));
#131947=CARTESIAN_POINT('Ctrl Pts',(15.5077029580282,14.6002240496569,4.8782423269934));
#131948=CARTESIAN_POINT('Ctrl Pts',(15.5079592924099,14.6028356704184,4.87657820375011));
#131949=CARTESIAN_POINT('Ctrl Pts',(15.5082153490777,14.6054581098794,4.8749304750595));
#131950=CARTESIAN_POINT('Ctrl Pts',(15.510949630506,14.6334616279128,4.85733533100091));
#131951=CARTESIAN_POINT('Ctrl Pts',(15.5136530819958,14.662704380166,4.84160919125144));
#131952=CARTESIAN_POINT('Ctrl Pts',(15.5163726786914,14.6928951544079,4.82789849849688));
#131953=CARTESIAN_POINT('Ctrl Pts',(15.5190894721413,14.7230548092714,4.81420193814694));
#131954=CARTESIAN_POINT('Ctrl Pts',(15.5218228580752,14.7541601598289,4.8025162421249));
#131955=CARTESIAN_POINT('Ctrl Pts',(15.5246020513376,14.78591151766,4.79294486361158));
#131956=CARTESIAN_POINT('Ctrl Pts',(15.5273799199213,14.8176477414778,4.78337804721402));
#131957=CARTESIAN_POINT('Ctrl Pts',(15.5302037769629,14.8500291864702,4.7759232651959));
#131958=CARTESIAN_POINT('Ctrl Pts',(15.5330799958899,14.8827511640677,4.77064655546633));
#131959=CARTESIAN_POINT('Ctrl Pts',(15.5359585666809,14.9154998981965,4.76536553100827));
#131960=CARTESIAN_POINT('Ctrl Pts',(15.5388896266881,14.9485896780001,4.76226605249483));
#131961=CARTESIAN_POINT('Ctrl Pts',(15.5418547451026,14.9817112101536,4.76137967478786));
#131962=CARTESIAN_POINT('Ctrl Pts',(15.5448212827776,15.0148485960011,4.76049287281426));
#131963=CARTESIAN_POINT('Ctrl Pts',(15.5478217485722,15.0480178284823,4.76182142709274));
#131964=CARTESIAN_POINT('Ctrl Pts',(15.5508137028031,15.0809051395052,4.76536202564308));
#131965=CARTESIAN_POINT('Ctrl Pts',(15.5538114590812,15.1138562261454,4.76890949018067));
#131966=CARTESIAN_POINT('Ctrl Pts',(15.5568001982077,15.1465243774485,4.77467809640339));
#131967=CARTESIAN_POINT('Ctrl Pts',(15.5597177765166,15.1785886845052,4.78262475853342));
#131968=CARTESIAN_POINT('Ctrl Pts',(15.5607505018425,15.1899383788234,4.78543761164969));
#131969=CARTESIAN_POINT('Ctrl Pts',(15.561774171273,15.2012123622676,4.78852295534572));
#131970=CARTESIAN_POINT('Ctrl Pts',(15.5627856754207,15.2123962407999,4.79187744433514));
#131971=CARTESIAN_POINT('Ctrl Pts',(15.5627869345069,15.2124101621135,4.79188161988956));
#131972=CARTESIAN_POINT('Ctrl Pts',(15.5627881935762,15.2124240833164,4.79188579586848));
#131973=CARTESIAN_POINT('Ctrl Pts',(15.5627894526286,15.2124380044084,4.79188997227193));
#131974=CARTESIAN_POINT('Ctrl Pts',(15.5653782067486,15.2410613434249,4.80047712991141));
#131975=CARTESIAN_POINT('Ctrl Pts',(15.5678956908651,15.2692187376239,4.81086252349366));
#131976=CARTESIAN_POINT('Ctrl Pts',(15.5703828680978,15.2966768492142,4.82295822031119));
#131977=CARTESIAN_POINT('Ctrl Pts',(15.570639525199,15.299510310068,4.82420640095606));
#131978=CARTESIAN_POINT('Ctrl Pts',(15.5708958595738,15.3023362990345,4.82547275596272));
#131979=CARTESIAN_POINT('Ctrl Pts',(15.5711519162349,15.3051545430087,4.82675716202661));
#131980=CARTESIAN_POINT('Ctrl Pts',(15.5738861976904,15.3352489455728,4.84047259386885));
#131981=CARTESIAN_POINT('Ctrl Pts',(15.5765896492107,15.3644636433141,4.8562507903979));
#131982=CARTESIAN_POINT('Ctrl Pts',(15.5793092459387,15.3925161939256,4.8739290360027));
#131983=CARTESIAN_POINT('Ctrl Pts',(15.5820260394214,15.4205398291541,4.8915890596195));
#131984=CARTESIAN_POINT('Ctrl Pts',(15.5847594253902,15.447403865845,4.91114466944784));
#131985=CARTESIAN_POINT('Ctrl Pts',(15.5875386186879,15.4728571084234,4.93240243204717));
#131986=CARTESIAN_POINT('Ctrl Pts',(15.5903164873072,15.498298218935,4.95365006231873));
#131987=CARTESIAN_POINT('Ctrl Pts',(15.5931403443849,15.5223300100993,4.97659793337382));
#131988=CARTESIAN_POINT('Ctrl Pts',(15.5960165633468,15.5447297884591,5.00102786236099));
#131989=CARTESIAN_POINT('Ctrl Pts',(15.598895134173,15.5671478829627,5.02547776753224));
#131990=CARTESIAN_POINT('Ctrl Pts',(15.6018261942143,15.5879313453698,5.05141206919082));
#131991=CARTESIAN_POINT('Ctrl Pts',(15.6047913126597,15.6068837525801,5.07858977762999));
#131992=CARTESIAN_POINT('Ctrl Pts',(15.6077578503658,15.6258452314031,5.1057804947409));
#131993=CARTESIAN_POINT('Ctrl Pts',(15.6107583161885,15.6429738229881,5.13421593755292));
#131994=CARTESIAN_POINT('Ctrl Pts',(15.6137502704426,15.6580997666351,5.16363220704589));
#131995=CARTESIAN_POINT('Ctrl Pts',(15.6167480267439,15.6732550427619,5.19310552105464));
#131996=CARTESIAN_POINT('Ctrl Pts',(15.6197367658887,15.6863995147595,5.22356381715342));
#131997=CARTESIAN_POINT('Ctrl Pts',(15.6226543442097,15.6973927169695,5.25471536204762));
#131998=CARTESIAN_POINT('Ctrl Pts',(15.6236870693484,15.7012839428522,5.26574196698586));
#131999=CARTESIAN_POINT('Ctrl Pts',(15.6247107385943,15.7049059383463,5.27685516403632));
#132000=CARTESIAN_POINT('Ctrl Pts',(15.6257222425617,15.7082535829996,5.28804109102039));
#132001=CARTESIAN_POINT('Ctrl Pts',(15.6257235016478,15.7082577500349,5.28805501488569));
#132002=CARTESIAN_POINT('Ctrl Pts',(15.625724760717,15.7082619166548,5.28806893889187));
#132003=CARTESIAN_POINT('Ctrl Pts',(15.6257260197694,15.7082660828591,5.2880828630389));
#132004=CARTESIAN_POINT('Ctrl Pts',(15.6283147738787,15.71683227034,5.31671248476454));
#132005=CARTESIAN_POINT('Ctrl Pts',(15.630832257985,15.7236402612103,5.34594169111475));
#132006=CARTESIAN_POINT('Ctrl Pts',(15.6333194352083,15.7286352001015,5.37552723412128));
#132007=CARTESIAN_POINT('Ctrl Pts',(15.6335760923015,15.7291506384404,5.37858022905785));
#132008=CARTESIAN_POINT('Ctrl Pts',(15.6338324266685,15.7296467880078,5.3816369762964));
#132009=CARTESIAN_POINT('Ctrl Pts',(15.6340884833215,15.7301236016266,5.38469717992357));
#132010=CARTESIAN_POINT('Ctrl Pts',(15.6368227647599,15.7352152194844,5.41737533092954));
#132011=CARTESIAN_POINT('Ctrl Pts',(15.6395262162643,15.7381001823414,5.45045292196372));
#132012=CARTESIAN_POINT('Ctrl Pts',(15.6422458129776,15.738759097609,5.48360457024803));
#132013=CARTESIAN_POINT('Ctrl Pts',(15.6449626064454,15.7394173336945,5.51672204721309));
#132014=CARTESIAN_POINT('Ctrl Pts',(15.6476959924004,15.7378546511993,5.54991325623536));
#132015=CARTESIAN_POINT('Ctrl Pts',(15.6504751856855,15.7340944960883,5.58286202331587));
#132016=CARTESIAN_POINT('Ctrl Pts',(15.653253054292,15.7303361332227,5.61579508565123));
#132017=CARTESIAN_POINT('Ctrl Pts',(15.6560769113579,15.7243827056555,5.64848588654057));
#132018=CARTESIAN_POINT('Ctrl Pts',(15.658953130309,15.7162940035838,5.68062845006448));
#132019=CARTESIAN_POINT('Ctrl Pts',(15.6618317011244,15.7081986874365,5.71279729633989));
#132020=CARTESIAN_POINT('Ctrl Pts',(15.6647627611558,15.6979647032516,5.74441700332746));
#132021=CARTESIAN_POINT('Ctrl Pts',(15.6677278795925,15.6856853357742,5.77519099721236));
#132022=CARTESIAN_POINT('Ctrl Pts',(15.6706944172898,15.67340009075,5.80597972113861));
#132023=CARTESIAN_POINT('Ctrl Pts',(15.6736948831047,15.6590673534345,5.83592192694714));
#132024=CARTESIAN_POINT('Ctrl Pts',(15.6766868373524,15.6428142042667,5.8647307140484));
#132025=CARTESIAN_POINT('Ctrl Pts',(15.6796845936473,15.6265295367228,5.89359536762682));
#132026=CARTESIAN_POINT('Ctrl Pts',(15.6826733327871,15.6083165017546,5.92132207483228));
#132027=CARTESIAN_POINT('Ctrl Pts',(15.6855909111045,15.5883415366898,5.94763309922456));
#132028=CARTESIAN_POINT('Ctrl Pts',(15.686623636346,15.5812710664653,5.95694632274894));
#132029=CARTESIAN_POINT('Ctrl Pts',(15.6876473056931,15.573980231511,5.96608228202831));
#132030=CARTESIAN_POINT('Ctrl Pts',(15.6886588097591,15.5664777948433,5.97502907795765));
#132031=CARTESIAN_POINT('Ctrl Pts',(15.6886600688453,15.566468456063,5.97504021462768));
#132032=CARTESIAN_POINT('Ctrl Pts',(15.6886613279146,15.5664591169365,5.97505135102813));
#132033=CARTESIAN_POINT('Ctrl Pts',(15.6886625869671,15.566449777464,5.97506248715896));
#132034=CARTESIAN_POINT('Ctrl Pts',(15.6912513410761,15.5472467664899,5.99795963052945));
#132035=CARTESIAN_POINT('Ctrl Pts',(15.6937688251809,15.526576192724,6.01971790758887));
#132036=CARTESIAN_POINT('Ctrl Pts',(15.6962560024016,15.5046110689217,6.04015774865318));
#132037=CARTESIAN_POINT('Ctrl Pts',(15.6965126595003,15.5023444411552,6.04226697925511));
#132038=CARTESIAN_POINT('Ctrl Pts',(15.6967689938728,15.5000640732066,6.04436216194234));
#132039=CARTESIAN_POINT('Ctrl Pts',(15.6970250505313,15.4977701863,6.04644309460028));
#132040=CARTESIAN_POINT('Ctrl Pts',(15.6997593319722,15.4732750904425,6.06866417480348));
#132041=CARTESIAN_POINT('Ctrl Pts',(15.7024627834775,15.4472330172999,6.08926175880403));
#132042=CARTESIAN_POINT('Ctrl Pts',(15.7051823801906,15.4199050829409,6.10804073529059));
#132043=CARTESIAN_POINT('Ctrl Pts',(15.7078991736582,15.392605317063,6.12680035520093));
#132044=CARTESIAN_POINT('Ctrl Pts',(15.7106325596118,15.3640227818022,6.14374547284348));
#132045=CARTESIAN_POINT('Ctrl Pts',(15.7134117528947,15.3344344565109,6.15872182172957));
#132046=CARTESIAN_POINT('Ctrl Pts',(15.7161896214991,15.3048602342394,6.17369103226823));
#132047=CARTESIAN_POINT('Ctrl Pts',(15.7190134785621,15.274281395181,6.18669358453111));
#132048=CARTESIAN_POINT('Ctrl Pts',(15.7218896975101,15.2429863847113,6.19761117637783));
#132049=CARTESIAN_POINT('Ctrl Pts',(15.7247682683224,15.211665784529,6.20853769546355));
#132050=CARTESIAN_POINT('Ctrl Pts',(15.7276993283503,15.1796279003228,6.21737592372426));
#132051=CARTESIAN_POINT('Ctrl Pts',(15.7306644467838,15.1471717414236,6.22404070546988));
#132052=CARTESIAN_POINT('Ctrl Pts',(15.7336309844779,15.1147000473112,6.23070867732821));
#132053=CARTESIAN_POINT('Ctrl Pts',(15.7366314502898,15.0818095912583,6.23520099846741));
#132054=CARTESIAN_POINT('Ctrl Pts',(15.739623404535,15.0488098856814,6.23746606025999));
#132055=CARTESIAN_POINT('Ctrl Pts',(15.7426211608274,15.0157461865294,6.23973551449787));
#132056=CARTESIAN_POINT('Ctrl Pts',(15.7456098999652,14.9825726452173,6.23976857485775));
#132057=CARTESIAN_POINT('Ctrl Pts',(15.7485274782814,14.9496127603104,6.23755154489927));
#132058=CARTESIAN_POINT('Ctrl Pts',(15.7495602035142,14.9379460624109,6.23676679037623));
#132059=CARTESIAN_POINT('Ctrl Pts',(15.7505838728528,14.9263062575021,6.23570050434283));
#132060=CARTESIAN_POINT('Ctrl Pts',(15.7515953769107,14.9147081028205,6.23435346340884));
#132061=CARTESIAN_POINT('Ctrl Pts',(15.7515966359968,14.9146936658287,6.23435178665771));
#132062=CARTESIAN_POINT('Ctrl Pts',(15.7515978950661,14.9146792288718,6.23435010946924));
#132063=CARTESIAN_POINT('Ctrl Pts',(15.7515991541185,14.9146647919497,6.23434843184341));
#132064=CARTESIAN_POINT('Ctrl Pts',(15.7541879082306,14.8849808480094,6.23089904346463));
#132065=CARTESIAN_POINT('Ctrl Pts',(15.756705392339,14.8554412061881,6.22559764700203));
#132066=CARTESIAN_POINT('Ctrl Pts',(15.7591925695637,14.8262909858308,6.21849001572236));
#132067=CARTESIAN_POINT('Ctrl Pts',(15.7594492266614,14.8232829127114,6.21775656416238));
#132068=CARTESIAN_POINT('Ctrl Pts',(15.7597055610327,14.8202790181393,6.21700391165846));
#132069=CARTESIAN_POINT('Ctrl Pts',(15.7599616176902,14.8172795925739,6.21623213185643));
#132070=CARTESIAN_POINT('Ctrl Pts',(15.7626958991342,14.7852504559489,6.20799074023513));
#132071=CARTESIAN_POINT('Ctrl Pts',(15.7653993506432,14.7537267468749,6.19756453245429));
#132072=CARTESIAN_POINT('Ctrl Pts',(15.7681189473603,14.7230150100721,6.18506432529857));
#132073=CARTESIAN_POINT('Ctrl Pts',(15.7708357408319,14.6923349296306,6.17257700282843));
#132074=CARTESIAN_POINT('Ctrl Pts',(15.7735691267899,14.662465092574,6.15802052075943));
#132075=CARTESIAN_POINT('Ctrl Pts',(15.7763483200773,14.6336866500919,6.14154140458493));
#132076=CARTESIAN_POINT('Ctrl Pts',(15.7791261886863,14.6049219246054,6.1250701430386));
#132077=CARTESIAN_POINT('Ctrl Pts',(15.7819500457541,14.5772474760076,6.10667838780921));
#132078=CARTESIAN_POINT('Ctrl Pts',(15.7848262647067,14.5509207205642,6.08654201668866));
#132079=CARTESIAN_POINT('Ctrl Pts',(15.7877048355236,14.5245724379154,6.06638918019703));
#132080=CARTESIAN_POINT('Ctrl Pts',(15.7906358955561,14.4995740184021,6.04448896725036));
#132081=CARTESIAN_POINT('Ctrl Pts',(15.7936010139937,14.4761610010362,6.02104430504163));
#132082=CARTESIAN_POINT('Ctrl Pts',(15.7965675516919,14.4527367769768,5.9975884209926));
#132083=CARTESIAN_POINT('Ctrl Pts',(15.7995680175075,14.4308995282325,5.97258646870972));
#132084=CARTESIAN_POINT('Ctrl Pts',(15.8025599717558,14.4108625484769,5.94626859422399));
#132085=CARTESIAN_POINT('Ctrl Pts',(15.8055577280513,14.3907867126787,5.91989968368066));
#132086=CARTESIAN_POINT('Ctrl Pts',(15.8085464671915,14.372518449713,5.89220933325829));
#132087=CARTESIAN_POINT('Ctrl Pts',(15.8114640455094,14.3562470770825,5.86346021727603));
#132088=CARTESIAN_POINT('Ctrl Pts',(15.81249677072,14.3504875550075,5.85328399109664));
#132089=CARTESIAN_POINT('Ctrl Pts',(15.8135204400367,14.3449779721579,5.84297542595422));
#132090=CARTESIAN_POINT('Ctrl Pts',(15.8145319440733,14.3397257942077,5.83254727499866));
#132091=CARTESIAN_POINT('Ctrl Pts',(15.8145332031598,14.3397192564715,5.83253429438356));
#132092=CARTESIAN_POINT('Ctrl Pts',(15.8145344622292,14.339712719122,5.83252131356128));
#132093=CARTESIAN_POINT('Ctrl Pts',(15.8145357212814,14.3397061821593,5.83250833253183));
#132094=CARTESIAN_POINT('Ctrl Pts',(15.8171533011343,14.3261157829449,5.80552066556783));
#132095=CARTESIAN_POINT('Ctrl Pts',(15.8196966394794,14.3141974283294,5.77763344311099));
#132096=CARTESIAN_POINT('Ctrl Pts',(15.8222092530609,14.3040405757782,5.7490739337915));
#132097=CARTESIAN_POINT('Origin',(13.2437274406976,15.,5.5));
#132098=CARTESIAN_POINT('',(16.3004622294836,14.3042076660467,5.7489859996302));
#132099=CARTESIAN_POINT('',(16.2213444347181,14.3044435251824,5.74885644548777));
#132100=CARTESIAN_POINT('',(13.2437274406976,14.3042076641721,5.74898599439144));
#132101=CARTESIAN_POINT('Ctrl Pts',(16.3004622294836,14.3042076679214,5.74898600486896));
#132102=CARTESIAN_POINT('Ctrl Pts',(16.2994517369524,14.3083860293658,5.76066245172471));
#132103=CARTESIAN_POINT('Ctrl Pts',(16.2984477733188,14.3128588604262,5.77223524884823));
#132104=CARTESIAN_POINT('Ctrl Pts',(16.2929454430558,14.3390315264409,5.83518931248759));
#132105=CARTESIAN_POINT('Ctrl Pts',(16.2885035166987,14.3661982337309,5.88409074977041));
#132106=CARTESIAN_POINT('Ctrl Pts',(16.2828018855551,14.4060020165941,5.93982887446734));
#132107=CARTESIAN_POINT('Ctrl Pts',(16.2817336435,14.4136657788038,5.94999464965032));
#132108=CARTESIAN_POINT('Ctrl Pts',(16.2799133217406,14.4270402699169,5.96681355123648));
#132109=CARTESIAN_POINT('Ctrl Pts',(16.2791666549248,14.4326139885565,5.97357242731626));
#132110=CARTESIAN_POINT('Ctrl Pts',(16.2776267006674,14.4442784741901,5.98721560616398));
#132111=CARTESIAN_POINT('Ctrl Pts',(16.2768330627778,14.450380141342,5.99408850973305));
#132112=CARTESIAN_POINT('Ctrl Pts',(16.274759435409,14.4665444102232,6.01162591928593));
#132113=CARTESIAN_POINT('Ctrl Pts',(16.2734716414276,14.476798521178,6.0221073584513));
#132114=CARTESIAN_POINT('Ctrl Pts',(16.2705622764027,14.5004203298335,6.04485787997494));
#132115=CARTESIAN_POINT('Ctrl Pts',(16.2689349142941,14.5139414905469,6.05695329495336));
#132116=CARTESIAN_POINT('Ctrl Pts',(16.2628065859188,14.5660075272807,6.10018830355885));
#132117=CARTESIAN_POINT('Ctrl Pts',(16.2582144284696,14.6072076165935,6.12792434102262));
#132118=CARTESIAN_POINT('Ctrl Pts',(16.2519397608728,14.6678688169862,6.16044075920834));
#132119=CARTESIAN_POINT('Ctrl Pts',(16.2501964108936,14.6852228537609,6.16888610813786));
#132120=CARTESIAN_POINT('Ctrl Pts',(16.2478605380079,14.709326048274,6.17946970058863));
#132121=CARTESIAN_POINT('Ctrl Pts',(16.2472410215083,14.7158032004805,6.1822042296793));
#132122=CARTESIAN_POINT('Ctrl Pts',(16.2461956952537,14.7268886467197,6.18669899219772));
#132123=CARTESIAN_POINT('Ctrl Pts',(16.2457673575847,14.7314771119835,6.18850619614771));
#132124=CARTESIAN_POINT('Ctrl Pts',(16.2448285044712,14.7416385581513,6.19239131391346));
#132125=CARTESIAN_POINT('Ctrl Pts',(16.2443191647446,14.7472190691158,6.19444810793961));
#132126=CARTESIAN_POINT('Ctrl Pts',(16.2427430721005,14.764679699825,6.20064514321187));
#132127=CARTESIAN_POINT('Ctrl Pts',(16.2416884022442,14.776641869792,6.20454982914273));
#132128=CARTESIAN_POINT('Ctrl Pts',(16.2398172509503,14.7982559150491,6.21099915045727));
#132129=CARTESIAN_POINT('Ctrl Pts',(16.2389969332587,14.807870113797,6.21365719647443));
#132130=CARTESIAN_POINT('Ctrl Pts',(16.234677573181,14.859063361113,6.22670102230444));
#132131=CARTESIAN_POINT('Ctrl Pts',(16.2312668776027,14.9014345153497,6.23365027564152));
#132132=CARTESIAN_POINT('Ctrl Pts',(16.227513995898,14.947678265039,6.23715385661125));
#132133=CARTESIAN_POINT('Ctrl Pts',(16.2272290538534,14.951187461355,6.23739454022586));
#132134=CARTESIAN_POINT('Ctrl Pts',(16.2246841239846,14.9825029434427,6.23931784241169));
#132135=CARTESIAN_POINT('Ctrl Pts',(16.2224024202493,15.0103788541925,6.23945182248278));
#132136=CARTESIAN_POINT('Ctrl Pts',(16.2191280149388,15.0495016434262,6.23742715382624));
#132137=CARTESIAN_POINT('Ctrl Pts',(16.2181745354255,15.0607943267638,6.23658213477939));
#132138=CARTESIAN_POINT('Ctrl Pts',(16.2164765984805,15.0806948903967,6.23463226694157));
#132139=CARTESIAN_POINT('Ctrl Pts',(16.2157355645625,15.0893112778201,6.23363459222357));
#132140=CARTESIAN_POINT('Ctrl Pts',(16.2141596971666,15.1074759079027,6.23120661578024));
#132141=CARTESIAN_POINT('Ctrl Pts',(16.213323881398,15.1170175919536,6.22974039876132));
#132142=CARTESIAN_POINT('Ctrl Pts',(16.2109833356914,15.1434632639723,6.22514466104485));
#132143=CARTESIAN_POINT('Ctrl Pts',(16.2094665257275,15.1602897243496,6.22161179777485));
#132144=CARTESIAN_POINT('Ctrl Pts',(16.2043397419378,15.21607839776,6.20785105990925));
#132145=CARTESIAN_POINT('Ctrl Pts',(16.2006587937955,15.2543211754153,6.19502723309645));
#132146=CARTESIAN_POINT('Ctrl Pts',(16.1934521527081,15.3263731291505,6.16412052970031));
#132147=CARTESIAN_POINT('Ctrl Pts',(16.1899398749359,15.3602094609348,6.14639399538106));
#132148=CARTESIAN_POINT('Ctrl Pts',(16.1857252512568,15.4001595372095,6.12134890298495));
#132149=CARTESIAN_POINT('Ctrl Pts',(16.1849264454501,15.4077028061472,6.11642563128004));
#132150=CARTESIAN_POINT('Ctrl Pts',(16.1836725673053,15.4195177080691,6.10840258587782));
#132151=CARTESIAN_POINT('Ctrl Pts',(16.1832122963809,15.4238491016908,6.10539306098997));
#132152=CARTESIAN_POINT('Ctrl Pts',(16.1822999433935,15.4324288427241,6.09929448456349));
#132153=CARTESIAN_POINT('Ctrl Pts',(16.1818478664713,15.4366772160495,6.09620600248864));
#132154=CARTESIAN_POINT('Ctrl Pts',(16.1806374201285,15.4480338803516,6.08776341003342));
#132155=CARTESIAN_POINT('Ctrl Pts',(16.1798843782696,15.4550792880145,6.08232555133863));
#132156=CARTESIAN_POINT('Ctrl Pts',(16.1766762745876,15.4849273452204,6.05841522031983));
#132157=CARTESIAN_POINT('Ctrl Pts',(16.1742877709097,15.5067194532521,6.03871878431391));
#132158=CARTESIAN_POINT('Ctrl Pts',(16.1671599541238,15.5685312217722,5.9757718637109));
#132159=CARTESIAN_POINT('Ctrl Pts',(16.1624818325113,15.6046066430114,5.92899486387698));
#132160=CARTESIAN_POINT('Ctrl Pts',(16.1565508664372,15.6410437584492,5.86787901320984));
#132161=CARTESIAN_POINT('Ctrl Pts',(16.1555182781162,15.6470731304854,5.85716718298428));
#132162=CARTESIAN_POINT('Ctrl Pts',(16.153732120129,15.6569461091196,5.83855557014548));
#132163=CARTESIAN_POINT('Ctrl Pts',(16.1529832734326,15.6609212494549,5.83072821505775));
#132164=CARTESIAN_POINT('Ctrl Pts',(16.151427344782,15.6688372745419,5.81442803510577));
#132165=CARTESIAN_POINT('Ctrl Pts',(16.1506197592493,15.6727587485998,5.80594760621321));
#132166=CARTESIAN_POINT('Ctrl Pts',(16.1484586982169,15.6827510787009,5.78321695762616));
#132167=CARTESIAN_POINT('Ctrl Pts',(16.1470960980081,15.6885361283502,5.76884717349373));
#132168=CARTESIAN_POINT('Ctrl Pts',(16.1431974357493,15.7036294570319,5.72766577761879));
#132169=CARTESIAN_POINT('Ctrl Pts',(16.14063083312,15.7118501264622,5.70048726058336));
#132170=CARTESIAN_POINT('Ctrl Pts',(16.1333611922224,15.7304593445063,5.62315946724311));
#132171=CARTESIAN_POINT('Ctrl Pts',(16.1286091628451,15.7372325108256,5.57230276390171));
#132172=CARTESIAN_POINT('Ctrl Pts',(16.1231163930742,15.7389859294872,5.51106993450556));
#132173=CARTESIAN_POINT('Ctrl Pts',(16.1222192695503,15.7390682070861,5.50098144736492));
#132174=CARTESIAN_POINT('Ctrl Pts',(16.1208490323358,15.7388762434804,5.48540427117969));
#132175=CARTESIAN_POINT('Ctrl Pts',(16.1203690880374,15.7387474241494,5.47991548355235));
#132176=CARTESIAN_POINT('Ctrl Pts',(16.1194506682585,15.7383813262252,5.46934187656149));
#132177=CARTESIAN_POINT('Ctrl Pts',(16.1190118194879,15.7381526675241,5.46425722848243));
#132178=CARTESIAN_POINT('Ctrl Pts',(16.1178846774055,15.7374260515046,5.45112430516183));
#132179=CARTESIAN_POINT('Ctrl Pts',(16.1172004730792,15.7368488511159,5.44308073742272));
#132180=CARTESIAN_POINT('Ctrl Pts',(16.1156800591803,15.7352609399702,5.42508406500585));
#132181=CARTESIAN_POINT('Ctrl Pts',(16.114847005266,15.7341795590782,5.41513865776079));
#132182=CARTESIAN_POINT('Ctrl Pts',(16.1121475273747,15.7299897172839,5.38274105617902));
#132183=CARTESIAN_POINT('Ctrl Pts',(16.1103088907729,15.7260502379792,5.36040823020972));
#132184=CARTESIAN_POINT('Ctrl Pts',(16.1039354346095,15.7087724728781,5.28336388715953));
#132185=CARTESIAN_POINT('Ctrl Pts',(16.099453702746,15.6902213510403,5.23003094407816));
#132186=CARTESIAN_POINT('Ctrl Pts',(16.0937134464031,15.6603054969069,5.16791887995087));
#132187=CARTESIAN_POINT('Ctrl Pts',(16.0926510421927,15.654521121012,5.1566586496617));
#132188=CARTESIAN_POINT('Ctrl Pts',(16.0908375506354,15.6442545999071,5.13787633009199));
#132189=CARTESIAN_POINT('Ctrl Pts',(16.0900917768073,15.6399226061558,5.13027498600969));
#132190=CARTESIAN_POINT('Ctrl Pts',(16.0885509856233,15.6307555689497,5.11483350634812));
#132191=CARTESIAN_POINT('Ctrl Pts',(16.087755583233,15.6259068700205,5.1070033220359));
#132192=CARTESIAN_POINT('Ctrl Pts',(16.085670895987,15.612906428095,5.0868599069873));
#132193=CARTESIAN_POINT('Ctrl Pts',(16.0843736437006,15.6045301393251,5.07469743833649));
#132194=CARTESIAN_POINT('Ctrl Pts',(16.0821946018103,15.5900018051966,5.05489913060011));
#132195=CARTESIAN_POINT('Ctrl Pts',(16.0813202022419,15.5840516577785,5.04711970995621));
#132196=CARTESIAN_POINT('Ctrl Pts',(16.0777183412289,15.5590533148954,5.01574826955821));
#132197=CARTESIAN_POINT('Ctrl Pts',(16.0749504526078,15.5387181570825,4.99322319274776));
#132198=CARTESIAN_POINT('Ctrl Pts',(16.0681965799785,15.4861752831793,4.94176780959381));
#132199=CARTESIAN_POINT('Ctrl Pts',(16.0642034676475,15.4526944752259,4.91428851100823));
#132200=CARTESIAN_POINT('Ctrl Pts',(16.0595658526669,15.4098179824205,4.8849829995674));
#132201=CARTESIAN_POINT('Ctrl Pts',(16.0587948830366,15.402548780796,4.88020068635026));
#132202=CARTESIAN_POINT('Ctrl Pts',(16.0575740714618,15.3907922703712,4.87276036027724));
#132203=CARTESIAN_POINT('Ctrl Pts',(16.0571194613647,15.3863585996155,4.87001968065359));
#132204=CARTESIAN_POINT('Ctrl Pts',(16.0562072769506,15.3773437510821,4.86457811825307));
#132205=CARTESIAN_POINT('Ctrl Pts',(16.0557498371956,15.3727616985852,4.86187932498903));
#132206=CARTESIAN_POINT('Ctrl Pts',(16.0545070172728,15.3601556106697,4.85463656913661));
#132207=CARTESIAN_POINT('Ctrl Pts',(16.0537274648998,15.3520746871094,4.8501927511099));
#132208=CARTESIAN_POINT('Ctrl Pts',(16.050260591106,15.3154516944331,4.83093711483149));
#132209=CARTESIAN_POINT('Ctrl Pts',(16.0476529092147,15.2860410521651,4.81784460919582));
#132210=CARTESIAN_POINT('Ctrl Pts',(16.0407098498805,15.2052851296335,4.7880406812357));
#132211=CARTESIAN_POINT('Ctrl Pts',(16.0364095748317,15.1528177150459,4.77496620498191));
#132212=CARTESIAN_POINT('Ctrl Pts',(16.0308455963803,15.0865407429377,4.76596999310194));
#132213=CARTESIAN_POINT('Ctrl Pts',(16.0297574123535,15.0736407351407,4.76456383569484));
#132214=CARTESIAN_POINT('Ctrl Pts',(16.0279136768122,15.0519402937685,4.76277502968693));
#132215=CARTESIAN_POINT('Ctrl Pts',(16.0271638811653,15.0431576224315,4.76220879891137));
#132216=CARTESIAN_POINT('Ctrl Pts',(16.0256262978969,15.0252481221696,4.76137501229877));
#132217=CARTESIAN_POINT('Ctrl Pts',(16.024838273481,15.0161222994786,4.76111949865441));
#132218=CARTESIAN_POINT('Ctrl Pts',(16.022799887066,14.9926675338573,4.76089749298013));
#132219=CARTESIAN_POINT('Ctrl Pts',(16.0215422321533,14.9783407858983,4.76117857548268));
#132220=CARTESIAN_POINT('Ctrl Pts',(16.0187160992876,14.9464939424655,4.7627304250224));
#132221=CARTESIAN_POINT('Ctrl Pts',(16.0171423687037,14.9289931362629,4.76420977877831));
#132222=CARTESIAN_POINT('Ctrl Pts',(16.0114400193112,14.8663993992292,4.77175466705736));
#132223=CARTESIAN_POINT('Ctrl Pts',(16.0072344764716,14.821837352697,4.78135695623573));
#132224=CARTESIAN_POINT('Ctrl Pts',(16.0009225239235,14.7560490643651,4.80203144599196));
#132225=CARTESIAN_POINT('Ctrl Pts',(15.9987900437993,14.7339976332204,4.81013396169094));
#132226=CARTESIAN_POINT('Ctrl Pts',(15.9960328669673,14.705435186727,4.82220268317415));
#132227=CARTESIAN_POINT('Ctrl Pts',(15.9953684601801,14.6985478953803,4.82523761627725));
#132228=CARTESIAN_POINT('Ctrl Pts',(15.9942767683819,14.6872102779137,4.83044187776041));
#132229=CARTESIAN_POINT('Ctrl Pts',(15.993846248157,14.682733403364,4.83255157290317));
#132230=CARTESIAN_POINT('Ctrl Pts',(15.9929285476355,14.6731743377037,4.83717413978791));
#132231=CARTESIAN_POINT('Ctrl Pts',(15.992442180808,14.6680992999583,4.83970077514199));
#132232=CARTESIAN_POINT('Ctrl Pts',(15.991019488024,14.6532437048725,4.84731128239167));
#132233=CARTESIAN_POINT('Ctrl Pts',(15.9900921046246,14.6435466937445,4.85255612606353));
#132234=CARTESIAN_POINT('Ctrl Pts',(15.9878880628603,14.6205635310667,4.86566008880557));
#132235=CARTESIAN_POINT('Ctrl Pts',(15.9866205851412,14.6073988567092,4.87372244904268));
#132236=CARTESIAN_POINT('Ctrl Pts',(15.9805803177298,14.5454225966811,4.91440118590786));
#132237=CARTESIAN_POINT('Ctrl Pts',(15.9759465432297,14.500363227696,4.95234149642313));
#132238=CARTESIAN_POINT('Ctrl Pts',(15.9696755283331,14.4483120568325,5.00799621496053));
#132239=CARTESIAN_POINT('Ctrl Pts',(15.9682213917082,14.4368160487304,5.02119831351721));
#132240=CARTESIAN_POINT('Ctrl Pts',(15.965923971035,14.4196306026858,5.04241020722167));
#132241=CARTESIAN_POINT('Ctrl Pts',(15.9650936615076,14.4136133593676,5.05014697471417));
#132242=CARTESIAN_POINT('Ctrl Pts',(15.9635196870945,14.4025821906683,5.06492796583384));
#132243=CARTESIAN_POINT('Ctrl Pts',(15.9627774851918,14.3975345266656,5.07194503447357));
#132244=CARTESIAN_POINT('Ctrl Pts',(15.9610585369559,14.3862043860028,5.08829324205044));
#132245=CARTESIAN_POINT('Ctrl Pts',(15.9600787316703,14.3800097453002,5.09768226004053));
#132246=CARTESIAN_POINT('Ctrl Pts',(15.9566108560075,14.3590194791475,5.1311331617797));
#132247=CARTESIAN_POINT('Ctrl Pts',(15.9540831653982,14.345392974958,5.1558953796543));
#132248=CARTESIAN_POINT('Ctrl Pts',(15.945984206961,14.306918924882,5.23640900976162));
#132249=CARTESIAN_POINT('Ctrl Pts',(15.9402934057937,14.287535892335,5.29448554910314));
#132250=CARTESIAN_POINT('Ctrl Pts',(15.933952087427,14.2735792845062,5.36387612304762));
#132251=CARTESIAN_POINT('Ctrl Pts',(15.9330823703939,14.271840270461,5.37350809422712));
#132252=CARTESIAN_POINT('Ctrl Pts',(15.9317444608854,14.2694344745218,5.38853474024009));
#132253=CARTESIAN_POINT('Ctrl Pts',(15.9312699092587,14.2686350526367,5.39390659417686));
#132254=CARTESIAN_POINT('Ctrl Pts',(15.9303538317602,14.2671962967282,5.40436523333159));
#132255=CARTESIAN_POINT('Ctrl Pts',(15.9299120316084,14.2665505446367,5.40945069976812));
#132256=CARTESIAN_POINT('Ctrl Pts',(15.9287655007803,14.2650026661564,5.42274631658249));
#132257=CARTESIAN_POINT('Ctrl Pts',(15.9280651414896,14.2641851237619,5.43096596306673));
#132258=CARTESIAN_POINT('Ctrl Pts',(15.9265017110519,14.262655414056,5.44949537110412));
#132259=CARTESIAN_POINT('Ctrl Pts',(15.9256420786784,14.2620213108645,5.45980998031163));
#132260=CARTESIAN_POINT('Ctrl Pts',(15.921511900116,14.2599991945482,5.50980596743498));
#132261=CARTESIAN_POINT('Ctrl Pts',(15.9183376690916,14.2615941501501,5.54954520300804));
#132262=CARTESIAN_POINT('Ctrl Pts',(15.9120257110401,14.2710262189477,5.62732246567828));
#132263=CARTESIAN_POINT('Ctrl Pts',(15.9088985736854,14.2786777125098,5.66524936995509));
#132264=CARTESIAN_POINT('Ctrl Pts',(15.9049235216853,14.2917510482803,5.71115705945049));
#132265=CARTESIAN_POINT('Ctrl Pts',(15.904160970047,14.2944059507075,5.71986565153891));
#132266=CARTESIAN_POINT('Ctrl Pts',(15.9027854288629,14.2994510306775,5.73538086262834));
#132267=CARTESIAN_POINT('Ctrl Pts',(15.9021752100555,14.3017780490148,5.74219642533103));
#132268=CARTESIAN_POINT('Ctrl Pts',(15.901560926295,14.3042076642396,5.74898599458032));
#132269=CARTESIAN_POINT('',(15.8432246779788,14.2612681978804,5.50006554428406));
#132270=CARTESIAN_POINT('Ctrl Pts',(15.822316354248,14.3042195800731,5.74901929091195));
#132271=CARTESIAN_POINT('Ctrl Pts',(15.8257720408061,14.2899780123663,5.70922717712378));
#132272=CARTESIAN_POINT('Ctrl Pts',(15.8291379930438,14.2791756081813,5.668284904552));
#132273=CARTESIAN_POINT('Ctrl Pts',(15.8348254834206,14.2671320011413,5.59904583292395));
#132274=CARTESIAN_POINT('Ctrl Pts',(15.8371105551477,14.2639051901807,5.57120207702545));
#132275=CARTESIAN_POINT('Ctrl Pts',(15.8401059855828,14.2617981889574,5.53525759524664));
#132276=CARTESIAN_POINT('Ctrl Pts',(15.8407749389911,14.2614597588463,5.52726379577456));
#132277=CARTESIAN_POINT('Ctrl Pts',(15.8419862648768,14.2610841869658,5.51286288273956));
#132278=CARTESIAN_POINT('Ctrl Pts',(15.8425272369543,14.2610004566375,5.50645771277246));
#132279=CARTESIAN_POINT('Ctrl Pts',(15.8430707068965,14.2610000018627,5.50005246929806));
#132280=CARTESIAN_POINT('Ctrl Pts',(15.8432343872441,14.261285110058,5.50006636877984));
#132281=CARTESIAN_POINT('Ctrl Pts',(15.8461654839889,14.2612946478705,5.46562025595231));
#132282=CARTESIAN_POINT('Ctrl Pts',(15.8491505168945,14.2636863127109,5.43121385975223));
#132283=CARTESIAN_POINT('Ctrl Pts',(15.852183835402,14.2684229126413,5.39717845675775));
#132284=CARTESIAN_POINT('Ctrl Pts',(15.8552208664968,14.2731653098663,5.3631013966129));
#132285=CARTESIAN_POINT('Ctrl Pts',(15.8583062235405,14.2802583961928,5.32939603907854));
#132286=CARTESIAN_POINT('Ctrl Pts',(15.8614058499154,14.2896334199308,5.29638824388491));
#132287=CARTESIAN_POINT('Ctrl Pts',(15.8645149786118,14.2990371840649,5.26327925885615));
#132288=CARTESIAN_POINT('Ctrl Pts',(15.8676381130064,14.3107373316171,5.23087191259096));
#132289=CARTESIAN_POINT('Ctrl Pts',(15.8707154043018,14.3246296874959,5.19949159250958));
#132290=CARTESIAN_POINT('Ctrl Pts',(15.8730027357389,14.3349557890202,5.17616679620788));
#132291=CARTESIAN_POINT('Ctrl Pts',(15.8752640840529,14.3464924798322,5.15340938928462));
#132292=CARTESIAN_POINT('Ctrl Pts',(15.8774685112417,14.3591812956108,5.13135232938189));
#132293=CARTESIAN_POINT('Ctrl Pts',(15.8774697703278,14.3591885429865,5.1313397312164));
#132294=CARTESIAN_POINT('Ctrl Pts',(15.8774710293971,14.3591957907502,5.13132713325581));
#132295=CARTESIAN_POINT('Ctrl Pts',(15.8774722884495,14.3592030389018,5.13131453550017));
#132296=CARTESIAN_POINT('Ctrl Pts',(15.88006104256,14.3741060580229,5.10541212580785));
#132297=CARTESIAN_POINT('Ctrl Pts',(15.8825785266667,14.3906531832454,5.08037439649702));
#132298=CARTESIAN_POINT('Ctrl Pts',(15.8850657038896,14.4087054696607,5.0564084055246));
#132299=CARTESIAN_POINT('Ctrl Pts',(15.8853223609872,14.4105683234191,5.05393530403883));
#132300=CARTESIAN_POINT('Ctrl Pts',(15.8855786953586,14.4124471622381,5.05147363121617));
#132301=CARTESIAN_POINT('Ctrl Pts',(15.8858347520161,14.4143418036469,5.04902362474293));
#132302=CARTESIAN_POINT('Ctrl Pts',(15.8885690334582,14.4345735870917,5.02286141791415));
#132303=CARTESIAN_POINT('Ctrl Pts',(15.8912724849652,14.4566124161231,4.99802716624137));
#132304=CARTESIAN_POINT('Ctrl Pts',(15.8939920816802,14.4802353179151,4.97475863671982));
#132305=CARTESIAN_POINT('Ctrl Pts',(15.8967088751499,14.5038338702174,4.95151409141598));
#132306=CARTESIAN_POINT('Ctrl Pts',(15.8994422611057,14.5290127331921,4.92983176695324));
#132307=CARTESIAN_POINT('Ctrl Pts',(15.9022214543911,14.5555261725094,4.90991198894262));
#132308=CARTESIAN_POINT('Ctrl Pts',(15.904999322998,14.582026974425,4.89000170552201));
#132309=CARTESIAN_POINT('Ctrl Pts',(15.9078231800637,14.6098608284518,4.87185209576196));
#132310=CARTESIAN_POINT('Ctrl Pts',(15.9106993990143,14.6387644217228,4.85563008019805));
#132311=CARTESIAN_POINT('Ctrl Pts',(15.9135779698292,14.6676916492615,4.83939480000458));
#132312=CARTESIAN_POINT('Ctrl Pts',(15.9165090298598,14.6976902939112,4.82509019853197));
#132313=CARTESIAN_POINT('Ctrl Pts',(15.9194741482956,14.7284808452098,4.81285240797014));
#132314=CARTESIAN_POINT('Ctrl Pts',(15.9224406859921,14.759286134475,4.80060875976236));
#132315=CARTESIAN_POINT('Ctrl Pts',(15.9254411518062,14.7908841955844,4.79043400749844));
#132316=CARTESIAN_POINT('Ctrl Pts',(15.9284331060532,14.8229793103559,4.78243308993879));
#132317=CARTESIAN_POINT('Ctrl Pts',(15.9314308623474,14.8551366645051,4.77441665686743));
#132318=CARTESIAN_POINT('Ctrl Pts',(15.9344196014866,14.887793253204,4.76858294864165));
#132319=CARTESIAN_POINT('Ctrl Pts',(15.9373371798038,14.9206329578154,4.76500202182394));
#132320=CARTESIAN_POINT('Ctrl Pts',(15.9383699050267,14.9322571157913,4.7637344934));
#132321=CARTESIAN_POINT('Ctrl Pts',(15.9393935743555,14.9439040274351,4.76274886121914));
#132322=CARTESIAN_POINT('Ctrl Pts',(15.9404050784039,14.9555590270972,4.76204694128078));
#132323=CARTESIAN_POINT('Ctrl Pts',(15.94040633749,14.9555735348478,4.76204606755451));
#132324=CARTESIAN_POINT('Ctrl Pts',(15.9404075965593,14.9555880426407,4.76204519426493));
#132325=CARTESIAN_POINT('Ctrl Pts',(15.9404088556117,14.9556025504756,4.76204432141208));
#132326=CARTESIAN_POINT('Ctrl Pts',(15.9429976097227,14.9854322993204,4.76024963727026));
#132327=CARTESIAN_POINT('Ctrl Pts',(15.94551509383,15.0154438358427,4.76030365815609));
#132328=CARTESIAN_POINT('Ctrl Pts',(15.9480022710536,15.0453878132334,4.76220418088315));
#132329=CARTESIAN_POINT('Ctrl Pts',(15.9482589281508,15.0484777958231,4.76240029985764));
#132330=CARTESIAN_POINT('Ctrl Pts',(15.9485152625218,15.0515670219798,4.76261605462374));
#132331=CARTESIAN_POINT('Ctrl Pts',(15.9487713191789,15.0546551928411,4.76285142346396));
#132332=CARTESIAN_POINT('Ctrl Pts',(15.9515056006213,15.0876319893532,4.76536479163489));
#132333=CARTESIAN_POINT('Ctrl Pts',(15.9542090521288,15.1204932118478,4.77011769576169));
#132334=CARTESIAN_POINT('Ctrl Pts',(15.9569286488443,15.152917660288,4.77705463303679));
#132335=CARTESIAN_POINT('Ctrl Pts',(15.9596454423144,15.185308686976,4.78398442000988));
#132336=CARTESIAN_POINT('Ctrl Pts',(15.9623788282709,15.2172637955092,4.7930931725959));
#132337=CARTESIAN_POINT('Ctrl Pts',(15.9651580215568,15.2484805436034,4.8042857888708));
#132338=CARTESIAN_POINT('Ctrl Pts',(15.9679358901642,15.2796824125045,4.81547307028191));
#132339=CARTESIAN_POINT('Ctrl Pts',(15.9707597472306,15.3101466471275,4.82874191248828));
#132340=CARTESIAN_POINT('Ctrl Pts',(15.9736359661817,15.3395890414552,4.8439641629593));
#132341=CARTESIAN_POINT('Ctrl Pts',(15.9765145369972,15.3690555106246,4.85919886055894));
#132342=CARTESIAN_POINT('Ctrl Pts',(15.9794455970283,15.3974984857032,4.87639006392071));
#132343=CARTESIAN_POINT('Ctrl Pts',(15.9824107154647,15.42465057061,4.89537916217598));
#132344=CARTESIAN_POINT('Ctrl Pts',(15.9853772531617,15.4518156519232,4.91437734960579));
#132345=CARTESIAN_POINT('Ctrl Pts',(15.9883777189763,15.4776885772525,4.93517530105871));
#132346=CARTESIAN_POINT('Ctrl Pts',(15.9913696732237,15.5020190932365,4.95758371613387));
#132347=CARTESIAN_POINT('Ctrl Pts',(15.9943674295183,15.5263967913596,4.98003558597831));
#132348=CARTESIAN_POINT('Ctrl Pts',(15.9973561686579,15.5492258537316,5.00410462934443));
#132349=CARTESIAN_POINT('Ctrl Pts',(16.0002737469752,15.5702739453929,5.02956532598645));
#132350=CARTESIAN_POINT('Ctrl Pts',(16.0013064721957,15.5777242664251,5.03857756171499));
#132351=CARTESIAN_POINT('Ctrl Pts',(16.0023301415221,15.5849516420565,5.04776380482493));
#132352=CARTESIAN_POINT('Ctrl Pts',(16.003341645568,15.5919464914698,5.05711280422425));
#132353=CARTESIAN_POINT('Ctrl Pts',(16.0033429046542,15.5919551984226,5.05712444154354));
#132354=CARTESIAN_POINT('Ctrl Pts',(16.0033441637235,15.5919639050338,5.05713607913817));
#132355=CARTESIAN_POINT('Ctrl Pts',(16.0033454227759,15.5919726113034,5.05714771700814));
#132356=CARTESIAN_POINT('Ctrl Pts',(16.0059341768868,15.6098736858217,5.08107649337375));
#132357=CARTESIAN_POINT('Ctrl Pts',(16.008451660994,15.6263305680899,5.10617363003627));
#132358=CARTESIAN_POINT('Ctrl Pts',(16.0109388382175,15.6412079936657,5.13222964617114));
#132359=CARTESIAN_POINT('Ctrl Pts',(16.0111954953145,15.6427432267902,5.1349184217834));
#132360=CARTESIAN_POINT('Ctrl Pts',(16.0114518296852,15.6442616429966,5.13761736242249));
#132361=CARTESIAN_POINT('Ctrl Pts',(16.0117078863421,15.6457630960937,5.14032620651912));
#132362=CARTESIAN_POINT('Ctrl Pts',(16.0144421677842,15.6617962482467,5.16925239118957));
#132363=CARTESIAN_POINT('Ctrl Pts',(16.0171456192913,15.6758952568307,5.19931346233171));
#132364=CARTESIAN_POINT('Ctrl Pts',(16.0198652160065,15.6879298675583,5.23021061591972));
#132365=CARTESIAN_POINT('Ctrl Pts',(16.0225820094763,15.6999520735174,5.26107592202646));
#132366=CARTESIAN_POINT('Ctrl Pts',(16.0253153954325,15.7099145849502,5.29277523906632));
#132367=CARTESIAN_POINT('Ctrl Pts',(16.0280945887181,15.7177305371739,5.32500365682599));
#132368=CARTESIAN_POINT('Ctrl Pts',(16.0308724573252,15.7255427639915,5.35721671318894));
#132369=CARTESIAN_POINT('Ctrl Pts',(16.0336963143912,15.7312107543982,5.3899582105465));
#132370=CARTESIAN_POINT('Ctrl Pts',(16.0365725333421,15.7346852768664,5.42292029765544));
#132371=CARTESIAN_POINT('Ctrl Pts',(16.0394511041573,15.7381626404275,5.45590933763434));
#132372=CARTESIAN_POINT('Ctrl Pts',(16.0423821641882,15.7394430394864,5.48911928919101));
#132373=CARTESIAN_POINT('Ctrl Pts',(16.0453472826244,15.7385119261771,5.52223959406798));
#132374=CARTESIAN_POINT('Ctrl Pts',(16.0483138203211,15.7375803671882,5.55537575205327));
#132375=CARTESIAN_POINT('Ctrl Pts',(16.0513142861355,15.7344350386086,5.58842223382762));
#132376=CARTESIAN_POINT('Ctrl Pts',(16.0543062403828,15.729096452324,5.62106592495639));
#132377=CARTESIAN_POINT('Ctrl Pts',(16.0573039966772,15.7237475133645,5.65377291927117));
#132378=CARTESIAN_POINT('Ctrl Pts',(16.0602927358166,15.7161962885673,5.68607561174723));
#132379=CARTESIAN_POINT('Ctrl Pts',(16.0632103141338,15.7065033953313,5.71765593879732));
#132380=CARTESIAN_POINT('Ctrl Pts',(16.0642430393564,15.70307243505,5.7288343191983));
#132381=CARTESIAN_POINT('Ctrl Pts',(16.0652667086848,15.6993735456597,5.7399221611344));
#132382=CARTESIAN_POINT('Ctrl Pts',(16.0662782127328,15.6954108566826,5.75090527566));
#132383=CARTESIAN_POINT('Ctrl Pts',(16.0662794718189,15.6954059240609,5.75091894707072));
#132384=CARTESIAN_POINT('Ctrl Pts',(16.0662807308882,15.6954009910215,5.75093261834753));
#132385=CARTESIAN_POINT('Ctrl Pts',(16.0662819899406,15.6953960575642,5.75094628949041));
#132386=CARTESIAN_POINT('Ctrl Pts',(16.0688707440513,15.6852523117074,5.77905570476472));
#132387=CARTESIAN_POINT('Ctrl Pts',(16.0713882281583,15.6733385845194,5.80660127331832));
#132388=CARTESIAN_POINT('Ctrl Pts',(16.0738754053815,15.6597554710563,5.83335483003574));
#132389=CARTESIAN_POINT('Ctrl Pts',(16.0741320624789,15.658353800744,5.83611558634535));
#132390=CARTESIAN_POINT('Ctrl Pts',(16.07438839685,15.6569343931202,5.838867885452));
#132391=CARTESIAN_POINT('Ctrl Pts',(16.0746444535072,15.6554973862791,5.84161146142266));
#132392=CARTESIAN_POINT('Ctrl Pts',(16.0773787349494,15.640152418565,5.87090852771709));
#132393=CARTESIAN_POINT('Ctrl Pts',(16.0800821864566,15.6227960265121,5.89921410483932));
#132394=CARTESIAN_POINT('Ctrl Pts',(16.0828017831719,15.6036061681248,5.92625509761583));
#132395=CARTESIAN_POINT('Ctrl Pts',(16.0855185766417,15.5844360898333,5.95326821767887));
#132396=CARTESIAN_POINT('Ctrl Pts',(16.0882519625979,15.5634368616103,5.97901954286687));
#132397=CARTESIAN_POINT('Ctrl Pts',(16.0910311558835,15.54081539972,6.00326886208316));
#132398=CARTESIAN_POINT('Ctrl Pts',(16.0938090244907,15.5182047201539,6.02750662307106));
#132399=CARTESIAN_POINT('Ctrl Pts',(16.0966328815568,15.4939736351654,6.05024395547408));
#132400=CARTESIAN_POINT('Ctrl Pts',(16.0995091005077,15.4683522103346,6.07127046451998));
#132401=CARTESIAN_POINT('Ctrl Pts',(16.1023876713229,15.4427098350425,6.09231416679644));
#132402=CARTESIAN_POINT('Ctrl Pts',(16.1053187313538,15.4156749284953,6.11164430213428));
#132403=CARTESIAN_POINT('Ctrl Pts',(16.1082838497899,15.38749888833,6.12907795716688));
#132404=CARTESIAN_POINT('Ctrl Pts',(16.1112503874867,15.3593093616398,6.14651995685763));
#132405=CARTESIAN_POINT('Ctrl Pts',(16.1142508533011,15.3299774848519,6.16206357463772));
#132406=CARTESIAN_POINT('Ctrl Pts',(16.1172428075483,15.2997760684677,6.17555377561747));
#132407=CARTESIAN_POINT('Ctrl Pts',(16.1202405638427,15.2695160849972,6.18907013701815));
#132408=CARTESIAN_POINT('Ctrl Pts',(16.1232293029821,15.2383828600024,6.2005247098438));
#132409=CARTESIAN_POINT('Ctrl Pts',(16.1261468812994,15.206675390044,6.2097932364135));
#132410=CARTESIAN_POINT('Ctrl Pts',(16.1271796065214,15.1954520053085,6.21307398507493));
#132411=CARTESIAN_POINT('Ctrl Pts',(16.1282032758492,15.1841569214697,6.21608116023705));
#132412=CARTESIAN_POINT('Ctrl Pts',(16.1292147798966,15.1728042606247,6.21881040925667));
#132413=CARTESIAN_POINT('Ctrl Pts',(16.1292160389828,15.1727901292151,6.21881380653385));
#132414=CARTESIAN_POINT('Ctrl Pts',(16.1292172980521,15.1727759976877,6.21881720338843));
#132415=CARTESIAN_POINT('Ctrl Pts',(16.1292185571045,15.1727618660425,6.21882059982039));
#132416=CARTESIAN_POINT('Ctrl Pts',(16.1318073112161,15.1437056057739,6.22580404788869));
#132417=CARTESIAN_POINT('Ctrl Pts',(16.1343247953239,15.1141470703662,6.2309990673935));
#132418=CARTESIAN_POINT('Ctrl Pts',(16.136811972548,15.0843321497203,6.23436422354309));
#132419=CARTESIAN_POINT('Ctrl Pts',(16.1370686296446,15.0812554847797,6.23471148114836));
#132420=CARTESIAN_POINT('Ctrl Pts',(16.1373249640148,15.0781761308462,6.23503927325043));
#132421=CARTESIAN_POINT('Ctrl Pts',(16.1375810206711,15.0750943859746,6.23534756896916));
#132422=CARTESIAN_POINT('Ctrl Pts',(16.1403153021134,15.0421862088087,6.23863968124789));
#132423=CARTESIAN_POINT('Ctrl Pts',(16.1430187536206,15.0090001903672,6.23970655581451));
#132424=CARTESIAN_POINT('Ctrl Pts',(16.1457383503359,14.9758622872572,6.2385466710135));
#132425=CARTESIAN_POINT('Ctrl Pts',(16.1484551438058,14.9427585412983,6.23738798177278));
#132426=CARTESIAN_POINT('Ctrl Pts',(16.1511885297621,14.9097029541351,6.23400767228793));
#132427=CARTESIAN_POINT('Ctrl Pts',(16.1539677230478,14.8770099384777,6.22844649006174));
#132428=CARTESIAN_POINT('Ctrl Pts',(16.156745591655,14.8443325056635,6.22288795852497));
#132429=CARTESIAN_POINT('Ctrl Pts',(16.1595694487211,14.8120173320975,6.2151509486412));
#132430=CARTESIAN_POINT('Ctrl Pts',(16.1624456676721,14.7803666548847,6.20531193827383));
#132431=CARTESIAN_POINT('Ctrl Pts',(16.1653242384874,14.7486900971328,6.19546488261594));
#132432=CARTESIAN_POINT('Ctrl Pts',(16.1682552985183,14.7176791223776,6.18351248750219));
#132433=CARTESIAN_POINT('Ctrl Pts',(16.1712204169545,14.6876247431539,6.16956415940564));
#132434=CARTESIAN_POINT('Ctrl Pts',(16.1741869546514,14.657555978334,6.1556091549105));
#132435=CARTESIAN_POINT('Ctrl Pts',(16.1771874204658,14.6284447284925,6.13965615574805));
#132436=CARTESIAN_POINT('Ctrl Pts',(16.1801793747131,14.6005704943679,6.12184778282757));
#132437=CARTESIAN_POINT('Ctrl Pts',(16.1831771310075,14.5726422060673,6.10400487561566));
#132438=CARTESIAN_POINT('Ctrl Pts',(16.1861658701469,14.5459558905665,6.08429889930881));
#132439=CARTESIAN_POINT('Ctrl Pts',(16.1890834484642,14.5207797401804,6.06291126999443));
#132440=CARTESIAN_POINT('Ctrl Pts',(16.190116173686,14.5118682243058,6.05534076397057));
#132441=CARTESIAN_POINT('Ctrl Pts',(16.1911398430137,14.5031457892696,6.04755994471023));
#132442=CARTESIAN_POINT('Ctrl Pts',(16.1921513470609,14.4946238357708,6.03957821451086));
#132443=CARTESIAN_POINT('Ctrl Pts',(16.1921526061468,14.4946132279322,6.03956827912393));
#132444=CARTESIAN_POINT('Ctrl Pts',(16.192153865216,14.4946026203798,6.0395583434045));
#132445=CARTESIAN_POINT('Ctrl Pts',(16.1921551242685,14.4945920131137,6.03954840735257));
#132446=CARTESIAN_POINT('Ctrl Pts',(16.1947166929634,14.4730113081658,6.01933330168643));
#132447=CARTESIAN_POINT('Ctrl Pts',(16.1972091345585,14.452614857626,5.99773757154862));
#132448=CARTESIAN_POINT('Ctrl Pts',(16.1996718468606,14.43357266356,5.9749388885128));
#132449=CARTESIAN_POINT('Ctrl Pts',(16.1999144880521,14.4316965123535,5.97269262547517));
#132450=CARTESIAN_POINT('Ctrl Pts',(16.2001568406503,14.4298335115516,5.97043472646499));
#132451=CARTESIAN_POINT('Ctrl Pts',(16.2003989423363,14.4279838256286,5.96816538861521));
#132452=CARTESIAN_POINT('Ctrl Pts',(16.2030952611575,14.4073836263946,5.94289146980893));
#132453=CARTESIAN_POINT('Ctrl Pts',(16.2057612561779,14.3884341056361,5.91619331180146));
#132454=CARTESIAN_POINT('Ctrl Pts',(16.2084419210787,14.3713139137559,5.88833392594945));
#132455=CARTESIAN_POINT('Ctrl Pts',(16.2111203234904,14.354208171369,5.86049805350281));
#132456=CARTESIAN_POINT('Ctrl Pts',(16.2138138376184,14.3389283469309,5.83150336784397));
#132457=CARTESIAN_POINT('Ctrl Pts',(16.2165508775019,14.3256113643662,5.80162775802377));
#132458=CARTESIAN_POINT('Ctrl Pts',(16.2181370964783,14.317893665191,5.78431370297036));
#132459=CARTESIAN_POINT('Ctrl Pts',(16.219737581817,14.3108344778435,5.76670402266428));
#132460=CARTESIAN_POINT('Ctrl Pts',(16.2213546080976,14.30445467332,5.74885446889987));
#132461=CARTESIAN_POINT('Origin',(13.2437274406976,15.,5.5));
#132462=CARTESIAN_POINT('',(16.700862083818,14.3042076661182,5.74898599983006));
#132463=CARTESIAN_POINT('',(16.6220124733702,14.3041067945379,5.74904127694233));
#132464=CARTESIAN_POINT('',(13.2437274406976,14.3042076641721,5.74898599439144));
#132465=CARTESIAN_POINT('Ctrl Pts',(16.700862083818,14.3042076680644,5.74898600526868));
#132466=CARTESIAN_POINT('Ctrl Pts',(16.697396127047,14.3169106070095,5.78448441611916));
#132467=CARTESIAN_POINT('Ctrl Pts',(16.6939254027009,14.3323145057219,5.81896699613406));
#132468=CARTESIAN_POINT('Ctrl Pts',(16.6897732313851,14.3544659205637,5.85983832197784));
#132469=CARTESIAN_POINT('Ctrl Pts',(16.688996145643,14.3587806335753,5.86747191840067));
#132470=CARTESIAN_POINT('Ctrl Pts',(16.6877680762403,14.3658822725913,5.87952998952657));
#132471=CARTESIAN_POINT('Ctrl Pts',(16.6873122307183,14.3685818987329,5.88400454741232));
#132472=CARTESIAN_POINT('Ctrl Pts',(16.6864000885435,14.3741159482379,5.89296089698515));
#132473=CARTESIAN_POINT('Ctrl Pts',(16.6859438966717,14.3769515865792,5.89744155900922));
#132474=CARTESIAN_POINT('Ctrl Pts',(16.6847086223169,14.3848090117365,5.90956646588726));
#132475=CARTESIAN_POINT('Ctrl Pts',(16.6839352496254,14.389925076977,5.91714895901912));
#132476=CARTESIAN_POINT('Ctrl Pts',(16.6805305820722,14.4132676031344,5.95039634309607));
#132477=CARTESIAN_POINT('Ctrl Pts',(16.6779756732664,14.4329841427522,5.97497927212336));
#132478=CARTESIAN_POINT('Ctrl Pts',(16.6709924275226,14.491334276544,6.0388989526216));
#132479=CARTESIAN_POINT('Ctrl Pts',(16.6666044889277,14.532881654663,6.07528474817825));
#132480=CARTESIAN_POINT('Ctrl Pts',(16.6609552702171,14.5886114384769,6.11403984977518));
#132481=CARTESIAN_POINT('Ctrl Pts',(16.6598792605772,14.5993290448737,6.1210863314509));
#132482=CARTESIAN_POINT('Ctrl Pts',(16.6580498333824,14.6176798711039,6.13247872328531));
#132483=CARTESIAN_POINT('Ctrl Pts',(16.657301961652,14.6252173257953,6.13697405708416));
#132484=CARTESIAN_POINT('Ctrl Pts',(16.6557630176664,14.6407869965908,6.14588778183389));
#132485=CARTESIAN_POINT('Ctrl Pts',(16.6549716400314,14.6488249119773,6.1502930489956));
#132486=CARTESIAN_POINT('Ctrl Pts',(16.6529121896104,14.6698091237733,6.16129117495463));
#132487=CARTESIAN_POINT('Ctrl Pts',(16.6516365194986,14.6828709577164,6.16765345707789));
#132488=CARTESIAN_POINT('Ctrl Pts',(16.6487607324478,14.7124306441505,6.18098855034726));
#132489=CARTESIAN_POINT('Ctrl Pts',(16.6471550449522,14.7290112016229,6.18775468449328));
#132490=CARTESIAN_POINT('Ctrl Pts',(16.6412055574989,14.7907332606746,6.21036351310312));
#132491=CARTESIAN_POINT('Ctrl Pts',(16.6367767559302,14.8371363246202,6.22241516764773));
#132492=CARTESIAN_POINT('Ctrl Pts',(16.6304810244729,14.9052189388955,6.2332005389251));
#132493=CARTESIAN_POINT('Ctrl Pts',(16.6285694675975,14.9261996763351,6.23560871969796));
#132494=CARTESIAN_POINT('Ctrl Pts',(16.626055319452,14.9544398303568,6.23762939867577));
#132495=CARTESIAN_POINT('Ctrl Pts',(16.6254202808825,14.961630338924,6.23803837322562));
#132496=CARTESIAN_POINT('Ctrl Pts',(16.6243576536445,14.9737733086633,6.23855106742231));
#132497=CARTESIAN_POINT('Ctrl Pts',(16.6239273106088,14.9787227017123,6.23871022856819));
#132498=CARTESIAN_POINT('Ctrl Pts',(16.6229947321607,14.9895208619953,6.23894884305295));
#132499=CARTESIAN_POINT('Ctrl Pts',(16.6224935252894,14.9953695683326,6.23900864080523));
#132500=CARTESIAN_POINT('Ctrl Pts',(16.6209730864128,15.013231077231,6.23897918571332));
#132501=CARTESIAN_POINT('Ctrl Pts',(16.6199647447072,15.0252422497625,6.23866648522819));
#132502=CARTESIAN_POINT('Ctrl Pts',(16.6181927584174,15.0465439788686,6.23759163177315));
#132503=CARTESIAN_POINT('Ctrl Pts',(16.6174252207451,15.0558372439007,6.23694638609425));
#132504=CARTESIAN_POINT('Ctrl Pts',(16.6135991214926,15.1023627928273,6.23283082534517));
#132505=CARTESIAN_POINT('Ctrl Pts',(16.6106116320748,15.1393077540344,6.2267137368902));
#132506=CARTESIAN_POINT('Ctrl Pts',(16.6046124570518,15.2115688710089,6.20903336982803));
#132507=CARTESIAN_POINT('Ctrl Pts',(16.6016095028439,15.2467892629939,6.1975558763184));
#132508=CARTESIAN_POINT('Ctrl Pts',(16.5975229952409,15.2920899763909,6.17893168891085));
#132509=CARTESIAN_POINT('Ctrl Pts',(16.5965147704517,15.303067313797,6.1741030799319));
#132510=CARTESIAN_POINT('Ctrl Pts',(16.5947567091956,15.3218290512853,6.16529944744243));
#132511=CARTESIAN_POINT('Ctrl Pts',(16.5940111956343,15.3296696118895,6.16144933747986));
#132512=CARTESIAN_POINT('Ctrl Pts',(16.5924490395351,15.3458467900563,6.15314645713499));
#132513=CARTESIAN_POINT('Ctrl Pts',(16.5916317210831,15.3541698543324,6.14867094340432));
#132514=CARTESIAN_POINT('Ctrl Pts',(16.5894093478587,15.3764080282279,6.13615736343223));
#132515=CARTESIAN_POINT('Ctrl Pts',(16.5879941970488,15.3901496615505,6.12782350210994));
#132516=CARTESIAN_POINT('Ctrl Pts',(16.5847236518551,15.4209303547678,6.10775510370916));
#132517=CARTESIAN_POINT('Ctrl Pts',(16.5828598036385,15.4377696776775,6.09574003307194));
#132518=CARTESIAN_POINT('Ctrl Pts',(16.5764441604068,15.4934134864181,6.05240335973789));
#132519=CARTESIAN_POINT('Ctrl Pts',(16.5718167743148,15.529542652497,6.01787128497162));
#132520=CARTESIAN_POINT('Ctrl Pts',(16.5659423369917,15.5716277765433,5.9686001628841));
#132521=CARTESIAN_POINT('Ctrl Pts',(16.5645991596043,15.5809897409556,5.95694138781113));
#132522=CARTESIAN_POINT('Ctrl Pts',(16.5627011205613,15.5938991736403,5.93982594648477));
#132523=CARTESIAN_POINT('Ctrl Pts',(16.5621304802254,15.5977377943766,5.93459478845771));
#132524=CARTESIAN_POINT('Ctrl Pts',(16.5611368577866,15.6043525755692,5.92532687817746));
#132525=CARTESIAN_POINT('Ctrl Pts',(16.560712074633,15.6071582351041,5.92131208336096));
#132526=CARTESIAN_POINT('Ctrl Pts',(16.5597509218269,15.6134555281901,5.91210730662903));
#132527=CARTESIAN_POINT('Ctrl Pts',(16.5592161696538,15.6169215213975,5.90690043275396));
#132528=CARTESIAN_POINT('Ctrl Pts',(16.5574544292141,15.628199438263,5.88948245097071));
#132529=CARTESIAN_POINT('Ctrl Pts',(16.5562439569937,15.6357187740616,5.87708465255163));
#132530=CARTESIAN_POINT('Ctrl Pts',(16.5531138415788,15.6544122566918,5.8441124417685));
#132531=CARTESIAN_POINT('Ctrl Pts',(16.551217036634,15.6649825220733,5.82321385037684));
#132532=CARTESIAN_POINT('Ctrl Pts',(16.5449197963812,15.6968646566975,5.75196624729619));
#132533=CARTESIAN_POINT('Ctrl Pts',(16.5405636196362,15.7135816886529,5.6997691359747));
#132534=CARTESIAN_POINT('Ctrl Pts',(16.5349452604301,15.7269404095369,5.63358346970776));
#132535=CARTESIAN_POINT('Ctrl Pts',(16.5338647721879,15.7291580570579,5.62089412508123));
#132536=CARTESIAN_POINT('Ctrl Pts',(16.5320300864344,15.7323285768023,5.59946371602465));
#132537=CARTESIAN_POINT('Ctrl Pts',(16.5312815117741,15.7334591455888,5.5907515445291));
#132538=CARTESIAN_POINT('Ctrl Pts',(16.5297430990076,15.7354498665781,5.57292633795143));
#132539=CARTESIAN_POINT('Ctrl Pts',(16.5289529810346,15.7362965390031,5.56381337809065));
#132540=CARTESIAN_POINT('Ctrl Pts',(16.526901438242,15.7380432181176,5.54027496343849));
#132541=CARTESIAN_POINT('Ctrl Pts',(16.5256325308499,15.7386896072786,5.52583534290751));
#132542=CARTESIAN_POINT('Ctrl Pts',(16.5227754168504,15.7391861397318,5.49361525066842));
#132543=CARTESIAN_POINT('Ctrl Pts',(16.5211817603835,15.738818750493,5.47584084334564));
#132544=CARTESIAN_POINT('Ctrl Pts',(16.5153274600387,15.7351503425984,5.41124689602264));
#132545=CARTESIAN_POINT('Ctrl Pts',(16.5109849894262,15.7280329359563,5.36475745325885));
#132546=CARTESIAN_POINT('Ctrl Pts',(16.5046705211652,15.7111389927466,5.29777930728284));
#132547=CARTESIAN_POINT('Ctrl Pts',(16.5026617415075,15.7047563474995,5.27654846837885));
#132548=CARTESIAN_POINT('Ctrl Pts',(16.5000485123283,15.6950277626955,5.24878272790917));
#132549=CARTESIAN_POINT('Ctrl Pts',(16.4994081496334,15.6925260842247,5.24196638968495));
#132550=CARTESIAN_POINT('Ctrl Pts',(16.4983395300471,15.6881470916671,5.23055765927861));
#132551=CARTESIAN_POINT('Ctrl Pts',(16.4979084411969,15.6863233397076,5.22594548918882));
#132552=CARTESIAN_POINT('Ctrl Pts',(16.4969777369728,15.6822596192105,5.2159636404118));
#132553=CARTESIAN_POINT('Ctrl Pts',(16.4964791027891,15.6800024631341,5.21060148807503));
#132554=CARTESIAN_POINT('Ctrl Pts',(16.4949759442973,15.6729612828783,5.19441168204379));
#132555=CARTESIAN_POINT('Ctrl Pts',(16.4939819524131,15.6679799518022,5.18367115264801));
#132556=CARTESIAN_POINT('Ctrl Pts',(16.4915748546421,15.6551676489959,5.15769971834669));
#132557=CARTESIAN_POINT('Ctrl Pts',(16.490173371231,15.647061095932,5.14261203177783));
#132558=CARTESIAN_POINT('Ctrl Pts',(16.4858317139062,15.6201453132324,5.09644091755839));
#132559=CARTESIAN_POINT('Ctrl Pts',(16.482932120987,15.59956492672,5.06645396042234));
#132560=CARTESIAN_POINT('Ctrl Pts',(16.479600182799,15.5738216035869,5.03430327486165));
#132561=CARTESIAN_POINT('Ctrl Pts',(16.479206018556,15.5707431444231,5.03053548097517));
#132562=CARTESIAN_POINT('Ctrl Pts',(16.4766041782743,15.5502167787151,5.00591313281881));
#132563=CARTESIAN_POINT('Ctrl Pts',(16.474375420893,15.5316683697906,4.98600700717737));
#132564=CARTESIAN_POINT('Ctrl Pts',(16.4711614918809,15.5039506608614,4.95936939270322));
#132565=CARTESIAN_POINT('Ctrl Pts',(16.4702134048853,15.4956574270842,4.95175606788137));
#132566=CARTESIAN_POINT('Ctrl Pts',(16.4685215121982,15.4806781161585,4.93862254815849));
#132567=CARTESIAN_POINT('Ctrl Pts',(16.4677810460902,15.4740625612184,4.93302489546963));
#132568=CARTESIAN_POINT('Ctrl Pts',(16.4662026513189,15.4598457832204,4.92141836183003));
#132569=CARTESIAN_POINT('Ctrl Pts',(16.4653636903635,15.4522218190262,4.91544011151077));
#132570=CARTESIAN_POINT('Ctrl Pts',(16.4630027609883,15.4305951544256,4.89915808710946));
#132571=CARTESIAN_POINT('Ctrl Pts',(16.4614683549362,15.4163441192289,4.88919671160989));
#132572=CARTESIAN_POINT('Ctrl Pts',(16.4588081736029,15.3913298926544,4.87299422773725));
#132573=CARTESIAN_POINT('Ctrl Pts',(16.4576911601493,15.3807353319335,4.86650501463834));
#132574=CARTESIAN_POINT('Ctrl Pts',(16.4523334905467,15.3294785882724,4.83686032626347));
#132575=CARTESIAN_POINT('Ctrl Pts',(16.448004017321,15.2868427769925,4.81733540362058));
#132576=CARTESIAN_POINT('Ctrl Pts',(16.4416874909688,15.2215838565512,4.79464963332036));
#132577=CARTESIAN_POINT('Ctrl Pts',(16.4396647726037,15.2001915974189,4.78828229344947));
#132578=CARTESIAN_POINT('Ctrl Pts',(16.4370369193232,15.1714841896348,4.78113487363869));
#132579=CARTESIAN_POINT('Ctrl Pts',(16.4363953816452,15.1644006132314,4.77948188899048));
#132580=CARTESIAN_POINT('Ctrl Pts',(16.4353254359835,15.1524459984151,4.7768777215563));
#132581=CARTESIAN_POINT('Ctrl Pts',(16.4348941789191,15.1475878987098,4.77587057029255));
#132582=CARTESIAN_POINT('Ctrl Pts',(16.433963870749,15.1370183212739,4.7737901520935));
#132583=CARTESIAN_POINT('Ctrl Pts',(16.4334657905818,15.1313037382141,4.77273519343357));
#132584=CARTESIAN_POINT('Ctrl Pts',(16.4319663339226,15.1139494771497,4.76974269173346));
#132585=CARTESIAN_POINT('Ctrl Pts',(16.4309754139526,15.1022746024243,4.7680162759527));
#132586=CARTESIAN_POINT('Ctrl Pts',(16.4285778563981,15.0736499010753,4.76448175641307));
#132587=CARTESIAN_POINT('Ctrl Pts',(16.4271827196844,15.0566688658583,4.76297888505902));
#132588=CARTESIAN_POINT('Ctrl Pts',(16.4228864016805,15.003866178877,4.76014175807839));
#132589=CARTESIAN_POINT('Ctrl Pts',(16.4200248331092,14.9679894091775,4.76082436630523));
#132590=CARTESIAN_POINT('Ctrl Pts',(16.416338688891,14.9225986707608,4.76499999611553));
#132591=CARTESIAN_POINT('Ctrl Pts',(16.4155484592389,14.9129131602611,4.7660845791198));
#132592=CARTESIAN_POINT('Ctrl Pts',(16.4127980377695,14.8794349905929,4.77050549853386));
#132593=CARTESIAN_POINT('Ctrl Pts',(16.4108213625446,14.8557878135062,4.77480982872409));
#132594=CARTESIAN_POINT('Ctrl Pts',(16.4078915331915,14.8217068295919,4.78274623831879));
#132595=CARTESIAN_POINT('Ctrl Pts',(16.4069660897088,14.8110768529963,4.78547258161488));
#132596=CARTESIAN_POINT('Ctrl Pts',(16.4053002469293,14.792212183767,4.79076130537416));
#132597=CARTESIAN_POINT('Ctrl Pts',(16.4045628499817,14.7839540346447,4.79323311490274));
#132598=CARTESIAN_POINT('Ctrl Pts',(16.4029620675492,14.7662382783447,4.79887524195338));
#132599=CARTESIAN_POINT('Ctrl Pts',(16.4020972545112,14.7567979574469,4.80209369250876));
#132600=CARTESIAN_POINT('Ctrl Pts',(16.3995645114551,14.7295466866203,4.81200438870312));
#132601=CARTESIAN_POINT('Ctrl Pts',(16.3978809421187,14.7119268698687,4.81919409007022));
#132602=CARTESIAN_POINT('Ctrl Pts',(16.3937876159225,14.6703002890944,4.83808496325697));
#132603=CARTESIAN_POINT('Ctrl Pts',(16.3913611777954,14.6466128856851,4.85042268709786));
#132604=CARTESIAN_POINT('Ctrl Pts',(16.3847133964604,14.5841709859134,4.88737345685745));
#132605=CARTESIAN_POINT('Ctrl Pts',(16.3804642203436,14.5469542834794,4.91435928191798));
#132606=CARTESIAN_POINT('Ctrl Pts',(16.3753883718121,14.5044745958915,4.95164883622007));
#132607=CARTESIAN_POINT('Ctrl Pts',(16.3744399295171,14.4966229480837,4.95884752259677));
#132608=CARTESIAN_POINT('Ctrl Pts',(16.3730094108972,14.4848851923959,4.97008578154907));
#132609=CARTESIAN_POINT('Ctrl Pts',(16.3725195867291,14.4808852239365,4.97400361262789));
#132610=CARTESIAN_POINT('Ctrl Pts',(16.3715958623317,14.4733734307764,4.98153032409678));
#132611=CARTESIAN_POINT('Ctrl Pts',(16.3711614344424,14.4698535181646,4.98513005670938));
#132612=CARTESIAN_POINT('Ctrl Pts',(16.3700648563114,14.4610079819816,4.99436308511563));
#132613=CARTESIAN_POINT('Ctrl Pts',(16.3694063748255,14.4557336417689,5.00004477037013));
#132614=CARTESIAN_POINT('Ctrl Pts',(16.3660162860778,14.4288302185592,5.02995647632269));
#132615=CARTESIAN_POINT('Ctrl Pts',(16.3633741567363,14.4087232839458,5.05551344210995));
#132616=CARTESIAN_POINT('Ctrl Pts',(16.3561068289732,14.3578586366054,5.12975363443086));
#132617=CARTESIAN_POINT('Ctrl Pts',(16.3515324557921,14.3310078152352,5.18081896613052));
#132618=CARTESIAN_POINT('Ctrl Pts',(16.3457023003394,14.3058621021702,5.24613093422921));
#132619=CARTESIAN_POINT('Ctrl Pts',(16.3446537826047,14.3016719122226,5.25789512980407));
#132620=CARTESIAN_POINT('Ctrl Pts',(16.3428564887666,14.2950646186758,5.27804689881088));
#132621=CARTESIAN_POINT('Ctrl Pts',(16.3421127916269,14.2924943198568,5.28638171969691));
#132622=CARTESIAN_POINT('Ctrl Pts',(16.340569722473,14.2875010275874,5.30365355611688));
#132623=CARTESIAN_POINT('Ctrl Pts',(16.339769880511,14.2850973039703,5.3125944774282));
#132624=CARTESIAN_POINT('Ctrl Pts',(16.3376573781823,14.2792337748496,5.3361619311406));
#132625=CARTESIAN_POINT('Ctrl Pts',(16.3363363354901,14.276051302438,5.35085216691753));
#132626=CARTESIAN_POINT('Ctrl Pts',(16.3341102538847,14.2714926668311,5.37550518710915));
#132627=CARTESIAN_POINT('Ctrl Pts',(16.3332127604705,14.2698679289812,5.38541800972001));
#132628=CARTESIAN_POINT('Ctrl Pts',(16.329471934667,14.263973833022,5.42662469209067));
#132629=CARTESIAN_POINT('Ctrl Pts',(16.3265850864333,14.2615111181704,5.45814030991767));
#132630=CARTESIAN_POINT('Ctrl Pts',(16.3199160195203,14.2605008124614,5.53071569711654));
#132631=CARTESIAN_POINT('Ctrl Pts',(16.3161331652276,14.2633436787261,5.57169786656442));
#132632=CARTESIAN_POINT('Ctrl Pts',(16.3116824894046,14.270910620945,5.62094333208096));
#132633=CARTESIAN_POINT('Ctrl Pts',(16.3109015453472,14.2724043019312,5.62962690176481));
#132634=CARTESIAN_POINT('Ctrl Pts',(16.3096688947638,14.2750324092338,5.64342380203196));
#132635=CARTESIAN_POINT('Ctrl Pts',(16.3092122670681,14.2760664444781,5.64855506591789));
#132636=CARTESIAN_POINT('Ctrl Pts',(16.308300127549,14.278255609077,5.65885228363348));
#132637=CARTESIAN_POINT('Ctrl Pts',(16.3078447020281,14.2794118903938,5.66401766855364));
#132638=CARTESIAN_POINT('Ctrl Pts',(16.3066140564873,14.2827066742947,5.67802833003765));
#132639=CARTESIAN_POINT('Ctrl Pts',(16.305844474352,14.2849532951371,5.68684762410514));
#132640=CARTESIAN_POINT('Ctrl Pts',(16.3035172559882,14.2923025791173,5.71362032009262));
#132641=CARTESIAN_POINT('Ctrl Pts',(16.3019823719936,14.2979219165104,5.73142044878301));
#132642=CARTESIAN_POINT('Ctrl Pts',(16.3004622294836,14.3042076679214,5.74898600486896));
#132643=CARTESIAN_POINT('',(16.2439139857417,14.2608925795155,5.49943231825045));
#132644=CARTESIAN_POINT('Ctrl Pts',(16.2211956582352,14.3041893991231,5.74893494673765));
#132645=CARTESIAN_POINT('Ctrl Pts',(16.2216107958238,14.3025459439714,5.74434124251259));
#132646=CARTESIAN_POINT('Ctrl Pts',(16.2220273713241,14.3009480621918,5.73973149340631));
#132647=CARTESIAN_POINT('Ctrl Pts',(16.2228901658018,14.2977448441053,5.73018608030003));
#132648=CARTESIAN_POINT('Ctrl Pts',(16.2233365551274,14.2961456329688,5.72524866831267));
#132649=CARTESIAN_POINT('Ctrl Pts',(16.2246645325414,14.291560634912,5.71056715181112));
#132650=CARTESIAN_POINT('Ctrl Pts',(16.2255508068294,14.2887243917547,5.70077810113298));
#132651=CARTESIAN_POINT('Ctrl Pts',(16.2283906682725,14.2803487823945,5.6694614364029));
#132652=CARTESIAN_POINT('Ctrl Pts',(16.2303672975008,14.2755783160696,5.64774322464492));
#132653=CARTESIAN_POINT('Ctrl Pts',(16.2361851377203,14.2645785358762,5.58409284640734));
#132654=CARTESIAN_POINT('Ctrl Pts',(16.2400864757065,14.2609679963021,5.54180086186545));
#132655=CARTESIAN_POINT('Ctrl Pts',(16.2439755819599,14.2610002137098,5.49943798301597));
#132656=CARTESIAN_POINT('Ctrl Pts',(16.2439139857417,14.2608925795155,5.49943231825045));
#132657=CARTESIAN_POINT('Ctrl Pts',(16.2468365782592,14.2608415859776,5.46711637395115));
#132658=CARTESIAN_POINT('Ctrl Pts',(16.2497445498771,14.2629206022102,5.43486649125833));
#132659=CARTESIAN_POINT('Ctrl Pts',(16.2525823523489,14.2671249071872,5.40291827216697));
#132660=CARTESIAN_POINT('Ctrl Pts',(16.2534241981765,14.2683721316287,5.39344070098001));
#132661=CARTESIAN_POINT('Ctrl Pts',(16.2542598688615,14.2698064864784,5.38398934254864));
#132662=CARTESIAN_POINT('Ctrl Pts',(16.2550879142251,14.2714281697843,5.37456952060223));
#132663=CARTESIAN_POINT('Ctrl Pts',(16.2550891733112,14.2714306356384,5.37455519727192));
#132664=CARTESIAN_POINT('Ctrl Pts',(16.2550904323805,14.2714331019271,5.37454087400039));
#132665=CARTESIAN_POINT('Ctrl Pts',(16.2550916914329,14.2714355686507,5.37452655078767));
#132666=CARTESIAN_POINT('Ctrl Pts',(16.2576804455433,14.2765074311787,5.34507640618042));
#132667=CARTESIAN_POINT('Ctrl Pts',(16.26019792965,14.2834206029643,5.3158718979988));
#132668=CARTESIAN_POINT('Ctrl Pts',(16.262685106873,14.2921159389437,5.28715526692191));
#132669=CARTESIAN_POINT('Ctrl Pts',(16.2629417639707,14.2930132291228,5.28419193679843));
#132670=CARTESIAN_POINT('Ctrl Pts',(16.2631980983421,14.2939294622358,5.28123383178361));
#132671=CARTESIAN_POINT('Ctrl Pts',(16.2634541549996,14.2948645488209,5.27828123786169));
#132672=CARTESIAN_POINT('Ctrl Pts',(16.2661884364418,14.3048497994343,5.24675218938546));
#132673=CARTESIAN_POINT('Ctrl Pts',(16.268891887949,14.3169888650432,5.21584760837416));
#132674=CARTESIAN_POINT('Ctrl Pts',(16.2716114846644,14.3311542867762,5.18586750192992));
#132675=CARTESIAN_POINT('Ctrl Pts',(16.2743282781342,14.3453051073906,5.15591829771342));
#132676=CARTESIAN_POINT('Ctrl Pts',(16.2770616640904,14.3614775464346,5.12689157639859));
#132677=CARTESIAN_POINT('Ctrl Pts',(16.2798408573761,14.3795098824573,5.09906003173981));
#132678=CARTESIAN_POINT('Ctrl Pts',(16.2826187259834,14.397533623523,5.07124175274624));
#132679=CARTESIAN_POINT('Ctrl Pts',(16.2854425830495,14.4174151856514,5.04461741703861));
#132680=CARTESIAN_POINT('Ctrl Pts',(16.2883188020004,14.4389648407132,5.01943440967743));
#132681=CARTESIAN_POINT('Ctrl Pts',(16.2911973728157,14.4605321167784,4.9942308103458));
#132682=CARTESIAN_POINT('Ctrl Pts',(16.2941284328466,14.4837701232007,4.97047085744732));
#132683=CARTESIAN_POINT('Ctrl Pts',(16.2970935512828,14.5084633227428,4.94837860849926));
#132684=CARTESIAN_POINT('Ctrl Pts',(16.3000600889796,14.5331683417405,4.92627578504663));
#132685=CARTESIAN_POINT('Ctrl Pts',(16.3030605547941,14.5593300841324,4.90584232511856));
#132686=CARTESIAN_POINT('Ctrl Pts',(16.3060525090414,14.5867070545747,4.88727858186716));
#132687=CARTESIAN_POINT('Ctrl Pts',(16.3090502653358,14.6141371148912,4.86867883949768));
#132688=CARTESIAN_POINT('Ctrl Pts',(16.3120390044752,14.6427875121405,4.85195640921161));
#132689=CARTESIAN_POINT('Ctrl Pts',(16.3149565827925,14.6723855863172,4.83728592043362));
#132690=CARTESIAN_POINT('Ctrl Pts',(16.3159893080143,14.6828623154375,4.8320930576794));
#132691=CARTESIAN_POINT('Ctrl Pts',(16.317012977342,14.6934574794728,4.82715701469034));
#132692=CARTESIAN_POINT('Ctrl Pts',(16.3180244813892,14.7041579350933,4.82248454661349));
#132693=CARTESIAN_POINT('Ctrl Pts',(16.3180257404753,14.7041712546597,4.82247873048274));
#132694=CARTESIAN_POINT('Ctrl Pts',(16.3180269995446,14.7041845744162,4.82247291474745));
#132695=CARTESIAN_POINT('Ctrl Pts',(16.318028258597,14.7041978943625,4.82246709940767));
#132696=CARTESIAN_POINT('Ctrl Pts',(16.3206170127076,14.7315852099172,4.81051010339048));
#132697=CARTESIAN_POINT('Ctrl Pts',(16.3231344968146,14.7597798089517,4.8002261436611));
#132698=CARTESIAN_POINT('Ctrl Pts',(16.3256216740378,14.788546836311,4.79169901605146));
#132699=CARTESIAN_POINT('Ctrl Pts',(16.3258783311352,14.7915153669307,4.79081908365207));
#132700=CARTESIAN_POINT('Ctrl Pts',(16.3261346655063,14.7944899491001,4.78995784657965));
#132701=CARTESIAN_POINT('Ctrl Pts',(16.3263907221636,14.797470294757,4.78911538736027));
#132702=CARTESIAN_POINT('Ctrl Pts',(16.3291250036058,14.8292956880439,4.78011925098165));
#132703=CARTESIAN_POINT('Ctrl Pts',(16.331828455113,14.8617837753845,4.77326547667347));
#132704=CARTESIAN_POINT('Ctrl Pts',(16.3345480518283,14.8946138889352,4.76861256365983));
#132705=CARTESIAN_POINT('Ctrl Pts',(16.3372648452982,14.9274101625911,4.76396444667244));
#132706=CARTESIAN_POINT('Ctrl Pts',(16.3399982312544,14.9605475209686,4.76151213864556));
#132707=CARTESIAN_POINT('Ctrl Pts',(16.3427774245401,14.9937092705058,4.76127050225467));
#132708=CARTESIAN_POINT('Ctrl Pts',(16.3455552931473,15.0268552137816,4.76102898103767));
#132709=CARTESIAN_POINT('Ctrl Pts',(16.3483791502134,15.0600254369483,4.76299571935205));
#132710=CARTESIAN_POINT('Ctrl Pts',(16.3512553691644,15.0929089861587,4.76714827089704));
#132711=CARTESIAN_POINT('Ctrl Pts',(16.3541339399797,15.1258194240193,4.77130421795463));
#132712=CARTESIAN_POINT('Ctrl Pts',(16.3570650000106,15.1584427019205,4.77764945578953));
#132713=CARTESIAN_POINT('Ctrl Pts',(16.3600301184468,15.1904731593011,4.7861271540139));
#132714=CARTESIAN_POINT('Ctrl Pts',(16.3629966561436,15.222518948132,4.79460891010755));
#132715=CARTESIAN_POINT('Ctrl Pts',(16.365997121958,15.2539713716961,4.80522531729318));
#132716=CARTESIAN_POINT('Ctrl Pts',(16.3689890762053,15.2845302955342,4.8178848294456));
#132717=CARTESIAN_POINT('Ctrl Pts',(16.3719868324997,15.3151484797431,4.83056889113345));
#132718=CARTESIAN_POINT('Ctrl Pts',(16.3749755716391,15.3448696292337,4.84530450140765));
#132719=CARTESIAN_POINT('Ctrl Pts',(16.3778931499564,15.3733979594889,4.86195993922172));
#132720=CARTESIAN_POINT('Ctrl Pts',(16.3789258751784,15.383496035013,4.86785540760101));
#132721=CARTESIAN_POINT('Ctrl Pts',(16.3799495445063,15.3934447213567,4.87399101363608));
#132722=CARTESIAN_POINT('Ctrl Pts',(16.3809610485537,15.4032311492864,4.88035949358426));
#132723=CARTESIAN_POINT('Ctrl Pts',(16.3809623076398,15.403243331102,4.88036742085342));
#132724=CARTESIAN_POINT('Ctrl Pts',(16.3809635667091,15.4032555126918,4.88037534849871));
#132725=CARTESIAN_POINT('Ctrl Pts',(16.3809648257615,15.4032676940556,4.88038327652013));
#132726=CARTESIAN_POINT('Ctrl Pts',(16.3835535798724,15.4283139551783,4.89668418480728));
#132727=CARTESIAN_POINT('Ctrl Pts',(16.3860710639795,15.4524066853143,4.91457931255719));
#132728=CARTESIAN_POINT('Ctrl Pts',(16.3885582412028,15.4753467568033,4.93391857026285));
#132729=CARTESIAN_POINT('Ctrl Pts',(16.3888148983,15.4777139914744,4.93591422931627));
#132730=CARTESIAN_POINT('Ctrl Pts',(16.3890712326708,15.4800689381655,4.9379252227119));
#132731=CARTESIAN_POINT('Ctrl Pts',(16.3893272893277,15.4824113695533,4.93995135522031));
#132732=CARTESIAN_POINT('Ctrl Pts',(16.3920615707698,15.5074248441075,4.96158725636354));
#132733=CARTESIAN_POINT('Ctrl Pts',(16.3947650222769,15.5310132754005,4.9849546685096));
#132734=CARTESIAN_POINT('Ctrl Pts',(16.397484618992,15.5529514804485,5.00981791677843));
#132735=CARTESIAN_POINT('Ctrl Pts',(16.4002014124618,15.5748670725211,5.03465553706087));
#132736=CARTESIAN_POINT('Ctrl Pts',(16.4029347984178,15.5951361406784,5.06098542902574));
#132737=CARTESIAN_POINT('Ctrl Pts',(16.4057139917034,15.613572135076,5.08855124356168));
#132738=CARTESIAN_POINT('Ctrl Pts',(16.4084918603105,15.6319993421162,5.11610391909035));
#132739=CARTESIAN_POINT('Ctrl Pts',(16.4113157173763,15.6485954289492,5.1448910979431));
#132740=CARTESIAN_POINT('Ctrl Pts',(16.4141919363272,15.6632081644352,5.17464071062246));
#132741=CARTESIAN_POINT('Ctrl Pts',(16.4170705071423,15.6778328486537,5.20441464935378));
#132742=CARTESIAN_POINT('Ctrl Pts',(16.4200015671731,15.6904710096386,5.23515252812032));
#132743=CARTESIAN_POINT('Ctrl Pts',(16.4229666856092,15.7010020464407,5.26656779241988));
#132744=CARTESIAN_POINT('Ctrl Pts',(16.4259332233059,15.7115381239473,5.29799809370624));
#132745=CARTESIAN_POINT('Ctrl Pts',(16.4289336891202,15.7199649479335,5.33010653009044));
#132746=CARTESIAN_POINT('Ctrl Pts',(16.4319256433674,15.7261939526705,5.36259207416802));
#132747=CARTESIAN_POINT('Ctrl Pts',(16.4349233996618,15.7324350367965,5.39514061475019));
#132748=CARTESIAN_POINT('Ctrl Pts',(16.4379121388011,15.7364693053219,5.42806795315767));
#132749=CARTESIAN_POINT('Ctrl Pts',(16.4408297171184,15.7382441408574,5.46105460492308));
#132750=CARTESIAN_POINT('Ctrl Pts',(16.441862442341,15.7388723733242,5.47273077727572));
#132751=CARTESIAN_POINT('Ctrl Pts',(16.4428861116694,15.7392178859971,5.48441421180992));
#132752=CARTESIAN_POINT('Ctrl Pts',(16.4438976157173,15.7392796697724,5.49609016536313));
#132753=CARTESIAN_POINT('Ctrl Pts',(16.4438988748035,15.7392797466787,5.49610469919649));
#132754=CARTESIAN_POINT('Ctrl Pts',(16.4439001338727,15.7392798231467,5.49611923304801));
#132755=CARTESIAN_POINT('Ctrl Pts',(16.4439013929252,15.7392798991764,5.49613376691765));
#132756=CARTESIAN_POINT('Ctrl Pts',(16.4464901470361,15.7394362246864,5.52601704601413));
#132757=CARTESIAN_POINT('Ctrl Pts',(16.4490076311434,15.7377366584986,5.55598046900575));
#132758=CARTESIAN_POINT('Ctrl Pts',(16.4514948083669,15.7341970729513,5.5857751850253));
#132759=CARTESIAN_POINT('Ctrl Pts',(16.4517514654643,15.733831815605,5.58884976501857));
#132760=CARTESIAN_POINT('Ctrl Pts',(16.4520077998353,15.7334469934861,5.59192251302494));
#132761=CARTESIAN_POINT('Ctrl Pts',(16.4522638564925,15.7330426446669,5.59499313182244));
#132762=CARTESIAN_POINT('Ctrl Pts',(16.454998137935,15.7287248367074,5.62778249994964));
#132763=CARTESIAN_POINT('Ctrl Pts',(16.4577015894424,15.7221771993878,5.66033366716369));
#132764=CARTESIAN_POINT('Ctrl Pts',(16.460421186158,15.7134727644175,5.69232896005582));
#132765=CARTESIAN_POINT('Ctrl Pts',(16.463137979628,15.7047773016111,5.7242912735511));
#132766=CARTESIAN_POINT('Ctrl Pts',(16.4658713655845,15.693930054134,5.7556988452053));
#132767=CARTESIAN_POINT('Ctrl Pts',(16.4686505588704,15.6810425646902,5.78625490248517));
#132768=CARTESIAN_POINT('Ctrl Pts',(16.4714284274778,15.6681612179569,5.81679639548447));
#132769=CARTESIAN_POINT('Ctrl Pts',(16.4742522845441,15.6532418888684,5.84648722545286));
#132770=CARTESIAN_POINT('Ctrl Pts',(16.4771285034953,15.6364281210601,5.87505064095674));
#132771=CARTESIAN_POINT('Ctrl Pts',(16.4800070743107,15.6196006047506,5.9036374125673));
#132772=CARTESIAN_POINT('Ctrl Pts',(16.4829381343418,15.6008756475668,5.93109494856035));
#132773=CARTESIAN_POINT('Ctrl Pts',(16.4859032527782,15.5804262839172,5.95716495227471));
#132774=CARTESIAN_POINT('Ctrl Pts',(16.4888697904752,15.5599671321338,5.98324743445488));
#132775=CARTESIAN_POINT('Ctrl Pts',(16.4918702562898,15.5377817769755,6.00794101795833));
#132776=CARTESIAN_POINT('Ctrl Pts',(16.4948622105372,15.5140729562227,6.03100620585586));
#132777=CARTESIAN_POINT('Ctrl Pts',(16.4978599668317,15.4903181589325,6.05411612214736));
#132778=CARTESIAN_POINT('Ctrl Pts',(16.5008487059713,15.4650335376564,6.07559105786966));
#132779=CARTESIAN_POINT('Ctrl Pts',(16.5037662842887,15.4384570130061,6.09521139358542));
#132780=CARTESIAN_POINT('Ctrl Pts',(16.5047990095091,15.429049811453,6.10215633672778));
#132781=CARTESIAN_POINT('Ctrl Pts',(16.5058226788356,15.4194810891018,6.10886912851364));
#132782=CARTESIAN_POINT('Ctrl Pts',(16.5068341828815,15.4097626054639,6.1153408194724));
#132783=CARTESIAN_POINT('Ctrl Pts',(16.5068354419677,15.4097505082231,6.11534887521515));
#132784=CARTESIAN_POINT('Ctrl Pts',(16.506836701037,15.4097384107261,6.11535693060174));
#132785=CARTESIAN_POINT('Ctrl Pts',(16.5068379600894,15.4097263129728,6.11536498563214));
#132786=CARTESIAN_POINT('Ctrl Pts',(16.5094267142004,15.3848519646828,6.13192703878028));
#132787=CARTESIAN_POINT('Ctrl Pts',(16.5119441983077,15.3588902034422,6.14698300756358));
#132788=CARTESIAN_POINT('Ctrl Pts',(16.5144313755313,15.3320576118916,6.16040931753061));
#132789=CARTESIAN_POINT('Ctrl Pts',(16.5146880326282,15.3292886998153,6.16179480695444));
#132790=CARTESIAN_POINT('Ctrl Pts',(16.5149443669988,15.3265105601295,6.16316294738053));
#132791=CARTESIAN_POINT('Ctrl Pts',(16.5152004236556,15.323723462026,6.16451360718012));
#132792=CARTESIAN_POINT('Ctrl Pts',(16.5179347050977,15.2939616479088,6.17893652463707));
#132793=CARTESIAN_POINT('Ctrl Pts',(16.5206381566049,15.2631727098718,6.1913659790012));
#132794=CARTESIAN_POINT('Ctrl Pts',(16.5233577533202,15.2316621446506,6.20168829630943));
#132795=CARTESIAN_POINT('Ctrl Pts',(16.52607454679,15.2001840591894,6.21199997380887));
#132796=CARTESIAN_POINT('Ctrl Pts',(16.5288079327462,15.1679861570418,6.22020932409411));
#132797=CARTESIAN_POINT('Ctrl Pts',(16.5315871260319,15.1353776527562,6.22624633234962));
#132798=CARTESIAN_POINT('Ctrl Pts',(16.5343649946392,15.1027846910322,6.23228046311734));
#132799=CARTESIAN_POINT('Ctrl Pts',(16.5371888517053,15.0697816585366,6.23614460733382));
#132800=CARTESIAN_POINT('Ctrl Pts',(16.5400650706562,15.0366786428791,6.2378064879869));
#132801=CARTESIAN_POINT('Ctrl Pts',(16.5429436414715,15.0035485591153,6.23946972754826));
#132802=CARTESIAN_POINT('Ctrl Pts',(16.5458747015025,14.9703183625751,6.23892719459613));
#132803=CARTESIAN_POINT('Ctrl Pts',(16.5488398199387,14.9372989419958,6.23618139203368));
#132804=CARTESIAN_POINT('Ctrl Pts',(16.5518063576355,14.9042637165967,6.23343427518667));
#132805=CARTESIAN_POINT('Ctrl Pts',(16.5548068234498,14.871439420416,6.22848163652201));
#132806=CARTESIAN_POINT('Ctrl Pts',(16.557798777697,14.8391375720869,6.22136112611124));
#132807=CARTESIAN_POINT('Ctrl Pts',(16.5607965339914,14.8067730834789,6.21422680748886));
#132808=CARTESIAN_POINT('Ctrl Pts',(16.5637852731306,14.7749330466829,6.20491568543388));
#132809=CARTESIAN_POINT('Ctrl Pts',(16.5667028514477,14.7439317229275,6.19350572657112));
#132810=CARTESIAN_POINT('Ctrl Pts',(16.5677355766706,14.7329582903388,6.1894669824385));
#132811=CARTESIAN_POINT('Ctrl Pts',(16.5687592459994,14.7220899513954,6.18516567679505));
#132812=CARTESIAN_POINT('Ctrl Pts',(16.5697707500476,14.7113406472614,6.1806067109747));
#132813=CARTESIAN_POINT('Ctrl Pts',(16.5697720091338,14.7113272668899,6.18060103612772));
#132814=CARTESIAN_POINT('Ctrl Pts',(16.5697732682031,14.7113138866751,6.18059536087092));
#132815=CARTESIAN_POINT('Ctrl Pts',(16.5697745272555,14.7113005066169,6.18058968520427));
#132816=CARTESIAN_POINT('Ctrl Pts',(16.5723632911273,14.6837894906899,6.16891982897771));
#132817=CARTESIAN_POINT('Ctrl Pts',(16.5748807844833,14.6569385324742,6.15551355888183));
#132818=CARTESIAN_POINT('Ctrl Pts',(16.5773679708376,14.6309699385419,6.14048383039845));
#132819=CARTESIAN_POINT('Ctrl Pts',(16.5776248130349,14.6282882614275,6.13893176797203));
#132820=CARTESIAN_POINT('Ctrl Pts',(16.5778813320413,14.6256160149713,6.13736243376493));
#132821=CARTESIAN_POINT('Ctrl Pts',(16.5781375729667,14.6229534576917,6.13577598057665));
#132822=CARTESIAN_POINT('Ctrl Pts',(16.5808718844585,14.5945416770366,6.11884715791783));
#132823=CARTESIAN_POINT('Ctrl Pts',(16.5835753690728,14.5672302344032,6.09996426653787));
#132824=CARTESIAN_POINT('Ctrl Pts',(16.586295002674,14.5412820633584,6.0793199811601));
#132825=CARTESIAN_POINT('Ctrl Pts',(16.5891089842951,14.5144337127617,6.05795951568898));
#132826=CARTESIAN_POINT('Ctrl Pts',(16.5919409097406,14.4890448400346,6.03471373893295));
#132827=CARTESIAN_POINT('Ctrl Pts',(16.5948228149276,14.4653687253073,6.00982733631907));
#132828=CARTESIAN_POINT('Ctrl Pts',(16.5976046135951,14.4425150295311,5.98580539349394));
#132829=CARTESIAN_POINT('Ctrl Pts',(16.6004330743049,14.4212568161143,5.96025523821325));
#132830=CARTESIAN_POINT('Ctrl Pts',(16.6033137008858,14.401790641754,5.93341904099662));
#132831=CARTESIAN_POINT('Ctrl Pts',(16.6061942600457,14.3823249229993,5.90658347188088));
#132832=CARTESIAN_POINT('Ctrl Pts',(16.6091270143045,14.3646510995958,5.87846199693993));
#132833=CARTESIAN_POINT('Ctrl Pts',(16.612092674658,14.3489367067677,5.84931589224036));
#132834=CARTESIAN_POINT('Ctrl Pts',(16.6150613409843,14.3332063859398,5.82014024525074));
#132835=CARTESIAN_POINT('Ctrl Pts',(16.6180628108254,14.3194395724126,5.78993776234784));
#132836=CARTESIAN_POINT('Ctrl Pts',(16.6210538554812,14.3077750183842,5.75899004845362));
#132837=CARTESIAN_POINT('Ctrl Pts',(16.6213735567761,14.3065282389286,5.75568216597613));
#132838=CARTESIAN_POINT('Ctrl Pts',(16.6216931184145,14.3053054482088,5.75236578931324));
#132839=CARTESIAN_POINT('Ctrl Pts',(16.6220124733702,14.3041067945379,5.74904127694233));
#132840=CARTESIAN_POINT('Origin',(13.2437274406976,15.,5.5));
#132841=CARTESIAN_POINT('',(17.1015120386236,14.3042076643465,5.74898599487892));
#132842=CARTESIAN_POINT('',(17.0220282051085,14.3041366315448,5.74902320646588));
#132843=CARTESIAN_POINT('',(13.2437274406976,14.3042076641721,5.74898599439144));
#132844=CARTESIAN_POINT('Ctrl Pts',(17.1015120386236,14.3042076645209,5.7489859953664));
#132845=CARTESIAN_POINT('Ctrl Pts',(17.1010629887414,14.306009822866,5.75402213389287));
#132846=CARTESIAN_POINT('Ctrl Pts',(17.1006122891737,14.3078666430159,5.7590386633245));
#132847=CARTESIAN_POINT('Ctrl Pts',(17.0993979148554,14.312996258662,5.77244816797651));
#132848=CARTESIAN_POINT('Ctrl Pts',(17.0986311940599,14.3163681184237,5.78080167409815));
#132849=CARTESIAN_POINT('Ctrl Pts',(17.0970874669747,14.3234155464965,5.79738127426927));
#132850=CARTESIAN_POINT('Ctrl Pts',(17.0963105928316,14.3270905347949,5.80560592432059));
#132851=CARTESIAN_POINT('Ctrl Pts',(17.0943428025253,14.3367138154367,5.82612726321211));
#132852=CARTESIAN_POINT('Ctrl Pts',(17.0931455852938,14.3428541473218,5.83832946778211));
#132853=CARTESIAN_POINT('Ctrl Pts',(17.0878380526966,14.3712930007245,5.89114566203298));
#132854=CARTESIAN_POINT('Ctrl Pts',(17.0836133526042,14.3970407641257,5.9297744573182));
#132855=CARTESIAN_POINT('Ctrl Pts',(17.0767942921161,14.4437964901717,5.98737637993273));
#132856=CARTESIAN_POINT('Ctrl Pts',(17.0742280057754,14.4625759471951,6.00800945654015));
#132857=CARTESIAN_POINT('Ctrl Pts',(17.0706800586025,14.4904828425965,6.03538681560242));
#132858=CARTESIAN_POINT('Ctrl Pts',(17.0696686565435,14.4986669011208,6.04305794538599));
#132859=CARTESIAN_POINT('Ctrl Pts',(17.067883286662,14.5135582107111,6.05639225507572));
#132860=CARTESIAN_POINT('Ctrl Pts',(17.0671057338256,14.5201976486511,6.06212781514659));
#132861=CARTESIAN_POINT('Ctrl Pts',(17.0658771095241,14.5309533831471,6.07108982414434));
#132862=CARTESIAN_POINT('Ctrl Pts',(17.0654211690367,14.5350042696298,6.07439297751985));
#132863=CARTESIAN_POINT('Ctrl Pts',(17.0645661448299,14.5427183944272,6.08054808511209));
#132864=CARTESIAN_POINT('Ctrl Pts',(17.064166421157,14.5463740626173,6.08340899767106));
#132865=CARTESIAN_POINT('Ctrl Pts',(17.0630517243684,14.5567003592184,6.09133456648626));
#132866=CARTESIAN_POINT('Ctrl Pts',(17.0623418065563,14.5634307619532,6.09632076947767));
#132867=CARTESIAN_POINT('Ctrl Pts',(17.0577403497939,14.6079677298945,6.12815751129518));
#132868=CARTESIAN_POINT('Ctrl Pts',(17.0540303975087,14.6481510188862,6.15151732457892));
#132869=CARTESIAN_POINT('Ctrl Pts',(17.0469629073583,14.7278513642259,6.18830946972849));
#132870=CARTESIAN_POINT('Ctrl Pts',(17.0436224891662,14.7668246479606,6.20246951165992));
#132871=CARTESIAN_POINT('Ctrl Pts',(17.0391043645555,14.8192384898768,6.21666799252661));
#132872=CARTESIAN_POINT('Ctrl Pts',(17.0380212531432,14.8317874139924,6.21971676368964));
#132873=CARTESIAN_POINT('Ctrl Pts',(17.0361760108917,14.8530885201933,6.22430438714678));
#132874=CARTESIAN_POINT('Ctrl Pts',(17.0354194559501,14.8618005907772,6.22601703619758));
#132875=CARTESIAN_POINT('Ctrl Pts',(17.0339650543251,14.8784936012233,6.22898727087771));
#132876=CARTESIAN_POINT('Ctrl Pts',(17.0332681652654,14.8864685026522,6.23027175342549));
#132877=CARTESIAN_POINT('Ctrl Pts',(17.0313991246292,14.9077827406307,6.23334718886206));
#132878=CARTESIAN_POINT('Ctrl Pts',(17.0302199909763,14.9211519719025,6.23490479594459));
#132879=CARTESIAN_POINT('Ctrl Pts',(17.0246506061707,14.9838846854003,6.24048221769656));
#132880=CARTESIAN_POINT('Ctrl Pts',(17.0201263347773,15.0335209023497,6.23989740917214));
#132881=CARTESIAN_POINT('Ctrl Pts',(17.0131866491669,15.108530822838,6.23144852099819));
#132882=CARTESIAN_POINT('Ctrl Pts',(17.0107980610273,15.1341760510584,6.22718141130333));
#132883=CARTESIAN_POINT('Ctrl Pts',(17.0070430561451,15.174615643203,6.21823994784909));
#132884=CARTESIAN_POINT('Ctrl Pts',(17.0056563068226,15.1895802475821,6.21443590866868));
#132885=CARTESIAN_POINT('Ctrl Pts',(17.0037252111576,15.2105584999238,6.20839746862312));
#132886=CARTESIAN_POINT('Ctrl Pts',(17.0031634824079,15.2166780735814,6.20654969879856));
#132887=CARTESIAN_POINT('Ctrl Pts',(17.0021793433855,15.227439621733,6.20314733182012));
#132888=CARTESIAN_POINT('Ctrl Pts',(17.0017552602062,15.232091188662,6.2016257095619));
#132889=CARTESIAN_POINT('Ctrl Pts',(17.0007876390334,15.2427358597911,6.19802616507192));
#132890=CARTESIAN_POINT('Ctrl Pts',(17.000245841114,15.2487178710238,6.19591713168326));
#132891=CARTESIAN_POINT('Ctrl Pts',(16.9985159888412,15.2678619419067,6.18888924453129));
#132892=CARTESIAN_POINT('Ctrl Pts',(16.997342980813,15.2809120440398,6.18367163761283));
#132893=CARTESIAN_POINT('Ctrl Pts',(16.9916447820021,15.3442202180977,6.15624090201944));
#132894=CARTESIAN_POINT('Ctrl Pts',(16.9873047325161,15.3920444802288,6.12884170678909));
#132895=CARTESIAN_POINT('Ctrl Pts',(16.981318040755,15.4515491397386,6.08530086199236));
#132896=CARTESIAN_POINT('Ctrl Pts',(16.9797825423878,15.4662765191978,6.07363738065959));
#132897=CARTESIAN_POINT('Ctrl Pts',(16.976984981612,15.4919588065323,6.05165508682364));
#132898=CARTESIAN_POINT('Ctrl Pts',(16.9757303191036,15.5030732358454,6.04153860379621));
#132899=CARTESIAN_POINT('Ctrl Pts',(16.973680316267,15.5205240239193,6.02465364322095));
#132900=CARTESIAN_POINT('Ctrl Pts',(16.9728937334068,15.5270552882818,6.01809208793202));
#132901=CARTESIAN_POINT('Ctrl Pts',(16.9713555527193,15.5394971974875,6.0051136983365));
#132902=CARTESIAN_POINT('Ctrl Pts',(16.9706046849001,15.5454208898163,5.99871145275268));
#132903=CARTESIAN_POINT('Ctrl Pts',(16.9687669541212,15.5595473143835,5.98289104202235));
#132904=CARTESIAN_POINT('Ctrl Pts',(16.9676753233456,15.567626966765,5.97336723648909));
#132905=CARTESIAN_POINT('Ctrl Pts',(16.961503387527,15.611539664855,5.91886411174524));
#132906=CARTESIAN_POINT('Ctrl Pts',(16.9562302586365,15.6422611978186,5.87003474592157));
#132907=CARTESIAN_POINT('Ctrl Pts',(16.9481829916127,15.6799640864898,5.79099051701522));
#132908=CARTESIAN_POINT('Ctrl Pts',(16.9454271662665,15.6912501490172,5.76305939908778));
#132909=CARTESIAN_POINT('Ctrl Pts',(16.9419335674514,15.7036541653223,5.72599244626899));
#132910=CARTESIAN_POINT('Ctrl Pts',(16.9411365006676,15.7063506742697,5.71741784093578));
#132911=CARTESIAN_POINT('Ctrl Pts',(16.9398846894468,15.7103792329684,5.70374032055653));
#132912=CARTESIAN_POINT('Ctrl Pts',(16.9394247738157,15.7118141618425,5.69866901433246));
#132913=CARTESIAN_POINT('Ctrl Pts',(16.93856834987,15.7144026134699,5.68913266812467));
#132914=CARTESIAN_POINT('Ctrl Pts',(16.9381711314264,15.7155688222134,5.68467139604451));
#132915=CARTESIAN_POINT('Ctrl Pts',(16.9370738941703,15.7186919723345,5.67224992483934));
#132916=CARTESIAN_POINT('Ctrl Pts',(16.9363786691551,15.7205584339007,5.66426730857187));
#132917=CARTESIAN_POINT('Ctrl Pts',(16.931657781287,15.73242601812,5.60940908720544));
#132918=CARTESIAN_POINT('Ctrl Pts',(16.9278284164877,15.7379804895321,5.56168074581195));
#132919=CARTESIAN_POINT('Ctrl Pts',(16.9217092438539,15.7393937807021,5.48570329407221));
#132920=CARTESIAN_POINT('Ctrl Pts',(16.9194463639833,15.7383186904235,5.45765739397033));
#132921=CARTESIAN_POINT('Ctrl Pts',(16.9155369902868,15.7337870368565,5.41020776228871));
#132922=CARTESIAN_POINT('Ctrl Pts',(16.9139113140119,15.731144315119,5.3907574938111));
#132923=CARTESIAN_POINT('Ctrl Pts',(16.9114158379383,15.7259786288951,5.36151713602058));
#132924=CARTESIAN_POINT('Ctrl Pts',(16.9105634616441,15.7240236218185,5.35163474920394));
#132925=CARTESIAN_POINT('Ctrl Pts',(16.9089706594558,15.7200240015546,5.33338493673109));
#132926=CARTESIAN_POINT('Ctrl Pts',(16.9082320696553,15.7180338863259,5.32500723829367));
#132927=CARTESIAN_POINT('Ctrl Pts',(16.9065535349365,15.7132102905085,5.3061715964801));
#132928=CARTESIAN_POINT('Ctrl Pts',(16.9056110541433,15.7102923453717,5.29573760669279));
#132929=CARTESIAN_POINT('Ctrl Pts',(16.9024902911401,15.6999545920789,5.26167724369267));
#132930=CARTESIAN_POINT('Ctrl Pts',(16.9002826684072,15.6915774701594,5.23836194032731));
#132931=CARTESIAN_POINT('Ctrl Pts',(16.8941641740181,15.6655130597364,5.17587332999429));
#132932=CARTESIAN_POINT('Ctrl Pts',(16.8902004338957,15.6455555552518,5.13775264625651));
#132933=CARTESIAN_POINT('Ctrl Pts',(16.8838122837411,15.6079988528801,5.07908161270821));
#132934=CARTESIAN_POINT('Ctrl Pts',(16.8813782184418,15.5923824361585,5.05737343289217));
#132935=CARTESIAN_POINT('Ctrl Pts',(16.8783242124831,15.5708506426264,5.03062973650073));
#132936=CARTESIAN_POINT('Ctrl Pts',(16.8776522086612,15.5659871648315,5.02477642728545));
#132937=CARTESIAN_POINT('Ctrl Pts',(16.8765517994293,15.5578043703098,5.01523211441731));
#132938=CARTESIAN_POINT('Ctrl Pts',(16.8761200477903,15.5545368592671,5.01149770005004));
#132939=CARTESIAN_POINT('Ctrl Pts',(16.8752040842733,15.5474796194494,5.00359411594678));
#132940=CARTESIAN_POINT('Ctrl Pts',(16.8747206298936,15.5436794176455,4.99943488666151));
#132941=CARTESIAN_POINT('Ctrl Pts',(16.8733166114837,15.5324329879911,4.98740514017314));
#132942=CARTESIAN_POINT('Ctrl Pts',(16.8724046388137,15.5248604090546,4.97965399453943));
#132943=CARTESIAN_POINT('Ctrl Pts',(16.870246488778,15.5063641917029,4.96153647205967));
#132944=CARTESIAN_POINT('Ctrl Pts',(16.8690089825265,15.4952886193859,4.95133168784819));
#132945=CARTESIAN_POINT('Ctrl Pts',(16.8633519836663,15.4428528917104,4.90590144068372));
#132946=CARTESIAN_POINT('Ctrl Pts',(16.8590557435465,15.3980011826466,4.87496631705344));
#132947=CARTESIAN_POINT('Ctrl Pts',(16.8528986192143,15.3317577763217,4.8393226121397));
#132948=CARTESIAN_POINT('Ctrl Pts',(16.8511703161143,15.3129423560662,4.83020543042086));
#132949=CARTESIAN_POINT('Ctrl Pts',(16.848552660313,15.2843353138525,4.81781227586705));
#132950=CARTESIAN_POINT('Ctrl Pts',(16.8476835965648,15.2748194829559,4.81392355263777));
#132951=CARTESIAN_POINT('Ctrl Pts',(16.846148564366,15.2580021904839,4.80745702613958));
#132952=CARTESIAN_POINT('Ctrl Pts',(16.8454855530226,15.2507353738999,4.80479307872245));
#132953=CARTESIAN_POINT('Ctrl Pts',(16.8439416446739,15.2338164194497,4.79889051058087));
#132954=CARTESIAN_POINT('Ctrl Pts',(16.843058147837,15.2241367733724,4.795736328985));
#132955=CARTESIAN_POINT('Ctrl Pts',(16.8403953716461,15.1949905876826,4.7869005464086));
#132956=CARTESIAN_POINT('Ctrl Pts',(16.8385977990153,15.1753538551609,4.78181964873577));
#132957=CARTESIAN_POINT('Ctrl Pts',(16.8341223707168,15.1266032869994,4.77132418064754));
#132958=CARTESIAN_POINT('Ctrl Pts',(16.8314228819217,15.0973265194249,4.76683968628251));
#132959=CARTESIAN_POINT('Ctrl Pts',(16.8246068168924,15.0233946123894,4.76002167337448));
#132960=CARTESIAN_POINT('Ctrl Pts',(16.8204783210415,14.9786428171387,4.75995961023736));
#132961=CARTESIAN_POINT('Ctrl Pts',(16.8157269978302,14.9256231363466,4.76470245771879));
#132962=CARTESIAN_POINT('Ctrl Pts',(16.8149681038898,14.9171035406863,4.76561414071456));
#132963=CARTESIAN_POINT('Ctrl Pts',(16.813761605079,14.9034554770302,4.76731518062048));
#132964=CARTESIAN_POINT('Ctrl Pts',(16.8133094160191,14.8983163777741,4.76801069900851));
#132965=CARTESIAN_POINT('Ctrl Pts',(16.8123970024063,14.8878919974392,4.7695334323692));
#132966=CARTESIAN_POINT('Ctrl Pts',(16.8119369730679,14.8826075634945,4.77036404136967));
#132967=CARTESIAN_POINT('Ctrl Pts',(16.8106784576917,14.8680853668081,4.77280851276459));
#132968=CARTESIAN_POINT('Ctrl Pts',(16.8098860480527,14.8588681707807,4.77454099930935));
#132969=CARTESIAN_POINT('Ctrl Pts',(16.8080714743497,14.8376527085884,4.77894840597014));
#132970=CARTESIAN_POINT('Ctrl Pts',(16.807054653506,14.8256830067229,4.78174818343004));
#132971=CARTESIAN_POINT('Ctrl Pts',(16.8033101110349,14.7815245768757,4.79324616393884));
#132972=CARTESIAN_POINT('Ctrl Pts',(16.8006374344958,14.7498644725895,4.80382112921949));
#132973=CARTESIAN_POINT('Ctrl Pts',(16.794830142338,14.6831619885609,4.83124132498402));
#132974=CARTESIAN_POINT('Ctrl Pts',(16.7916988447189,14.6485191436547,4.8487817891561));
#132975=CARTESIAN_POINT('Ctrl Pts',(16.7873489532573,14.6037902530223,4.8760415459075));
#132976=CARTESIAN_POINT('Ctrl Pts',(16.7862089460339,14.5923646076857,4.8834453345144));
#132977=CARTESIAN_POINT('Ctrl Pts',(16.7843722103877,14.5744753983555,4.89575215313949));
#132978=CARTESIAN_POINT('Ctrl Pts',(16.7836829649347,14.5678764309258,4.90045362391436));
#132979=CARTESIAN_POINT('Ctrl Pts',(16.7822317113484,14.5542294688992,4.91051882492109));
#132980=CARTESIAN_POINT('Ctrl Pts',(16.7814690203417,14.5471979840458,4.91590262656079));
#132981=CARTESIAN_POINT('Ctrl Pts',(16.779593885952,14.5302631960329,4.92935866077688));
#132982=CARTESIAN_POINT('Ctrl Pts',(16.7784763837562,14.5204696121644,4.93756354510834));
#132983=CARTESIAN_POINT('Ctrl Pts',(16.7735779817468,14.4788635628557,4.97429712734431));
#132984=CARTESIAN_POINT('Ctrl Pts',(16.7696992591317,14.4493517391013,5.00529611961691));
#132985=CARTESIAN_POINT('Ctrl Pts',(16.7616414124294,14.3945523610328,5.07387174876006));
#132986=CARTESIAN_POINT('Ctrl Pts',(16.7574739573392,14.3696951817944,5.11158186296606));
#132987=CARTESIAN_POINT('Ctrl Pts',(16.7526905897982,14.344406392462,5.15883924840147));
#132988=CARTESIAN_POINT('Ctrl Pts',(16.7519357170864,14.3405152226653,5.16642319531918));
#132989=CARTESIAN_POINT('Ctrl Pts',(16.750778616955,14.3346971724314,5.17826262774972));
#132990=CARTESIAN_POINT('Ctrl Pts',(16.750371365387,14.3326781132605,5.1824715881774));
#132991=CARTESIAN_POINT('Ctrl Pts',(16.7495161272941,14.328496886686,5.19140390675305));
#132992=CARTESIAN_POINT('Ctrl Pts',(16.7490687759639,14.3263443621103,5.19613149938571));
#132993=CARTESIAN_POINT('Ctrl Pts',(16.74788720829,14.3207565631175,5.20875526596189));
#132994=CARTESIAN_POINT('Ctrl Pts',(16.747157882137,14.3174089866019,5.21668979860382));
#132995=CARTESIAN_POINT('Ctrl Pts',(16.7433826877292,14.3006602953589,5.25840964077225));
#132996=CARTESIAN_POINT('Ctrl Pts',(16.7404445143384,14.2896245216491,5.29309574667645));
#132997=CARTESIAN_POINT('Ctrl Pts',(16.7334970652377,14.2696087221208,5.37696808254232));
#132998=CARTESIAN_POINT('Ctrl Pts',(16.7295073315853,14.2629733896052,5.42652006416303));
#132999=CARTESIAN_POINT('Ctrl Pts',(16.7242487805051,14.2609487094766,5.48977930657587));
#133000=CARTESIAN_POINT('Ctrl Pts',(16.7231239182279,14.2608850291573,5.50320730468455));
#133001=CARTESIAN_POINT('Ctrl Pts',(16.721304951729,14.2613687563276,5.52469920782863));
#133002=CARTESIAN_POINT('Ctrl Pts',(16.7206180532956,14.2616826171588,5.53276577919979));
#133003=CARTESIAN_POINT('Ctrl Pts',(16.7191666066163,14.2626192895688,5.54969509756409));
#133004=CARTESIAN_POINT('Ctrl Pts',(16.7184013146512,14.2632699133235,5.55855492479974));
#133005=CARTESIAN_POINT('Ctrl Pts',(16.716508785168,14.265260388448,5.58028816418176));
#133006=CARTESIAN_POINT('Ctrl Pts',(16.7153762601525,14.266778980117,5.59314169845822));
#133007=CARTESIAN_POINT('Ctrl Pts',(16.7102443827919,14.2751111994405,5.65065960781032));
#133008=CARTESIAN_POINT('Ctrl Pts',(16.7061345551986,14.2856735042036,5.69467485559293));
#133009=CARTESIAN_POINT('Ctrl Pts',(16.7016111543801,14.3014937675516,5.74130199537794));
#133010=CARTESIAN_POINT('Ctrl Pts',(16.7012366265413,14.3028349465736,5.74514992987891));
#133011=CARTESIAN_POINT('Ctrl Pts',(16.700862083818,14.3042076680644,5.74898600526868));
#133012=CARTESIAN_POINT('',(16.6438825647488,14.2609107381065,5.50061424492574));
#133013=CARTESIAN_POINT('Ctrl Pts',(16.6220124734468,14.3041067942504,5.74904127614493));
#133014=CARTESIAN_POINT('Ctrl Pts',(16.6250063842204,14.2928695735229,5.71787440921185));
#133015=CARTESIAN_POINT('Ctrl Pts',(16.6279833582934,14.283756768005,5.68599041700478));
#133016=CARTESIAN_POINT('Ctrl Pts',(16.6308791641049,14.2768707640213,5.65369834793092));
#133017=CARTESIAN_POINT('Ctrl Pts',(16.6314924590787,14.2754123956401,5.64685929692086));
#133018=CARTESIAN_POINT('Ctrl Pts',(16.6321020669945,14.2740537690431,5.64000203572447));
#133019=CARTESIAN_POINT('Ctrl Pts',(16.6327073172076,14.2727956189547,5.63312965534444));
#133020=CARTESIAN_POINT('Ctrl Pts',(16.632708576295,14.2727930016555,5.63311535889766));
#133021=CARTESIAN_POINT('Ctrl Pts',(16.6327098353647,14.2727903847881,5.63310106237043));
#133022=CARTESIAN_POINT('Ctrl Pts',(16.6327110944169,14.2727877683526,5.63308676576276));
#133023=CARTESIAN_POINT('Ctrl Pts',(16.6355088912899,14.2669736682273,5.60131762472554));
#133024=CARTESIAN_POINT('Ctrl Pts',(16.6382196158601,14.2632907979205,5.56914710280213));
#133025=CARTESIAN_POINT('Ctrl Pts',(16.6408988670525,14.2617459925759,5.53680734929748));
#133026=CARTESIAN_POINT('Ctrl Pts',(16.6418968418795,14.2611705792474,5.52476134928105));
#133027=CARTESIAN_POINT('Ctrl Pts',(16.6428904499833,14.2608919445406,5.51269237424421));
#133028=CARTESIAN_POINT('Ctrl Pts',(16.6438825646895,14.2609107381054,5.50061424564688));
#133029=CARTESIAN_POINT('Ctrl Pts',(16.643882564756,14.2609107381066,5.50061424483712));
#133030=CARTESIAN_POINT('Ctrl Pts',(16.6465594256901,14.2609614457461,5.46802580481307));
#133031=CARTESIAN_POINT('Ctrl Pts',(16.6492248243156,14.2631785677597,5.43537629957805));
#133032=CARTESIAN_POINT('Ctrl Pts',(16.6519184636661,14.2675388665903,5.40297839022479));
#133033=CARTESIAN_POINT('Ctrl Pts',(16.6546091468162,14.2718943801043,5.37061603674961));
#133034=CARTESIAN_POINT('Ctrl Pts',(16.6573283838935,14.2783879342007,5.33850485702922));
#133035=CARTESIAN_POINT('Ctrl Pts',(16.6600972580023,14.2869564952498,5.30694519284429));
#133036=CARTESIAN_POINT('Ctrl Pts',(16.6629358361132,14.2957407623855,5.27459104150862));
#133037=CARTESIAN_POINT('Ctrl Pts',(16.6658268589015,14.3067057226881,5.24281665383555));
#133038=CARTESIAN_POINT('Ctrl Pts',(16.6687685064462,14.3197454173502,5.21193175497587));
#133039=CARTESIAN_POINT('Ctrl Pts',(16.6716387263794,14.3324684886811,5.18179678775293));
#133040=CARTESIAN_POINT('Ctrl Pts',(16.6745570252431,14.3471665761053,5.15250863134965));
#133041=CARTESIAN_POINT('Ctrl Pts',(16.6774978093645,14.3637081100762,5.12434123441606));
#133042=CARTESIAN_POINT('Ctrl Pts',(16.6805483689687,14.3808671170754,5.0951223867577));
#133043=CARTESIAN_POINT('Ctrl Pts',(16.6836229974486,14.400010227424,5.06710973508013));
#133044=CARTESIAN_POINT('Ctrl Pts',(16.6866684347531,14.4209520888332,5.04059252345234));
#133045=CARTESIAN_POINT('Ctrl Pts',(16.689419504486,14.4398697401633,5.01663842720363));
#133046=CARTESIAN_POINT('Ctrl Pts',(16.6921461764301,14.4602558442988,4.99390399701323));
#133047=CARTESIAN_POINT('Ctrl Pts',(16.6947959895646,14.4819398756577,4.97259029927949));
#133048=CARTESIAN_POINT('Ctrl Pts',(16.6950795225656,14.4842600915272,4.97030970952653));
#133049=CARTESIAN_POINT('Ctrl Pts',(16.6953621755916,14.4865951746014,4.96804533731648));
#133050=CARTESIAN_POINT('Ctrl Pts',(16.6956438843734,14.4889449220592,4.96579739400117));
#133051=CARTESIAN_POINT('Ctrl Pts',(16.6956451434595,14.4889554241615,4.96578734690839));
#133052=CARTESIAN_POINT('Ctrl Pts',(16.6956464025288,14.4889659265784,4.96577730012147));
#133053=CARTESIAN_POINT('Ctrl Pts',(16.6956476615812,14.4889764293097,4.96576725364046));
#133054=CARTESIAN_POINT('Ctrl Pts',(16.698236415692,14.5105712324155,4.94511055288288));
#133055=CARTESIAN_POINT('Ctrl Pts',(16.7007538997991,14.5335000660394,4.92574657004337));
#133056=CARTESIAN_POINT('Ctrl Pts',(16.7032410770228,14.5575712947012,4.90783484987428));
#133057=CARTESIAN_POINT('Ctrl Pts',(16.7034977341184,14.5600552558676,4.90598650146011));
#133058=CARTESIAN_POINT('Ctrl Pts',(16.7037540684878,14.5625513363268,4.9041536210528));
#133059=CARTESIAN_POINT('Ctrl Pts',(16.7040101251433,14.5650592940532,4.90233638532723));
#133060=CARTESIAN_POINT('Ctrl Pts',(16.7067444065843,14.5918403291031,4.882931172413));
#133061=CARTESIAN_POINT('Ctrl Pts',(16.7094478580905,14.6199812640224,4.86530908904674));
#133062=CARTESIAN_POINT('Ctrl Pts',(16.712167454805,14.6492011879857,4.84963548072506));
#133063=CARTESIAN_POINT('Ctrl Pts',(16.714884248274,14.6783909932855,4.8339780280969));
#133064=CARTESIAN_POINT('Ctrl Pts',(16.7176176342296,14.7086571639179,4.82026463139376));
#133065=CARTESIAN_POINT('Ctrl Pts',(16.7203968275148,14.7397074937255,4.80861829985391));
#133066=CARTESIAN_POINT('Ctrl Pts',(16.7231746961215,14.770743023662,4.79697751943725));
#133067=CARTESIAN_POINT('Ctrl Pts',(16.7259985531871,14.8025617776855,4.78740157792263));
#133068=CARTESIAN_POINT('Ctrl Pts',(16.7288747721376,14.8348640907066,4.7799764809219));
#133069=CARTESIAN_POINT('Ctrl Pts',(16.7317533429524,14.8671928171055,4.77254531247075));
#133070=CARTESIAN_POINT('Ctrl Pts',(16.7346844029829,14.9000058437402,4.76726842074805));
#133071=CARTESIAN_POINT('Ctrl Pts',(16.7376495214185,14.932996634669,4.76419770746982));
#133072=CARTESIAN_POINT('Ctrl Pts',(16.7406160591147,14.9660032167143,4.76112552438776));
#133073=CARTESIAN_POINT('Ctrl Pts',(16.7436165249284,14.9991878060083,4.76026176405387));
#133074=CARTESIAN_POINT('Ctrl Pts',(16.7466084791747,15.0322371001287,4.76162383275038));
#133075=CARTESIAN_POINT('Ctrl Pts',(16.7496062354682,15.0653504839878,4.76298854279306));
#133076=CARTESIAN_POINT('Ctrl Pts',(16.7525949746064,15.0983281615029,4.76658822636295));
#133077=CARTESIAN_POINT('Ctrl Pts',(16.7555125529221,15.1308470796392,4.77240107403294));
#133078=CARTESIAN_POINT('Ctrl Pts',(16.7565452781547,15.1423576900358,4.77445862787109));
#133079=CARTESIAN_POINT('Ctrl Pts',(16.7575689474929,15.1538107410985,4.77679307545662));
#133080=CARTESIAN_POINT('Ctrl Pts',(16.7585804515502,15.1651916493713,4.77940202891363));
#133081=CARTESIAN_POINT('Ctrl Pts',(16.7585817106364,15.1652058159424,4.77940527645099));
#133082=CARTESIAN_POINT('Ctrl Pts',(16.7585829697057,15.165219982431,4.77940852441924));
#133083=CARTESIAN_POINT('Ctrl Pts',(16.7585842287581,15.1652341488371,4.77941177281841));
#133084=CARTESIAN_POINT('Ctrl Pts',(16.7611729828629,15.1943618804791,4.78609084857802));
#133085=CARTESIAN_POINT('Ctrl Pts',(16.7636904669635,15.2231433804942,4.79459499438346));
#133086=CARTESIAN_POINT('Ctrl Pts',(16.7661776441801,15.2513400157569,4.80485187133802));
#133087=CARTESIAN_POINT('Ctrl Pts',(16.7664343012795,15.2542496864349,4.80591030025496));
#133088=CARTESIAN_POINT('Ctrl Pts',(16.7666906356525,15.2571531011647,4.80698735709798));
#133089=CARTESIAN_POINT('Ctrl Pts',(16.7669466923117,15.2600499792979,4.80808293685841));
#133090=CARTESIAN_POINT('Ctrl Pts',(16.7696809737491,15.2909840707281,4.81978200147913));
#133091=CARTESIAN_POINT('Ctrl Pts',(16.7723844252509,15.3211765337626,4.8335973992389));
#133092=CARTESIAN_POINT('Ctrl Pts',(16.7751040219605,15.3503348016202,4.84938541269512));
#133093=CARTESIAN_POINT('Ctrl Pts',(16.7778208154246,15.3794630143664,4.86515715253361));
#133094=CARTESIAN_POINT('Ctrl Pts',(16.7805542013748,15.407559280387,4.88289688671094));
#133095=CARTESIAN_POINT('Ctrl Pts',(16.7833333946544,15.4343601838811,4.90242818442848));
#133096=CARTESIAN_POINT('Ctrl Pts',(16.7861112632556,15.461148312956,4.92195017272166));
#133097=CARTESIAN_POINT('Ctrl Pts',(16.7889351203156,15.4866424248478,4.94326171939172));
#133098=CARTESIAN_POINT('Ctrl Pts',(16.7918113392609,15.5106059100672,4.96615981685137));
#133099=CARTESIAN_POINT('Ctrl Pts',(16.7946899100705,15.5345889900622,4.9890766379265));
#133100=CARTESIAN_POINT('Ctrl Pts',(16.7976209700962,15.5570389841673,5.01358251613917));
#133101=CARTESIAN_POINT('Ctrl Pts',(16.8005860885279,15.5777439905351,5.03944995274565));
#133102=CARTESIAN_POINT('Ctrl Pts',(16.8035526262203,15.5984589074007,5.06532977085873));
#133103=CARTESIAN_POINT('Ctrl Pts',(16.8065530920311,15.617427095542,5.0925725843381));
#133104=CARTESIAN_POINT('Ctrl Pts',(16.8095450462761,15.6344617451785,5.12092627517138));
#133105=CARTESIAN_POINT('Ctrl Pts',(16.8125428025684,15.6515294286896,5.1493349499514));
#133106=CARTESIAN_POINT('Ctrl Pts',(16.8155315417069,15.6666557095804,5.1788591868016));
#133107=CARTESIAN_POINT('Ctrl Pts',(16.818449120025,15.6796811719533,5.20921716044695));
#133108=CARTESIAN_POINT('Ctrl Pts',(16.8194818452668,15.6842917504234,5.21996286878954));
#133109=CARTESIAN_POINT('Ctrl Pts',(16.8205055146144,15.6886394013387,5.23081275163717));
#133110=CARTESIAN_POINT('Ctrl Pts',(16.8215170186811,15.6927181004045,5.24175331502708));
#133111=CARTESIAN_POINT('Ctrl Pts',(16.8215182777672,15.6927231774313,5.24176693347078));
#133112=CARTESIAN_POINT('Ctrl Pts',(16.8215195368365,15.6927282540528,5.24178055208245));
#133113=CARTESIAN_POINT('Ctrl Pts',(16.8215207958888,15.692733330269,5.24179417086212));
#133114=CARTESIAN_POINT('Ctrl Pts',(16.8241095500145,15.7031706050995,5.26979592275927));
#133115=CARTESIAN_POINT('Ctrl Pts',(16.8266270341365,15.7118930947728,5.29851200578593));
#133116=CARTESIAN_POINT('Ctrl Pts',(16.8291142113749,15.7188300073692,5.32770332332898));
#133117=CARTESIAN_POINT('Ctrl Pts',(16.8293708684722,15.7195458421008,5.3307156373331));
#133118=CARTESIAN_POINT('Ctrl Pts',(16.8296272028431,15.7202426778066,5.33373296865914));
#133119=CARTESIAN_POINT('Ctrl Pts',(16.8298832595002,15.7209204478801,5.3367550251531));
#133120=CARTESIAN_POINT('Ctrl Pts',(16.8326175409575,15.7281579638471,5.36902582462275));
#133121=CARTESIAN_POINT('Ctrl Pts',(16.83532099248,15.7332200032505,5.40184084872015));
#133122=CARTESIAN_POINT('Ctrl Pts',(16.8380405892106,15.7360657380996,5.43487670433805));
#133123=CARTESIAN_POINT('Ctrl Pts',(16.8407573826957,15.7389085396853,5.467878507991));
#133124=CARTESIAN_POINT('Ctrl Pts',(16.8434907686671,15.7395401330745,5.50110048012781));
#133125=CARTESIAN_POINT('Ctrl Pts',(16.8462699619677,15.7379630432526,5.53422558867269));
#133126=CARTESIAN_POINT('Ctrl Pts',(16.8490478305899,15.7363867051369,5.56733490842048));
#133127=CARTESIAN_POINT('Ctrl Pts',(16.8518716876706,15.732604098387,5.60034738573811));
#133128=CARTESIAN_POINT('Ctrl Pts',(16.8547479066354,15.726654686108,5.63295376539774));
#133129=CARTESIAN_POINT('Ctrl Pts',(16.8576264774643,15.7207004090362,5.66558680706586));
#133130=CARTESIAN_POINT('Ctrl Pts',(16.8605575375082,15.7125758807696,5.69781307511916));
#133131=CARTESIAN_POINT('Ctrl Pts',(16.8635226559561,15.7023546065231,5.72933048503895));
#133132=CARTESIAN_POINT('Ctrl Pts',(16.8664891936645,15.692128439841,5.76086298083677));
#133133=CARTESIAN_POINT('Ctrl Pts',(16.8694896594893,15.6798033696425,5.79168595445143));
#133134=CARTESIAN_POINT('Ctrl Pts',(16.872481613745,15.6654872616378,5.82150474272471));
#133135=CARTESIAN_POINT('Ctrl Pts',(16.8754793700477,15.651143391601,5.85138135608267));
#133136=CARTESIAN_POINT('Ctrl Pts',(16.8784681091935,15.6348002466764,5.88024979143524));
#133137=CARTESIAN_POINT('Ctrl Pts',(16.8813856875151,15.6166055685332,5.90782193193857));
#133138=CARTESIAN_POINT('Ctrl Pts',(16.8824184126543,15.6101652610429,5.9175815474487));
#133139=CARTESIAN_POINT('Ctrl Pts',(16.8834420819007,15.6034933686891,5.92717883105449));
#133140=CARTESIAN_POINT('Ctrl Pts',(16.8844535858685,15.5965978499449,5.93660133118031));
#133141=CARTESIAN_POINT('Ctrl Pts',(16.8844548449546,15.5965892666349,5.93661305999177));
#133142=CARTESIAN_POINT('Ctrl Pts',(16.8844561040239,15.5965806829618,5.93662478855707));
#133143=CARTESIAN_POINT('Ctrl Pts',(16.8844573630763,15.5965720989255,5.93663651687619));
#133144=CARTESIAN_POINT('Ctrl Pts',(16.8870461171823,15.5789223498776,5.96075126681616));
#133145=CARTESIAN_POINT('Ctrl Pts',(16.8895636012852,15.5597330649106,5.9838265042824));
#133146=CARTESIAN_POINT('Ctrl Pts',(16.8920507785056,15.5391650265205,6.00567163107275));
#133147=CARTESIAN_POINT('Ctrl Pts',(16.8923074355913,15.5370425670722,6.00792587597812));
#133148=CARTESIAN_POINT('Ctrl Pts',(16.8925637699507,15.5349054701415,6.01016701056156));
#133149=CARTESIAN_POINT('Ctrl Pts',(16.8928198265962,15.5327539431289,6.01239481854684));
#133150=CARTESIAN_POINT('Ctrl Pts',(16.8955541080245,15.5097790254493,6.03618429679496));
#133151=CARTESIAN_POINT('Ctrl Pts',(16.8982575595193,15.4851533413693,6.05845593155753));
#133152=CARTESIAN_POINT('Ctrl Pts',(16.9009771562235,15.4591245586892,6.0789978014248));
#133153=CARTESIAN_POINT('Ctrl Pts',(16.9036939496823,15.4331226053783,6.09951849760078));
#133154=CARTESIAN_POINT('Ctrl Pts',(16.9064273356287,15.4057209095348,6.11831332109029));
#133155=CARTESIAN_POINT('Ctrl Pts',(16.9092065289052,15.3771856637107,6.13521005913319));
#133156=CARTESIAN_POINT('Ctrl Pts',(16.9119843975034,15.3486640189634,6.1520987434928));
#133157=CARTESIAN_POINT('Ctrl Pts',(16.9148082545612,15.3190101342279,6.16709137084068));
#133158=CARTESIAN_POINT('Ctrl Pts',(16.9176844735039,15.2885040169897,6.18005085748797));
#133159=CARTESIAN_POINT('Ctrl Pts',(16.9205630443112,15.2579729551071,6.19302094101928));
#133160=CARTESIAN_POINT('Ctrl Pts',(16.9234941043344,15.2265883307033,6.20395463414458));
#133161=CARTESIAN_POINT('Ctrl Pts',(16.9264592227623,15.1946428800942,6.21274723003703));
#133162=CARTESIAN_POINT('Ctrl Pts',(16.9294257604509,15.1626821387212,6.22154403452584));
#133163=CARTESIAN_POINT('Ctrl Pts',(16.9324262262567,15.1301599394637,6.22819757454658));
#133164=CARTESIAN_POINT('Ctrl Pts',(16.9354181804942,15.0973817131741,6.23263592389099));
#133165=CARTESIAN_POINT('Ctrl Pts',(16.9384159367794,15.0645399228002,6.23708288015662));
#133166=CARTESIAN_POINT('Ctrl Pts',(16.9414046759084,15.0314409111029,6.23930557025361));
#133167=CARTESIAN_POINT('Ctrl Pts',(16.9443222542134,14.9984065670693,6.23926897428871));
#133168=CARTESIAN_POINT('Ctrl Pts',(16.9453549795373,14.9867135120508,6.2392560205388));
#133169=CARTESIAN_POINT('Ctrl Pts',(16.946378648965,14.9750287081898,6.23896037407447));
#133170=CARTESIAN_POINT('Ctrl Pts',(16.9473901531091,14.963366931805,6.23838183572383));
#133171=CARTESIAN_POINT('Ctrl Pts',(16.9473914121955,14.9633524156181,6.23838111557875));
#133172=CARTESIAN_POINT('Ctrl Pts',(16.9473926712649,14.9633378994371,6.23838039499499));
#133173=CARTESIAN_POINT('Ctrl Pts',(16.9473939303175,14.963323383262,6.23837967397251));
#133174=CARTESIAN_POINT('Ctrl Pts',(16.949982684385,14.9334764912267,6.23689717049036));
#133175=CARTESIAN_POINT('Ctrl Pts',(16.9525001684468,14.9036513402204,6.23355717295173));
#133176=CARTESIAN_POINT('Ctrl Pts',(16.9549873456218,14.8740955363832,6.22838917508527));
#133177=CARTESIAN_POINT('Ctrl Pts',(16.9552440027414,14.8710456099215,6.22785587835838));
#133178=CARTESIAN_POINT('Ctrl Pts',(16.9555003371347,14.8679985854887,6.22730314674342));
#133179=CARTESIAN_POINT('Ctrl Pts',(16.9557563938139,14.8649547577722,6.22673103455314));
#133180=CARTESIAN_POINT('Ctrl Pts',(16.9584906752287,14.8324514792832,6.22062177884627));
#133181=CARTESIAN_POINT('Ctrl Pts',(16.9611941267044,14.8003083118629,6.21229910980488));
#133182=CARTESIAN_POINT('Ctrl Pts',(16.9639137233856,14.7688384464318,6.20185336829151));
#133183=CARTESIAN_POINT('Ctrl Pts',(16.9666305168212,14.7374010188114,6.19141839380819));
#133184=CARTESIAN_POINT('Ctrl Pts',(16.9693639027405,14.7066354875256,6.17886529019366));
#133185=CARTESIAN_POINT('Ctrl Pts',(16.972143095989,14.6768320623852,6.16432170530663));
#133186=CARTESIAN_POINT('Ctrl Pts',(16.9749209645589,14.6470428427916,6.14978505249452));
#133187=CARTESIAN_POINT('Ctrl Pts',(16.9777448215873,14.6182147553789,6.13326012794015));
#133188=CARTESIAN_POINT('Ctrl Pts',(16.9806210405032,14.5906162642677,6.11490543446986));
#133189=CARTESIAN_POINT('Ctrl Pts',(16.9834996112832,14.5629952060628,6.09653573249482));
#133190=CARTESIAN_POINT('Ctrl Pts',(16.9864306712816,14.53660572719,6.07633336382567));
#133191=CARTESIAN_POINT('Ctrl Pts',(16.9893957896912,14.5116962476894,6.05448526576069));
#133192=CARTESIAN_POINT('Ctrl Pts',(16.9923623273612,14.4867748452112,6.03262671005515));
#133193=CARTESIAN_POINT('Ctrl Pts',(16.9953627931549,14.4633349049778,6.00912070567207));
#133194=CARTESIAN_POINT('Ctrl Pts',(16.9983547473907,14.4416044468513,5.98418281774479));
#133195=CARTESIAN_POINT('Ctrl Pts',(17.0013525036737,14.4198318486605,5.95919656985214));
#133196=CARTESIAN_POINT('Ctrl Pts',(17.0043412428111,14.3997756562837,5.93277245066423));
#133197=CARTESIAN_POINT('Ctrl Pts',(17.0072588211384,14.381642112811,5.90516006526719));
#133198=CARTESIAN_POINT('Ctrl Pts',(17.008291546456,14.3752234438528,5.89538620274128));
#133199=CARTESIAN_POINT('Ctrl Pts',(17.0093152158794,14.3690454337186,5.88546379198059));
#133200=CARTESIAN_POINT('Ctrl Pts',(17.0103267200215,14.3631163736062,5.87540506553523));
#133201=CARTESIAN_POINT('Ctrl Pts',(17.0103279791075,14.3631089933137,5.87539254477437));
#133202=CARTESIAN_POINT('Ctrl Pts',(17.0103292381764,14.3631016133924,5.87538002377966));
#133203=CARTESIAN_POINT('Ctrl Pts',(17.0103304972283,14.3630942338424,5.87536750255111));
#133204=CARTESIAN_POINT('Ctrl Pts',(17.0129669905362,14.3476412299281,5.8491476661129));
#133205=CARTESIAN_POINT('Ctrl Pts',(17.0155288023521,14.333816461648,5.8218980821737));
#133206=CARTESIAN_POINT('Ctrl Pts',(17.018059794483,14.3217298456503,5.79384698268585));
#133207=CARTESIAN_POINT('Ctrl Pts',(17.0183643532261,14.320275441849,5.79047154445453));
#133208=CARTESIAN_POINT('Ctrl Pts',(17.0186684657083,14.3188462012054,5.7870845623239));
#133209=CARTESIAN_POINT('Ctrl Pts',(17.0189722083533,14.3174423095076,5.78368648438178));
#133210=CARTESIAN_POINT('Ctrl Pts',(17.0199941883175,14.3127187410174,5.77225322787141));
#133211=CARTESIAN_POINT('Ctrl Pts',(17.0210119584363,14.3082816751944,5.76069359196684));
#133212=CARTESIAN_POINT('Ctrl Pts',(17.0220282051085,14.3041366315448,5.74902320646588));
#133213=CARTESIAN_POINT('Origin',(13.2437274406976,15.,5.5));
#133214=CARTESIAN_POINT('',(17.5003341500486,14.3042076695831,5.74898600951276));
#133215=CARTESIAN_POINT('',(17.4213402632629,14.3044416670805,5.74885636750768));
#133216=CARTESIAN_POINT('',(13.2437274406976,14.3042076641721,5.74898599439144));
#133217=CARTESIAN_POINT('Ctrl Pts',(17.5003341513661,14.3042076696198,5.74898600961524));
#133218=CARTESIAN_POINT('Ctrl Pts',(17.4972553158012,14.3167672541012,5.78408381518432));
#133219=CARTESIAN_POINT('Ctrl Pts',(17.4942672188542,14.3319708724109,5.81819884060891));
#133220=CARTESIAN_POINT('Ctrl Pts',(17.4881127680215,14.3682787239195,5.88546027188228));
#133221=CARTESIAN_POINT('Ctrl Pts',(17.4849548566992,14.3895632982255,5.91835138223574));
#133222=CARTESIAN_POINT('Ctrl Pts',(17.4805719250421,14.4216642604325,5.96025617662959));
#133223=CARTESIAN_POINT('Ctrl Pts',(17.4794269773732,14.430278752553,5.97087750846475));
#133224=CARTESIAN_POINT('Ctrl Pts',(17.4775083910314,14.4450506291391,5.98809158652496));
#133225=CARTESIAN_POINT('Ctrl Pts',(17.4767414204593,14.4510431997034,5.99482180356909));
#133226=CARTESIAN_POINT('Ctrl Pts',(17.4751976334742,14.4632679565182,6.00805592303277));
#133227=CARTESIAN_POINT('Ctrl Pts',(17.4744209550709,14.4694989702461,6.01455879081484));
#133228=CARTESIAN_POINT('Ctrl Pts',(17.472454575248,14.4854656639902,6.03062378244077));
#133229=CARTESIAN_POINT('Ctrl Pts',(17.4712585933215,14.4953498166343,6.04003270274499));
#133230=CARTESIAN_POINT('Ctrl Pts',(17.4659219023786,14.5401729688918,6.08039526416728));
#133231=CARTESIAN_POINT('Ctrl Pts',(17.4616648018957,14.5777326604915,6.10826666023725));
#133232=CARTESIAN_POINT('Ctrl Pts',(17.4548342759243,14.6413256415667,6.14671353176405));
#133233=CARTESIAN_POINT('Ctrl Pts',(17.4522889052361,14.665775403901,6.15968155006906));
#133234=CARTESIAN_POINT('Ctrl Pts',(17.4487659629934,14.7010388234447,6.17592005403915));
#133235=CARTESIAN_POINT('Ctrl Pts',(17.4477589957908,14.7112873842711,6.18036075857157));
#133236=CARTESIAN_POINT('Ctrl Pts',(17.4459805103426,14.7297342480112,6.18786183205677));
#133237=CARTESIAN_POINT('Ctrl Pts',(17.4452054447519,14.7378936057274,6.19101210962597));
#133238=CARTESIAN_POINT('Ctrl Pts',(17.4439797511875,14.7510109136677,6.19581081915619));
#133239=CARTESIAN_POINT('Ctrl Pts',(17.4435242929751,14.7559334604094,6.19755271581981));
#133240=CARTESIAN_POINT('Ctrl Pts',(17.4426120944944,14.7658962211096,6.2009597631587));
#133241=CARTESIAN_POINT('Ctrl Pts',(17.44215546894,14.7709367198055,6.20262307677959));
#133242=CARTESIAN_POINT('Ctrl Pts',(17.4409175937611,14.7847349068951,6.20701206158565));
#133243=CARTESIAN_POINT('Ctrl Pts',(17.4401420942822,14.7935264853455,6.20962935900119));
#133244=CARTESIAN_POINT('Ctrl Pts',(17.4365288396037,14.835072150401,6.22116014710213));
#133245=CARTESIAN_POINT('Ctrl Pts',(17.4337809467226,14.8683703438025,6.22797486952268));
#133246=CARTESIAN_POINT('Ctrl Pts',(17.4281623663082,14.9374594804032,6.23721630585713));
#133247=CARTESIAN_POINT('Ctrl Pts',(17.4252996026559,14.9731913928919,6.23937834349708));
#133248=CARTESIAN_POINT('Ctrl Pts',(17.4210917831851,15.0247218210748,6.23875502303427));
#133249=CARTESIAN_POINT('Ctrl Pts',(17.4197935663145,15.0404940500274,6.23805848364246));
#133250=CARTESIAN_POINT('Ctrl Pts',(17.4173785191698,15.0694650856811,6.23584764944318));
#133251=CARTESIAN_POINT('Ctrl Pts',(17.4162661623708,15.0826686903264,6.23448145293848));
#133252=CARTESIAN_POINT('Ctrl Pts',(17.4143863539818,15.1046921126254,6.23160131619872));
#133253=CARTESIAN_POINT('Ctrl Pts',(17.4136249880668,15.1135344755246,6.23028133778899));
#133254=CARTESIAN_POINT('Ctrl Pts',(17.4121710105326,15.1302595083462,6.22747355882875));
#133255=CARTESIAN_POINT('Ctrl Pts',(17.4114794823583,15.1381462078188,6.22601717095219));
#133256=CARTESIAN_POINT('Ctrl Pts',(17.4096483898093,15.1588404287998,6.22184631112805));
#133257=CARTESIAN_POINT('Ctrl Pts',(17.4085023743042,15.1716016049001,6.2189194810426));
#133258=CARTESIAN_POINT('Ctrl Pts',(17.4026644463572,15.2355995079454,6.20244036307807));
#133259=CARTESIAN_POINT('Ctrl Pts',(17.3978146161543,15.2853414486772,6.18374533499249));
#133260=CARTESIAN_POINT('Ctrl Pts',(17.3899365297226,15.3618650182442,6.14517078710181));
#133261=CARTESIAN_POINT('Ctrl Pts',(17.3869332843097,15.3900757758338,6.12851646826257));
#133262=CARTESIAN_POINT('Ctrl Pts',(17.3831751251128,15.4247543845494,6.10480647307162));
#133263=CARTESIAN_POINT('Ctrl Pts',(17.3823512528713,15.4323179264026,6.09942338296729));
#133264=CARTESIAN_POINT('Ctrl Pts',(17.3810676167843,15.4440617714532,6.09072713565176));
#133265=CARTESIAN_POINT('Ctrl Pts',(17.3806022536796,15.448310767146,6.08750903591734));
#133266=CARTESIAN_POINT('Ctrl Pts',(17.3796890629601,15.4566368328577,6.08106011388874));
#133267=CARTESIAN_POINT('Ctrl Pts',(17.3792411373661,15.4607153085466,6.07783168987902));
#133268=CARTESIAN_POINT('Ctrl Pts',(17.3780560003865,15.4714818473284,6.0691226805321));
#133269=CARTESIAN_POINT('Ctrl Pts',(17.3773237329482,15.4781086852653,6.06356708854487));
#133270=CARTESIAN_POINT('Ctrl Pts',(17.3729155636115,15.5177434826501,6.02913686594567));
#133271=CARTESIAN_POINT('Ctrl Pts',(17.369399024819,15.5482296430383,5.99748324302881));
#133272=CARTESIAN_POINT('Ctrl Pts',(17.3623485650639,15.6031403928285,5.92924814340135));
#133273=CARTESIAN_POINT('Ctrl Pts',(17.3588270392535,15.6274693853144,5.89282789855888));
#133274=CARTESIAN_POINT('Ctrl Pts',(17.3541259872636,15.6545601417638,5.84327108936484));
#133275=CARTESIAN_POINT('Ctrl Pts',(17.3530546324049,15.6603927359816,5.83191175705035));
#133276=CARTESIAN_POINT('Ctrl Pts',(17.3512232269182,15.6697668239488,5.81242887405811));
#133277=CARTESIAN_POINT('Ctrl Pts',(17.350468550847,15.673461912783,5.80438205821612));
#133278=CARTESIAN_POINT('Ctrl Pts',(17.3490136729502,15.6802601245934,5.78884741519722));
#133279=CARTESIAN_POINT('Ctrl Pts',(17.3483143760169,15.6833864026305,5.7813710711164));
#133280=CARTESIAN_POINT('Ctrl Pts',(17.3464284689983,15.6914364023944,5.76119386100506));
#133281=CARTESIAN_POINT('Ctrl Pts',(17.3452346368047,15.6961326977508,5.74840641126145));
#133282=CARTESIAN_POINT('Ctrl Pts',(17.3405659245649,15.7129493797112,5.69838621438272));
#133283=CARTESIAN_POINT('Ctrl Pts',(17.3370134985905,15.7224550607806,5.66034846312654));
#133284=CARTESIAN_POINT('Ctrl Pts',(17.3303908306401,15.7343481749539,5.58914178676758));
#133285=CARTESIAN_POINT('Ctrl Pts',(17.3273399070407,15.7376000936515,5.5562112461603));
#133286=CARTESIAN_POINT('Ctrl Pts',(17.3232203449116,15.7390203373181,5.51094108151652));
#133287=CARTESIAN_POINT('Ctrl Pts',(17.3221141862803,15.7391002079377,5.49870072897666));
#133288=CARTESIAN_POINT('Ctrl Pts',(17.3201825555629,15.7387047717546,5.47711660377838));
#133289=CARTESIAN_POINT('Ctrl Pts',(17.3193526676311,15.7383561857298,5.46777334067163));
#133290=CARTESIAN_POINT('Ctrl Pts',(17.3180618964234,15.7375298708302,5.45310396790918));
#133291=CARTESIAN_POINT('Ctrl Pts',(17.3175953162649,15.737171516468,5.44777252543667));
#133292=CARTESIAN_POINT('Ctrl Pts',(17.3166818254238,15.736351115501,5.43727062804039));
#133293=CARTESIAN_POINT('Ctrl Pts',(17.3162347928536,15.7358923645335,5.43210028471894));
#133294=CARTESIAN_POINT('Ctrl Pts',(17.3150552043292,15.7345297889885,5.41838633548142));
#133295=CARTESIAN_POINT('Ctrl Pts',(17.3143275088876,15.7335313612004,5.40985254694462));
#133296=CARTESIAN_POINT('Ctrl Pts',(17.3098755623672,15.726453933101,5.3573158777159));
#133297=CARTESIAN_POINT('Ctrl Pts',(17.3063154763725,15.7165656769522,5.31391150405181));
#133298=CARTESIAN_POINT('Ctrl Pts',(17.299258459848,15.6894777051499,5.23053668676709));
#133299=CARTESIAN_POINT('Ctrl Pts',(17.2957747123472,15.6725389913239,5.19067721357551));
#133300=CARTESIAN_POINT('Ctrl Pts',(17.2911133554634,15.6462068937121,5.14125083197125));
#133301=CARTESIAN_POINT('Ctrl Pts',(17.2900410608193,15.6399069496065,5.13013060275953));
#133302=CARTESIAN_POINT('Ctrl Pts',(17.2882085393285,15.6287583889146,5.11159000477155));
#133303=CARTESIAN_POINT('Ctrl Pts',(17.2874537028228,15.6240586683491,5.10408308952639));
#133304=CARTESIAN_POINT('Ctrl Pts',(17.2859988391251,15.6148036617242,5.08987429640336));
#133305=CARTESIAN_POINT('Ctrl Pts',(17.2852997210036,15.6102707973551,5.08315928976659));
#133306=CARTESIAN_POINT('Ctrl Pts',(17.2834151216731,15.5978305048511,5.06536811794136));
#133307=CARTESIAN_POINT('Ctrl Pts',(17.2822224374505,15.5897263981578,5.05443417170294));
#133308=CARTESIAN_POINT('Ctrl Pts',(17.2776065800594,15.5575123116031,5.01339068248128));
#133309=CARTESIAN_POINT('Ctrl Pts',(17.2741085145448,15.5313642809265,4.98496633100814));
#133310=CARTESIAN_POINT('Ctrl Pts',(17.2674998463669,15.4785847887242,4.93590789039152));
#133311=CARTESIAN_POINT('Ctrl Pts',(17.2644070207186,15.4525240480725,4.91479457515334));
#133312=CARTESIAN_POINT('Ctrl Pts',(17.2602387033681,15.4150438298827,4.88843530709106));
#133313=CARTESIAN_POINT('Ctrl Pts',(17.2591250392081,15.4047910983087,4.88160129293183));
#133314=CARTESIAN_POINT('Ctrl Pts',(17.2571819021886,15.3864279797015,4.87001377413554));
#133315=CARTESIAN_POINT('Ctrl Pts',(17.2563479449911,15.3783888842978,4.86515269097576));
#133316=CARTESIAN_POINT('Ctrl Pts',(17.2550523438402,15.3656268249375,4.85776431882953));
#133317=CARTESIAN_POINT('Ctrl Pts',(17.2545849367553,15.3609656982122,4.85513302486518));
#133318=CARTESIAN_POINT('Ctrl Pts',(17.2536712250853,15.3517351974141,4.85005368275396));
#133319=CARTESIAN_POINT('Ctrl Pts',(17.253224782554,15.347167900265,4.84760263840116));
#133320=CARTESIAN_POINT('Ctrl Pts',(17.2520488565903,15.3349955242147,4.84123435738164));
#133321=CARTESIAN_POINT('Ctrl Pts',(17.2513241789541,15.3273472363192,4.83740058874753));
#133322=CARTESIAN_POINT('Ctrl Pts',(17.2468453907719,15.279269591135,4.81433704999345));
#133323=CARTESIAN_POINT('Ctrl Pts',(17.2432584704832,15.2372230829113,4.79867864571787));
#133324=CARTESIAN_POINT('Ctrl Pts',(17.236229241115,15.1529678813465,4.77575478051669));
#133325=CARTESIAN_POINT('Ctrl Pts',(17.2328008102522,15.1110415590772,4.76815342371463));
#133326=CARTESIAN_POINT('Ctrl Pts',(17.2281841570181,15.0557860959489,4.76299452374808));
#133327=CARTESIAN_POINT('Ctrl Pts',(17.227096570197,15.0428459306969,4.76212918119837));
#133328=CARTESIAN_POINT('Ctrl Pts',(17.2252460531384,15.0210099546185,4.76124525410686));
#133329=CARTESIAN_POINT('Ctrl Pts',(17.2244887760184,15.0121241056453,4.76104602023288));
#133330=CARTESIAN_POINT('Ctrl Pts',(17.2230345123442,14.9951692815685,4.76097174808373));
#133331=CARTESIAN_POINT('Ctrl Pts',(17.2223385031601,14.987101661909,4.76106853187728));
#133332=CARTESIAN_POINT('Ctrl Pts',(17.2204756393179,14.9656444599169,4.76167743018121));
#133333=CARTESIAN_POINT('Ctrl Pts',(17.2193018897837,14.9522651578383,4.76242162853785));
#133334=CARTESIAN_POINT('Ctrl Pts',(17.2136806686628,14.8889058233142,4.7676768842616));
#133335=CARTESIAN_POINT('Ctrl Pts',(17.2090948613312,14.8394589897758,4.77690679133383));
#133336=CARTESIAN_POINT('Ctrl Pts',(17.2021276124978,14.7667594346147,4.79830469824513));
#133337=CARTESIAN_POINT('Ctrl Pts',(17.1997724484413,14.7425721087787,4.80681281243023));
#133338=CARTESIAN_POINT('Ctrl Pts',(17.1960619496991,14.7047160181459,4.82238451130966));
#133339=CARTESIAN_POINT('Ctrl Pts',(17.1946867633643,14.6907405367587,4.82864759232853));
#133340=CARTESIAN_POINT('Ctrl Pts',(17.1927685570382,14.6712357464062,4.83812713269096));
#133341=CARTESIAN_POINT('Ctrl Pts',(17.192208449292,14.6655389844987,4.84098750773224));
#133342=CARTESIAN_POINT('Ctrl Pts',(17.1912259241255,14.6555345742557,4.84617393443511));
#133343=CARTESIAN_POINT('Ctrl Pts',(17.1908018582693,14.6512120472506,4.84846955413507));
#133344=CARTESIAN_POINT('Ctrl Pts',(17.1898327539284,14.6413249768413,4.85384701553971));
#133345=CARTESIAN_POINT('Ctrl Pts',(17.1892894797715,14.6357769078452,4.85695801104753));
#133346=CARTESIAN_POINT('Ctrl Pts',(17.1877683150316,14.6202480380471,4.86593107106127));
#133347=CARTESIAN_POINT('Ctrl Pts',(17.1867993688603,14.6103633000766,4.87195681379342));
#133348=CARTESIAN_POINT('Ctrl Pts',(17.181860133925,14.5602415742904,4.90415020883126));
#133349=CARTESIAN_POINT('Ctrl Pts',(17.1780445005885,14.5224781849726,4.93396257138102));
#133350=CARTESIAN_POINT('Ctrl Pts',(17.1719584401556,14.4681245241494,4.98621053043894));
#133351=CARTESIAN_POINT('Ctrl Pts',(17.1697343947959,14.4494512517061,5.00627235077205));
#133352=CARTESIAN_POINT('Ctrl Pts',(17.1661944107989,14.4220653978625,5.03918471847699));
#133353=CARTESIAN_POINT('Ctrl Pts',(17.1649069705786,14.4125699151752,5.05135207933829));
#133354=CARTESIAN_POINT('Ctrl Pts',(17.1628175416868,14.3979544137257,5.07134022138535));
#133355=CARTESIAN_POINT('Ctrl Pts',(17.1620249741564,14.3925894540662,5.07897683467634));
#133356=CARTESIAN_POINT('Ctrl Pts',(17.1604757732621,14.3824586072107,5.093994116164));
#133357=CARTESIAN_POINT('Ctrl Pts',(17.1597198920099,14.3776768745417,5.10136224143373));
#133358=CARTESIAN_POINT('Ctrl Pts',(17.1578917417277,14.3665047766077,5.11926826499025));
#133359=CARTESIAN_POINT('Ctrl Pts',(17.1568150229615,14.3602447117821,5.12988382448421));
#133360=CARTESIAN_POINT('Ctrl Pts',(17.1505592434479,14.3257297973587,5.19190665856902));
#133361=CARTESIAN_POINT('Ctrl Pts',(17.1451777429052,14.303416073196,5.24636693159946));
#133362=CARTESIAN_POINT('Ctrl Pts',(17.1370839950809,14.2799168439172,5.33127148617539));
#133363=CARTESIAN_POINT('Ctrl Pts',(17.134387508867,14.273762103389,5.36011453335841));
#133364=CARTESIAN_POINT('Ctrl Pts',(17.1309577831167,14.268010081453,5.39806279212652));
#133365=CARTESIAN_POINT('Ctrl Pts',(17.1301674933819,14.2668338306156,5.40689884409029));
#133366=CARTESIAN_POINT('Ctrl Pts',(17.1289237390216,14.2652186113887,5.4209751681117));
#133367=CARTESIAN_POINT('Ctrl Pts',(17.1284652089325,14.2646752364168,5.42620223133049));
#133368=CARTESIAN_POINT('Ctrl Pts',(17.1276093151926,14.2637588866787,5.43603611896898));
#133369=CARTESIAN_POINT('Ctrl Pts',(17.1272112647142,14.2633732820652,5.44064145291514));
#133370=CARTESIAN_POINT('Ctrl Pts',(17.1261081807337,14.2624191916769,5.45348417390834));
#133371=CARTESIAN_POINT('Ctrl Pts',(17.1254080284913,14.2619454875646,5.46172826718913));
#133372=CARTESIAN_POINT('Ctrl Pts',(17.120727278434,14.2596842394592,5.51734562730788));
#133373=CARTESIAN_POINT('Ctrl Pts',(17.1169379661085,14.2623203270669,5.56479544511568));
#133374=CARTESIAN_POINT('Ctrl Pts',(17.1099792581425,14.2753797401333,5.65022502463752));
#133375=CARTESIAN_POINT('Ctrl Pts',(17.1068305705428,14.2843152073538,5.68824668079661));
#133376=CARTESIAN_POINT('Ctrl Pts',(17.102902867527,14.2987417464203,5.73329572408496));
#133377=CARTESIAN_POINT('Ctrl Pts',(17.1022094454944,14.3014087825667,5.74116450882544));
#133378=CARTESIAN_POINT('Ctrl Pts',(17.1015120386236,14.3042076645209,5.7489859953664));
#133379=CARTESIAN_POINT('',(17.0432316689992,14.2612664936,5.49980856841249));
#133380=CARTESIAN_POINT('Ctrl Pts',(17.0220737370494,14.3042126623665,5.74899996142335));
#133381=CARTESIAN_POINT('Ctrl Pts',(17.0254895451321,14.2899493039172,5.70914347251323));
#133382=CARTESIAN_POINT('Ctrl Pts',(17.0288728794103,14.2791376675812,5.66813750052812));
#133383=CARTESIAN_POINT('Ctrl Pts',(17.0339152333952,14.2686243049792,5.60759292999941));
#133384=CARTESIAN_POINT('Ctrl Pts',(17.0354997623189,14.2660855606134,5.58863477947617));
#133385=CARTESIAN_POINT('Ctrl Pts',(17.0379545737325,14.2633339362743,5.55954880952728));
#133386=CARTESIAN_POINT('Ctrl Pts',(17.0388087427715,14.2625891360241,5.54947875477171));
#133387=CARTESIAN_POINT('Ctrl Pts',(17.0402426101667,14.2616922806603,5.53267971049496));
#133388=CARTESIAN_POINT('Ctrl Pts',(17.0408187074412,14.2614254076138,5.52595798472993));
#133389=CARTESIAN_POINT('Ctrl Pts',(17.0419554109074,14.2610816714149,5.5127554362252));
#133390=CARTESIAN_POINT('Ctrl Pts',(17.0425157620651,14.2609982333761,5.50627538393103));
#133391=CARTESIAN_POINT('Ctrl Pts',(17.0430787344308,14.2610000283511,5.49979529801652));
#133392=CARTESIAN_POINT('Ctrl Pts',(17.0432403769393,14.2612816658625,5.49980932401545));
#133393=CARTESIAN_POINT('Ctrl Pts',(17.046308805676,14.2612728636063,5.46438385344786));
#133394=CARTESIAN_POINT('Ctrl Pts',(17.0494339926232,14.263783384481,5.42902470624598));
#133395=CARTESIAN_POINT('Ctrl Pts',(17.052595132431,14.2687728192454,5.39408059525951));
#133396=CARTESIAN_POINT('Ctrl Pts',(17.0557641770926,14.27377473076,5.35904910184047));
#133397=CARTESIAN_POINT('Ctrl Pts',(17.0589691313495,14.281268181868,5.32443430767273));
#133398=CARTESIAN_POINT('Ctrl Pts',(17.0621585736971,14.2911823715331,5.29058356494859));
#133399=CARTESIAN_POINT('Ctrl Pts',(17.065079447934,14.3002617333829,5.25958323587894));
#133400=CARTESIAN_POINT('Ctrl Pts',(17.0679867788057,14.3113720892566,5.22922255134883));
#133401=CARTESIAN_POINT('Ctrl Pts',(17.0708225258615,14.3244300074377,5.19977228326336));
#133402=CARTESIAN_POINT('Ctrl Pts',(17.071094799487,14.3256837605594,5.19694462229645));
#133403=CARTESIAN_POINT('Ctrl Pts',(17.0713664131928,14.3269554708206,5.19412531468191));
#133404=CARTESIAN_POINT('Ctrl Pts',(17.0716373156049,14.3282450672071,5.19131457491902));
#133405=CARTESIAN_POINT('Ctrl Pts',(17.0721823852581,14.3308398017824,5.18565922125862));
#133406=CARTESIAN_POINT('Ctrl Pts',(17.0727245311859,14.3335068116493,5.18003875659509));
#133407=CARTESIAN_POINT('Ctrl Pts',(17.0732632874351,14.3362453362973,5.17445512840284));
#133408=CARTESIAN_POINT('Ctrl Pts',(17.0732645465214,14.3362517362952,5.17444207932964));
#133409=CARTESIAN_POINT('Ctrl Pts',(17.0732658055909,14.3362581366937,5.17442903043528));
#133410=CARTESIAN_POINT('Ctrl Pts',(17.0732670646434,14.3362645374928,5.1744159817198));
#133411=CARTESIAN_POINT('Ctrl Pts',(17.0758558186791,14.3494253021247,5.14758635162535));
#133412=CARTESIAN_POINT('Ctrl Pts',(17.0783733027148,14.364283662599,5.12151099280864));
#133413=CARTESIAN_POINT('Ctrl Pts',(17.0808604798743,14.3807146444064,5.09640568306478));
#133414=CARTESIAN_POINT('Ctrl Pts',(17.0811171368961,14.382410191843,5.09381501355526));
#133415=CARTESIAN_POINT('Ctrl Pts',(17.0813734711919,14.3841224438466,5.09123469264477));
#133416=CARTESIAN_POINT('Ctrl Pts',(17.0816295277741,14.3858512340337,5.08866496954552));
#133417=CARTESIAN_POINT('Ctrl Pts',(17.0843638090811,14.4043119924029,5.06122437116249));
#133418=CARTESIAN_POINT('Ctrl Pts',(17.0870672604627,14.4246635102563,5.03498955318868));
#133419=CARTESIAN_POINT('Ctrl Pts',(17.0897868570603,14.4466989954632,5.01021248193811));
#133420=CARTESIAN_POINT('Ctrl Pts',(17.0925036504131,14.4687117674274,4.98546094984072));
#133421=CARTESIAN_POINT('Ctrl Pts',(17.0952370362601,14.4924045217501,4.96216391911936));
#133422=CARTESIAN_POINT('Ctrl Pts',(17.0980162294418,14.517545283025,4.94053749879048));
#133423=CARTESIAN_POINT('Ctrl Pts',(17.1007940979461,14.5426740611825,4.91892138650011));
#133424=CARTESIAN_POINT('Ctrl Pts',(17.1036179549144,14.569249201768,4.89897411650705));
#133425=CARTESIAN_POINT('Ctrl Pts',(17.1064941737705,14.597018984189,4.88087962592021));
#133426=CARTESIAN_POINT('Ctrl Pts',(17.1093727444936,14.6248114737966,4.86277033957565));
#133427=CARTESIAN_POINT('Ctrl Pts',(17.1123038044352,14.6538004830513,4.84651679968675));
#133428=CARTESIAN_POINT('Ctrl Pts',(17.1152689227827,14.6837160968295,4.83227329132449));
#133429=CARTESIAN_POINT('Ctrl Pts',(17.1182354603923,14.7136460297993,4.81802296526741));
#133430=CARTESIAN_POINT('Ctrl Pts',(17.1212359261201,14.7445035682296,4.80578469411534));
#133431=CARTESIAN_POINT('Ctrl Pts',(17.1242278802789,14.7760005656261,4.79568270736877));
#133432=CARTESIAN_POINT('Ctrl Pts',(17.1272256364889,14.8075586425646,4.78556113066843));
#133433=CARTESIAN_POINT('Ctrl Pts',(17.1302143755419,14.8397589414177,4.77758456517678));
#133434=CARTESIAN_POINT('Ctrl Pts',(17.1331319537673,14.8722906572434,4.77184378085331));
#133435=CARTESIAN_POINT('Ctrl Pts',(17.1341646798948,14.8838058079304,4.76981173320786));
#133436=CARTESIAN_POINT('Ctrl Pts',(17.135188350111,14.8953622699967,4.76805946559736));
#133437=CARTESIAN_POINT('Ctrl Pts',(17.1361998550209,14.9069455296076,4.76658975811008));
#133438=CARTESIAN_POINT('Ctrl Pts',(17.1362011141082,14.9069599480604,4.76658792866753));
#133439=CARTESIAN_POINT('Ctrl Pts',(17.1362023731787,14.906974366584,4.76658609965795));
#133440=CARTESIAN_POINT('Ctrl Pts',(17.1362036322324,14.9069887851785,4.76658427108136));
#133441=CARTESIAN_POINT('Ctrl Pts',(17.1387923860856,14.9366350139168,4.76282451490147));
#133442=CARTESIAN_POINT('Ctrl Pts',(17.1413098699205,14.9665846622022,4.7608974322932));
#133443=CARTESIAN_POINT('Ctrl Pts',(17.143797046848,14.996588781652,4.76081728363642));
#133444=CARTESIAN_POINT('Ctrl Pts',(17.1440537041177,14.9996849728769,4.76080901291985));
#133445=CARTESIAN_POINT('Ctrl Pts',(17.1443100386603,15.0027817054289,4.7608203851297));
#133446=CARTESIAN_POINT('Ctrl Pts',(17.1445660954884,15.005878679663,4.760851398323));
#133447=CARTESIAN_POINT('Ctrl Pts',(17.1473003767961,15.038949458605,4.76118257009975));
#133448=CARTESIAN_POINT('Ctrl Pts',(17.1500038281384,15.0720527417223,4.76375602239136));
#133449=CARTESIAN_POINT('Ctrl Pts',(17.152723424668,15.1048643658765,4.76853757504343));
#133450=CARTESIAN_POINT('Ctrl Pts',(17.1554402179507,15.1376421691747,4.77331419907012));
#133451=CARTESIAN_POINT('Ctrl Pts',(17.1581736036993,15.1701288330478,4.78029381047501));
#133452=CARTESIAN_POINT('Ctrl Pts',(17.1609527967733,15.2020162973659,4.78940147819089));
#133453=CARTESIAN_POINT('Ctrl Pts',(17.1637306651674,15.2338885627823,4.7985048048107));
#133454=CARTESIAN_POINT('Ctrl Pts',(17.1665545220162,15.2651622012134,4.80973384193559));
#133455=CARTESIAN_POINT('Ctrl Pts',(17.1694307407666,15.2955451674421,4.8229794762384));
#133456=CARTESIAN_POINT('Ctrl Pts',(17.1723093113792,15.3259529775915,4.83623594139577));
#133457=CARTESIAN_POINT('Ctrl Pts',(17.1752403712242,15.3554686698087,4.85151220363314));
#133458=CARTESIAN_POINT('Ctrl Pts',(17.1782054895142,15.3838149616789,4.8686676481297));
#133459=CARTESIAN_POINT('Ctrl Pts',(17.1811720270636,15.4121748215541,4.88583130411152));
#133460=CARTESIAN_POINT('Ctrl Pts',(17.1841724927706,15.4393641414083,4.904876090957));
#133461=CARTESIAN_POINT('Ctrl Pts',(17.1871644469736,15.4651207184266,4.92562963969941));
#133462=CARTESIAN_POINT('Ctrl Pts',(17.1901622032226,15.4909272430153,4.94642343405885));
#133463=CARTESIAN_POINT('Ctrl Pts',(17.1931509423804,15.5152952548463,4.96893309656858));
#133464=CARTESIAN_POINT('Ctrl Pts',(17.196068520799,15.5379780396529,4.9929489346695));
#133465=CARTESIAN_POINT('Ctrl Pts',(17.1971012463288,15.5460069895539,5.00144974101178));
#133466=CARTESIAN_POINT('Ctrl Pts',(17.19812491597,15.5538249659581,5.01013889140464));
#133467=CARTESIAN_POINT('Ctrl Pts',(17.1991364203344,15.5614216662791,5.01900579169129));
#133468=CARTESIAN_POINT('Ctrl Pts',(17.1991376794173,15.5614311223686,5.01901682887835));
#133469=CARTESIAN_POINT('Ctrl Pts',(17.1991389384834,15.5614405781354,5.01902786636269));
#133470=CARTESIAN_POINT('Ctrl Pts',(17.1991401975326,15.5614500335796,5.01903890414432));
#133471=CARTESIAN_POINT('Ctrl Pts',(17.2017289524822,15.5808915513842,5.04173389603124));
#133472=CARTESIAN_POINT('Ctrl Pts',(17.2042464374443,15.5989691462508,5.0656900281609));
#133473=CARTESIAN_POINT('Ctrl Pts',(17.2067336155454,15.6155340213903,5.09070720489167));
#133474=CARTESIAN_POINT('Ctrl Pts',(17.2069902725584,15.617243384854,5.09328877870422));
#133475=CARTESIAN_POINT('Ctrl Pts',(17.2072466068458,15.6189366390559,5.09588160540596));
#133476=CARTESIAN_POINT('Ctrl Pts',(17.2075026634199,15.6206136208584,5.09848543364811));
#133477=CARTESIAN_POINT('Ctrl Pts',(17.2102369456637,15.638521153918,5.12629023168492));
#133478=CARTESIAN_POINT('Ctrl Pts',(17.2129403980013,15.6545736717429,5.15535510938026));
#133479=CARTESIAN_POINT('Ctrl Pts',(17.2156599955616,15.6686214807986,5.18539051200979));
#133480=CARTESIAN_POINT('Ctrl Pts',(17.2183767898766,15.6826548099718,5.21539495542685));
#133481=CARTESIAN_POINT('Ctrl Pts',(17.2211101766924,15.6946879867136,5.24636754632892));
#133482=CARTESIAN_POINT('Ctrl Pts',(17.2238893708266,15.7046142094085,5.27800977309107));
#133483=CARTESIAN_POINT('Ctrl Pts',(17.2266672402813,15.7145357008532,5.30963691785302));
#133484=CARTESIAN_POINT('Ctrl Pts',(17.2294910981837,15.7223525124384,5.34193288686681));
#133485=CARTESIAN_POINT('Ctrl Pts',(17.2323673179249,15.7279951994938,5.37459374982264));
#133486=CARTESIAN_POINT('Ctrl Pts',(17.2352458895242,15.7336425005215,5.40728131926023));
#133487=CARTESIAN_POINT('Ctrl Pts',(17.2381769502925,15.7371122093331,5.44033433456266));
#133488=CARTESIAN_POINT('Ctrl Pts',(17.2411420693788,15.7383693105905,5.47344387492055));
#133489=CARTESIAN_POINT('Ctrl Pts',(17.2441086077226,15.7396270135607,5.50656926319572));
#133490=CARTESIAN_POINT('Ctrl Pts',(17.2471090740959,15.7386698547313,5.53975129605358));
#133491=CARTESIAN_POINT('Ctrl Pts',(17.2501010287738,15.7354976333302,5.57267618785584));
#133492=CARTESIAN_POINT('Ctrl Pts',(17.2530987854865,15.7323192603188,5.6056649280081));
#133493=CARTESIAN_POINT('Ctrl Pts',(17.2560875249143,15.726916716557,5.63839561513311));
#133494=CARTESIAN_POINT('Ctrl Pts',(17.2590051033636,15.7193294926593,5.6705468779432));
#133495=CARTESIAN_POINT('Ctrl Pts',(17.2600378244874,15.7166438797354,5.6819273048409));
#133496=CARTESIAN_POINT('Ctrl Pts',(17.2610614897705,15.7136849478903,5.69323507658317));
#133497=CARTESIAN_POINT('Ctrl Pts',(17.2620729898636,15.7104558810248,5.70445576275555));
#133498=CARTESIAN_POINT('Ctrl Pts',(17.262074248952,15.7104518615684,5.70446972996684));
#133499=CARTESIAN_POINT('Ctrl Pts',(17.2620755080235,15.7104478416862,5.7044836970721));
#133500=CARTESIAN_POINT('Ctrl Pts',(17.2620767670781,15.7104438213783,5.70449766407129));
#133501=CARTESIAN_POINT('Ctrl Pts',(17.2646655203705,15.7021776311295,5.73321533333194));
#133502=CARTESIAN_POINT('Ctrl Pts',(17.267183003679,15.6921081022342,5.76148721799749));
#133503=CARTESIAN_POINT('Ctrl Pts',(17.2696701801455,15.6803205496886,5.78907901055691));
#133504=CARTESIAN_POINT('Ctrl Pts',(17.269926836768,15.6791041689991,5.79192626180144));
#133505=CARTESIAN_POINT('Ctrl Pts',(17.2701831706658,15.6778695315053,5.79476624510982));
#133506=CARTESIAN_POINT('Ctrl Pts',(17.2704392268509,15.6766167574458,5.79759868601503));
#133507=CARTESIAN_POINT('Ctrl Pts',(17.2731735070861,15.6632390866486,5.82784473213549));
#133508=CARTESIAN_POINT('Ctrl Pts',(17.2758769574401,15.6477889337777,5.85723422131644));
#133509=CARTESIAN_POINT('Ctrl Pts',(17.2785965530498,15.6304258422559,5.88548290756499));
#133510=CARTESIAN_POINT('Ctrl Pts',(17.2813133454188,15.613080647852,5.91370247629913));
#133511=CARTESIAN_POINT('Ctrl Pts',(17.2840467303213,15.5938270059046,5.94078374056712));
#133512=CARTESIAN_POINT('Ctrl Pts',(17.2868259225927,15.5728555255426,5.96647335525849));
#133513=CARTESIAN_POINT('Ctrl Pts',(17.289603790193,15.5518940410031,5.99215072528127));
#133514=CARTESIAN_POINT('Ctrl Pts',(17.2924276462916,15.5292166464172,6.01643789898743));
#133515=CARTESIAN_POINT('Ctrl Pts',(17.2953038643106,15.5050390178502,6.03910975453352));
#133516=CARTESIAN_POINT('Ctrl Pts',(17.2981824342153,15.4808416192177,6.06180014887329));
#133517=CARTESIAN_POINT('Ctrl Pts',(17.3011134933721,15.4551416188525,6.08287263208124));
#133518=CARTESIAN_POINT('Ctrl Pts',(17.3040786109701,15.4281777923325,6.10212809571443));
#133519=CARTESIAN_POINT('Ctrl Pts',(17.3070451478403,15.4012010594086,6.12139277609551));
#133520=CARTESIAN_POINT('Ctrl Pts',(17.3100456128648,15.3729591609748,6.13883861972739));
#133521=CARTESIAN_POINT('Ctrl Pts',(17.3130375663572,15.3437140789445,6.15429292244444));
#133522=CARTESIAN_POINT('Ctrl Pts',(17.3160353219279,15.314412284048,6.16977719456968));
#133523=CARTESIAN_POINT('Ctrl Pts',(17.3190240603795,15.2841030590818,6.18326181658168));
#133524=CARTESIAN_POINT('Ctrl Pts',(17.3219416380291,15.2530765464079,6.19460306592388));
#133525=CARTESIAN_POINT('Ctrl Pts',(17.3229743708641,15.2420941143211,6.19861751969088));
#133526=CARTESIAN_POINT('Ctrl Pts',(17.3239980476698,15.2310220802754,6.20236372539087));
#133527=CARTESIAN_POINT('Ctrl Pts',(17.325009558987,15.2198742485695,6.2058364075973));
#133528=CARTESIAN_POINT('Ctrl Pts',(17.3250108180805,15.219860372143,6.20584073026926));
#133529=CARTESIAN_POINT('Ctrl Pts',(17.3250120771571,15.219846495571,6.20584505252731));
#133530=CARTESIAN_POINT('Ctrl Pts',(17.3250133362169,15.2198326188534,6.20584937437144));
#133531=CARTESIAN_POINT('Ctrl Pts',(17.3276020888975,15.1913007013954,6.21473551761589));
#133532=CARTESIAN_POINT('Ctrl Pts',(17.3301195714695,15.1621495551006,6.22187028834272));
#133533=CARTESIAN_POINT('Ctrl Pts',(17.3326067469824,15.132621798228,6.22719611158677));
#133534=CARTESIAN_POINT('Ctrl Pts',(17.3328634054165,15.1295747483517,6.22774569783293));
#133535=CARTESIAN_POINT('Ctrl Pts',(17.3331197411185,15.126523730433,6.22827603831381));
#133536=CARTESIAN_POINT('Ctrl Pts',(17.3333757991017,15.1234690398434,6.22878708254196));
#133537=CARTESIAN_POINT('Ctrl Pts',(17.3361100800865,15.0908499342459,6.23424420009751));
#133538=CARTESIAN_POINT('Ctrl Pts',(17.3388135309118,15.0578067108807,6.23749927227484));
#133539=CARTESIAN_POINT('Ctrl Pts',(17.341533126788,15.0246645151019,6.23852926515128));
#133540=CARTESIAN_POINT('Ctrl Pts',(17.3442499194075,14.9915564810471,6.23955819634996));
#133541=CARTESIAN_POINT('Ctrl Pts',(17.3469833043578,14.9583498571705,6.23836717331611));
#133542=CARTESIAN_POINT('Ctrl Pts',(17.3497624965953,14.9253610601702,6.23497610112255));
#133543=CARTESIAN_POINT('Ctrl Pts',(17.352540364142,14.8923879871464,6.23158664526983));
#133544=CARTESIAN_POINT('Ctrl Pts',(17.3553642201057,14.8596325874684,6.22599955006262));
#133545=CARTESIAN_POINT('Ctrl Pts',(17.3582404380528,14.8274014872314,6.21827117671232));
#133546=CARTESIAN_POINT('Ctrl Pts',(17.3611190078425,14.7951440320821,6.21053648398104));
#133547=CARTESIAN_POINT('Ctrl Pts',(17.3640500669466,14.7634117402433,6.20065710972179));
#133548=CARTESIAN_POINT('Ctrl Pts',(17.3670151847103,14.732502211224,6.18872301285149));
#133549=CARTESIAN_POINT('Ctrl Pts',(17.3699817217219,14.7015778874172,6.17678320374838));
#133550=CARTESIAN_POINT('Ctrl Pts',(17.3729821871067,14.6714771077787,6.16278655417432));
#133551=CARTESIAN_POINT('Ctrl Pts',(17.3759741413366,14.6424881774962,6.14685692489324));
#133552=CARTESIAN_POINT('Ctrl Pts',(17.3789718975937,14.6134430315937,6.13089640471772));
#133553=CARTESIAN_POINT('Ctrl Pts',(17.3819606371119,14.5855141733538,6.11299489910472));
#133554=CARTESIAN_POINT('Ctrl Pts',(17.3848782163587,14.5589811849392,6.09331572577658));
#133555=CARTESIAN_POINT('Ctrl Pts',(17.3859109408273,14.5495894035875,6.08634996337569));
#133556=CARTESIAN_POINT('Ctrl Pts',(17.3869346094895,14.5403724080828,6.07916186612232));
#133557=CARTESIAN_POINT('Ctrl Pts',(17.3879461129728,14.5313421948412,6.07176006324632));
#133558=CARTESIAN_POINT('Ctrl Pts',(17.3879473720345,14.5313309545482,6.07175084990541));
#133559=CARTESIAN_POINT('Ctrl Pts',(17.3879486310795,14.5313197145191,6.07174163621408));
#133560=CARTESIAN_POINT('Ctrl Pts',(17.3879498901077,14.531308474754,6.0717324221723));
#133561=CARTESIAN_POINT('Ctrl Pts',(17.3905172407073,14.5083888796025,6.05294358580232));
#133562=CARTESIAN_POINT('Ctrl Pts',(17.3930150706138,14.4865659871349,6.03269332893148));
#133563=CARTESIAN_POINT('Ctrl Pts',(17.3954830725674,14.466021281195,6.01114853856156));
#133564=CARTESIAN_POINT('Ctrl Pts',(17.3957679506134,14.4636498342539,6.00866165326039));
#133565=CARTESIAN_POINT('Ctrl Pts',(17.3960524312387,14.4612954273727,6.00615757615927));
#133566=CARTESIAN_POINT('Ctrl Pts',(17.3963365754886,14.4589583459032,6.00363660801193));
#133567=CARTESIAN_POINT('Ctrl Pts',(17.3990370942771,14.4367466262545,5.97967722171588));
#133568=CARTESIAN_POINT('Ctrl Pts',(17.4017080289432,14.4160984659131,5.95418669569636));
#133569=CARTESIAN_POINT('Ctrl Pts',(17.4043944413958,14.3972091715163,5.92741709576108));
#133570=CARTESIAN_POINT('Ctrl Pts',(17.4071502058762,14.3778322338807,5.89995641578101));
#133571=CARTESIAN_POINT('Ctrl Pts',(17.4099228436392,14.3603060093141,5.87115019365405));
#133572=CARTESIAN_POINT('Ctrl Pts',(17.4127425977568,14.3447974178845,5.84129019182417));
#133573=CARTESIAN_POINT('Ctrl Pts',(17.4155623518744,14.329288826455,5.81143018999427));
#133574=CARTESIAN_POINT('Ctrl Pts',(17.4184294660874,14.3157976460623,5.78051669501691));
#133575=CARTESIAN_POINT('Ctrl Pts',(17.4213499029956,14.304450533742,5.74885545845108));
#133576=CARTESIAN_POINT('Origin',(13.2437274406976,15.,5.5));
#133577=CARTESIAN_POINT('',(17.9010383741602,14.3042076641721,5.74898599439144));
#133578=CARTESIAN_POINT('',(17.8222024383386,14.3040135853341,5.74909189204507));
#133579=CARTESIAN_POINT('',(13.2437274406976,14.3042076641721,5.74898599439144));
#133580=CARTESIAN_POINT('Ctrl Pts',(17.9010383741602,14.3042076641721,5.74898599439144));
#133581=CARTESIAN_POINT('Ctrl Pts',(17.9000384603042,14.3078805994981,5.75925002653544));
#133582=CARTESIAN_POINT('Ctrl Pts',(17.8990357742742,14.3117816194058,5.76943549672321));
#133583=CARTESIAN_POINT('Ctrl Pts',(17.894600037722,14.3300218189885,5.81407382881705));
#133584=CARTESIAN_POINT('Ctrl Pts',(17.8911650746411,14.3467321536784,5.84749794462777));
#133585=CARTESIAN_POINT('Ctrl Pts',(17.8870512634926,14.3703816273505,5.88701155111811));
#133586=CARTESIAN_POINT('Ctrl Pts',(17.8862772581325,14.3749984053375,5.89442396414004));
#133587=CARTESIAN_POINT('Ctrl Pts',(17.88505488578,14.3825700483691,5.90611358429325));
#133588=CARTESIAN_POINT('Ctrl Pts',(17.8846016477165,14.3854403739368,5.91044422397341));
#133589=CARTESIAN_POINT('Ctrl Pts',(17.8836930093189,14.3913257897608,5.91912373034288));
#133590=CARTESIAN_POINT('Ctrl Pts',(17.8832377222116,14.3943423619815,5.9234711637284));
#133591=CARTESIAN_POINT('Ctrl Pts',(17.8820084580608,14.402664405411,5.93519388745609));
#133592=CARTESIAN_POINT('Ctrl Pts',(17.8812400921136,14.408059819301,5.94250466435763));
#133593=CARTESIAN_POINT('Ctrl Pts',(17.8771815965658,14.4375218777562,5.98092208253775));
#133594=CARTESIAN_POINT('Ctrl Pts',(17.8740151442579,14.4639112807589,6.01017395289943));
#133595=CARTESIAN_POINT('Ctrl Pts',(17.8682413450271,14.5160426850946,6.0594234311034));
#133596=CARTESIAN_POINT('Ctrl Pts',(17.865640759731,14.5410121975035,6.08008557158004));
#133597=CARTESIAN_POINT('Ctrl Pts',(17.8617627384983,14.5794450817572,6.1078492467406));
#133598=CARTESIAN_POINT('Ctrl Pts',(17.860523755482,14.5919003971697,6.1162806240157));
#133599=CARTESIAN_POINT('Ctrl Pts',(17.8582050200211,14.6154368489631,6.13118667298788));
#133600=CARTESIAN_POINT('Ctrl Pts',(17.8571291043679,14.6264462082628,6.13776402984319));
#133601=CARTESIAN_POINT('Ctrl Pts',(17.855290973987,14.645359064967,6.14840546913147));
#133602=CARTESIAN_POINT('Ctrl Pts',(17.8545341858223,14.6531751626598,6.15261961573129));
#133603=CARTESIAN_POINT('Ctrl Pts',(17.8530757964975,14.6682804200302,6.16041581773013));
#133604=CARTESIAN_POINT('Ctrl Pts',(17.8523751104655,14.6755564652651,6.16402056696697));
#133605=CARTESIAN_POINT('Ctrl Pts',(17.8504863735569,14.6952087361591,6.17335672703167));
#133606=CARTESIAN_POINT('Ctrl Pts',(17.849291109414,14.7076860520455,6.17886633339106));
#133607=CARTESIAN_POINT('Ctrl Pts',(17.843979450735,14.7632628714261,6.20159116583678));
#133608=CARTESIAN_POINT('Ctrl Pts',(17.8397485794156,14.8077692527472,6.21506676510296));
#133609=CARTESIAN_POINT('Ctrl Pts',(17.8329486414327,14.8803065654519,6.22976528263476));
#133610=CARTESIAN_POINT('Ctrl Pts',(17.830407290844,14.9076642256996,6.23372892075528));
#133611=CARTESIAN_POINT('Ctrl Pts',(17.8268887289436,14.9463004534994,6.23713090235582));
#133612=CARTESIAN_POINT('Ctrl Pts',(17.8258824031434,14.9574417272552,6.23785800358135));
#133613=CARTESIAN_POINT('Ctrl Pts',(17.8241045149926,14.9773347265326,6.23870412961868));
#133614=CARTESIAN_POINT('Ctrl Pts',(17.8233294329946,14.986080095653,6.2389206742171));
#133615=CARTESIAN_POINT('Ctrl Pts',(17.8221026698386,15.0000612901527,6.23901852936151));
#133616=CARTESIAN_POINT('Ctrl Pts',(17.8216461887232,15.0052952749617,6.23899956451928));
#133617=CARTESIAN_POINT('Ctrl Pts',(17.8207314458554,15.0158540218926,6.2388491136678));
#133618=CARTESIAN_POINT('Ctrl Pts',(17.8202733090936,15.0211784369813,6.23871567069239));
#133619=CARTESIAN_POINT('Ctrl Pts',(17.8190279724218,15.0357376744717,6.23819322733457));
#133620=CARTESIAN_POINT('Ctrl Pts',(17.8182466222171,15.044967776164,6.23768851536866));
#133621=CARTESIAN_POINT('Ctrl Pts',(17.8145572389187,15.0888834387855,6.23445974063924));
#133622=CARTESIAN_POINT('Ctrl Pts',(17.8117434313418,15.1233616936699,6.22946139450966));
#133623=CARTESIAN_POINT('Ctrl Pts',(17.8061125579971,15.1916311761641,6.21458277587953));
#133624=CARTESIAN_POINT('Ctrl Pts',(17.8033022874982,15.2253221172352,6.204684912613));
#133625=CARTESIAN_POINT('Ctrl Pts',(17.7995643188042,15.2682001810777,6.18869730783189));
#133626=CARTESIAN_POINT('Ctrl Pts',(17.7986865934601,15.2781357857205,6.18474505181408));
#133627=CARTESIAN_POINT('Ctrl Pts',(17.7965061778855,15.3024357126063,6.17446272120241));
#133628=CARTESIAN_POINT('Ctrl Pts',(17.7951973605519,15.3166900371444,6.16788821900382));
#133629=CARTESIAN_POINT('Ctrl Pts',(17.7930819921121,15.3391145368598,6.15666610818905));
#133630=CARTESIAN_POINT('Ctrl Pts',(17.7922852957676,15.3474245970957,6.15230758016244));
#133631=CARTESIAN_POINT('Ctrl Pts',(17.7907335736692,15.3633330250821,6.14357358052954));
#133632=CARTESIAN_POINT('Ctrl Pts',(17.7899793786343,15.3709409727368,6.13921875835267));
#133633=CARTESIAN_POINT('Ctrl Pts',(17.7881648719207,15.388937575467,6.12848795379586));
#133634=CARTESIAN_POINT('Ctrl Pts',(17.7871002931057,15.3992490987736,6.12198847590305));
#133635=CARTESIAN_POINT('Ctrl Pts',(17.78076740689,15.4590942968259,6.08216596608944));
#133636=CARTESIAN_POINT('Ctrl Pts',(17.7752878249124,15.5045937966032,6.04320053010109));
#133637=CARTESIAN_POINT('Ctrl Pts',(17.7671456565326,15.5644643549734,5.97784891596493));
#133638=CARTESIAN_POINT('Ctrl Pts',(17.7644964291953,15.5827562249121,5.95536263593209));
#133639=CARTESIAN_POINT('Ctrl Pts',(17.7611176699925,15.6048558590097,5.92467488315749));
#133640=CARTESIAN_POINT('Ctrl Pts',(17.7603328184777,15.6098999625671,5.91739839937542));
#133641=CARTESIAN_POINT('Ctrl Pts',(17.7590955700563,15.6177209700958,5.90567139697697));
#133642=CARTESIAN_POINT('Ctrl Pts',(17.7586381896056,15.6205831801299,5.90127920620893));
#133643=CARTESIAN_POINT('Ctrl Pts',(17.7577265276395,15.6262330406788,5.89240417700884));
#133644=CARTESIAN_POINT('Ctrl Pts',(17.7572723100364,15.6290198849706,5.88792118929938));
#133645=CARTESIAN_POINT('Ctrl Pts',(17.7560478520044,15.6364487983189,5.87568025118322));
#133646=CARTESIAN_POINT('Ctrl Pts',(17.7552831649684,15.6409971341373,5.86786603678916));
#133647=CARTESIAN_POINT('Ctrl Pts',(17.7512837644971,15.6642332271655,5.82620530852942));
#133648=CARTESIAN_POINT('Ctrl Pts',(17.748168794692,15.6803893692854,5.79101004835711));
#133649=CARTESIAN_POINT('Ctrl Pts',(17.7424137329593,15.7050261840549,5.72390949017262));
#133650=CARTESIAN_POINT('Ctrl Pts',(17.7397798216937,15.7142699582852,5.69239444765107));
#133651=CARTESIAN_POINT('Ctrl Pts',(17.7358606719001,15.7246712388821,5.64560680992097));
#133652=CARTESIAN_POINT('Ctrl Pts',(17.734614964762,15.7274991761849,5.63074648288295));
#133653=CARTESIAN_POINT('Ctrl Pts',(17.7322860581138,15.7318853442907,5.60310371277995));
#133654=CARTESIAN_POINT('Ctrl Pts',(17.7312067842912,15.7335692872186,5.59034706958058));
#133655=CARTESIAN_POINT('Ctrl Pts',(17.7293665494819,15.7358496682767,5.56873758539821));
#133656=CARTESIAN_POINT('Ctrl Pts',(17.7286111087456,15.7366212500323,5.55990583796171));
#133657=CARTESIAN_POINT('Ctrl Pts',(17.7271578981829,15.7377918055203,5.54300559131467));
#133658=CARTESIAN_POINT('Ctrl Pts',(17.7264610725707,15.7382177191518,5.53494019173273));
#133659=CARTESIAN_POINT('Ctrl Pts',(17.7245899423742,15.7390015656981,5.51339629710099));
#133660=CARTESIAN_POINT('Ctrl Pts',(17.7234086093312,15.7391229365185,5.49991295132311));
#133661=CARTESIAN_POINT('Ctrl Pts',(17.719128989283,15.7382346614887,5.45153012444489));
#133662=CARTESIAN_POINT('Ctrl Pts',(17.7159712737335,15.7351214353682,5.41672030624534));
#133663=CARTESIAN_POINT('Ctrl Pts',(17.7099731759565,15.7246829704905,5.352036499593));
#133664=CARTESIAN_POINT('Ctrl Pts',(17.7071476266353,15.7179306639605,5.32214010715026));
#133665=CARTESIAN_POINT('Ctrl Pts',(17.7028842479441,15.7048621289642,5.27741135825029));
#133666=CARTESIAN_POINT('Ctrl Pts',(17.7014302638556,15.699884297055,5.26222202625305));
#133667=CARTESIAN_POINT('Ctrl Pts',(17.6989806038956,15.6905675821346,5.23662938264491));
#133668=CARTESIAN_POINT('Ctrl Pts',(17.6979768736244,15.6864762076922,5.22614214523881));
#133669=CARTESIAN_POINT('Ctrl Pts',(17.6964804699617,15.6799439712499,5.21046591513333));
#133670=CARTESIAN_POINT('Ctrl Pts',(17.6959790340752,15.6776799417493,5.205205675752));
#133671=CARTESIAN_POINT('Ctrl Pts',(17.6950479604336,15.6733316556893,5.19541780124666));
#133672=CARTESIAN_POINT('Ctrl Pts',(17.6946175951702,15.6712625050802,5.19088434848346));
#133673=CARTESIAN_POINT('Ctrl Pts',(17.6935517128162,15.665992422427,5.17964026349543));
#133674=CARTESIAN_POINT('Ctrl Pts',(17.6929194274527,15.6627357863013,5.17295633534131));
#133675=CARTESIAN_POINT('Ctrl Pts',(17.6902579158978,15.6484945915148,5.14481439098841));
#133676=CARTESIAN_POINT('Ctrl Pts',(17.6882765813078,15.6365632969928,5.12384907552866));
#133677=CARTESIAN_POINT('Ctrl Pts',(17.6826442071829,15.5993934126117,5.06538687230828));
#133678=CARTESIAN_POINT('Ctrl Pts',(17.6790535765827,15.5717167211382,5.02957341986894));
#133679=CARTESIAN_POINT('Ctrl Pts',(17.6739532852413,15.5290121786705,4.98369217558182));
#133680=CARTESIAN_POINT('Ctrl Pts',(17.6725181465541,15.5166302967901,4.97130281259466));
#133681=CARTESIAN_POINT('Ctrl Pts',(17.6698810594746,15.4933583087574,4.94961549065774));
#133682=CARTESIAN_POINT('Ctrl Pts',(17.6686851847012,15.4826157001997,4.94017184727217));
#133683=CARTESIAN_POINT('Ctrl Pts',(17.6667055549473,15.4645800091548,4.92522203335335));
#133684=CARTESIAN_POINT('Ctrl Pts',(17.6659294088749,15.4574464802409,4.91952864165879));
#133685=CARTESIAN_POINT('Ctrl Pts',(17.6643938356443,15.4432246853306,4.90860295602732));
#133686=CARTESIAN_POINT('Ctrl Pts',(17.6636348941104,15.4361446565706,4.90336241383473));
#133687=CARTESIAN_POINT('Ctrl Pts',(17.6617430796023,15.4183822588667,4.89070003330132));
#133688=CARTESIAN_POINT('Ctrl Pts',(17.6606047350061,15.4075948418936,4.88343162418332));
#133689=CARTESIAN_POINT('Ctrl Pts',(17.6547182680103,15.3513552918553,4.84765916410755));
#133690=CARTESIAN_POINT('Ctrl Pts',(17.6498075183872,15.3030963671255,4.82388650524745));
#133691=CARTESIAN_POINT('Ctrl Pts',(17.6419098790068,15.2223576673412,4.79450671670751));
#133692=CARTESIAN_POINT('Ctrl Pts',(17.6389472842578,15.1913190883785,4.78546439627623));
#133693=CARTESIAN_POINT('Ctrl Pts',(17.6352322293206,15.1507672843944,4.77648390056853));
#133694=CARTESIAN_POINT('Ctrl Pts',(17.6344124872322,15.1417115889341,4.7746558266021));
#133695=CARTESIAN_POINT('Ctrl Pts',(17.6331335878699,15.1273873595482,4.77204272868788));
#133696=CARTESIAN_POINT('Ctrl Pts',(17.6326689031502,15.1221409192571,4.77114409544008));
#133697=CARTESIAN_POINT('Ctrl Pts',(17.6317555355925,15.1117391030106,4.76947790431085));
#133698=CARTESIAN_POINT('Ctrl Pts',(17.6313067728169,15.1065844509896,4.76870804829337));
#133699=CARTESIAN_POINT('Ctrl Pts',(17.6301167437775,15.0928095386986,4.7667994914346));
#133700=CARTESIAN_POINT('Ctrl Pts',(17.6293804925715,15.0841762227602,4.76575822754224));
#133701=CARTESIAN_POINT('Ctrl Pts',(17.6250160098549,15.0324584782375,4.76044484134559));
#133702=CARTESIAN_POINT('Ctrl Pts',(17.62154249778,14.9890786829572,4.75981269019647));
#133703=CARTESIAN_POINT('Ctrl Pts',(17.6145033534909,14.9018684671185,4.76621574794428));
#133704=CARTESIAN_POINT('Ctrl Pts',(17.6109495026657,14.8582329838677,4.77338420293328));
#133705=CARTESIAN_POINT('Ctrl Pts',(17.6062122060801,14.8031189195521,4.78759397256809));
#133706=CARTESIAN_POINT('Ctrl Pts',(17.6051392942247,14.7908225715475,4.79110701001482));
#133707=CARTESIAN_POINT('Ctrl Pts',(17.603306043425,14.770173349812,4.79759045462644));
#133708=CARTESIAN_POINT('Ctrl Pts',(17.6025511050842,14.761771231832,4.80039547021402));
#133709=CARTESIAN_POINT('Ctrl Pts',(17.601096260436,14.7457859469826,4.80605343979563));
#133710=CARTESIAN_POINT('Ctrl Pts',(17.60039726597,14.7381952558168,4.80888143007729));
#133711=CARTESIAN_POINT('Ctrl Pts',(17.59851355857,14.7179887948858,4.81679020149647));
#133712=CARTESIAN_POINT('Ctrl Pts',(17.5973216553542,14.7054648931511,4.8220951644158));
#133713=CARTESIAN_POINT('Ctrl Pts',(17.5919065423122,14.649781713568,4.8475161089425));
#133714=CARTESIAN_POINT('Ctrl Pts',(17.5875613246051,14.6084883446173,4.87142614538585));
#133715=CARTESIAN_POINT('Ctrl Pts',(17.5806957622174,14.5477641622675,4.91490387860572));
#133716=CARTESIAN_POINT('Ctrl Pts',(17.5782033041361,14.5266226302212,4.93187261042478));
#133717=CARTESIAN_POINT('Ctrl Pts',(17.5747437895731,14.4982395749508,4.95734039382775));
#133718=CARTESIAN_POINT('Ctrl Pts',(17.5737481911643,14.4901853216079,4.96490001219207));
#133719=CARTESIAN_POINT('Ctrl Pts',(17.5719874088784,14.4761129942051,4.97871442797565));
#133720=CARTESIAN_POINT('Ctrl Pts',(17.5712187713798,14.4700299598114,4.98489999090565));
#133721=CARTESIAN_POINT('Ctrl Pts',(17.5700007470199,14.4604721029733,4.99496756896773));
#133722=CARTESIAN_POINT('Ctrl Pts',(17.5695466269355,14.4569271547867,4.99878148582861));
#133723=CARTESIAN_POINT('Ctrl Pts',(17.5686921882016,14.4502886329577,5.00607683150433));
#133724=CARTESIAN_POINT('Ctrl Pts',(17.5682912631719,14.447187136588,5.00955058852532));
#133725=CARTESIAN_POINT('Ctrl Pts',(17.5671681689619,14.4385435135944,5.01941785416487));
#133726=CARTESIAN_POINT('Ctrl Pts',(17.5664511832961,14.4330778083794,5.02587782916741));
#133727=CARTESIAN_POINT('Ctrl Pts',(17.5612718209102,14.3940763707777,5.0736131911522));
#133728=CARTESIAN_POINT('Ctrl Pts',(17.5570484972381,14.3649670176315,5.11831413405712));
#133729=CARTESIAN_POINT('Ctrl Pts',(17.550404627432,14.3277103715715,5.1917810746355));
#133730=CARTESIAN_POINT('Ctrl Pts',(17.5480389773663,14.3160681034596,5.21855879345734));
#133731=CARTESIAN_POINT('Ctrl Pts',(17.5443432185663,14.3006976901226,5.26054488911534));
#133732=CARTESIAN_POINT('Ctrl Pts',(17.543047047265,14.2958176965653,5.27530089849097));
#133733=CARTESIAN_POINT('Ctrl Pts',(17.5409471662091,14.2887517903108,5.29916564517675));
#133734=CARTESIAN_POINT('Ctrl Pts',(17.5401530592254,14.2862674392464,5.30818167766472));
#133735=CARTESIAN_POINT('Ctrl Pts',(17.5386032568386,14.2817852988349,5.32574268440951));
#133736=CARTESIAN_POINT('Ctrl Pts',(17.5378483472904,14.2797673018426,5.33428091515895));
#133737=CARTESIAN_POINT('Ctrl Pts',(17.5360267496239,14.2752947951494,5.35483225656747));
#133738=CARTESIAN_POINT('Ctrl Pts',(17.5349556938405,14.2729864167714,5.36687405158692));
#133739=CARTESIAN_POINT('Ctrl Pts',(17.5286685695326,14.2613008568798,5.43725994863433));
#133740=CARTESIAN_POINT('Ctrl Pts',(17.5232463597049,14.2586515972324,5.49649196972236));
#133741=CARTESIAN_POINT('Ctrl Pts',(17.5151346763136,14.2652698972504,5.58454088115257));
#133742=CARTESIAN_POINT('Ctrl Pts',(17.5124599248356,14.2691887837803,5.613537699438));
#133743=CARTESIAN_POINT('Ctrl Pts',(17.5090536742073,14.2765258409504,5.65094726546426));
#133744=CARTESIAN_POINT('Ctrl Pts',(17.5082659322136,14.2783929847485,5.65963481161436));
#133745=CARTESIAN_POINT('Ctrl Pts',(17.5070252356715,14.2816117531252,5.67339802907555));
#133746=CARTESIAN_POINT('Ctrl Pts',(17.5065672542576,14.2828614985113,5.67849628847932));
#133747=CARTESIAN_POINT('Ctrl Pts',(17.5057115869217,14.2853144601774,5.68806108013354));
#133748=CARTESIAN_POINT('Ctrl Pts',(17.505313223435,14.2865054772999,5.69253041433309));
#133749=CARTESIAN_POINT('Ctrl Pts',(17.5042079666093,14.2899452142966,5.70496765274709));
#133750=CARTESIAN_POINT('Ctrl Pts',(17.5035059867801,14.2922860716379,5.71290972519018));
#133751=CARTESIAN_POINT('Ctrl Pts',(17.5019765370958,14.29772112311,5.73026850801131));
#133752=CARTESIAN_POINT('Ctrl Pts',(17.5011520742185,14.3008710928694,5.73966193347026));
#133753=CARTESIAN_POINT('Ctrl Pts',(17.5003341513661,14.3042076696198,5.74898600961524));
#133754=CARTESIAN_POINT('',(17.4440936240989,14.2607889278854,5.49961548488437));
#133755=CARTESIAN_POINT('Ctrl Pts',(17.4211934345165,14.3041892428936,5.74893451005237));
#133756=CARTESIAN_POINT('Ctrl Pts',(17.4224519124576,14.2993228908923,5.73533229768884));
#133757=CARTESIAN_POINT('Ctrl Pts',(17.4237230400774,14.2948568242566,5.72159138443025));
#133758=CARTESIAN_POINT('Ctrl Pts',(17.4274963788901,14.2829172297248,5.6808287340023));
#133759=CARTESIAN_POINT('Ctrl Pts',(17.4300299028855,14.2765757763358,5.65350491668053));
#133760=CARTESIAN_POINT('Ctrl Pts',(17.4364551078773,14.2645924814883,5.58418881435459));
#133761=CARTESIAN_POINT('Ctrl Pts',(17.4403722648504,14.2609787020888,5.54194608807033));
#133762=CARTESIAN_POINT('Ctrl Pts',(17.4442144194927,14.2610000944162,5.49962643999587));
#133763=CARTESIAN_POINT('Ctrl Pts',(17.4440936240989,14.2607889278854,5.49961548488437));
#133764=CARTESIAN_POINT('Ctrl Pts',(17.4463925298371,14.2607552983813,5.47398865868977));
#133765=CARTESIAN_POINT('Ctrl Pts',(17.4486651958888,14.2620694570682,5.44839224160943));
#133766=CARTESIAN_POINT('Ctrl Pts',(17.4508827009377,14.2647377317864,5.42293429490633));
#133767=CARTESIAN_POINT('Ctrl Pts',(17.4508839600479,14.2647392468458,5.42291983976008));
#133768=CARTESIAN_POINT('Ctrl Pts',(17.4508852191412,14.2647407623429,5.42290538464378));
#133769=CARTESIAN_POINT('Ctrl Pts',(17.4508864782176,14.2647422782778,5.42289092955747));
#133770=CARTESIAN_POINT('Ctrl Pts',(17.4534752245319,14.2678591428434,5.39317029482624));
#133771=CARTESIAN_POINT('Ctrl Pts',(17.4559927009204,14.2728295072601,5.36357321786261));
#133772=CARTESIAN_POINT('Ctrl Pts',(17.4584798706255,14.2796103457723,5.33434531442345));
#133773=CARTESIAN_POINT('Ctrl Pts',(17.4587365249233,14.2803100693751,5.33132924880557));
#133774=CARTESIAN_POINT('Ctrl Pts',(17.458992856502,14.2810290391182,5.32831714642689));
#133775=CARTESIAN_POINT('Ctrl Pts',(17.4592489103732,14.2817671846145,5.32530929854553));
#133776=CARTESIAN_POINT('Ctrl Pts',(17.4619831816311,14.289649471282,5.29318999500387));
#133777=CARTESIAN_POINT('Ctrl Pts',(17.4646866232128,14.2997220837668,5.26155162396274));
#133778=CARTESIAN_POINT('Ctrl Pts',(17.4674062102649,14.311877644897,5.23070195007791));
#133779=CARTESIAN_POINT('Ctrl Pts',(17.4701229941021,14.3240206766796,5.19988407450164));
#133780=CARTESIAN_POINT('Ctrl Pts',(17.4728563706849,14.3382417983359,5.16985322151559));
#133781=CARTESIAN_POINT('Ctrl Pts',(17.4756355548843,14.3543976419034,5.14089216370232));
#133782=CARTESIAN_POINT('Ctrl Pts',(17.4784134144559,14.3705457851971,5.11194490944399));
#133783=CARTESIAN_POINT('Ctrl Pts',(17.4812372627742,14.3886264976727,5.08406635675437));
#133784=CARTESIAN_POINT('Ctrl Pts',(17.484113473344,14.4084667951577,5.05751587338498));
#133785=CARTESIAN_POINT('Ctrl Pts',(17.4869920359349,14.4283233170452,5.0309436783589));
#133786=CARTESIAN_POINT('Ctrl Pts',(17.4899230881165,14.4499422088045,5.00570169173601));
#133787=CARTESIAN_POINT('Ctrl Pts',(17.4928881991985,14.4731231936543,4.98202770814059));
#133788=CARTESIAN_POINT('Ctrl Pts',(17.4958547296242,14.4963152748123,4.95834239224758));
#133789=CARTESIAN_POINT('Ctrl Pts',(17.4988551886701,14.5210710856156,4.93622663440896));
#133790=CARTESIAN_POINT('Ctrl Pts',(17.5018471367613,14.5471628832735,4.9158962898947));
#133791=CARTESIAN_POINT('Ctrl Pts',(17.5048448871375,14.5733052807554,4.89552651874272));
#133792=CARTESIAN_POINT('Ctrl Pts',(17.5078336209821,14.6007892643748,4.87694940277729));
#133793=CARTESIAN_POINT('Ctrl Pts',(17.5107511946049,14.6293542969684,4.86035718671592));
#133794=CARTESIAN_POINT('Ctrl Pts',(17.5117839811728,14.6394659807813,4.85448373840042));
#133795=CARTESIAN_POINT('Ctrl Pts',(17.512807710816,14.6497128091566,4.84885876088503));
#133796=CARTESIAN_POINT('Ctrl Pts',(17.5138192735669,14.6600821110534,4.84348986345622));
#133797=CARTESIAN_POINT('Ctrl Pts',(17.5138205326936,14.6600950180781,4.84348318060596));
#133798=CARTESIAN_POINT('Ctrl Pts',(17.5138217918035,14.6601079253185,4.8434764981378));
#133799=CARTESIAN_POINT('Ctrl Pts',(17.5138230508965,14.6601208327746,4.84346981605176));
#133800=CARTESIAN_POINT('Ctrl Pts',(17.5164117982747,14.6866590966042,4.82973117061418));
#133801=CARTESIAN_POINT('Ctrl Pts',(17.5189292749153,14.714113311098,4.81760861770762));
#133802=CARTESIAN_POINT('Ctrl Pts',(17.5214164434176,14.7422546666011,4.8072012718735));
#133803=CARTESIAN_POINT('Ctrl Pts',(17.5216731105494,14.7451587565303,4.80612727001093));
#133804=CARTESIAN_POINT('Ctrl Pts',(17.5219294549139,14.7480701194309,4.80507152471403));
#133805=CARTESIAN_POINT('Ctrl Pts',(17.5221855215289,14.7509884732826,4.80403413735497));
#133806=CARTESIAN_POINT('Ctrl Pts',(17.5249198036721,14.7821506879431,4.79295690367745));
#133807=CARTESIAN_POINT('Ctrl Pts',(17.5276232542732,14.8141155650103,4.78397362308434));
#133808=CARTESIAN_POINT('Ctrl Pts',(17.5303428489279,14.8465669963551,4.77716383381978));
#133809=CARTESIAN_POINT('Ctrl Pts',(17.5330596402498,14.8789849770681,4.77036106402229));
#133810=CARTESIAN_POINT('Ctrl Pts',(17.5357930229162,14.9118882390937,4.76572680621878));
#133811=CARTESIAN_POINT('Ctrl Pts',(17.5385722125199,14.9449617596833,4.76329679466272));
#133812=CARTESIAN_POINT('Ctrl Pts',(17.5413500773439,14.9780195148378,4.76086794144083));
#133813=CARTESIAN_POINT('Ctrl Pts',(17.5441739302386,15.0112472583002,4.76064093479088));
#133814=CARTESIAN_POINT('Ctrl Pts',(17.5470501455451,15.0443332319865,4.76261390234366));
#133815=CARTESIAN_POINT('Ctrl Pts',(17.5499287125112,15.0774462575234,4.76458848303993));
#133816=CARTESIAN_POINT('Ctrl Pts',(17.5528597692182,15.1104172579024,4.76876653967552));
#133817=CARTESIAN_POINT('Ctrl Pts',(17.555824885858,15.1429374873463,4.77511154133677));
#133818=CARTESIAN_POINT('Ctrl Pts',(17.5587914216427,15.1754732814116,4.7814595798016));
#133819=CARTESIAN_POINT('Ctrl Pts',(17.5617918870776,15.2075579056174,4.78997678500314));
#133820=CARTESIAN_POINT('Ctrl Pts',(17.5647838434917,15.2388858369081,4.80059162129109));
#133821=CARTESIAN_POINT('Ctrl Pts',(17.5677816017304,15.270274517466,4.81122704124027));
#133822=CARTESIAN_POINT('Ctrl Pts',(17.5707703453829,15.3009035352746,4.82396875050107));
#133823=CARTESIAN_POINT('Ctrl Pts',(17.5736879316955,15.3304690561188,4.83870483921705));
#133824=CARTESIAN_POINT('Ctrl Pts',(17.5747206290912,15.3409339517916,4.84392076731959));
#133825=CARTESIAN_POINT('Ctrl Pts',(17.5757442715644,15.3512656426126,4.84938615583841));
#133826=CARTESIAN_POINT('Ctrl Pts',(17.5767557500387,15.3614508091328,4.85509460692846));
#133827=CARTESIAN_POINT('Ctrl Pts',(17.5767570089466,15.3614634858098,4.85510171178929));
#133828=CARTESIAN_POINT('Ctrl Pts',(17.5767582678376,15.3614761622863,4.85510881704021));
#133829=CARTESIAN_POINT('Ctrl Pts',(17.5767595267117,15.3614888385623,4.85511592268124));
#133830=CARTESIAN_POINT('Ctrl Pts',(17.5793483248545,15.3875568298914,4.86972824171119));
#133831=CARTESIAN_POINT('Ctrl Pts',(17.5818658542699,15.412778570209,4.88599428489849));
#133832=CARTESIAN_POINT('Ctrl Pts',(17.5843530787296,15.4369454539258,4.90377742783721));
#133833=CARTESIAN_POINT('Ctrl Pts',(17.5846097249538,15.4394391329468,4.90561239551419));
#133834=CARTESIAN_POINT('Ctrl Pts',(17.5848660485118,15.4419215639731,4.90746347358738));
#133835=CARTESIAN_POINT('Ctrl Pts',(17.5851220944084,15.4443925073284,4.90933048228485));
#133836=CARTESIAN_POINT('Ctrl Pts',(17.5878564130194,15.4707797546574,4.92926830083465));
#133837=CARTESIAN_POINT('Ctrl Pts',(17.5905599041572,15.4958593325918,4.95102793994418));
#133838=CARTESIAN_POINT('Ctrl Pts',(17.5932795419803,15.5193909909641,4.97438909846681));
#133839=CARTESIAN_POINT('Ctrl Pts',(17.5959963766293,15.5428983948807,4.99772617827074));
#133840=CARTESIAN_POINT('Ctrl Pts',(17.5987298052276,15.5648613381575,5.02266097655755));
#133841=CARTESIAN_POINT('Ctrl Pts',(17.6015090409049,15.585076754593,5.04895001344882));
#133842=CARTESIAN_POINT('Ctrl Pts',(17.6042869519286,15.6052825358525,5.07522652032378));
#133843=CARTESIAN_POINT('Ctrl Pts',(17.60711085115,15.6237426458637,5.10285572076104));
#133844=CARTESIAN_POINT('Ctrl Pts',(17.6099871097348,15.6402872241836,5.13157618360784));
#133845=CARTESIAN_POINT('Ctrl Pts',(17.6128657200272,15.6568453298027,5.16032012908953));
#133846=CARTESIAN_POINT('Ctrl Pts',(17.6157968169858,15.6714848383772,5.19015704918847));
#133847=CARTESIAN_POINT('Ctrl Pts',(17.6187619671962,15.6840664940894,5.22080897116232));
#133848=CARTESIAN_POINT('Ctrl Pts',(17.6217285365992,15.6966541716867,5.25147556388791));
#133849=CARTESIAN_POINT('Ctrl Pts',(17.6247290289276,15.7071819212573,5.28295804698363));
#133850=CARTESIAN_POINT('Ctrl Pts',(17.6277210019063,15.7155414967452,5.31496189073705));
#133851=CARTESIAN_POINT('Ctrl Pts',(17.6307187765062,15.7239172819685,5.34702779192869));
#133852=CARTESIAN_POINT('Ctrl Pts',(17.6337075260791,15.7301160283842,5.37961733394));
#133853=CARTESIAN_POINT('Ctrl Pts',(17.636625105088,15.7340641420407,5.41241519569096));
#133854=CARTESIAN_POINT('Ctrl Pts',(17.6376576570014,15.7354614074784,5.42402259168815));
#133855=CARTESIAN_POINT('Ctrl Pts',(17.6386811548528,15.7365771384209,5.43565588644526));
#133856=CARTESIAN_POINT('Ctrl Pts',(17.6396924907964,15.7374093556554,5.44730044262293));
#133857=CARTESIAN_POINT('Ctrl Pts',(17.6396937501104,15.737410391931,5.44731494240699));
#133858=CARTESIAN_POINT('Ctrl Pts',(17.6396950094076,15.7374114277703,5.4473294422381));
#133859=CARTESIAN_POINT('Ctrl Pts',(17.6396962686879,15.7374124631733,5.44734394211627));
#133860=CARTESIAN_POINT('Ctrl Pts',(17.6422849540133,15.7395409268393,5.47715114426387));
#133861=CARTESIAN_POINT('Ctrl Pts',(17.6448023693862,15.7398229088094,5.50716082859561));
#133862=CARTESIAN_POINT('Ctrl Pts',(17.6472894785076,15.7382578165603,5.53712364710993));
#133863=CARTESIAN_POINT('Ctrl Pts',(17.6475461208021,15.7380963162616,5.54021548028671));
#133864=CARTESIAN_POINT('Ctrl Pts',(17.6478024403967,15.7379151748501,5.54330677711932));
#133865=CARTESIAN_POINT('Ctrl Pts',(17.6480584823002,15.7377144106899,5.54639723855675));
#133866=CARTESIAN_POINT('Ctrl Pts',(17.6507926814368,15.7355705069541,5.57939940295987));
#133867=CARTESIAN_POINT('Ctrl Pts',(17.6534960514656,15.7311860084348,5.61231109590126));
#133868=CARTESIAN_POINT('Ctrl Pts',(17.6562155679204,15.7246128128331,5.64481052808752));
#133869=CARTESIAN_POINT('Ctrl Pts',(17.6589322813081,15.7180463923725,5.67727646237531));
#133870=CARTESIAN_POINT('Ctrl Pts',(17.6616655883834,15.7092963512731,5.70933093486746));
#133871=CARTESIAN_POINT('Ctrl Pts',(17.6644447048133,15.698454394239,5.74067046867308));
#133872=CARTESIAN_POINT('Ctrl Pts',(17.6672224968963,15.6876176037791,5.77199506808764));
#133873=CARTESIAN_POINT('Ctrl Pts',(17.6700462794709,15.6746912077568,5.80260542889568));
#133874=CARTESIAN_POINT('Ctrl Pts',(17.6729224273329,15.6598001639789,5.83221593928102));
#133875=CARTESIAN_POINT('Ctrl Pts',(17.675800928172,15.6448969378356,5.86185067402984));
#133876=CARTESIAN_POINT('Ctrl Pts',(17.6787319216953,15.6280259466993,5.89048393857087));
#133877=CARTESIAN_POINT('Ctrl Pts',(17.6816969788667,15.6093427930072,5.91784658956881));
#133878=CARTESIAN_POINT('Ctrl Pts',(17.6846634558833,15.5906506927132,5.94522234342655));
#133879=CARTESIAN_POINT('Ctrl Pts',(17.6876638663243,15.5701445460918,5.97132623845906));
#133880=CARTESIAN_POINT('Ctrl Pts',(17.6906557722056,15.5480108339518,5.99590593065765));
#133881=CARTESIAN_POINT('Ctrl Pts',(17.6936534818921,15.5258341860522,6.02053330341454));
#133882=CARTESIAN_POINT('Ctrl Pts',(17.6966421815377,15.5020231917903,6.04363032092347));
#133883=CARTESIAN_POINT('Ctrl Pts',(17.6995597280143,15.476800747688,6.06496215169117));
#133884=CARTESIAN_POINT('Ctrl Pts',(17.7005929302518,15.4678686241065,6.07251647703187));
#133885=CARTESIAN_POINT('Ctrl Pts',(17.7016170689804,15.4587598479432,6.07984962154434));
#133886=CARTESIAN_POINT('Ctrl Pts',(17.7026290303306,15.449485577811,6.08695186598542));
#133887=CARTESIAN_POINT('Ctrl Pts',(17.7026302896054,15.4494740369995,6.08696070394931));
#133888=CARTESIAN_POINT('Ctrl Pts',(17.7026315488634,15.4494624959087,6.08696954157464));
#133889=CARTESIAN_POINT('Ctrl Pts',(17.7026328081046,15.4494509545388,6.08697837886135));
#133890=CARTESIAN_POINT('Ctrl Pts',(17.705221542436,15.4257243305525,6.10514597762664));
#133891=CARTESIAN_POINT('Ctrl Pts',(17.7077390018072,15.4008132845558,6.12188257860068));
#133892=CARTESIAN_POINT('Ctrl Pts',(17.7102261456198,15.3749257598694,6.13705058790182));
#133893=CARTESIAN_POINT('Ctrl Pts',(17.7104828757241,15.3722535754633,6.1386162732432));
#133894=CARTESIAN_POINT('Ctrl Pts',(17.7107392828173,15.3695710324748,6.14016524690346));
#133895=CARTESIAN_POINT('Ctrl Pts',(17.710995411948,15.366878391042,6.14169735964926));
#133896=CARTESIAN_POINT('Ctrl Pts',(17.713729728643,15.3381329906211,6.15805349003897));
#133897=CARTESIAN_POINT('Ctrl Pts',(17.7164332042827,15.3082310928872,6.1724882306324));
#133898=CARTESIAN_POINT('Ctrl Pts',(17.7191528169111,15.2774700364291,6.18486798769374));
#133899=CARTESIAN_POINT('Ctrl Pts',(17.7218696256405,15.2467406943755,6.19723498132404));
#133900=CARTESIAN_POINT('Ctrl Pts',(17.7246030187271,15.2151543181013,6.20755167245362));
#133901=CARTESIAN_POINT('Ctrl Pts',(17.7273822157546,15.1830148370127,6.21572778788368));
#133902=CARTESIAN_POINT('Ctrl Pts',(17.7301600872982,15.1508906842223,6.22390000387509));
#133903=CARTESIAN_POINT('Ctrl Pts',(17.7329839439362,15.1182141126201,6.22993396079429));
#133904=CARTESIAN_POINT('Ctrl Pts',(17.7358601647421,15.0852924129001,6.2337769843443));
#133905=CARTESIAN_POINT('Ctrl Pts',(17.7387387356219,15.0523438138463,6.23762314791363));
#133906=CARTESIAN_POINT('Ctrl Pts',(17.7416697979649,15.0191497260224,6.23927488801611));
#133907=CARTESIAN_POINT('Ctrl Pts',(17.7446349270463,14.9860205343245,6.23871418193894));
#133908=CARTESIAN_POINT('Ctrl Pts',(17.7476014743928,14.9528754964446,6.23815320766777));
#133909=CARTESIAN_POINT('Ctrl Pts',(17.7506019582001,14.9197953589216,6.23537753125499));
#133910=CARTESIAN_POINT('Ctrl Pts',(17.7535939449745,14.8870934545809,6.2304041588691));
#133911=CARTESIAN_POINT('Ctrl Pts',(17.7565917316453,14.8543281583636,6.22542114571718));
#133912=CARTESIAN_POINT('Ctrl Pts',(17.7595805158066,14.8219425048939,6.2182313951504));
#133913=CARTESIAN_POINT('Ctrl Pts',(17.7624981597374,14.7902552237342,6.20889196031308));
#133914=CARTESIAN_POINT('Ctrl Pts',(17.7635305207602,14.7790431928056,6.20558735264657));
#133915=CARTESIAN_POINT('Ctrl Pts',(17.7645538352473,14.7679186330585,6.20201401295087));
#133916=CARTESIAN_POINT('Ctrl Pts',(17.7655649975604,14.7568957630668,6.19817590699701));
#133917=CARTESIAN_POINT('Ctrl Pts',(17.7655662553768,14.7568820513741,6.19817113265698));
#133918=CARTESIAN_POINT('Ctrl Pts',(17.7655675131764,14.7568683398103,6.19816635789855));
#133919=CARTESIAN_POINT('Ctrl Pts',(17.7655687709592,14.7568546283756,6.19816158272171));
#133920=CARTESIAN_POINT('Ctrl Pts',(17.7681578335635,14.7286305475446,6.18833219726503));
#133921=CARTESIAN_POINT('Ctrl Pts',(17.7706756363368,14.7009506171342,6.17672629876546));
#133922=CARTESIAN_POINT('Ctrl Pts',(17.7731631483601,14.6740441602152,6.16344195838684));
#133923=CARTESIAN_POINT('Ctrl Pts',(17.7734197974233,14.6712680864123,6.16207134651384));
#133924=CARTESIAN_POINT('Ctrl Pts',(17.7736761240389,14.6685002701096,6.16068290654834));
#133925=CARTESIAN_POINT('Ctrl Pts',(17.7739321732037,14.665740978691,6.15927677356913));
#133926=CARTESIAN_POINT('Ctrl Pts',(17.7766666913574,14.6362726830942,6.14425975072063));
#133927=CARTESIAN_POINT('Ctrl Pts',(17.779370402119,14.6077734432019,6.12722017812163));
#133928=CARTESIAN_POINT('Ctrl Pts',(17.7820902725442,14.5805183433097,6.10833296822113));
#133929=CARTESIAN_POINT('Ctrl Pts',(17.7848072466106,14.5532922670595,6.08946587109295));
#133930=CARTESIAN_POINT('Ctrl Pts',(17.7875408262062,14.5273075043819,6.06875561023286));
#133931=CARTESIAN_POINT('Ctrl Pts',(17.7903202095314,14.5028065590824,6.04640639711805));
#133932=CARTESIAN_POINT('Ctrl Pts',(17.7930996912874,14.4783047460923,6.02405639251532));
#133933=CARTESIAN_POINT('Ctrl Pts',(17.7959252069821,14.4552867150597,6.00006760155612));
#133934=CARTESIAN_POINT('Ctrl Pts',(17.7988031159527,14.4339657418564,5.97466806841847));
#133935=CARTESIAN_POINT('Ctrl Pts',(17.8016809333757,14.4126454468827,5.94926934325114));
#133936=CARTESIAN_POINT('Ctrl Pts',(17.804611178714,14.3930220433968,5.92246005215071));
#133937=CARTESIAN_POINT('Ctrl Pts',(17.8075754145475,14.3752810566636,5.89448927635161));
#133938=CARTESIAN_POINT('Ctrl Pts',(17.8105439488833,14.3575143433425,5.8664779395268));
#133939=CARTESIAN_POINT('Ctrl Pts',(17.8135464127681,14.3416355993389,5.83730161808677));
#133940=CARTESIAN_POINT('Ctrl Pts',(17.8165402612616,14.3278032035129,5.80723189254072));
#133941=CARTESIAN_POINT('Ctrl Pts',(17.8184366140737,14.3190415367889,5.78818523446117));
#133942=CARTESIAN_POINT('Ctrl Pts',(17.8203290112871,14.3111003597056,5.76878054731838));
#133943=CARTESIAN_POINT('Ctrl Pts',(17.8222024383386,14.3040135853341,5.74909189204504));
#133944=CARTESIAN_POINT('Origin',(13.2437274406976,15.,5.5));
#133945=CARTESIAN_POINT('',(17.8436773584655,14.2610291961454,5.50063939925591));
#133946=CARTESIAN_POINT('Ctrl Pts',(17.8222024383946,14.3040135851224,5.74909189145678));
#133947=CARTESIAN_POINT('Ctrl Pts',(17.8243357978047,14.295943542177,5.72667149457543));
#133948=CARTESIAN_POINT('Ctrl Pts',(17.8264445030159,14.2889817446023,5.70388266077197));
#133949=CARTESIAN_POINT('Ctrl Pts',(17.8285029552338,14.2831690256882,5.68084193278501));
#133950=CARTESIAN_POINT('Ctrl Pts',(17.828504216325,14.2831654645812,5.68082781710211));
#133951=CARTESIAN_POINT('Ctrl Pts',(17.8285054773985,14.2831619039007,5.68081370130835));
#133952=CARTESIAN_POINT('Ctrl Pts',(17.8285067384545,14.2831583436466,5.68079958540374));
#133953=CARTESIAN_POINT('Ctrl Pts',(17.8312998697714,14.2752726846418,5.64953406105414));
#133954=CARTESIAN_POINT('Ctrl Pts',(17.8340065810712,14.2694783607943,5.6177204690563));
#133955=CARTESIAN_POINT('Ctrl Pts',(17.8366815091306,14.2658017005483,5.58560485200468));
#133956=CARTESIAN_POINT('Ctrl Pts',(17.8375267351236,14.2646399463859,5.57545693261783));
#133957=CARTESIAN_POINT('Ctrl Pts',(17.8383687877544,14.2636896841653,5.56527924594083));
#133958=CARTESIAN_POINT('Ctrl Pts',(17.8392093907452,14.2629518112339,5.55508063474149));
#133959=CARTESIAN_POINT('Ctrl Pts',(17.8407006737749,14.2616427778463,5.53698765152026));
#133960=CARTESIAN_POINT('Ctrl Pts',(17.8421872462419,14.2610012335988,5.51882616272172));
#133961=CARTESIAN_POINT('Ctrl Pts',(17.8436773584384,14.2610291961449,5.50063939958663));
#133962=CARTESIAN_POINT('',(18.1999951595719,14.4315705875013,5.97264794125123));
#133963=CARTESIAN_POINT('Ctrl Pts',(17.8436773585104,14.2610291961463,5.50063939870812));
#133964=CARTESIAN_POINT('Ctrl Pts',(17.8463594095494,14.2610795259361,5.46790506697329));
#133965=CARTESIAN_POINT('Ctrl Pts',(17.8490517590635,14.2633033205486,5.43512841146423));
#133966=CARTESIAN_POINT('Ctrl Pts',(17.8517858606446,14.2676752024076,5.40262005104255));
#133967=CARTESIAN_POINT('Ctrl Pts',(17.8545179415039,14.2720438530929,5.37013571692455));
#133968=CARTESIAN_POINT('Ctrl Pts',(17.8572919721943,14.2785570835378,5.33791937843377));
#133969=CARTESIAN_POINT('Ctrl Pts',(17.8601181797673,14.2871520781629,5.30627092034022));
#133970=CARTESIAN_POINT('Ctrl Pts',(17.8629460917766,14.2957522562788,5.27460337561596));
#133971=CARTESIAN_POINT('Ctrl Pts',(17.8658263187323,14.3064365697756,5.24350444886535));
#133972=CARTESIAN_POINT('Ctrl Pts',(17.8687454375362,14.31910807561,5.21326341890527));
#133973=CARTESIAN_POINT('Ctrl Pts',(17.8716654355075,14.3317833977924,5.18301328108585));
#133974=CARTESIAN_POINT('Ctrl Pts',(17.8746242343264,14.3464471824028,5.15362159625291));
#133975=CARTESIAN_POINT('Ctrl Pts',(17.8775849802679,14.3629689473109,5.12536610898706));
#133976=CARTESIAN_POINT('Ctrl Pts',(17.8805516191879,14.3795235966361,5.09705438286081));
#133977=CARTESIAN_POINT('Ctrl Pts',(17.8835198303149,14.3979440054524,5.06988351684653));
#133978=CARTESIAN_POINT('Ctrl Pts',(17.8864326303791,14.4180620188063,5.04411993333822));
#133979=CARTESIAN_POINT('Ctrl Pts',(17.8881248041672,14.4297494584233,5.02915273348248));
#133980=CARTESIAN_POINT('Ctrl Pts',(17.889797916704,14.4420091275208,5.01466025184568));
#133981=CARTESIAN_POINT('Ctrl Pts',(17.8914388206508,14.4548013425205,5.00069220202942));
#133982=CARTESIAN_POINT('Ctrl Pts',(17.8914400802631,14.4548111622496,5.00068147969052));
#133983=CARTESIAN_POINT('Ctrl Pts',(17.8914413398586,14.4548209823129,5.0006707576363));
#133984=CARTESIAN_POINT('Ctrl Pts',(17.8914425994372,14.4548308027104,5.00066003586679));
#133985=CARTESIAN_POINT('Ctrl Pts',(17.8940314338703,14.4750148415794,4.97862339112774));
#133986=CARTESIAN_POINT('Ctrl Pts',(17.8965489662599,14.496615226222,4.95778864968078));
#133987=CARTESIAN_POINT('Ctrl Pts',(17.8990361340503,14.5194513004904,4.93832760805207));
#133988=CARTESIAN_POINT('Ctrl Pts',(17.8992933057813,14.5218125375449,4.93631534744756));
#133989=CARTESIAN_POINT('Ctrl Pts',(17.8995501528709,14.5241869404141,4.93431778010501));
#133990=CARTESIAN_POINT('Ctrl Pts',(17.899806720575,14.5265742779001,4.93233509938062));
#133991=CARTESIAN_POINT('Ctrl Pts',(17.902541477429,14.552020923942,4.91120169243526));
#133992=CARTESIAN_POINT('Ctrl Pts',(17.9052453302838,14.578942617527,4.89175844415563));
#133993=CARTESIAN_POINT('Ctrl Pts',(17.9079652717836,14.6070698664759,4.87418892292457));
#133994=CARTESIAN_POINT('Ctrl Pts',(17.9106824052865,14.635168077584,4.85663754001058));
#133995=CARTESIAN_POINT('Ctrl Pts',(17.9134160753429,14.6644689296677,4.84095563974389));
#133996=CARTESIAN_POINT('Ctrl Pts',(17.91619552483,14.694688870348,4.82728527763572));
#133997=CARTESIAN_POINT('Ctrl Pts',(17.918973643444,14.7248943409312,4.81362146125409));
#133998=CARTESIAN_POINT('Ctrl Pts',(17.9217977227498,14.756017816082,4.80196701342871));
#133999=CARTESIAN_POINT('Ctrl Pts',(17.9246741683966,14.7877658634584,4.7924275524122));
#134000=CARTESIAN_POINT('Ctrl Pts',(17.927552951004,14.8195397044511,4.78288034108607));
#134001=CARTESIAN_POINT('Ctrl Pts',(17.9304842268543,14.8519390777149,4.77545147120308));
#134002=CARTESIAN_POINT('Ctrl Pts',(17.9334495989564,14.8846614480637,4.77021298268738));
#134003=CARTESIAN_POINT('Ctrl Pts',(17.9364163821299,14.9173993893415,4.76497200143866));
#134004=CARTESIAN_POINT('Ctrl Pts',(17.9394171311389,14.9504607166395,4.76192361340681));
#134005=CARTESIAN_POINT('Ctrl Pts',(17.9424094410172,14.9835338646715,4.76110588474489));
#134006=CARTESIAN_POINT('Ctrl Pts',(17.9454075337696,15.016670929163,4.76028657575803));
#134007=CARTESIAN_POINT('Ctrl Pts',(17.9483966821973,15.0498200071206,4.76170705120555));
#134008=CARTESIAN_POINT('Ctrl Pts',(17.9513147792807,15.0826572162376,4.76536688948503));
#134009=CARTESIAN_POINT('Ctrl Pts',(17.952343720405,15.0942358422743,4.76665737366236));
#134010=CARTESIAN_POINT('Ctrl Pts',(17.9533636886311,15.1057755873781,4.7682258913146));
#134011=CARTESIAN_POINT('Ctrl Pts',(17.9543716120705,15.1172619072478,4.77007104090789));
#134012=CARTESIAN_POINT('Ctrl Pts',(17.9543728624177,15.1172761562348,4.77007332984923));
#134013=CARTESIAN_POINT('Ctrl Pts',(17.9543741127484,15.1172904051685,4.77007561921983));
#134014=CARTESIAN_POINT('Ctrl Pts',(17.9543753630624,15.1173046540489,4.77007790901972));
#134015=CARTESIAN_POINT('Ctrl Pts',(17.956966132579,15.1468296885974,4.77482259201186));
#134016=CARTESIAN_POINT('Ctrl Pts',(17.959485714194,15.1761291355963,4.78141356596197));
#134017=CARTESIAN_POINT('Ctrl Pts',(17.9619751194107,15.2049597393243,4.78979421528902));
#134018=CARTESIAN_POINT('Ctrl Pts',(17.962230909525,15.2079221270356,4.79065533955868));
#134019=CARTESIAN_POINT('Ctrl Pts',(17.9624863810408,15.210879534695,4.79153532500646));
#134020=CARTESIAN_POINT('Ctrl Pts',(17.9627415784489,15.2138316785748,4.79243408630913));
#134021=CARTESIAN_POINT('Ctrl Pts',(17.9654772791855,15.245478481916,4.80206875296297));
#134022=CARTESIAN_POINT('Ctrl Pts',(17.9681823166877,15.2765243880882,4.81386500752228));
#134023=CARTESIAN_POINT('Ctrl Pts',(17.9709036077638,15.3066678945923,4.82769865939054));
#134024=CARTESIAN_POINT('Ctrl Pts',(17.9736221022352,15.3367804233474,4.84151809475102));
#134025=CARTESIAN_POINT('Ctrl Pts',(17.9763572964495,15.3659924876036,4.85737017958949));
#134026=CARTESIAN_POINT('Ctrl Pts',(17.979138305386,15.3940294988691,4.87509618555731));
#134027=CARTESIAN_POINT('Ctrl Pts',(17.9819179950805,15.4220532100699,4.89281378274626));
#134028=CARTESIAN_POINT('Ctrl Pts',(17.9847436800359,15.4489030742888,4.91240322043754));
#134029=CARTESIAN_POINT('Ctrl Pts',(17.987621605196,15.4743294733481,4.93367749389957));
#134030=CARTESIAN_POINT('Ctrl Pts',(17.9905018851045,15.4997766765523,4.95496917419406));
#134031=CARTESIAN_POINT('Ctrl Pts',(17.993434531532,15.5237981235656,4.97794835812273));
#134032=CARTESIAN_POINT('Ctrl Pts',(17.9964009679253,15.5461672042858,5.00240196307429));
#134033=CARTESIAN_POINT('Ctrl Pts',(17.9993688260062,15.5685470055611,5.02686728760528));
#134034=CARTESIAN_POINT('Ctrl Pts',(18.0023703420288,15.5892727947365,5.05280858692245));
#134035=CARTESIAN_POINT('Ctrl Pts',(18.005362930613,15.6081413450034,5.07998651472653));
#134036=CARTESIAN_POINT('Ctrl Pts',(18.0083613143937,15.6270464345251,5.10721707303048));
#134037=CARTESIAN_POINT('Ctrl Pts',(18.011350260665,15.6440867502017,5.13568945173416));
#134038=CARTESIAN_POINT('Ctrl Pts',(18.0142675126761,15.6590844306501,5.16513277119679));
#134039=CARTESIAN_POINT('Ctrl Pts',(18.0152947004806,15.6643652340887,5.17549999986241));
#134040=CARTESIAN_POINT('Ctrl Pts',(18.0163128615438,15.6693930587093,5.18598730274498));
#134041=CARTESIAN_POINT('Ctrl Pts',(18.0173189327465,15.6741611019489,5.19658180756563));
#134042=CARTESIAN_POINT('Ctrl Pts',(18.0173202085358,15.6741671482592,5.19659524235646));
#134043=CARTESIAN_POINT('Ctrl Pts',(18.0173214843078,15.6741731941654,5.19660867734728));
#134044=CARTESIAN_POINT('Ctrl Pts',(18.0173227600623,15.6741792396675,5.19662211253806));
#134045=CARTESIAN_POINT('Ctrl Pts',(18.0199069065493,15.6864249048209,5.22383620391819));
#134046=CARTESIAN_POINT('Ctrl Pts',(18.0224197289205,15.697011589596,5.25187499153676));
#134047=CARTESIAN_POINT('Ctrl Pts',(18.0249021843778,15.7058528471292,5.28050526628785));
#134048=CARTESIAN_POINT('Ctrl Pts',(18.0251587405207,15.7067665710492,5.28346414026898));
#134049=CARTESIAN_POINT('Ctrl Pts',(18.0254149723221,15.7076616645656,5.28642928749976));
#134050=CARTESIAN_POINT('Ctrl Pts',(18.0256709249919,15.7085380415357,5.28940042032651));
#134051=CARTESIAN_POINT('Ctrl Pts',(18.0284003719407,15.7178836148767,5.32108420560131));
#134052=CARTESIAN_POINT('Ctrl Pts',(18.0310989130854,15.7250996821711,5.35345416599969));
#134053=CARTESIAN_POINT('Ctrl Pts',(18.0338135819061,15.7301240673385,5.3861910161145));
#134054=CARTESIAN_POINT('Ctrl Pts',(18.0365254513628,15.7351432713645,5.41889410801899));
#134055=CARTESIAN_POINT('Ctrl Pts',(18.0392538957621,15.7379758245001,5.451963087929));
#134056=CARTESIAN_POINT('Ctrl Pts',(18.0420282370079,15.7386032531471,5.4850821085239));
#134057=CARTESIAN_POINT('Ctrl Pts',(18.044801265282,15.7392303848602,5.51818545536712));
#134058=CARTESIAN_POINT('Ctrl Pts',(18.0476203722892,15.7376547832463,5.5513387005063));
#134059=CARTESIAN_POINT('Ctrl Pts',(18.0504920836694,15.7338953786096,5.58423131758289));
#134060=CARTESIAN_POINT('Ctrl Pts',(18.0533661966296,15.7301328300251,5.61715144238518));
#134061=CARTESIAN_POINT('Ctrl Pts',(18.0562930450686,15.7241829251285,5.64981048106769));
#134062=CARTESIAN_POINT('Ctrl Pts',(18.0592543812016,15.7160990512311,5.68190285989289));
#134063=CARTESIAN_POINT('Ctrl Pts',(18.0622171618623,15.7080112340529,5.71401089325004));
#134064=CARTESIAN_POINT('Ctrl Pts',(18.0652143040956,15.6977872225133,5.74555173553004));
#134065=CARTESIAN_POINT('Ctrl Pts',(18.0682035479844,15.6855151363698,5.7762250552271));
#134066=CARTESIAN_POINT('Ctrl Pts',(18.071198680356,15.6732188755617,5.80695879800219));
#134067=CARTESIAN_POINT('Ctrl Pts',(18.0741854168822,15.6588659589358,5.83682153768798));
#134068=CARTESIAN_POINT('Ctrl Pts',(18.0771017174444,15.6425845871123,5.865516948982));
#134069=CARTESIAN_POINT('Ctrl Pts',(18.078160626474,15.6366728193537,5.87593625573006));
#134070=CARTESIAN_POINT('Ctrl Pts',(18.0792101010587,15.6305072187241,5.88620172070509));
#134071=CARTESIAN_POINT('Ctrl Pts',(18.0802467831717,15.6240954635429,5.89629941435817));
#134072=CARTESIAN_POINT('Ctrl Pts',(18.0802480395688,15.6240876928765,5.89631165216296));
#134073=CARTESIAN_POINT('Ctrl Pts',(18.0802492959491,15.6240799218336,5.89632388974701));
#134074=CARTESIAN_POINT('Ctrl Pts',(18.0802505523126,15.6240721504142,5.8963361271103));
#134075=CARTESIAN_POINT('Ctrl Pts',(18.0828415305574,15.6080452773152,5.92157304428439));
#134076=CARTESIAN_POINT('Ctrl Pts',(18.085361043973,15.5904128634294,5.94587256850564));
#134077=CARTESIAN_POINT('Ctrl Pts',(18.0878498837288,15.5713228325143,5.96903414038106));
#134078=CARTESIAN_POINT('Ctrl Pts',(18.0881100761095,15.5693270910931,5.97145553553635));
#134079=CARTESIAN_POINT('Ctrl Pts',(18.0883699332463,15.5673154634936,5.9738644790996));
#134080=CARTESIAN_POINT('Ctrl Pts',(18.0886295017471,15.5652881502086,5.9762607327977));
#134081=CARTESIAN_POINT('Ctrl Pts',(18.0913687823211,15.5438934899064,6.00154889829641));
#134082=CARTESIAN_POINT('Ctrl Pts',(18.0940767605781,15.520746688581,6.02542590128219));
#134083=CARTESIAN_POINT('Ctrl Pts',(18.0968005095287,15.4960817934527,6.04766341424653));
#134084=CARTESIAN_POINT('Ctrl Pts',(18.0995214210206,15.4714425929172,6.06987776133736));
#134085=CARTESIAN_POINT('Ctrl Pts',(18.1022585547669,15.4452889468507,6.09045633377021));
#134086=CARTESIAN_POINT('Ctrl Pts',(18.1050412775618,15.4178759723684,6.1092093085127));
#134087=CARTESIAN_POINT('Ctrl Pts',(18.1078226284374,15.3904765128458,6.12795303779016));
#134088=CARTESIAN_POINT('Ctrl Pts',(18.110649750084,15.3618192081673,6.14487317653914));
#134089=CARTESIAN_POINT('Ctrl Pts',(18.1135291801814,15.332175245214,6.15981408324162));
#134090=CARTESIAN_POINT('Ctrl Pts',(18.1164108409359,15.3025083174676,6.1747665644705));
#134091=CARTESIAN_POINT('Ctrl Pts',(18.1193449331285,15.2718532680766,6.18773681972673));
#134092=CARTESIAN_POINT('Ctrl Pts',(18.1223131902413,15.2404961073911,6.19860068044639));
#134093=CARTESIAN_POINT('Ctrl Pts',(18.1252828002271,15.2091246547293,6.20946949269979));
#134094=CARTESIAN_POINT('Ctrl Pts',(18.128286442416,15.1770503451651,6.21822987810168));
#134095=CARTESIAN_POINT('Ctrl Pts',(18.1312818493294,15.1445740698856,6.22478953106497));
#134096=CARTESIAN_POINT('Ctrl Pts',(18.13428289449,15.1120366645917,6.23136153124717));
#134097=CARTESIAN_POINT('Ctrl Pts',(18.1372751985486,15.0790955465581,6.23572404130749));
#134098=CARTESIAN_POINT('Ctrl Pts',(18.1401968316883,15.0460705208212,6.23782052554615));
#134099=CARTESIAN_POINT('Ctrl Pts',(18.1411943618116,15.0347948210935,6.23853632594998));
#134100=CARTESIAN_POINT('Ctrl Pts',(18.1421835232276,15.0235095039505,6.23898831423258));
#134101=CARTESIAN_POINT('Ctrl Pts',(18.1431615371195,15.0122278243948,6.23917541247216));
#134102=CARTESIAN_POINT('Ctrl Pts',(18.1431627392938,15.0122139569584,6.23917564245324));
#134103=CARTESIAN_POINT('Ctrl Pts',(18.1431639414532,15.0122000894994,6.23917587203561));
#134104=CARTESIAN_POINT('Ctrl Pts',(18.1431651435976,15.0121862220177,6.23917610121923));
#134105=CARTESIAN_POINT('Ctrl Pts',(18.1457442399221,14.9824347454704,6.23966779475253));
#134106=CARTESIAN_POINT('Ctrl Pts',(18.1482544763774,14.9525758663653,6.23832151875025));
#134107=CARTESIAN_POINT('Ctrl Pts',(18.1507358914744,14.9228585657899,6.23514796266056));
#134108=CARTESIAN_POINT('Ctrl Pts',(18.1509738968701,14.9200082253161,6.23484357043135));
#134109=CARTESIAN_POINT('Ctrl Pts',(18.1512116371173,14.917159217899,6.23452239287036));
#134110=CARTESIAN_POINT('Ctrl Pts',(18.1514491475457,14.9143117821302,6.23418445593601));
#134111=CARTESIAN_POINT('Ctrl Pts',(18.1541598189073,14.8818144191945,6.23032763172769));
#134112=CARTESIAN_POINT('Ctrl Pts',(18.1568413521458,14.8495173610134,6.22428465180375));
#134113=CARTESIAN_POINT('Ctrl Pts',(18.1595386565067,14.8177334913946,6.21612134156257));
#134114=CARTESIAN_POINT('Ctrl Pts',(18.1622333190795,14.7859807514648,6.20796602661311));
#134115=CARTESIAN_POINT('Ctrl Pts',(18.1649441825578,14.7547402622896,6.19769508183801));
#134116=CARTESIAN_POINT('Ctrl Pts',(18.1676990754875,14.7243051351502,6.18541363159718));
#134117=CARTESIAN_POINT('Ctrl Pts',(18.170454816463,14.6938606390862,6.17312840072546));
#134118=CARTESIAN_POINT('Ctrl Pts',(18.1732548315693,14.6642220109734,6.15883174278628));
#134119=CARTESIAN_POINT('Ctrl Pts',(18.1761050002291,14.6356632829083,6.14266198635992));
#134120=CARTESIAN_POINT('Ctrl Pts',(18.1789554229838,14.6071020088089,6.12649078838641));
#134121=CARTESIAN_POINT('Ctrl Pts',(18.1818560391891,14.5796208401452,6.1084462818842));
#134122=CARTESIAN_POINT('Ctrl Pts',(18.1847889192762,14.5534743933048,6.08869663707073));
#134123=CARTESIAN_POINT('Ctrl Pts',(18.1877272800705,14.5272790862942,6.06891008586564));
#134124=CARTESIAN_POINT('Ctrl Pts',(18.1906978645508,14.5024235641472,6.04741190910945));
#134125=CARTESIAN_POINT('Ctrl Pts',(18.193659652731,14.4791437569311,6.02440097586502));
#134126=CARTESIAN_POINT('Ctrl Pts',(18.195783601337,14.4624494118007,6.0078994448261));
#134127=CARTESIAN_POINT('Ctrl Pts',(18.1979025422642,14.4465649110223,5.99062033918995));
#134128=CARTESIAN_POINT('Ctrl Pts',(18.1999951595719,14.4315705875013,5.97264794125123));
#134129=CARTESIAN_POINT('',(18.2,15.2587465130648,6.19222196005097));
#134130=CARTESIAN_POINT('Origin',(18.2,15.,5.5));
#134131=CARTESIAN_POINT('',(17.9231997159231,14.2612470260202,5.49963276901434));
#134132=CARTESIAN_POINT('Ctrl Pts',(17.9231997159231,14.2612470260202,5.49963276901434));
#134133=CARTESIAN_POINT('Ctrl Pts',(17.9262586431742,14.2612187711484,5.46303332832203));
#134134=CARTESIAN_POINT('Ctrl Pts',(17.9292580652234,14.2638801053733,5.42651463730436));
#134135=CARTESIAN_POINT('Ctrl Pts',(17.9322433460566,14.2691950817959,5.39045683330052));
#134136=CARTESIAN_POINT('Ctrl Pts',(17.9350059852405,14.2741136683366,5.3570882131299));
#134137=CARTESIAN_POINT('Ctrl Pts',(17.9377571858871,14.2813058278008,5.32411334875332));
#134138=CARTESIAN_POINT('Ctrl Pts',(17.9405516084341,14.2907103743296,5.29184004945994));
#134139=CARTESIAN_POINT('Ctrl Pts',(17.9407977040603,14.2915386018895,5.2889978458681));
#134140=CARTESIAN_POINT('Ctrl Pts',(17.9410441349047,14.2923839944149,5.28616105055996));
#134141=CARTESIAN_POINT('Ctrl Pts',(17.9412909383015,14.2932465145934,5.28332985490843));
#134142=CARTESIAN_POINT('Ctrl Pts',(17.9433011938874,14.3002718879439,5.26026928545832));
#134143=CARTESIAN_POINT('Ctrl Pts',(17.9453367038473,14.3084321983208,5.23758299047853));
#134144=CARTESIAN_POINT('Ctrl Pts',(17.9474199441049,14.3176914668121,5.21538482826282));
#134145=CARTESIAN_POINT('Ctrl Pts',(17.9474212056243,14.3176970738209,5.21537138602483));
#134146=CARTESIAN_POINT('Ctrl Pts',(17.9474224671611,14.3177026812326,5.21535794396523));
#134147=CARTESIAN_POINT('Ctrl Pts',(17.9474237287155,14.3177082890473,5.21534450208405));
#134148=CARTESIAN_POINT('Ctrl Pts',(17.9500793537949,14.3295129750619,5.18704877605385));
#134149=CARTESIAN_POINT('Ctrl Pts',(17.9528186941826,14.3431481780221,5.15945251371052));
#134150=CARTESIAN_POINT('Ctrl Pts',(17.9555881595096,14.3584881298957,5.13278509509163));
#134151=CARTESIAN_POINT('Ctrl Pts',(17.9558022896295,14.3596741876162,5.13072321784466));
#134152=CARTESIAN_POINT('Ctrl Pts',(17.9560165998394,14.3608704140577,5.12866690604059));
#134153=CARTESIAN_POINT('Ctrl Pts',(17.956231065369,14.3620767396463,5.12661627172541));
#134154=CARTESIAN_POINT('Ctrl Pts',(17.959214568465,14.3788583461549,5.0980891986902));
#134155=CARTESIAN_POINT('Ctrl Pts',(17.9622275004938,14.3975989598379,5.0706576239006));
#134156=CARTESIAN_POINT('Ctrl Pts',(17.9652194777493,14.4181104527675,5.04457671855219));
#134157=CARTESIAN_POINT('Ctrl Pts',(17.9682083269364,14.4386005012313,5.01852308040877));
#134158=CARTESIAN_POINT('Ctrl Pts',(17.9711760074106,14.4608575905549,4.99381705473338));
#134159=CARTESIAN_POINT('Ctrl Pts',(17.9740950538289,14.4846693294737,4.97068678059164));
#134160=CARTESIAN_POINT('Ctrl Pts',(17.9770126517411,14.5084692523937,4.9475679842883));
#134161=CARTESIAN_POINT('Ctrl Pts',(17.9798816370051,14.53382229895,4.92602338806137));
#134162=CARTESIAN_POINT('Ctrl Pts',(17.982699375066,14.5604923181853,4.9062561976417));
#134163=CARTESIAN_POINT('Ctrl Pts',(17.9855192979158,14.5871830165468,4.88647368034056));
#134164=CARTESIAN_POINT('Ctrl Pts',(17.988288046098,14.6151928189579,4.86847155315384));
#134165=CARTESIAN_POINT('Ctrl Pts',(17.9910268829266,14.6442600716981,4.85242704013227));
#134166=CARTESIAN_POINT('Ctrl Pts',(17.9937669623233,14.6733405118036,4.83637524796198));
#134167=CARTESIAN_POINT('Ctrl Pts',(17.9964774831177,14.7034794728911,4.8222833046908));
#134168=CARTESIAN_POINT('Ctrl Pts',(17.9991997379415,14.7343884256453,4.81029712951543));
#134169=CARTESIAN_POINT('Ctrl Pts',(18.0017724321862,14.7635992416821,4.79896947435947));
#134170=CARTESIAN_POINT('Ctrl Pts',(18.0043562329034,14.7934981500566,4.78952287559149));
#134171=CARTESIAN_POINT('Ctrl Pts',(18.0069960990905,14.8238172483661,4.78204727574495));
#134172=CARTESIAN_POINT('Ctrl Pts',(18.0071548466427,14.8256404781444,4.78159773281623));
#134173=CARTESIAN_POINT('Ctrl Pts',(18.0073137969379,14.8274652383969,4.78115530619246));
#134174=CARTESIAN_POINT('Ctrl Pts',(18.0074729597527,14.8292914752232,4.78072001126449));
#134175=CARTESIAN_POINT('Ctrl Pts',(18.0084596254331,14.8406124939122,4.77802157591165));
#134176=CARTESIAN_POINT('Ctrl Pts',(18.0094545130156,14.8519895282679,4.77559725406811));
#134177=CARTESIAN_POINT('Ctrl Pts',(18.0104600051911,14.863407987732,4.77345012771598));
#134178=CARTESIAN_POINT('Ctrl Pts',(18.0104612096985,14.8634216662258,4.77344755561293));
#134179=CARTESIAN_POINT('Ctrl Pts',(18.0104624142211,14.8634353447791,4.77344498390754));
#134180=CARTESIAN_POINT('Ctrl Pts',(18.0104636187589,14.8634490233919,4.77344241259979));
#134181=CARTESIAN_POINT('Ctrl Pts',(18.0131276391294,14.8937013768235,4.76775557053046));
#134182=CARTESIAN_POINT('Ctrl Pts',(18.0158740544306,14.9243765590572,4.76399716531421));
#134183=CARTESIAN_POINT('Ctrl Pts',(18.0186488845286,14.9552108250908,4.76218805642328));
#134184=CARTESIAN_POINT('Ctrl Pts',(18.0188507331611,14.9574537928449,4.76205645695853));
#134185=CARTESIAN_POINT('Ctrl Pts',(18.0190527321505,14.9596975819019,4.76193516207424));
#134186=CARTESIAN_POINT('Ctrl Pts',(18.0192548607188,14.9619420812788,4.76182417475526));
#134187=CARTESIAN_POINT('Ctrl Pts',(18.0222310129887,14.9949902147955,4.76018999130471));
#134188=CARTESIAN_POINT('Ctrl Pts',(18.0252346457585,15.0281975228741,4.76079239557386));
#134189=CARTESIAN_POINT('Ctrl Pts',(18.0282161966136,15.0612477944481,4.76361442227235));
#134190=CARTESIAN_POINT('Ctrl Pts',(18.0311947334598,15.0942646559551,4.7664335962227));
#134191=CARTESIAN_POINT('Ctrl Pts',(18.0341509866931,15.127124915222,4.77146767607796));
#134192=CARTESIAN_POINT('Ctrl Pts',(18.0370585499895,15.1595213805558,4.77866468462933));
#134193=CARTESIAN_POINT('Ctrl Pts',(18.0399647749284,15.1919029337276,4.78585838038234));
#134194=CARTESIAN_POINT('Ctrl Pts',(18.0428223355274,15.2238211150562,4.79521304283486));
#134195=CARTESIAN_POINT('Ctrl Pts',(18.0456297593615,15.2549763339614,4.80664310001928));
#134196=CARTESIAN_POINT('Ctrl Pts',(18.0484395231808,15.286157520714,4.81808268414624));
#134197=CARTESIAN_POINT('Ctrl Pts',(18.051199226476,15.3165743283291,4.83160133119134));
#134198=CARTESIAN_POINT('Ctrl Pts',(18.0539312956373,15.3459347183123,4.84707770639228));
#134199=CARTESIAN_POINT('Ctrl Pts',(18.0566646943394,15.3753093963082,4.86256161305463));
#134200=CARTESIAN_POINT('Ctrl Pts',(18.059370824189,15.4036263000318,4.88000550871002));
#134201=CARTESIAN_POINT('Ctrl Pts',(18.0620919965398,15.430604726856,4.89924808088519));
#134202=CARTESIAN_POINT('Ctrl Pts',(18.0646486288197,15.4559518596304,4.91732711992713));
#134203=CARTESIAN_POINT('Ctrl Pts',(18.0672191753305,15.4801174868315,4.9369943935669));
#134204=CARTESIAN_POINT('Ctrl Pts',(18.0698483381693,15.5028828544892,4.95807777932273));
#134205=CARTESIAN_POINT('Ctrl Pts',(18.0700229900163,15.5043951280735,4.95947832105024));
#134206=CARTESIAN_POINT('Ctrl Pts',(18.0701979005238,15.505901241427,4.96088511527658));
#134207=CARTESIAN_POINT('Ctrl Pts',(18.0703730827954,15.5074011384115,4.96229811330113));
#134208=CARTESIAN_POINT('Ctrl Pts',(18.0713722545889,15.5159559695936,4.97035730648927));
#134209=CARTESIAN_POINT('Ctrl Pts',(18.0723803185353,15.5243081081095,4.97861772452402));
#134210=CARTESIAN_POINT('Ctrl Pts',(18.0733997415326,15.5324466368762,4.98706847934758));
#134211=CARTESIAN_POINT('Ctrl Pts',(18.0734011530142,15.5324579053915,4.98708018016755));
#134212=CARTESIAN_POINT('Ctrl Pts',(18.0734025645176,15.5324691734975,4.98709188135243));
#134213=CARTESIAN_POINT('Ctrl Pts',(18.0734039760428,15.5324804411942,4.98710358290217));
#134214=CARTESIAN_POINT('Ctrl Pts',(18.0760361129181,15.55349184138,5.00892400905151));
#134215=CARTESIAN_POINT('Ctrl Pts',(18.0787525505888,15.5731714229398,5.03212001337143));
#134216=CARTESIAN_POINT('Ctrl Pts',(18.0814995687192,15.5913606132484,5.05649077204578));
#134217=CARTESIAN_POINT('Ctrl Pts',(18.0817129673223,15.5927736173208,5.05838398338004));
#134218=CARTESIAN_POINT('Ctrl Pts',(18.0819265504713,15.5941776246337,5.06028425816411));
#134219=CARTESIAN_POINT('Ctrl Pts',(18.0821402929818,15.5955725599306,5.06219148916643));
#134220=CARTESIAN_POINT('Ctrl Pts',(18.0851007307266,15.6148930923556,5.08860756631621));
#134221=CARTESIAN_POINT('Ctrl Pts',(18.0880911152758,15.632474380568,5.11636357154761));
#134222=CARTESIAN_POINT('Ctrl Pts',(18.0910604661353,15.6481590152578,5.14519179339049));
#134223=CARTESIAN_POINT('Ctrl Pts',(18.0940267905801,15.663827663892,5.1739906330025));
#134224=CARTESIAN_POINT('Ctrl Pts',(18.0969718624657,15.6776037789831,5.20385944642274));
#134225=CARTESIAN_POINT('Ctrl Pts',(18.0998672483404,15.6893644578681,5.23451869707503));
#134226=CARTESIAN_POINT('Ctrl Pts',(18.1027613698272,15.7011200009754,5.26516455912119));
#134227=CARTESIAN_POINT('Ctrl Pts',(18.105605811157,15.7108618521799,5.29660014770083));
#134228=CARTESIAN_POINT('Ctrl Pts',(18.1083967095201,15.7184995766532,5.32853413618579));
#134229=CARTESIAN_POINT('Ctrl Pts',(18.1111903662473,15.7261448498155,5.36049968639429));
#134230=CARTESIAN_POINT('Ctrl Pts',(18.1139305056239,15.7316816118874,5.39296458302346));
#134231=CARTESIAN_POINT('Ctrl Pts',(18.1166371406068,15.7350533739779,5.4256248738587));
#134232=CARTESIAN_POINT('Ctrl Pts',(18.1193452857107,15.7384270172859,5.45830338694855));
#134233=CARTESIAN_POINT('Ctrl Pts',(18.1220202337102,15.7396328222108,5.49117741633699));
#134234=CARTESIAN_POINT('Ctrl Pts',(18.1247024284304,15.7386532460656,5.52393168756679));
#134235=CARTESIAN_POINT('Ctrl Pts',(18.1273905478049,15.7376715061513,5.55675830914863));
#134236=CARTESIAN_POINT('Ctrl Pts',(18.1300865965977,15.7344940531765,5.5894643583877));
#134237=CARTESIAN_POINT('Ctrl Pts',(18.1328444052418,15.7291506235284,5.62172425242653));
#134238=CARTESIAN_POINT('Ctrl Pts',(18.1340515200849,15.7268117617459,5.63584466539077));
#134239=CARTESIAN_POINT('Ctrl Pts',(18.1352705770035,15.7240585966878,5.64987951970821));
#134240=CARTESIAN_POINT('Ctrl Pts',(18.1365062824139,15.7208970220618,5.66380134551847));
#134241=CARTESIAN_POINT('Ctrl Pts',(18.1365074611802,15.7208940061668,5.66381462585182));
#134242=CARTESIAN_POINT('Ctrl Pts',(18.1365086399617,15.7208909899003,5.66382790608253));
#134243=CARTESIAN_POINT('Ctrl Pts',(18.1365098187584,15.7208879732623,5.66384118621058));
#134244=CARTESIAN_POINT('Ctrl Pts',(18.1391948817415,15.7140166752005,5.69409066155985));
#134245=CARTESIAN_POINT('Ctrl Pts',(18.1419671514301,15.7051788823793,5.72394224967107));
#134246=CARTESIAN_POINT('Ctrl Pts',(18.1447739657266,15.694462611726,5.75314652340991));
#134247=CARTESIAN_POINT('Ctrl Pts',(18.1450263104535,15.6934991727144,5.75577211374216));
#134248=CARTESIAN_POINT('Ctrl Pts',(18.1452789343971,15.6925205776409,5.75839245032495));
#134249=CARTESIAN_POINT('Ctrl Pts',(18.145531799289,15.6915269069812,5.7610073396442));
#134250=CARTESIAN_POINT('Ctrl Pts',(18.1485916398169,15.6795028029924,5.79264931356071));
#134251=CARTESIAN_POINT('Ctrl Pts',(18.151686076699,15.6652670591775,5.82349779433561));
#134252=CARTESIAN_POINT('Ctrl Pts',(18.1547633469966,15.6489696089779,5.85325730727982));
#134253=CARTESIAN_POINT('Ctrl Pts',(18.1578363265298,15.6326948829827,5.88297532531258));
#134254=CARTESIAN_POINT('Ctrl Pts',(18.1608919108916,15.6143643562405,5.91160769582046));
#134255=CARTESIAN_POINT('Ctrl Pts',(18.1639015842225,15.5941559133991,5.93888206377511));
#134256=CARTESIAN_POINT('Ctrl Pts',(18.167046497236,15.5730394041011,5.96738200555838));
#134257=CARTESIAN_POINT('Ctrl Pts',(18.1701410440723,15.5498720918774,5.99439903315508));
#134258=CARTESIAN_POINT('Ctrl Pts',(18.1731820964075,15.524889787163,6.01964515254271));
#134259=CARTESIAN_POINT('Ctrl Pts',(18.1760889395079,15.5010100139497,6.04377709762875));
#134260=CARTESIAN_POINT('Ctrl Pts',(18.1789472914065,15.4754719407094,6.06629093511547));
#134261=CARTESIAN_POINT('Ctrl Pts',(18.1817788165681,15.4485123983593,6.08695637872067));
#134262=CARTESIAN_POINT('Ctrl Pts',(18.184610023612,15.4215558848736,6.10761950059419));
#134263=CARTESIAN_POINT('Ctrl Pts',(18.1874148502887,15.393177972699,6.12643415537824));
#134264=CARTESIAN_POINT('Ctrl Pts',(18.1902341341642,15.3636490638303,6.14319609094456));
#134265=CARTESIAN_POINT('Ctrl Pts',(18.1928660235342,15.3360829070351,6.15884388023692));
#134266=CARTESIAN_POINT('Ctrl Pts',(18.1955111969388,15.307513215976,6.17270255698526));
#134267=CARTESIAN_POINT('Ctrl Pts',(18.1982110692341,15.27819089864,6.18463367103899));
#134268=CARTESIAN_POINT('Ctrl Pts',(18.198405389526,15.2760804576117,6.18549239964232));
#134269=CARTESIAN_POINT('Ctrl Pts',(18.1985999931712,15.2739661059831,6.18634116207877));
#134270=CARTESIAN_POINT('Ctrl Pts',(18.1987948956111,15.2718479315203,6.18717991544739));
#134271=CARTESIAN_POINT('Ctrl Pts',(18.199195287804,15.2674965210454,6.18890298418335));
#134272=CARTESIAN_POINT('Ctrl Pts',(18.1995969446575,15.2631290938655,6.19058378968675));
#134273=CARTESIAN_POINT('Ctrl Pts',(18.2,15.2587465130648,6.19222196005096));
#134274=CARTESIAN_POINT('Ctrl Pts',(17.923341485608,14.2610000854617,5.49964459555407));
#134275=CARTESIAN_POINT('Ctrl Pts',(17.9225815974421,14.2609956726983,5.50882014690639));
#134276=CARTESIAN_POINT('Ctrl Pts',(17.9218174632575,14.2611621479354,5.5179946088016));
#134277=CARTESIAN_POINT('Ctrl Pts',(17.9203821612323,14.2617915619612,5.5351068011193));
#134278=CARTESIAN_POINT('Ctrl Pts',(17.9197123156157,14.2622118728923,5.54304480225922));
#134279=CARTESIAN_POINT('Ctrl Pts',(17.9183512131026,14.2633194823334,5.5590641664964));
#134280=CARTESIAN_POINT('Ctrl Pts',(17.9176598927818,14.2640119385344,5.5671440470472));
#134281=CARTESIAN_POINT('Ctrl Pts',(17.9162760949469,14.2656539206357,5.5831939763794));
#134282=CARTESIAN_POINT('Ctrl Pts',(17.9155837976166,14.2666006122747,5.59116319934));
#134283=CARTESIAN_POINT('Ctrl Pts',(17.9137274759009,14.2694695281316,5.61236051175744));
#134284=CARTESIAN_POINT('Ctrl Pts',(17.9125565197848,14.2716210926636,5.62555385800917));
#134285=CARTESIAN_POINT('Ctrl Pts',(17.9079979409858,14.2812957517057,5.67619215007037));
#134286=CARTESIAN_POINT('Ctrl Pts',(17.9045372590169,14.2913553792326,5.71307023382596));
#134287=CARTESIAN_POINT('Ctrl Pts',(17.9010383741602,14.3042076641721,5.74898599439144));
#134288=CARTESIAN_POINT('Origin',(16.125,15.,5.5));
#134289=CARTESIAN_POINT('',(18.1999858262452,15.63646577564,4.77232089562845));
#134290=CARTESIAN_POINT('Ctrl Pts',(18.0542644868187,14.0332501467026,5.49946741256401));
#134291=CARTESIAN_POINT('Ctrl Pts',(18.057199765697,14.0332748136958,5.45469201895388));
#134292=CARTESIAN_POINT('Ctrl Pts',(18.0601350445753,14.0364143245651,5.41002345185869));
#134293=CARTESIAN_POINT('Ctrl Pts',(18.0630703234536,14.0425996866789,5.3658724392504));
#134294=CARTESIAN_POINT('Ctrl Pts',(18.0660254309054,14.0488268325252,5.32142317504943));
#134295=CARTESIAN_POINT('Ctrl Pts',(18.0689805383573,14.0581409715527,5.27749883510395));
#134296=CARTESIAN_POINT('Ctrl Pts',(18.0719356458091,14.0704217023092,5.23450093980893));
#134297=CARTESIAN_POINT('Ctrl Pts',(18.0744302810105,14.0807888188164,5.19820308433721));
#134298=CARTESIAN_POINT('Ctrl Pts',(18.0769249162119,14.0932691063426,5.16256523878398));
#134299=CARTESIAN_POINT('Ctrl Pts',(18.0794195514133,14.1077639963729,5.12781660927507));
#134300=CARTESIAN_POINT('Ctrl Pts',(18.0820953694329,14.123311635528,5.09054422213671));
#134301=CARTESIAN_POINT('Ctrl Pts',(18.0847711874525,14.1412341479741,5.05416295996415));
#134302=CARTESIAN_POINT('Ctrl Pts',(18.0874470054721,14.1614073125235,5.01899286178791));
#134303=CARTESIAN_POINT('Ctrl Pts',(18.0901187885368,14.181550057288,4.98387579777091));
#134304=CARTESIAN_POINT('Ctrl Pts',(18.0927905716015,14.2039364576989,4.94996678884093));
#134305=CARTESIAN_POINT('Ctrl Pts',(18.0954623546662,14.2283949697251,4.91756439003576));
#134306=CARTESIAN_POINT('Ctrl Pts',(18.0981313920739,14.2528283469689,4.88519528954568));
#134307=CARTESIAN_POINT('Ctrl Pts',(18.1008004294816,14.2793292742131,4.85433020017197));
#134308=CARTESIAN_POINT('Ctrl Pts',(18.1034694668893,14.3076828035228,4.8252389593627));
#134309=CARTESIAN_POINT('Ctrl Pts',(18.1061370431678,14.3360208110682,4.79616364416803));
#134310=CARTESIAN_POINT('Ctrl Pts',(18.1088046194463,14.366209006091,4.76886067145898));
#134311=CARTESIAN_POINT('Ctrl Pts',(18.1114721957247,14.3979940771723,4.7435646548578));
#134312=CARTESIAN_POINT('Ctrl Pts',(18.1141415978985,14.4298009044114,4.71825132370897));
#134313=CARTESIAN_POINT('Ctrl Pts',(18.1168110000722,14.4632063406363,4.69494806480106));
#134314=CARTESIAN_POINT('Ctrl Pts',(18.119480402246,14.4979240827197,4.67384908413343));
#134315=CARTESIAN_POINT('Ctrl Pts',(18.1221505771933,14.5326518753514,4.65274399545559));
#134316=CARTESIAN_POINT('Ctrl Pts',(18.1248207521407,14.5686922188595,4.63384473813471));
#134317=CARTESIAN_POINT('Ctrl Pts',(18.127490927088,14.605733371958,4.61729994419824));
#134318=CARTESIAN_POINT('Ctrl Pts',(18.1301663774595,14.6428477067007,4.60072246296345));
#134319=CARTESIAN_POINT('Ctrl Pts',(18.132841827831,14.6809662559188,4.5865089510119));
#134320=CARTESIAN_POINT('Ctrl Pts',(18.1355172782025,14.7197581761722,4.57475944604785));
#134321=CARTESIAN_POINT('Ctrl Pts',(18.137824033639,14.7532043106584,4.56462910136252));
#134322=CARTESIAN_POINT('Ctrl Pts',(18.1401307890754,14.7871505220092,4.55632967343333));
#134323=CARTESIAN_POINT('Ctrl Pts',(18.1424375445119,14.8213793569691,4.54989462248485));
#134324=CARTESIAN_POINT('Ctrl Pts',(18.1450794771382,14.8605817251136,4.54252454294207));
#134325=CARTESIAN_POINT('Ctrl Pts',(18.1477214097645,14.9003400967497,4.53756637294437));
#134326=CARTESIAN_POINT('Ctrl Pts',(18.1503633423907,14.9403264071641,4.53509346316959));
#134327=CARTESIAN_POINT('Ctrl Pts',(18.153001353725,14.9802533678442,4.53262422381442));
#134328=CARTESIAN_POINT('Ctrl Pts',(18.1556393650593,15.0204070062996,4.5326329975251));
#134329=CARTESIAN_POINT('Ctrl Pts',(18.1582773763936,15.0604508144803,4.53514184382954));
#134330=CARTESIAN_POINT('Ctrl Pts',(18.1609128218753,15.1004556741906,4.53764824991336));
#134331=CARTESIAN_POINT('Ctrl Pts',(18.1635482673571,15.1403503188792,4.54264988585039));
#134332=CARTESIAN_POINT('Ctrl Pts',(18.1661837128388,15.1797982127067,4.55011676232945));
#134333=CARTESIAN_POINT('Ctrl Pts',(18.1688179428531,15.2192279131654,4.55758019508506));
#134334=CARTESIAN_POINT('Ctrl Pts',(18.1714521728674,15.2582106825453,4.56750650590994));
#134335=CARTESIAN_POINT('Ctrl Pts',(18.1740864028817,15.2964183852975,4.57981431039294));
#134336=CARTESIAN_POINT('Ctrl Pts',(18.1767224548429,15.3346525141424,4.59213062748356));
#134337=CARTESIAN_POINT('Ctrl Pts',(18.1793585068041,15.3721099340013,4.60683154494961));
#134338=CARTESIAN_POINT('Ctrl Pts',(18.1819945587653,15.4084785178229,4.62378606323728));
#134339=CARTESIAN_POINT('Ctrl Pts',(18.1846317349793,15.4448626125227,4.64074781247653));
#134340=CARTESIAN_POINT('Ctrl Pts',(18.1872689111933,15.4801564184663,4.65996479166206));
#134341=CARTESIAN_POINT('Ctrl Pts',(18.1899060874073,15.5140723338457,4.68125999360335));
#134342=CARTESIAN_POINT('Ctrl Pts',(18.192547721285,15.5480455778733,4.70259119118638));
#134343=CARTESIAN_POINT('Ctrl Pts',(18.1951893551628,15.5806358017996,4.72600726524789));
#134344=CARTESIAN_POINT('Ctrl Pts',(18.1978309890405,15.6115864189532,4.75128936520711));
#134345=CARTESIAN_POINT('Ctrl Pts',(18.1985492681088,15.6200021122244,4.75816374827521));
#134346=CARTESIAN_POINT('Ctrl Pts',(18.199267547177,15.6282967904242,4.7651758787105));
#134347=CARTESIAN_POINT('Ctrl Pts',(18.1999858262452,15.63646577564,4.77232089562845));
#134348=CARTESIAN_POINT('',(18.2,14.8153312661022,4.55105162352181));
#134349=CARTESIAN_POINT('Origin',(18.2,15.,5.5));
#134350=CARTESIAN_POINT('Ctrl Pts',(18.2,14.8153312661022,4.55105162352181));
#134351=CARTESIAN_POINT('Ctrl Pts',(18.1972671579687,14.7745953964148,4.55897896885046));
#134352=CARTESIAN_POINT('Ctrl Pts',(18.1945343159374,14.7343346850379,4.56954063396579));
#134353=CARTESIAN_POINT('Ctrl Pts',(18.1918014739061,14.6948998275967,4.58265630906431));
#134354=CARTESIAN_POINT('Ctrl Pts',(18.1890702629705,14.6554885068346,4.59576415607738));
#134355=CARTESIAN_POINT('Ctrl Pts',(18.1863390520349,14.6169025808847,4.61142281906072));
#134356=CARTESIAN_POINT('Ctrl Pts',(18.1836078410993,14.5794777686934,4.62950208760912));
#134357=CARTESIAN_POINT('Ctrl Pts',(18.1808772139826,14.5420609563654,4.64757749156423));
#134358=CARTESIAN_POINT('Ctrl Pts',(18.178146586866,14.5058052572839,4.6680722364678));
#134359=CARTESIAN_POINT('Ctrl Pts',(18.1754159597493,14.4710241480299,4.69080897772373));
#134360=CARTESIAN_POINT('Ctrl Pts',(18.1726848705559,14.4362371531159,4.71354956649145));
#134361=CARTESIAN_POINT('Ctrl Pts',(18.1699537813624,14.402925699129,4.73853260300311));
#134362=CARTESIAN_POINT('Ctrl Pts',(18.167222692169,14.3713742597232,4.76553744740701));
#134363=CARTESIAN_POINT('Ctrl Pts',(18.1644876254829,14.3397768695595,4.79258162101713));
#134364=CARTESIAN_POINT('Ctrl Pts',(18.1617525587968,14.3099450268696,4.82165312352018));
#134365=CARTESIAN_POINT('Ctrl Pts',(18.1590174921107,14.2821287646877,4.85249212204697));
#134366=CARTESIAN_POINT('Ctrl Pts',(18.1562804141889,14.2542920477726,4.883353798081));
#134367=CARTESIAN_POINT('Ctrl Pts',(18.1535433362672,14.2284742061419,4.91598513157478));
#134368=CARTESIAN_POINT('Ctrl Pts',(18.1508062583454,14.2048846110525,4.95009357090598));
#134369=CARTESIAN_POINT('Ctrl Pts',(18.1480629990315,14.1812417414341,4.98427904042942));
#134370=CARTESIAN_POINT('Ctrl Pts',(18.1453197397175,14.1598374571409,5.01994781177225));
#134371=CARTESIAN_POINT('Ctrl Pts',(18.1425764804036,14.1408366890334,5.05678000091504));
#134372=CARTESIAN_POINT('Ctrl Pts',(18.140738797881,14.12810826074,5.08145352336108));
#134373=CARTESIAN_POINT('Ctrl Pts',(18.1389011153584,14.1164574565062,5.1066486149651));
#134374=CARTESIAN_POINT('Ctrl Pts',(18.1370634328358,14.1059216241396,5.13226446959972));
#134375=CARTESIAN_POINT('Ctrl Pts',(18.1341448700766,14.0891888710095,5.17294694791745));
#134376=CARTESIAN_POINT('Ctrl Pts',(18.1312263073175,14.0752047801112,5.21485093037565));
#134377=CARTESIAN_POINT('Ctrl Pts',(18.1283077445583,14.0641310269153,5.25760604851314));
#134378=CARTESIAN_POINT('Ctrl Pts',(18.1254081725836,14.0531293294803,5.30008296354149));
#134379=CARTESIAN_POINT('Ctrl Pts',(18.1225086006089,14.045000411785,5.34339961698888));
#134380=CARTESIAN_POINT('Ctrl Pts',(18.1196090286342,14.0398567688201,5.38717031366046));
#134381=CARTESIAN_POINT('Ctrl Pts',(18.117151479958,14.0354972450457,5.42426841593273));
#134382=CARTESIAN_POINT('Ctrl Pts',(18.1146939312818,14.0332814876152,5.46169218001169));
#134383=CARTESIAN_POINT('Ctrl Pts',(18.1122363826056,14.0332503335345,5.49919695023161));
#134384=CARTESIAN_POINT('Ctrl Pts',(13.8510043077487,14.6757204956766,6.16261990718442));
#134385=CARTESIAN_POINT('Ctrl Pts',(13.8720142555048,14.4570381267508,6.05560288018805));
#134386=CARTESIAN_POINT('Ctrl Pts',(13.9140302009604,14.1375601906771,5.61006110330474));
#134387=CARTESIAN_POINT('Ctrl Pts',(13.9770521441157,14.4351930444452,4.83797560757758));
#134388=CARTESIAN_POINT('Ctrl Pts',(14.0400701372144,15.2432695205923,4.66524858954316));
#134389=CARTESIAN_POINT('Ctrl Pts',(14.103088130313,15.8314236186915,5.24489867692567));
#134390=CARTESIAN_POINT('Ctrl Pts',(14.1661061234117,15.6694783302998,6.05523004482602));
#134391=CARTESIAN_POINT('Ctrl Pts',(14.2291241165104,14.9032753408017,6.36426544000879));
#134392=CARTESIAN_POINT('Ctrl Pts',(14.292142109609,14.2244118963622,5.89348843559075));
#134393=CARTESIAN_POINT('Ctrl Pts',(14.3551601027077,14.2454329761124,5.06755325204506));
#134394=CARTESIAN_POINT('Ctrl Pts',(14.4181780958064,14.9474094818699,4.63190231135811));
#134395=CARTESIAN_POINT('Ctrl Pts',(14.481196088905,15.6968379606444,4.97962926523951));
#134396=CARTESIAN_POINT('Ctrl Pts',(14.5442140820037,15.817424801238,5.79696136639344));
#134397=CARTESIAN_POINT('Ctrl Pts',(14.6072320751024,15.2003436632176,6.34630312821531));
#134398=CARTESIAN_POINT('Ctrl Pts',(14.670250068201,14.4024679858008,6.13192048352086));
#134399=CARTESIAN_POINT('Ctrl Pts',(14.7332680612997,14.1438207552115,5.34727465160558));
#134400=CARTESIAN_POINT('Ctrl Pts',(14.7962860543983,14.6578129302989,4.7004528760265));
#134401=CARTESIAN_POINT('Ctrl Pts',(14.859304047497,15.480603779217,4.77516359700903));
#134402=CARTESIAN_POINT('Ctrl Pts',(14.9223220405957,15.8696849336051,5.50398631841823));
#134403=CARTESIAN_POINT('Ctrl Pts',(14.9853400336943,15.4739390057675,6.22921159789105));
#134404=CARTESIAN_POINT('Ctrl Pts',(15.048358026793,14.6504978046365,6.29637678311753));
#134405=CARTESIAN_POINT('Ctrl Pts',(15.1113760198917,14.1424567647499,5.64487014355418));
#134406=CARTESIAN_POINT('Ctrl Pts',(15.1743940129904,14.4082857825444,4.86262880555434));
#134407=CARTESIAN_POINT('Ctrl Pts',(15.237412006089,15.2080936039251,4.65556835048665));
#134408=CARTESIAN_POINT('Ctrl Pts',(15.3004299991877,15.8201121680078,5.21054570412811));
#134409=CARTESIAN_POINT('Ctrl Pts',(15.3634479922863,15.6920394790885,6.02673438894278));
#134410=CARTESIAN_POINT('Ctrl Pts',(15.426465985385,14.9394517732209,6.36758381144615));
#134411=CARTESIAN_POINT('Ctrl Pts',(15.4894839784837,14.2415044136345,5.92550229484266));
#134412=CARTESIAN_POINT('Ctrl Pts',(15.5525019715823,14.2280438479273,5.09943607663833));
#134413=CARTESIAN_POINT('Ctrl Pts',(15.615519964681,14.9112172520766,4.63484950374971));
#134414=CARTESIAN_POINT('Ctrl Pts',(15.6785379577797,15.6745105930848,4.95099798062628));
#134415=CARTESIAN_POINT('Ctrl Pts',(15.7415559508783,15.8291074544448,5.76258062846155));
#134416=CARTESIAN_POINT('Ctrl Pts',(15.804573943977,15.2354954753046,6.33720346307143));
#134417=CARTESIAN_POINT('Ctrl Pts',(15.8675919370757,14.429366052762,6.15631140148769));
#134418=CARTESIAN_POINT('Ctrl Pts',(15.9306099301743,14.1381920340439,5.38314629968156));
#134419=CARTESIAN_POINT('Ctrl Pts',(15.993627923273,14.624736675904,4.71543311626554));
#134420=CARTESIAN_POINT('Ctrl Pts',(16.0566459163717,15.4499290227168,4.75573416578379));
#134421=CARTESIAN_POINT('Ctrl Pts',(16.1196639094703,15.8690933322795,5.46768069848062));
#134422=CARTESIAN_POINT('Ctrl Pts',(16.182681902569,15.503964470976,6.20879303711113));
#134423=CARTESIAN_POINT('Ctrl Pts',(16.2456998956676,14.6840445322729,6.31027149763592));
#134424=CARTESIAN_POINT('Ctrl Pts',(16.3087178887663,14.1492512956584,5.68053919109209));
#134425=CARTESIAN_POINT('Ctrl Pts',(16.371735881865,14.3821965448323,4.88788346841236));
#134426=CARTESIAN_POINT('Ctrl Pts',(16.4347538749637,15.1726642289878,4.64761814805864));
#134427=CARTESIAN_POINT('Ctrl Pts',(16.4977718680623,15.8073150743269,5.17656510981916));
#134428=CARTESIAN_POINT('Ctrl Pts',(16.560789861161,15.713423108475,5.99738840531947));
#134429=CARTESIAN_POINT('Ctrl Pts',(16.6238078542597,14.9757189636257,6.36935504192598));
#134430=CARTESIAN_POINT('Ctrl Pts',(16.6868258473583,14.2599266785039,5.95679233347536));
#134431=CARTESIAN_POINT('Ctrl Pts',(16.749843840457,14.2119964400548,5.13200795249525));
#134432=CARTESIAN_POINT('Ctrl Pts',(16.8128618335556,14.8751817842497,4.63930947971334));
#134433=CARTESIAN_POINT('Ctrl Pts',(16.8758798266543,15.6510064380201,4.92332125728043));
#134434=CARTESIAN_POINT('Ctrl Pts',(16.938897819753,15.8393453960448,5.72774341912552));
#134435=CARTESIAN_POINT('Ctrl Pts',(17.0019158128517,15.2702365143165,6.32664381179715));
#134436=CARTESIAN_POINT('Ctrl Pts',(17.0649338059503,14.4572589533998,6.17955860087412));
#134437=CARTESIAN_POINT('Ctrl Pts',(17.127951799049,14.1340654717869,5.41922149219832));
#134438=CARTESIAN_POINT('Ctrl Pts',(17.1909697921477,14.5923146135604,4.73178100167847));
#134439=CARTESIAN_POINT('Ctrl Pts',(17.2539877852463,15.4184699182281,4.73760212378108));
#134440=CARTESIAN_POINT('Ctrl Pts',(17.317005778345,15.866986886601,5.43143127746081));
#134441=CARTESIAN_POINT('Ctrl Pts',(17.3800237714436,15.5331112858198,6.18713925984319));
#134442=CARTESIAN_POINT('Ctrl Pts',(17.4430417645423,14.7181423454594,6.32275320163177));
#134443=CARTESIAN_POINT('Ctrl Pts',(17.506059757641,14.1575281433043,5.71589471852043));
#134444=CARTESIAN_POINT('Ctrl Pts',(17.5690777507396,14.3571854776964,4.91420282101584));
#134445=CARTESIAN_POINT('Ctrl Pts',(17.6320957438383,15.1369314259542,4.64115825426989));
#134446=CARTESIAN_POINT('Ctrl Pts',(17.695113736937,15.7931155014792,5.1431395445431));
#134447=CARTESIAN_POINT('Ctrl Pts',(17.7581317300356,15.7335538507685,5.96719246940726));
#134448=CARTESIAN_POINT('Ctrl Pts',(17.8211497231343,15.0120465880597,6.36957765047564));
#134449=CARTESIAN_POINT('Ctrl Pts',(17.884167716233,14.279603718542,5.98735083367125));
#134450=CARTESIAN_POINT('Ctrl Pts',(17.9471857093316,14.1973913188042,5.16509520215214));
#134451=CARTESIAN_POINT('Ctrl Pts',(18.0102037024303,14.8392299862402,4.6455159570919));
#134452=CARTESIAN_POINT('Ctrl Pts',(18.073221695529,15.6266295424263,4.89616342462223));
#134453=CARTESIAN_POINT('Ctrl Pts',(18.1362428391242,15.8476078068145,5.69356706237978));
#134454=CARTESIAN_POINT('Ctrl Pts',(18.1782579850199,15.4862513157781,6.10585161173504));
#134455=CARTESIAN_POINT('Ctrl Pts',(18.1992671332161,15.2581937444145,6.19105595229305));
#134456=CARTESIAN_POINT('Ctrl Pts',(13.8957032291166,14.6416883768802,6.23215979205983));
#134457=CARTESIAN_POINT('Ctrl Pts',(13.9167131768727,14.4000559779379,6.11391166310539));
#134458=CARTESIAN_POINT('Ctrl Pts',(13.9587291223284,14.0470498326241,5.62161167154166));
#134459=CARTESIAN_POINT('Ctrl Pts',(14.0217510654837,14.3759183226323,4.76849822011212));
#134460=CARTESIAN_POINT('Ctrl Pts',(14.0847690585823,15.2687998952042,4.57764404227048));
#134461=CARTESIAN_POINT('Ctrl Pts',(14.147787051681,15.9186789246364,5.21812659168372));
#134462=CARTESIAN_POINT('Ctrl Pts',(14.2108050447797,15.7397379852103,6.11349969983931));
#134463=CARTESIAN_POINT('Ctrl Pts',(14.2738230378784,14.8931243906229,6.45496739228697));
#134464=CARTESIAN_POINT('Ctrl Pts',(14.336841030977,14.1430163529249,5.93478381505961));
#134465=CARTESIAN_POINT('Ctrl Pts',(14.3998590240757,14.1662435291866,5.02216931965564));
#134466=CARTESIAN_POINT('Ctrl Pts',(14.4628770171744,14.941890271631,4.54079817658305));
#134467=CARTESIAN_POINT('Ctrl Pts',(14.525895010273,15.7699689231081,4.92501798568779));
#134468=CARTESIAN_POINT('Ctrl Pts',(14.5889130033717,15.9032109751155,5.82812653213556));
#134469=CARTESIAN_POINT('Ctrl Pts',(14.6519309964703,15.2213691034807,6.43511999210321));
#134470=CARTESIAN_POINT('Ctrl Pts',(14.714948989569,14.3397588715313,6.19823855998974));
#134471=CARTESIAN_POINT('Ctrl Pts',(14.7779669826677,14.0539674238071,5.33124660441028));
#134472=CARTESIAN_POINT('Ctrl Pts',(14.8409849757663,14.6219014685772,4.61654290841046));
#134473=CARTESIAN_POINT('Ctrl Pts',(14.904002968865,15.531041641278,4.69909428567233));
#134474=CARTESIAN_POINT('Ctrl Pts',(14.9670209619637,15.96095564477,5.50440467005673));
#134475=CARTESIAN_POINT('Ctrl Pts',(15.0300389550623,15.5236774207196,6.30574007223561));
#134476=CARTESIAN_POINT('Ctrl Pts',(15.093056948161,14.6138186433772,6.37995403338573));
#134477=CARTESIAN_POINT('Ctrl Pts',(15.1560749412596,14.0524602868168,5.66007381159285));
#134478=CARTESIAN_POINT('Ctrl Pts',(15.2190929343583,14.3461872278302,4.79573869403778));
#134479=CARTESIAN_POINT('Ctrl Pts',(15.282110927457,15.2299323762038,4.56694789242973));
#134480=CARTESIAN_POINT('Ctrl Pts',(15.3451289205557,15.9061803726147,5.18016838193572));
#134481=CARTESIAN_POINT('Ctrl Pts',(15.4081469136543,15.764666855935,6.08201351407901));
#134482=CARTESIAN_POINT('Ctrl Pts',(15.471164906753,14.9330974263714,6.45863401641825));
#134483=CARTESIAN_POINT('Ctrl Pts',(15.5341828998516,14.1619026763754,5.9701574286181));
#134484=CARTESIAN_POINT('Ctrl Pts',(15.5972008929503,14.1470294664366,5.05739814687831));
#134485=CARTESIAN_POINT('Ctrl Pts',(15.660218886049,14.9018997806234,4.54405466758972));
#134486=CARTESIAN_POINT('Ctrl Pts',(15.7232368791476,15.7452983682207,4.8933819373869));
#134487=CARTESIAN_POINT('Ctrl Pts',(15.7862548722463,15.9161196862029,5.79013764338932));
#134488=CARTESIAN_POINT('Ctrl Pts',(15.849272865345,15.2602099882008,6.42506534558968));
#134489=CARTESIAN_POINT('Ctrl Pts',(15.9122908584437,14.3694798064137,6.22518922843951));
#134490=CARTESIAN_POINT('Ctrl Pts',(15.9753088515423,14.0477479859742,5.37088286965281));
#134491=CARTESIAN_POINT('Ctrl Pts',(16.038326844641,14.5853539648314,4.63309527796577));
#134492=CARTESIAN_POINT('Ctrl Pts',(16.1013448377396,15.4971476651128,4.67762579646536));
#134493=CARTESIAN_POINT('Ctrl Pts',(16.1643628308383,15.9603019567375,5.46428888896427));
#134494=CARTESIAN_POINT('Ctrl Pts',(16.227380823937,15.5568539645045,6.28317864742375));
#134495=CARTESIAN_POINT('Ctrl Pts',(16.2903988170356,14.6508859950583,6.39530695469434));
#134496=CARTESIAN_POINT('Ctrl Pts',(16.3534168101343,14.0599678824732,5.6994862140051));
#134497=CARTESIAN_POINT('Ctrl Pts',(16.416434803233,14.3173600062946,4.82364375470104));
#134498=CARTESIAN_POINT('Ctrl Pts',(16.4794527963316,15.1907847992811,4.55816334114562));
#134499=CARTESIAN_POINT('Ctrl Pts',(16.5424707894303,15.8920402640143,5.14262163063297));
#134500=CARTESIAN_POINT('Ctrl Pts',(16.605488782529,15.7882946302824,6.04958776134433));
#134501=CARTESIAN_POINT('Ctrl Pts',(16.6685067756276,14.973170744872,6.46059113199196));
#134502=CARTESIAN_POINT('Ctrl Pts',(16.7315247687263,14.1822583002706,6.00473125884937));
#134503=CARTESIAN_POINT('Ctrl Pts',(16.794542761825,14.1292979333455,5.09338833913761));
#134504=CARTESIAN_POINT('Ctrl Pts',(16.8575607549236,14.8620825032599,4.54898270406844));
#134505=CARTESIAN_POINT('Ctrl Pts',(16.9205787480223,15.7193275256635,4.86280062857004));
#134506=CARTESIAN_POINT('Ctrl Pts',(16.9835967411209,15.9274320677232,5.75164437799412));
#134507=CARTESIAN_POINT('Ctrl Pts',(17.0466147342196,15.2985969904974,6.41339749197198));
#134508=CARTESIAN_POINT('Ctrl Pts',(17.1096327273182,14.4002999796526,6.25087614862437));
#134509=CARTESIAN_POINT('Ctrl Pts',(17.172650720417,14.0431883539269,5.41074404068799));
#134510=CARTESIAN_POINT('Ctrl Pts',(17.2356687135156,14.5495293085446,4.65115882277445));
#134511=CARTESIAN_POINT('Ctrl Pts',(17.2986867066143,15.4623870260932,4.65759085341827));
#134512=CARTESIAN_POINT('Ctrl Pts',(17.361704699713,15.9579744461793,5.42423520469007));
#134513=CARTESIAN_POINT('Ctrl Pts',(17.4247226928116,15.5890596463198,6.25925237402038));
#134514=CARTESIAN_POINT('Ctrl Pts',(17.4877406859102,14.6885622669929,6.40909857444962));
#134515=CARTESIAN_POINT('Ctrl Pts',(17.550758679009,14.0691133593682,5.73855219335379));
#134516=CARTESIAN_POINT('Ctrl Pts',(17.6137766721076,14.289724105962,4.85272524096548));
#134517=CARTESIAN_POINT('Ctrl Pts',(17.6767946652063,15.1513019504334,4.55102550172695));
#134518=CARTESIAN_POINT('Ctrl Pts',(17.739812658305,15.876350490449,5.10568815692254));
#134519=CARTESIAN_POINT('Ctrl Pts',(17.8028306514036,15.8105380309588,6.01622285648888));
#134520=CARTESIAN_POINT('Ctrl Pts',(17.8658486445023,15.0133108397638,6.46083710261201));
#134521=CARTESIAN_POINT('Ctrl Pts',(17.9288666376009,14.20400038406,6.03849677797505));
#134522=CARTESIAN_POINT('Ctrl Pts',(17.9918846306996,14.1131600503421,5.12994799206374));
#134523=CARTESIAN_POINT('Ctrl Pts',(18.0549026237983,14.8223576765992,4.55584053181802));
#134524=CARTESIAN_POINT('Ctrl Pts',(18.1179206168969,15.6923923511911,4.83279266639408));
#134525=CARTESIAN_POINT('Ctrl Pts',(18.1809417604922,15.936561592637,5.71388131959968));
#134526=CARTESIAN_POINT('Ctrl Pts',(18.2229569063879,15.5372818691211,6.16943384172064));
#134527=CARTESIAN_POINT('Ctrl Pts',(18.243966054584,15.2852903695951,6.26358011108135));
#134528=CARTESIAN_POINT('Ctrl Pts',(13.9404021504847,14.6076562580839,6.30169967693524));
#134529=CARTESIAN_POINT('Ctrl Pts',(13.9614120982408,14.3430738291251,6.17222044602273));
#134530=CARTESIAN_POINT('Ctrl Pts',(14.0034280436965,13.956539474571,5.63316223977858));
#134531=CARTESIAN_POINT('Ctrl Pts',(14.0664499868517,14.3166436008192,4.69902083264669));
#134532=CARTESIAN_POINT('Ctrl Pts',(14.1294679799503,15.2943302698161,4.49003949499779));
#134533=CARTESIAN_POINT('Ctrl Pts',(14.192485973049,16.0059342305812,5.19135450644176));
#134534=CARTESIAN_POINT('Ctrl Pts',(14.2555039661476,15.8099976401209,6.1717693548526));
#134535=CARTESIAN_POINT('Ctrl Pts',(14.3185219592463,14.8829734404442,6.54566934456515));
#134536=CARTESIAN_POINT('Ctrl Pts',(14.381539952345,14.0616208094874,5.97607919452845));
#134537=CARTESIAN_POINT('Ctrl Pts',(14.4445579454437,14.0870540822609,4.97678538726625));
#134538=CARTESIAN_POINT('Ctrl Pts',(14.5075759385423,14.9363710613919,4.44969404180798));
#134539=CARTESIAN_POINT('Ctrl Pts',(14.570593931641,15.8430998855718,4.87040670613608));
#134540=CARTESIAN_POINT('Ctrl Pts',(14.6336119247396,15.988997148993,5.85929169787771));
#134541=CARTESIAN_POINT('Ctrl Pts',(14.6966299178383,15.242394543744,6.52393685599109));
#134542=CARTESIAN_POINT('Ctrl Pts',(14.759647910937,14.277049757262,6.26455663645863));
#134543=CARTESIAN_POINT('Ctrl Pts',(14.8226659040356,13.9641140924029,5.31521855721497));
#134544=CARTESIAN_POINT('Ctrl Pts',(14.8856838971343,14.5859900068555,4.53263294079442));
#134545=CARTESIAN_POINT('Ctrl Pts',(14.948701890233,15.581479503339,4.62302497433563));
#134546=CARTESIAN_POINT('Ctrl Pts',(15.0117198833317,16.052226355935,5.50482302169524));
#134547=CARTESIAN_POINT('Ctrl Pts',(15.0747378764303,15.5734158356716,6.38226854658017));
#134548=CARTESIAN_POINT('Ctrl Pts',(15.137755869529,14.5771394821179,6.46353128365394));
#134549=CARTESIAN_POINT('Ctrl Pts',(15.2007738626276,13.9624638088836,5.67527747963153));
#134550=CARTESIAN_POINT('Ctrl Pts',(15.2637918557263,14.284088673116,4.72884858252123));
#134551=CARTESIAN_POINT('Ctrl Pts',(15.326809848825,15.2517711484823,4.47832743437281));
#134552=CARTESIAN_POINT('Ctrl Pts',(15.3898278419236,15.9922485772217,5.14979105974335));
#134553=CARTESIAN_POINT('Ctrl Pts',(15.4528458350223,15.8372942327814,6.13729263921524));
#134554=CARTESIAN_POINT('Ctrl Pts',(15.5158638281209,14.9267430795219,6.54968422139037));
#134555=CARTESIAN_POINT('Ctrl Pts',(15.5788818212196,14.0823009391162,6.01481256239352));
#134556=CARTESIAN_POINT('Ctrl Pts',(15.6418998143183,14.0660150849458,5.01536021711829));
#134557=CARTESIAN_POINT('Ctrl Pts',(15.704917807417,14.8925823091702,4.45325983142974));
#134558=CARTESIAN_POINT('Ctrl Pts',(15.7679358005156,15.8160861433567,4.8357658941475));
#134559=CARTESIAN_POINT('Ctrl Pts',(15.8309537936143,16.0031319179609,5.81769465831711));
#134560=CARTESIAN_POINT('Ctrl Pts',(15.893971786713,15.284924501097,6.51292722810789));
#134561=CARTESIAN_POINT('Ctrl Pts',(15.9569897798116,14.3095935600653,6.29406705539134));
#134562=CARTESIAN_POINT('Ctrl Pts',(16.0200077729103,13.9573039379045,5.35861943962407));
#134563=CARTESIAN_POINT('Ctrl Pts',(16.083025766009,14.5459712537588,4.55075743966601));
#134564=CARTESIAN_POINT('Ctrl Pts',(16.1460437591076,15.5443663075088,4.59951742714692));
#134565=CARTESIAN_POINT('Ctrl Pts',(16.2090617522063,16.0515105811953,5.46089707944791));
#134566=CARTESIAN_POINT('Ctrl Pts',(16.272079745305,15.6097434580332,6.35756425773636));
#134567=CARTESIAN_POINT('Ctrl Pts',(16.3350977384036,14.6177274578437,6.48034241175276));
#134568=CARTESIAN_POINT('Ctrl Pts',(16.3981157315023,13.9706844692882,5.71843323691812));
#134569=CARTESIAN_POINT('Ctrl Pts',(16.461133724601,14.2525234677569,4.75940404098975));
#134570=CARTESIAN_POINT('Ctrl Pts',(16.5241517176996,15.2089053695745,4.46870853423261));
#134571=CARTESIAN_POINT('Ctrl Pts',(16.5871697107983,15.9767654537018,5.10867815144677));
#134572=CARTESIAN_POINT('Ctrl Pts',(16.6501877038969,15.8631661520898,6.10178711736918));
#134573=CARTESIAN_POINT('Ctrl Pts',(16.7132056969956,14.9706225261181,6.55182722205794));
#134574=CARTESIAN_POINT('Ctrl Pts',(16.7762236900943,14.1045899220371,6.05267018422339));
#134575=CARTESIAN_POINT('Ctrl Pts',(16.839241683193,14.0465994266362,5.05476872577994));
#134576=CARTESIAN_POINT('Ctrl Pts',(16.9022596762916,14.8489832222702,4.45865592842353));
#134577=CARTESIAN_POINT('Ctrl Pts',(16.9652776693903,15.787648613307,4.80227999985966));
#134578=CARTESIAN_POINT('Ctrl Pts',(17.0282956624889,16.0155187394014,5.77554533686269));
#134579=CARTESIAN_POINT('Ctrl Pts',(17.0913136555876,15.3269574666784,6.5001511721468));
#134580=CARTESIAN_POINT('Ctrl Pts',(17.1543316486863,14.3433410059052,6.3221936963746));
#134581=CARTESIAN_POINT('Ctrl Pts',(17.217349641785,13.952311236067,5.40226658917767));
#134582=CARTESIAN_POINT('Ctrl Pts',(17.2803676348836,14.5067440035288,4.57053664387043));
#134583=CARTESIAN_POINT('Ctrl Pts',(17.3433856279823,15.5063041339583,4.57757958305543));
#134584=CARTESIAN_POINT('Ctrl Pts',(17.4064036210809,16.0489620057577,5.41703913191933));
#134585=CARTESIAN_POINT('Ctrl Pts',(17.4694216141796,15.6450080068199,6.33136548819757));
#134586=CARTESIAN_POINT('Ctrl Pts',(17.5324396072783,14.6589821885264,6.49544394726743));
#134587=CARTESIAN_POINT('Ctrl Pts',(17.5954576003769,13.9806985754322,5.76120966818718));
#134588=CARTESIAN_POINT('Ctrl Pts',(17.6584755934756,14.2222627342275,4.7912476609151));
#134589=CARTESIAN_POINT('Ctrl Pts',(17.7214935865743,15.1656724749127,4.46089274918404));
#134590=CARTESIAN_POINT('Ctrl Pts',(17.7845115796729,15.9595854794191,5.06823676930197));
#134591=CARTESIAN_POINT('Ctrl Pts',(17.8475295727716,15.8875222111491,6.0652532435705));
#134592=CARTESIAN_POINT('Ctrl Pts',(17.9105475658703,15.0145750914678,6.5520965547484));
#134593=CARTESIAN_POINT('Ctrl Pts',(17.9735655589689,14.1283970495782,6.08964272227883));
#134594=CARTESIAN_POINT('Ctrl Pts',(18.0365835520676,14.0289287818801,5.09480078197536));
#134595=CARTESIAN_POINT('Ctrl Pts',(18.0996015451662,14.8054853669582,4.46616510654412));
#134596=CARTESIAN_POINT('Ctrl Pts',(18.1626195382649,15.7581551599557,4.76942190816593));
#134597=CARTESIAN_POINT('Ctrl Pts',(18.2256406818602,16.0255153784595,5.73419557681956));
#134598=CARTESIAN_POINT('Ctrl Pts',(18.2676558277559,15.5883124224641,6.23301607170624));
#134599=CARTESIAN_POINT('Ctrl Pts',(18.2886649759521,15.3123869947755,6.33610426986964));
#134600=CARTESIAN_POINT('Ctrl Pts',(13.9851010718527,14.5736241392876,6.37123956181065));
#134601=CARTESIAN_POINT('Ctrl Pts',(14.0061110196089,14.2860916803124,6.23052922894009));
#134602=CARTESIAN_POINT('Ctrl Pts',(14.0481269650644,13.8660291165181,5.64471280801549));
#134603=CARTESIAN_POINT('Ctrl Pts',(14.1111489082198,14.2573688790063,4.62954344518124));
#134604=CARTESIAN_POINT('Ctrl Pts',(14.1741669013184,15.3198606444279,4.4024349477251));
#134605=CARTESIAN_POINT('Ctrl Pts',(14.2371848944171,16.0931895365261,5.16458242119979));
#134606=CARTESIAN_POINT('Ctrl Pts',(14.3002028875157,15.8802572950314,6.23003900986589));
#134607=CARTESIAN_POINT('Ctrl Pts',(14.3632208806144,14.8728224902654,6.63637129684331));
#134608=CARTESIAN_POINT('Ctrl Pts',(14.426238873713,13.9802252660501,6.0173745739973));
#134609=CARTESIAN_POINT('Ctrl Pts',(14.4892568668117,14.0078646353351,4.93140145487682));
#134610=CARTESIAN_POINT('Ctrl Pts',(14.5522748599104,14.930851851153,4.35858990703292));
#134611=CARTESIAN_POINT('Ctrl Pts',(14.615292853009,15.9162308480355,4.81579542658434));
#134612=CARTESIAN_POINT('Ctrl Pts',(14.6783108461077,16.0747833228706,5.89045686361985));
#134613=CARTESIAN_POINT('Ctrl Pts',(14.7413288392064,15.263419984007,6.61275371987895));
#134614=CARTESIAN_POINT('Ctrl Pts',(14.8043468323051,14.2143406429926,6.33087471292751));
#134615=CARTESIAN_POINT('Ctrl Pts',(14.8673648254037,13.8742607609987,5.29919051001966));
#134616=CARTESIAN_POINT('Ctrl Pts',(14.9303828185024,14.5500785451338,4.4487229731784));
#134617=CARTESIAN_POINT('Ctrl Pts',(14.993400811601,15.6319173654,4.54695566299893));
#134618=CARTESIAN_POINT('Ctrl Pts',(15.0564188046997,16.1434970671,5.50524137333374));
#134619=CARTESIAN_POINT('Ctrl Pts',(15.1194367977984,15.6231542506237,6.45879702092473));
#134620=CARTESIAN_POINT('Ctrl Pts',(15.1824547908971,14.5404603208586,6.54710853392214));
#134621=CARTESIAN_POINT('Ctrl Pts',(15.2454727839957,13.8724673309506,5.6904811476702));
#134622=CARTESIAN_POINT('Ctrl Pts',(15.3084907770944,14.2219901184019,4.66195847100467));
#134623=CARTESIAN_POINT('Ctrl Pts',(15.371508770193,15.2736099207609,4.38970697631589));
#134624=CARTESIAN_POINT('Ctrl Pts',(15.4345267632917,16.0783167818286,5.11941373755096));
#134625=CARTESIAN_POINT('Ctrl Pts',(15.4975447563904,15.9099216096279,6.19257176435145));
#134626=CARTESIAN_POINT('Ctrl Pts',(15.560562749489,14.9203887326725,6.64073442636246));
#134627=CARTESIAN_POINT('Ctrl Pts',(15.6235807425877,14.002699201857,6.05946769616896));
#134628=CARTESIAN_POINT('Ctrl Pts',(15.6865987356864,13.9850007034551,4.97332228735827));
#134629=CARTESIAN_POINT('Ctrl Pts',(15.749616728785,14.8832648377169,4.36246499526975));
#134630=CARTESIAN_POINT('Ctrl Pts',(15.8126347218837,15.8868739184927,4.7781498509081));
#134631=CARTESIAN_POINT('Ctrl Pts',(15.8756527149824,16.090144149719,5.84525167324489));
#134632=CARTESIAN_POINT('Ctrl Pts',(15.938670708081,15.3096390139932,6.60078911062615));
#134633=CARTESIAN_POINT('Ctrl Pts',(16.0016887011797,14.2497073137171,6.36294488234316));
#134634=CARTESIAN_POINT('Ctrl Pts',(16.0647066942784,13.866859889835,5.34635600959533));
#134635=CARTESIAN_POINT('Ctrl Pts',(16.127724687377,14.5065885426861,4.46841960136624));
#134636=CARTESIAN_POINT('Ctrl Pts',(16.1907426804757,15.5915849499048,4.5214090578285));
#134637=CARTESIAN_POINT('Ctrl Pts',(16.2537606735744,16.1427192056532,5.45750526993156));
#134638=CARTESIAN_POINT('Ctrl Pts',(16.316778666673,15.6626329515618,6.43194986804897));
#134639=CARTESIAN_POINT('Ctrl Pts',(16.3797966597717,14.5845689206292,6.56537786881118));
#134640=CARTESIAN_POINT('Ctrl Pts',(16.4428146528704,13.881401056103,5.73738025983114));
#134641=CARTESIAN_POINT('Ctrl Pts',(16.505832645969,14.1876869292192,4.69516432727843));
#134642=CARTESIAN_POINT('Ctrl Pts',(16.5688506390677,15.2270259398679,4.37925372731961));
#134643=CARTESIAN_POINT('Ctrl Pts',(16.6318686321664,16.0614906433893,5.07473467226058));
#134644=CARTESIAN_POINT('Ctrl Pts',(16.694886625265,15.9380376738973,6.15398647339405));
#134645=CARTESIAN_POINT('Ctrl Pts',(16.7579046183637,14.9680743073643,6.64306331212394));
#134646=CARTESIAN_POINT('Ctrl Pts',(16.8209226114623,14.0269215438038,6.10060910959739));
#134647=CARTESIAN_POINT('Ctrl Pts',(16.883940604561,13.9639009199269,5.0161491124223));
#134648=CARTESIAN_POINT('Ctrl Pts',(16.9469585976597,14.8358839412804,4.36832915277863));
#134649=CARTESIAN_POINT('Ctrl Pts',(17.0099765907584,15.8559697009506,4.74175937114927));
#134650=CARTESIAN_POINT('Ctrl Pts',(17.072994583857,16.1036054110797,5.79944629573126));
#134651=CARTESIAN_POINT('Ctrl Pts',(17.1360125769557,15.3553179428593,6.58690485232163));
#134652=CARTESIAN_POINT('Ctrl Pts',(17.1990305700544,14.286382032158,6.39351124412484));
#134653=CARTESIAN_POINT('Ctrl Pts',(17.262048563153,13.861434118207,5.39378913766735));
#134654=CARTESIAN_POINT('Ctrl Pts',(17.3250665562517,14.463958698513,4.48991446496641));
#134655=CARTESIAN_POINT('Ctrl Pts',(17.3880845493504,15.5502212418235,4.49756831269261));
#134656=CARTESIAN_POINT('Ctrl Pts',(17.451102542449,16.139949565336,5.40984305914861));
#134657=CARTESIAN_POINT('Ctrl Pts',(17.5141205355477,15.7009563673201,6.40347860237476));
#134658=CARTESIAN_POINT('Ctrl Pts',(17.5771385286463,14.6294021100598,6.58178932008526));
#134659=CARTESIAN_POINT('Ctrl Pts',(17.640156521745,13.8922837914963,5.78386714302055));
#134660=CARTESIAN_POINT('Ctrl Pts',(17.7031745148437,14.154801362493,4.72977008086474));
#134661=CARTESIAN_POINT('Ctrl Pts',(17.7661925079424,15.180042999392,4.3707599966411));
#134662=CARTESIAN_POINT('Ctrl Pts',(17.829210501041,16.042820468389,5.03078538168141));
#134663=CARTESIAN_POINT('Ctrl Pts',(17.8922284941397,15.9645063913394,6.11428363065212));
#134664=CARTESIAN_POINT('Ctrl Pts',(17.9552464872383,15.0158393431718,6.64335600688478));
#134665=CARTESIAN_POINT('Ctrl Pts',(18.018264480337,14.0527937150962,6.14078866658263));
#134666=CARTESIAN_POINT('Ctrl Pts',(18.0812824734357,13.9446975134179,5.05965357188695));
#134667=CARTESIAN_POINT('Ctrl Pts',(18.1443004665343,14.7886130573173,4.37648968127024));
#134668=CARTESIAN_POINT('Ctrl Pts',(18.207318459633,15.8239179687204,4.70605114993779));
#134669=CARTESIAN_POINT('Ctrl Pts',(18.2703396032283,16.114469164282,5.75450983403944));
#134670=CARTESIAN_POINT('Ctrl Pts',(18.312354749124,15.6393429758072,6.29659830169184));
#134671=CARTESIAN_POINT('Ctrl Pts',(18.3333638973201,15.3394836199561,6.40862842865793));
#134672=CARTESIAN_POINT('',(14.0280374670081,14.0780374670081,5.50000000327438));
#134673=CARTESIAN_POINT('Ctrl Pts',(14.0280374670081,14.0780374670081,5.50000000654876));
#134674=CARTESIAN_POINT('Ctrl Pts',(14.0336707525267,14.0836707516792,5.38068063053235));
#134675=CARTESIAN_POINT('Ctrl Pts',(14.0394414468597,14.1127440757323,5.26304138084325));
#134676=CARTESIAN_POINT('Ctrl Pts',(14.0496371634471,14.2112191405822,5.05112665797812));
#134677=CARTESIAN_POINT('Ctrl Pts',(14.0540832508647,14.2782937417532,4.95704494172787));
#134678=CARTESIAN_POINT('Ctrl Pts',(14.0646664677378,14.4586721851121,4.78677377365687));
#134679=CARTESIAN_POINT('Ctrl Pts',(14.0701889998458,14.5559376608619,4.73662342738342));
#134680=CARTESIAN_POINT('Ctrl Pts',(14.0796677175689,14.7331134953084,4.66368605021134));
#134681=CARTESIAN_POINT('Ctrl Pts',(14.08506495303,14.84742847341,4.64092381676413));
#134682=CARTESIAN_POINT('Ctrl Pts',(14.0944011777295,15.0592500270387,4.6409810781504));
#134683=CARTESIAN_POINT('Ctrl Pts',(14.0984589285287,15.1558116203124,4.65722900890055));
#134684=CARTESIAN_POINT('Ctrl Pts',(14.108532644215,15.351725110515,4.7275697529941));
#134685=CARTESIAN_POINT('Ctrl Pts',(14.1145177155538,15.4478924506123,4.78605667147313));
#134686=CARTESIAN_POINT('Ctrl Pts',(14.1249265358644,15.6016864042129,4.92708381458633));
#134687=CARTESIAN_POINT('Ctrl Pts',(14.129415714943,15.6619331275998,5.00531324896704));
#134688=CARTESIAN_POINT('Ctrl Pts',(14.1386402801144,15.7544728653423,5.18408713983558));
#134689=CARTESIAN_POINT('Ctrl Pts',(14.1435958781485,15.7837880958418,5.28377178093206));
#134690=CARTESIAN_POINT('Ctrl Pts',(14.1545039313174,15.8014139214458,5.48546862399363));
#134691=CARTESIAN_POINT('Ctrl Pts',(14.1598505847911,15.7917261955478,5.58470225767358));
#134692=CARTESIAN_POINT('Ctrl Pts',(14.1696529264411,15.7378044704229,5.77166909773013));
#134693=CARTESIAN_POINT('Ctrl Pts',(14.1740949113336,15.6946341146314,5.85877380590229));
#134694=CARTESIAN_POINT('Ctrl Pts',(14.1851465525943,15.5609075800702,6.03474948161481));
#134695=CARTESIAN_POINT('Ctrl Pts',(14.1911371129321,15.4767337706299,6.09477078358694));
#134696=CARTESIAN_POINT('Ctrl Pts',(14.2007965388827,15.328712435131,6.1804779565484));
#134697=CARTESIAN_POINT('Ctrl Pts',(14.2060770183145,15.2336306819364,6.21318772401287));
#134698=CARTESIAN_POINT('Ctrl Pts',(14.2111576979006,15.1353877924827,6.22633194409867));
#134699=CARTESIAN_POINT('',(18.2,15.6465738458316,4.7812873840077));
#134700=CARTESIAN_POINT('Ctrl Pts',(18.2,15.6465738458316,4.78128738400769));
#134701=CARTESIAN_POINT('Ctrl Pts',(18.2,15.6619638572722,4.79851741080685));
#134702=CARTESIAN_POINT('Ctrl Pts',(18.2,15.6766698976115,4.81631464232827));
#134703=CARTESIAN_POINT('Ctrl Pts',(18.2,15.6906448654999,4.83466849716618));
#134704=CARTESIAN_POINT('Ctrl Pts',(18.2,15.7133028676804,4.8644261099392));
#134705=CARTESIAN_POINT('Ctrl Pts',(18.2,15.7340406678333,4.89564678969883));
#134706=CARTESIAN_POINT('Ctrl Pts',(18.2,15.752815722504,4.92811617435309));
#134707=CARTESIAN_POINT('Ctrl Pts',(18.2,15.7609364545188,4.94216008400264));
#134708=CARTESIAN_POINT('Ctrl Pts',(18.2,15.7686896018272,4.9564376928423));
#134709=CARTESIAN_POINT('Ctrl Pts',(18.2,15.7760699087929,4.97093183307526));
#134710=CARTESIAN_POINT('Ctrl Pts',(18.2,15.7809487495338,4.98051335891182));
#134711=CARTESIAN_POINT('Ctrl Pts',(18.2,15.7856650391499,4.99019075750296));
#134712=CARTESIAN_POINT('Ctrl Pts',(18.2,15.7902099091838,4.99994269671711));
#134713=CARTESIAN_POINT('Ctrl Pts',(18.2,15.8078416972689,5.03777526934493));
#134714=CARTESIAN_POINT('Ctrl Pts',(18.2,15.8229264746598,5.07678379042559));
#134715=CARTESIAN_POINT('Ctrl Pts',(18.2,15.8354041793666,5.11666566334121));
#134716=CARTESIAN_POINT('Ctrl Pts',(18.2,15.8426768939495,5.13991108271611));
#134717=CARTESIAN_POINT('Ctrl Pts',(18.2,15.8490629577306,5.16345335684645));
#134718=CARTESIAN_POINT('Ctrl Pts',(18.2,15.8545422976518,5.18723193817096));
#134719=CARTESIAN_POINT('Ctrl Pts',(18.2,15.8568489985993,5.19724228190916));
#134720=CARTESIAN_POINT('Ctrl Pts',(18.2,15.8589949315482,5.20729448794936));
#134721=CARTESIAN_POINT('Ctrl Pts',(18.2,15.8609782780096,5.21738393794125));
#134722=CARTESIAN_POINT('Ctrl Pts',(18.2,15.8626367821966,5.22582088800598));
#134723=CARTESIAN_POINT('Ctrl Pts',(18.2,15.8641798770857,5.2342752559103));
#134724=CARTESIAN_POINT('Ctrl Pts',(18.2,15.8656067899539,5.24274194350229));
#134725=CARTESIAN_POINT('Ctrl Pts',(18.2,15.8722734405497,5.28229898243267));
#134726=CARTESIAN_POINT('Ctrl Pts',(18.2,15.8764114541761,5.3221428446593));
#134727=CARTESIAN_POINT('Ctrl Pts',(18.2,15.8779609221616,5.36200248215288));
#134728=CARTESIAN_POINT('Ctrl Pts',(18.2,15.8794724375262,5.40088579891964));
#134729=CARTESIAN_POINT('Ctrl Pts',(18.2,15.878520444433,5.43978518781648));
#134730=CARTESIAN_POINT('Ctrl Pts',(18.2,15.8750036525905,5.47843420519303));
#134731=CARTESIAN_POINT('Ctrl Pts',(18.2,15.8732775467615,5.49740385058803));
#134732=CARTESIAN_POINT('Ctrl Pts',(18.2,15.8709328890102,5.51631285417556));
#134733=CARTESIAN_POINT('Ctrl Pts',(18.2,15.867953759687,5.53512721905791));
#134734=CARTESIAN_POINT('Ctrl Pts',(18.2,15.8667539586533,5.54270443105018));
#134735=CARTESIAN_POINT('Ctrl Pts',(18.2,15.8654512196989,5.55026627040294));
#134736=CARTESIAN_POINT('Ctrl Pts',(18.2,15.8640443848231,5.55781041816403));
#134737=CARTESIAN_POINT('Ctrl Pts',(18.2,15.862571092852,5.56571094189791));
#134738=CARTESIAN_POINT('Ctrl Pts',(18.2,15.8609851714727,5.57358365073891));
#134739=CARTESIAN_POINT('Ctrl Pts',(18.2,15.8592867750134,5.58142260636899));
#134740=CARTESIAN_POINT('Ctrl Pts',(18.2,15.8514062407123,5.6177952438591));
#134741=CARTESIAN_POINT('Ctrl Pts',(18.2,15.8411029443695,5.6534686019582));
#134742=CARTESIAN_POINT('Ctrl Pts',(18.2,15.828297120991,5.6882046655143));
#134743=CARTESIAN_POINT('Ctrl Pts',(18.2,15.8160303433657,5.72147855619873));
#134744=CARTESIAN_POINT('Ctrl Pts',(18.2,15.8014660665262,5.75389278659253));
#134745=CARTESIAN_POINT('Ctrl Pts',(18.2,15.7847628740101,5.78528187055323));
#134746=CARTESIAN_POINT('Ctrl Pts',(18.2,15.7761700718178,5.80142969314545));
#134747=CARTESIAN_POINT('Ctrl Pts',(18.2,15.767010787845,5.81730575509916));
#134748=CARTESIAN_POINT('Ctrl Pts',(18.2,15.7573045304862,5.83288422857645));
#134749=CARTESIAN_POINT('Ctrl Pts',(18.2,15.7524647891595,5.84065197871007));
#134750=CARTESIAN_POINT('Ctrl Pts',(18.2,15.7474890404345,5.84834570361276));
#134751=CARTESIAN_POINT('Ctrl Pts',(18.2,15.742379616577,5.85596196283741));
#134752=CARTESIAN_POINT('Ctrl Pts',(18.2,15.7379704818769,5.86253435020793));
#134753=CARTESIAN_POINT('Ctrl Pts',(18.2,15.7334665877127,5.86904185446495));
#134754=CARTESIAN_POINT('Ctrl Pts',(18.2,15.728872202191,5.87547971657246));
#134755=CARTESIAN_POINT('Ctrl Pts',(18.2,15.7072110042844,5.90583237299332));
#134756=CARTESIAN_POINT('Ctrl Pts',(18.2,15.6835253756505,5.93466343247602));
#134757=CARTESIAN_POINT('Ctrl Pts',(18.2,15.6580146973991,5.96178851524292));
#134758=CARTESIAN_POINT('Ctrl Pts',(18.2,15.6328139718729,5.98858403039735));
#134759=CARTESIAN_POINT('Ctrl Pts',(18.2,15.6058311072394,6.01371535851912));
#134760=CARTESIAN_POINT('Ctrl Pts',(18.2,15.5772374383809,6.03695901454861));
#134761=CARTESIAN_POINT('Ctrl Pts',(18.2,15.5637070537067,6.04795779924012));
#134762=CARTESIAN_POINT('Ctrl Pts',(18.2,15.5498157916581,6.05853318696841));
#134763=CARTESIAN_POINT('Ctrl Pts',(18.2,15.535581267231,6.0686573074634));
#134764=CARTESIAN_POINT('Ctrl Pts',(18.2,15.5278719685831,6.07414044593024));
#134765=CARTESIAN_POINT('Ctrl Pts',(18.2,15.5200592747775,6.07949273630841));
#134766=CARTESIAN_POINT('Ctrl Pts',(18.2,15.5121669270856,6.08469624357819));
#134767=CARTESIAN_POINT('Ctrl Pts',(18.2,15.4829267970524,6.10397456672572));
#134768=CARTESIAN_POINT('Ctrl Pts',(18.2,15.4525389626987,6.12125574713354));
#134769=CARTESIAN_POINT('Ctrl Pts',(18.2,15.421162325823,6.13635948517253));
#134770=CARTESIAN_POINT('Ctrl Pts',(18.2,15.39038989133,6.15117237895856));
#134771=CARTESIAN_POINT('Ctrl Pts',(18.2,15.3586654362256,6.16389118075813));
#134772=CARTESIAN_POINT('Ctrl Pts',(18.2,15.3261350604803,6.17429720693868));
#134773=CARTESIAN_POINT('Ctrl Pts',(18.2,15.3040284533689,6.18136881085022));
#134774=CARTESIAN_POINT('Ctrl Pts',(18.2,15.2815495952911,6.18737133729665));
#134775=CARTESIAN_POINT('Ctrl Pts',(18.2,15.2587465130648,6.19222196005096));
#134776=CARTESIAN_POINT('Ctrl Pts',(18.1991564130999,15.6365194374333,4.77236310691848));
#134777=CARTESIAN_POINT('Ctrl Pts',(18.199295405163,15.6381966008544,4.7738318074538));
#134778=CARTESIAN_POINT('Ctrl Pts',(18.1994348289128,15.6398688368353,4.77530606333199));
#134779=CARTESIAN_POINT('Ctrl Pts',(18.1997162076013,15.6432228597935,4.77828289048378));
#134780=CARTESIAN_POINT('Ctrl Pts',(18.1998575472869,15.6448971332663,4.77977896678006));
#134781=CARTESIAN_POINT('Ctrl Pts',(18.2,15.6465738458316,4.78128738400769));
#134782=CARTESIAN_POINT('Ctrl Pts',(13.98325,14.5748808714849,6.36826222368044));
#134783=CARTESIAN_POINT('Ctrl Pts',(13.9875417602103,14.4844399306344,6.31920189146972));
#134784=CARTESIAN_POINT('Ctrl Pts',(13.9922799151223,14.4025086332371,6.25551032335682));
#134785=CARTESIAN_POINT('Ctrl Pts',(14.0008552261829,14.2697005535018,6.11314868208129));
#134786=CARTESIAN_POINT('Ctrl Pts',(14.0047036502539,14.2168248101705,6.03725042346018));
#134787=CARTESIAN_POINT('Ctrl Pts',(14.0105260091161,14.1516119367069,5.90710469125805));
#134788=CARTESIAN_POINT('Ctrl Pts',(14.0126201956516,14.1316248252275,5.85705808156466));
#134789=CARTESIAN_POINT('Ctrl Pts',(14.0187426631304,14.0868108221527,5.70870074149093));
#134790=CARTESIAN_POINT('Ctrl Pts',(14.0229471609679,14.0736800775832,5.60806525442127));
#134791=CARTESIAN_POINT('Ctrl Pts',(14.0278346537838,14.0778421664996,5.50429828067971));
#134792=CARTESIAN_POINT('Ctrl Pts',(14.0279360152398,14.0779360152551,5.50214887005762));
#134793=CARTESIAN_POINT('Ctrl Pts',(14.0280374670081,14.0780374670081,5.50000000654876));
#134794=CARTESIAN_POINT('Origin',(18.2,15.,5.5));
#134795=CARTESIAN_POINT('',(18.2,15.,6.46675));
#134796=CARTESIAN_POINT('Origin',(18.2,15.,5.5));
#134797=CARTESIAN_POINT('',(18.2002863776289,14.4279740780313,5.96873714629846));
#134798=CARTESIAN_POINT('Ctrl Pts',(18.1999951595719,14.4317719229139,5.97248053125074));
#134799=CARTESIAN_POINT('Ctrl Pts',(18.2000922322575,14.4306418421285,5.97112144111024));
#134800=CARTESIAN_POINT('Ctrl Pts',(18.2001893049432,14.4295166373798,5.96975829655493));
#134801=CARTESIAN_POINT('Ctrl Pts',(18.2002863776289,14.428396337634,5.96839113267634));
#134802=CARTESIAN_POINT('Ctrl Pts',(18.2,14.4275267117712,5.96905018147065));
#134803=CARTESIAN_POINT('Ctrl Pts',(18.2,14.4110560788823,5.95432723823809));
#134804=CARTESIAN_POINT('Ctrl Pts',(18.2,14.3953252123756,5.93885849755578));
#134805=CARTESIAN_POINT('Ctrl Pts',(18.2,14.3803983141861,5.92267896053057));
#134806=CARTESIAN_POINT('Ctrl Pts',(18.2,14.3578580110206,5.89824711507976));
#134807=CARTESIAN_POINT('Ctrl Pts',(18.2,14.3371491699726,5.87219655019198));
#134808=CARTESIAN_POINT('Ctrl Pts',(18.2,14.3182680759095,5.84477757422518));
#134809=CARTESIAN_POINT('Ctrl Pts',(18.2,14.312272357361,5.83607063901083));
#134810=CARTESIAN_POINT('Ctrl Pts',(18.2,14.3064611356987,5.82722540504078));
#134811=CARTESIAN_POINT('Ctrl Pts',(18.2,14.3008348537117,5.81824908509359));
#134812=CARTESIAN_POINT('Ctrl Pts',(18.2,14.2956258061032,5.80993843197276));
#134813=CARTESIAN_POINT('Ctrl Pts',(18.2,14.2905790444203,5.80152119332205));
#134814=CARTESIAN_POINT('Ctrl Pts',(18.2,14.2856985275162,5.79301102887662));
#134815=CARTESIAN_POINT('Ctrl Pts',(18.2,14.2679154747507,5.76200269382717));
#134816=CARTESIAN_POINT('Ctrl Pts',(18.2,14.252318999542,5.72973535427369));
#134817=CARTESIAN_POINT('Ctrl Pts',(18.2,14.2389065388398,5.69650131415319));
#134818=CARTESIAN_POINT('Ctrl Pts',(18.2,14.2330453803533,5.68197825379763));
#134819=CARTESIAN_POINT('Ctrl Pts',(18.2,14.2276016983777,5.66727002000594));
#134820=CARTESIAN_POINT('Ctrl Pts',(18.2,14.2225773518228,5.65239869796253));
#134821=CARTESIAN_POINT('Ctrl Pts',(18.2,14.2195918595483,5.64356208277537));
#134822=CARTESIAN_POINT('Ctrl Pts',(18.2,14.2167544515313,5.63466786072778));
#134823=CARTESIAN_POINT('Ctrl Pts',(18.2,14.2140657538221,5.62572048401501));
#134824=CARTESIAN_POINT('Ctrl Pts',(18.2,14.2114827872951,5.61712495671811));
#134825=CARTESIAN_POINT('Ctrl Pts',(18.2,14.2090397158183,5.60848901704883));
#134826=CARTESIAN_POINT('Ctrl Pts',(18.2,14.2067374833686,5.5998213650989));
#134827=CARTESIAN_POINT('Ctrl Pts',(18.2,14.1970355687405,5.56329472364009));
#134828=CARTESIAN_POINT('Ctrl Pts',(18.2,14.1898245868981,5.526184207686));
#134829=CARTESIAN_POINT('Ctrl Pts',(18.2,14.1851036775246,5.48880133972137));
#134830=CARTESIAN_POINT('Ctrl Pts',(18.2,14.1803510104794,5.45116699629885));
#134831=CARTESIAN_POINT('Ctrl Pts',(18.2,14.1781214585709,5.41325537129091));
#134832=CARTESIAN_POINT('Ctrl Pts',(18.2,14.1784579006432,5.37535412581749));
#134833=CARTESIAN_POINT('Ctrl Pts',(18.2,14.1786450716592,5.35426872893824));
#134834=CARTESIAN_POINT('Ctrl Pts',(18.2,14.1796272365876,5.33318611320977));
#134835=CARTESIAN_POINT('Ctrl Pts',(18.2,14.1814185858649,5.31215405814663));
#134836=CARTESIAN_POINT('Ctrl Pts',(18.2,14.1821024176586,5.30412525654898));
#134837=CARTESIAN_POINT('Ctrl Pts',(18.2,14.1829035768574,5.29611199368922));
#134838=CARTESIAN_POINT('Ctrl Pts',(18.2,14.1838216163247,5.28812180317335));
#134839=CARTESIAN_POINT('Ctrl Pts',(18.2,14.1882918266273,5.24921516218645));
#134840=CARTESIAN_POINT('Ctrl Pts',(18.2,14.195532536316,5.21082134697863));
#134841=CARTESIAN_POINT('Ctrl Pts',(18.2,14.2055656184632,5.1732481664357));
#134842=CARTESIAN_POINT('Ctrl Pts',(18.2,14.2152472940966,5.13699097834594));
#134843=CARTESIAN_POINT('Ctrl Pts',(18.2,14.227528570009,5.10149645494108));
#134844=CARTESIAN_POINT('Ctrl Pts',(18.2,14.2421925851606,5.0669049975911));
#134845=CARTESIAN_POINT('Ctrl Pts',(18.2,14.2489467564536,5.05097234709937));
#134846=CARTESIAN_POINT('Ctrl Pts',(18.2,14.2562071429791,5.03523130804939));
#134847=CARTESIAN_POINT('Ctrl Pts',(18.2,14.2639560523831,5.01969608757539));
#134848=CARTESIAN_POINT('Ctrl Pts',(18.2,14.2677892194207,5.01201125195023));
#134849=CARTESIAN_POINT('Ctrl Pts',(18.2,14.2717419603285,5.00437678786767));
#134850=CARTESIAN_POINT('Ctrl Pts',(18.2,14.2758123165251,4.99679447067505));
#134851=CARTESIAN_POINT('Ctrl Pts',(18.2,14.2797099298683,4.98953394131724));
#134852=CARTESIAN_POINT('Ctrl Pts',(18.2,14.2837112647265,4.98232898818152));
#134853=CARTESIAN_POINT('Ctrl Pts',(18.2,14.2878118668406,4.97518441495171));
#134854=CARTESIAN_POINT('Ctrl Pts',(18.2,14.307746884195,4.9404511764259));
#134855=CARTESIAN_POINT('Ctrl Pts',(18.2,14.33003748588,4.90711848704015));
#134856=CARTESIAN_POINT('Ctrl Pts',(18.2,14.3544187642976,4.87534375641278));
#134857=CARTESIAN_POINT('Ctrl Pts',(18.2,14.3788000427153,4.84356902578541));
#134858=CARTESIAN_POINT('Ctrl Pts',(18.2,14.4052726360747,4.81335131532712));
#134859=CARTESIAN_POINT('Ctrl Pts',(18.2,14.4336230376443,4.78485942579126));
#134860=CARTESIAN_POINT('Ctrl Pts',(18.2,14.447387658005,4.77102611052555));
#134861=CARTESIAN_POINT('Ctrl Pts',(18.2,14.4615956412497,4.75759987717825));
#134862=CARTESIAN_POINT('Ctrl Pts',(18.2,14.4762262189405,4.74460203982858));
#134863=CARTESIAN_POINT('Ctrl Pts',(18.2,14.4829425087495,4.73863527321316));
#134864=CARTESIAN_POINT('Ctrl Pts',(18.2,14.489747884209,4.73275880670212));
#134865=CARTESIAN_POINT('Ctrl Pts',(18.2,14.4966404830651,4.72697482667735));
#134866=CARTESIAN_POINT('Ctrl Pts',(18.2,14.5028292708112,4.72178145543251));
#134867=CARTESIAN_POINT('Ctrl Pts',(18.2,14.5090804061117,4.71666934181821));
#134868=CARTESIAN_POINT('Ctrl Pts',(18.2,14.515391912452,4.7116396578817));
#134869=CARTESIAN_POINT('Ctrl Pts',(18.2,14.5484748964647,4.6852755944886));
#134870=CARTESIAN_POINT('Ctrl Pts',(18.2,14.583212849161,4.66117452364675));
#134871=CARTESIAN_POINT('Ctrl Pts',(18.2,14.6193549193654,4.63951288687606));
#134872=CARTESIAN_POINT('Ctrl Pts',(18.2,14.6552623674113,4.61799187016251));
#134873=CARTESIAN_POINT('Ctrl Pts',(18.2,14.6925565889502,4.59887772234494));
#134874=CARTESIAN_POINT('Ctrl Pts',(18.2,14.7310329626811,4.58237205343048));
#134875=CARTESIAN_POINT('Ctrl Pts',(18.2,14.7585486993975,4.57056829969433));
#134876=CARTESIAN_POINT('Ctrl Pts',(18.2,14.7866698996498,4.56009911105786));
#134877=CARTESIAN_POINT('Ctrl Pts',(18.2,14.8153312661022,4.55105162352181));
#134878=CARTESIAN_POINT('Origin',(18.2,15.,5.5));
#134879=CARTESIAN_POINT('Ctrl Pts',(13.9812628603546,15.4268458854961,6.37121714501327));
#134880=CARTESIAN_POINT('Ctrl Pts',(14.0022472159886,15.1396755667749,6.51192110495675));
#134881=CARTESIAN_POINT('Ctrl Pts',(14.0442104273441,14.420290532822,6.48498127166269));
#134882=CARTESIAN_POINT('Ctrl Pts',(14.1071524944209,13.8574310494572,5.55569014930716));
#134883=CARTESIAN_POINT('Ctrl Pts',(14.170089061585,14.3258164373528,4.57705680776936));
#134884=CARTESIAN_POINT('Ctrl Pts',(14.2330256287492,15.3998968445188,4.42900222271004));
#134885=CARTESIAN_POINT('Ctrl Pts',(14.2959621959134,16.1145993730642,5.24532569248693));
#134886=CARTESIAN_POINT('Ctrl Pts',(14.3588987630776,15.8255094218027,6.29084264316953));
#134887=CARTESIAN_POINT('Ctrl Pts',(14.4218353302418,14.7933917703228,6.62441707563672));
#134888=CARTESIAN_POINT('Ctrl Pts',(14.4847718974059,13.9471942622981,5.94566791670918));
#134889=CARTESIAN_POINT('Ctrl Pts',(14.5477084645701,14.0488711730629,4.86570045630136));
#134890=CARTESIAN_POINT('Ctrl Pts',(14.6106450317343,15.006816278288,4.35678006002944));
#134891=CARTESIAN_POINT('Ctrl Pts',(14.6735815988985,15.958636524409,4.87709145345759));
#134892=CARTESIAN_POINT('Ctrl Pts',(14.7365181660626,16.0474005173,5.95819916383029));
#134893=CARTESIAN_POINT('Ctrl Pts',(14.7994547332268,15.1932041177945,6.62679588022745));
#134894=CARTESIAN_POINT('Ctrl Pts',(14.862391300391,14.1650665262539,6.28094989097661));
#134895=CARTESIAN_POINT('Ctrl Pts',(14.9253278675552,13.888611432723,5.23202327700034));
#134896=CARTESIAN_POINT('Ctrl Pts',(14.9882644347194,14.6127271683571,4.42435313218742));
#134897=CARTESIAN_POINT('Ctrl Pts',(15.0512010018835,15.6855007097753,4.58507642183189));
#134898=CARTESIAN_POINT('Ctrl Pts',(15.1141375690477,16.141125178985,5.56949560057099));
#134899=CARTESIAN_POINT('Ctrl Pts',(15.1770741362119,15.5694069032307,6.4913486478301));
#134900=CARTESIAN_POINT('Ctrl Pts',(15.2400107033761,14.4850576496457,6.52070109597772));
#134901=CARTESIAN_POINT('Ctrl Pts',(15.3029472705403,13.8643055049512,5.63112726125519));
#134902=CARTESIAN_POINT('Ctrl Pts',(15.3658838377044,14.2660069674623,4.62350095278392));
#134903=CARTESIAN_POINT('Ctrl Pts',(15.4288204048686,15.3285145156993,4.40497736896518));
#134904=CARTESIAN_POINT('Ctrl Pts',(15.4917569720328,16.0952639548138,5.17229095502555));
#134905=CARTESIAN_POINT('Ctrl Pts',(15.554693539197,15.8759589633338,6.23463749178203));
#134906=CARTESIAN_POINT('Ctrl Pts',(15.6176301063612,14.8680374794508,6.63559774682888));
#134907=CARTESIAN_POINT('Ctrl Pts',(15.6805666735253,13.9789204425895,6.01419148848167));
#134908=CARTESIAN_POINT('Ctrl Pts',(15.7435032406895,14.0090704171655,4.92986412902933));
#134909=CARTESIAN_POINT('Ctrl Pts',(15.8064398078537,14.9313437035418,4.3588240002493));
#134910=CARTESIAN_POINT('Ctrl Pts',(15.8693763750179,15.9154275197398,4.81517242640679));
#134911=CARTESIAN_POINT('Ctrl Pts',(15.9323129421821,16.075361724617,5.88806379719466));
#134912=CARTESIAN_POINT('Ctrl Pts',(15.9952495093462,15.2671592629749,6.61158547924259));
#134913=CARTESIAN_POINT('Ctrl Pts',(16.0581860765104,14.2184361724521,6.33435863567591));
#134914=CARTESIAN_POINT('Ctrl Pts',(16.1211226436746,13.8733466420087,5.30596763057404));
#134915=CARTESIAN_POINT('Ctrl Pts',(16.1840592108388,14.5425710873636,4.45226189372512));
#134916=CARTESIAN_POINT('Ctrl Pts',(16.246995778003,15.623613893471,4.54182357504772));
#134917=CARTESIAN_POINT('Ctrl Pts',(16.3099323451671,16.1432237768698,5.49402125015251));
#134918=CARTESIAN_POINT('Ctrl Pts',(16.3728689123313,15.633601513481,6.45160152982487));
#134919=CARTESIAN_POINT('Ctrl Pts',(16.4358054794955,14.5535545798252,6.55246512355937));
#134920=CARTESIAN_POINT('Ctrl Pts',(16.4987420466597,13.8754376861007,5.70580561592405));
#134921=CARTESIAN_POINT('Ctrl Pts',(16.5616786138239,14.2097522234401,4.67386151216965));
#134922=CARTESIAN_POINT('Ctrl Pts',(16.624615180988,15.2555183875101,4.38568105848424));
#134923=CARTESIAN_POINT('Ctrl Pts',(16.6875517481522,16.0712440781121,5.10071003771423));
#134924=CARTESIAN_POINT('Ctrl Pts',(16.7504883153164,15.9225401760006,6.17521550127969));
#134925=CARTESIAN_POINT('Ctrl Pts',(16.8134248824806,14.9432832128561,6.64183166782179));
#134926=CARTESIAN_POINT('Ctrl Pts',(16.8763614496447,14.0150877694587,6.08046898526848));
#134927=CARTESIAN_POINT('Ctrl Pts',(16.9392980168089,13.9735982749522,4.99651628592629));
#134928=CARTESIAN_POINT('Ctrl Pts',(17.0022345839731,14.8561672921798,4.36584458068467));
#134929=CARTESIAN_POINT('Ctrl Pts',(17.0651711511373,15.8682273403298,4.75624090048179));
#134930=CARTESIAN_POINT('Ctrl Pts',(17.1281077183015,16.0986316303056,5.81623554177613));
#134931=CARTESIAN_POINT('Ctrl Pts',(17.1910442854656,15.3399495359646,6.59152679461439));
#134932=CARTESIAN_POINT('Ctrl Pts',(17.2539808526298,14.2752146452534,6.38412796646659));
#134933=CARTESIAN_POINT('Ctrl Pts',(17.316917419794,13.8629959949843,5.38075852074024));
#134934=CARTESIAN_POINT('Ctrl Pts',(17.3798539869582,14.4744104185701,4.48474024076459));
#134935=CARTESIAN_POINT('Ctrl Pts',(17.4427905541224,15.5590065089138,4.50275076316532));
#134936=CARTESIAN_POINT('Ctrl Pts',(17.5057271212865,16.1403369932313,5.41857159491376));
#134937=CARTESIAN_POINT('Ctrl Pts',(17.5686636884507,15.6950304150661,6.40770645856968));
#134938=CARTESIAN_POINT('Ctrl Pts',(17.6316002556149,14.6240028972271,6.57963333371724));
#134939=CARTESIAN_POINT('Ctrl Pts',(17.6945368227791,13.8914669101736,5.77959649869392));
#134940=CARTESIAN_POINT('Ctrl Pts',(17.7574733899432,14.1569599465065,4.72780560170415));
#134941=CARTESIAN_POINT('Ctrl Pts',(17.8204099571074,15.1813773355444,4.37128384706725));
#134942=CARTESIAN_POINT('Ctrl Pts',(17.8833465242716,16.042610986541,5.03079525142366));
#134943=CARTESIAN_POINT('Ctrl Pts',(17.9462830914358,15.9649819702309,6.11299553207626));
#134944=CARTESIAN_POINT('Ctrl Pts',(18.0092196586,15.0190017581962,6.64279768350049));
#134945=CARTESIAN_POINT('Ctrl Pts',(18.0721562257642,14.0551086903138,6.1447833840553));
#134946=CARTESIAN_POINT('Ctrl Pts',(18.1350967229588,13.9434899186243,5.06410065696252));
#134947=CARTESIAN_POINT('Ctrl Pts',(18.177058364432,14.5009678185522,4.60868560308863));
#134948=CARTESIAN_POINT('Ctrl Pts',(18.1980411501839,14.814855634692,4.54766692269823));
#134949=CARTESIAN_POINT('Ctrl Pts',(14.0259231306101,15.3928122569186,6.30175254026682));
#134950=CARTESIAN_POINT('Ctrl Pts',(14.0469074862441,15.1285388391585,6.43123777590067));
#134951=CARTESIAN_POINT('Ctrl Pts',(14.0888706975995,14.4665124067093,6.4064459316383));
#134952=CARTESIAN_POINT('Ctrl Pts',(14.1518127646763,13.94853130041,5.55124981634076));
#134953=CARTESIAN_POINT('Ctrl Pts',(14.2147493318405,14.3795709978247,4.65064567642131));
#134954=CARTESIAN_POINT('Ctrl Pts',(14.2776858990047,15.3680119391277,4.51439590178259));
#134955=CARTESIAN_POINT('Ctrl Pts',(14.3406224661689,16.0257292155568,5.26563159465118));
#134956=CARTESIAN_POINT('Ctrl Pts',(14.403559033333,15.7596892229829,6.22778652456713));
#134957=CARTESIAN_POINT('Ctrl Pts',(14.4664956004972,14.8098652282821,6.53476412496152));
#134958=CARTESIAN_POINT('Ctrl Pts',(14.5294321676614,14.0311374386496,5.91013355439827));
#134959=CARTESIAN_POINT('Ctrl Pts',(14.5923687348256,14.1247073620134,4.91627495124337));
#134960=CARTESIAN_POINT('Ctrl Pts',(14.6553053019898,15.0062727971596,4.44793221620871));
#134961=CARTESIAN_POINT('Ctrl Pts',(14.718241869154,15.8822017255247,4.92675771200912));
#134962=CARTESIAN_POINT('Ctrl Pts',(14.7811784363181,15.9638883144447,5.92166564977722));
#134963=CARTESIAN_POINT('Ctrl Pts',(14.8441150034823,15.1777994075511,6.53695326074052));
#134964=CARTESIAN_POINT('Ctrl Pts',(14.9070515706465,14.2316381313645,6.21868254946021));
#134965=CARTESIAN_POINT('Ctrl Pts',(14.9699881378107,13.9772255836124,5.25338981833962));
#134966=CARTESIAN_POINT('Ctrl Pts',(15.0329247049749,14.6436055255302,4.51011749638414));
#134967=CARTESIAN_POINT('Ctrl Pts',(15.095861272139,15.6308438011843,4.65802586399385));
#134968=CARTESIAN_POINT('Ctrl Pts',(15.1587978393032,16.0501400440184,5.56395451996565));
#134969=CARTESIAN_POINT('Ctrl Pts',(15.2217344064674,15.5240064818785,6.41230561891176));
#134970=CARTESIAN_POINT('Ctrl Pts',(15.2846709736316,14.5261154582979,6.43931771342815));
#134971=CARTESIAN_POINT('Ctrl Pts',(15.3476075407957,13.9548576361425,5.62067211419259));
#134972=CARTESIAN_POINT('Ctrl Pts',(15.4105441079599,14.3245303059707,4.69338669851791));
#134973=CARTESIAN_POINT('Ctrl Pts',(15.4734806751241,15.302321125088,4.49228661751318));
#134974=CARTESIAN_POINT('Ctrl Pts',(15.5364172422883,16.007935464839,5.19842012317987));
#134975=CARTESIAN_POINT('Ctrl Pts',(15.5993538094524,15.8061162800138,6.17606276871713));
#134976=CARTESIAN_POINT('Ctrl Pts',(15.6622903766167,14.8785592240971,6.54505332964661));
#134977=CARTESIAN_POINT('Ctrl Pts',(15.7252269437808,14.0603340009386,5.97319354816815));
#134978=CARTESIAN_POINT('Ctrl Pts',(15.788163510945,14.0880800328476,4.9753226730392));
#134979=CARTESIAN_POINT('Ctrl Pts',(15.8511000781092,14.9368178640586,4.44981318729933));
#134980=CARTESIAN_POINT('Ctrl Pts',(15.9140366452733,15.8424378968923,4.86977566394798));
#134981=CARTESIAN_POINT('Ctrl Pts',(15.9769732124375,15.989620095693,5.85712237410304));
#134982=CARTESIAN_POINT('Ctrl Pts',(16.0399097796017,15.2458579000332,6.52295562800579));
#134983=CARTESIAN_POINT('Ctrl Pts',(16.1028463467659,14.2807524648661,6.26783286402901));
#134984=CARTESIAN_POINT('Ctrl Pts',(16.1657829139301,13.963177897795,5.32143837966034));
#134985=CARTESIAN_POINT('Ctrl Pts',(16.2287194810942,14.5790431871124,4.53580101350342));
#134986=CARTESIAN_POINT('Ctrl Pts',(16.2916560482584,15.5738913956158,4.61822168890217));
#134987=CARTESIAN_POINT('Ctrl Pts',(16.3545926154226,16.0520713147637,5.49449795277187));
#134988=CARTESIAN_POINT('Ctrl Pts',(16.4175291825868,15.5830826744606,6.37572765093743));
#134989=CARTESIAN_POINT('Ctrl Pts',(16.480465749751,14.5891509346843,6.46854910533599));
#134990=CARTESIAN_POINT('Ctrl Pts',(16.5434023169151,13.9651022170329,5.68939615262709));
#134991=CARTESIAN_POINT('Ctrl Pts',(16.6063388840793,14.2727609116468,4.73973186820137));
#134992=CARTESIAN_POINT('Ctrl Pts',(16.6692754512435,15.2351451844627,4.47452885639193));
#134993=CARTESIAN_POINT('Ctrl Pts',(16.7322120184077,15.985830760779,5.13254655467003));
#134994=CARTESIAN_POINT('Ctrl Pts',(16.7951485855719,15.8489834409714,6.12137866142463));
#134995=CARTESIAN_POINT('Ctrl Pts',(16.858085152736,14.9478054025582,6.55079020250375));
#134996=CARTESIAN_POINT('Ctrl Pts',(16.9210217199002,14.0936176046393,6.03418655285762));
#134997=CARTESIAN_POINT('Ctrl Pts',(16.9839582870644,14.0554361847655,5.03666046512959));
#134998=CARTESIAN_POINT('Ctrl Pts',(17.0468948542286,14.8676354803984,4.45627399701871));
#134999=CARTESIAN_POINT('Ctrl Pts',(17.1098314213928,15.799001121159,4.81554291510618));
#135000=CARTESIAN_POINT('Ctrl Pts',(17.1727679885569,16.0110346260479,5.79102118845218));
#135001=CARTESIAN_POINT('Ctrl Pts',(17.2357045557211,15.312844398876,6.50449627898228));
#135002=CARTESIAN_POINT('Ctrl Pts',(17.2986411228853,14.3330038295935,6.3136339454439));
#135003=CARTESIAN_POINT('Ctrl Pts',(17.3615776900495,13.9536525371054,5.39026598081901));
#135004=CARTESIAN_POINT('Ctrl Pts',(17.4245142572136,14.5163171610417,4.56568977016024));
#135005=CARTESIAN_POINT('Ctrl Pts',(17.4874508243779,15.5144353403885,4.58226426271812));
#135006=CARTESIAN_POINT('Ctrl Pts',(17.550387391542,16.0494147025417,5.4250641117413));
#135007=CARTESIAN_POINT('Ctrl Pts',(17.6133239587062,15.6396136761443,6.33533245774653));
#135008=CARTESIAN_POINT('Ctrl Pts',(17.6762605258703,14.653982208676,6.49355111732947));
#135009=CARTESIAN_POINT('Ctrl Pts',(17.7391970930346,13.9798533857772,5.75730347980486));
#135010=CARTESIAN_POINT('Ctrl Pts',(17.8021336601987,14.2241779121268,4.78937484304891));
#135011=CARTESIAN_POINT('Ctrl Pts',(17.8650702273629,15.1669156080684,4.46127957532304));
#135012=CARTESIAN_POINT('Ctrl Pts',(17.9280067945271,15.9594806665067,5.06820627184672));
#135013=CARTESIAN_POINT('Ctrl Pts',(17.9909433616913,15.8880412310211,6.06411966617906));
#135014=CARTESIAN_POINT('Ctrl Pts',(18.0538799288554,15.0174866943225,6.55167919502274));
#135015=CARTESIAN_POINT('Ctrl Pts',(18.1168164960196,14.1304475443887,6.09337298289774));
#135016=CARTESIAN_POINT('Ctrl Pts',(18.1797569932142,14.0277284527642,5.09885614329179));
#135017=CARTESIAN_POINT('Ctrl Pts',(18.2217186346875,14.5407570644806,4.67975261851716));
#135018=CARTESIAN_POINT('Ctrl Pts',(18.2427014204393,14.8296177180955,4.62359912993311));
#135019=CARTESIAN_POINT('Ctrl Pts',(14.0705834008655,15.3587786283412,6.23228793552038));
#135020=CARTESIAN_POINT('Ctrl Pts',(14.0915677564996,15.1174021115421,6.35055444684459));
#135021=CARTESIAN_POINT('Ctrl Pts',(14.1335309678549,14.5127342805966,6.32791059161392));
#135022=CARTESIAN_POINT('Ctrl Pts',(14.1964730349317,14.0396315513625,5.54680948337434));
#135023=CARTESIAN_POINT('Ctrl Pts',(14.2594096020959,14.4333255582968,4.72423454507328));
#135024=CARTESIAN_POINT('Ctrl Pts',(14.3223461692601,15.3361270337367,4.59978958085514));
#135025=CARTESIAN_POINT('Ctrl Pts',(14.3852827364243,15.9368590580494,5.28593749681547));
#135026=CARTESIAN_POINT('Ctrl Pts',(14.4482193035884,15.6938690241632,6.16473040596473));
#135027=CARTESIAN_POINT('Ctrl Pts',(14.5111558707526,14.8263386862416,6.44511117428634));
#135028=CARTESIAN_POINT('Ctrl Pts',(14.5740924379168,14.115080615001,5.87459919208737));
#135029=CARTESIAN_POINT('Ctrl Pts',(14.637029005081,14.2005435509639,4.96684944618539));
#135030=CARTESIAN_POINT('Ctrl Pts',(14.6999655722452,15.0057293160312,4.53908437238796));
#135031=CARTESIAN_POINT('Ctrl Pts',(14.7629021394093,15.8057669266405,4.97642397056065));
#135032=CARTESIAN_POINT('Ctrl Pts',(14.8258387065735,15.8803761115893,5.88513213572415));
#135033=CARTESIAN_POINT('Ctrl Pts',(14.8887752737377,15.1623946973077,6.44711064125359));
#135034=CARTESIAN_POINT('Ctrl Pts',(14.9517118409019,14.2982097364751,6.15641520794383));
#135035=CARTESIAN_POINT('Ctrl Pts',(15.014648408066,14.0658397345017,5.27475635967888));
#135036=CARTESIAN_POINT('Ctrl Pts',(15.0775849752302,14.6744838827034,4.59588186058087));
#135037=CARTESIAN_POINT('Ctrl Pts',(15.1405215423944,15.5761868925933,4.7309753061558));
#135038=CARTESIAN_POINT('Ctrl Pts',(15.2034581095586,15.9591549090515,5.55841343936032));
#135039=CARTESIAN_POINT('Ctrl Pts',(15.2663946767228,15.4786060605264,6.33326258999341));
#135040=CARTESIAN_POINT('Ctrl Pts',(15.3293312438869,14.5671732669502,6.3579343308786));
#135041=CARTESIAN_POINT('Ctrl Pts',(15.3922678110511,14.0454097673336,5.61021696712997));
#135042=CARTESIAN_POINT('Ctrl Pts',(15.4552043782153,14.3830536444789,4.76327244425191));
#135043=CARTESIAN_POINT('Ctrl Pts',(15.5181409453795,15.2761277344769,4.57959586606118));
#135044=CARTESIAN_POINT('Ctrl Pts',(15.5810775125437,15.9206069748642,5.2245492913342));
#135045=CARTESIAN_POINT('Ctrl Pts',(15.6440140797078,15.7362735966939,6.11748804565223));
#135046=CARTESIAN_POINT('Ctrl Pts',(15.706950646872,14.8890809687434,6.45450891246436));
#135047=CARTESIAN_POINT('Ctrl Pts',(15.7698872140362,14.1417475592875,5.93219560785463));
#135048=CARTESIAN_POINT('Ctrl Pts',(15.8328237812004,14.1670896485298,5.02078121704908));
#135049=CARTESIAN_POINT('Ctrl Pts',(15.8957603483645,14.9422920245755,4.54080237434935));
#135050=CARTESIAN_POINT('Ctrl Pts',(15.9586969155287,15.7694482740449,4.92437890148916));
#135051=CARTESIAN_POINT('Ctrl Pts',(16.0216334826929,15.903878466769,5.82618095101143));
#135052=CARTESIAN_POINT('Ctrl Pts',(16.0845700498571,15.2245565370916,6.434325776769));
#135053=CARTESIAN_POINT('Ctrl Pts',(16.1475066170213,14.3430687572802,6.20130709238213));
#135054=CARTESIAN_POINT('Ctrl Pts',(16.2104431841855,14.0530091535813,5.33690912874664));
#135055=CARTESIAN_POINT('Ctrl Pts',(16.2733797513496,14.6155152868614,4.61934013328171));
#135056=CARTESIAN_POINT('Ctrl Pts',(16.3363163185138,15.5241688977606,4.6946198027566));
#135057=CARTESIAN_POINT('Ctrl Pts',(16.399252885678,15.9609188526577,5.49497465539119));
#135058=CARTESIAN_POINT('Ctrl Pts',(16.4621894528422,15.5325638354403,6.29985377205));
#135059=CARTESIAN_POINT('Ctrl Pts',(16.5251260200063,14.6247472895435,6.38463308711259));
#135060=CARTESIAN_POINT('Ctrl Pts',(16.5880625871705,14.0547667479651,5.67298668933017));
#135061=CARTESIAN_POINT('Ctrl Pts',(16.6509991543347,14.3357695998536,4.80560222423307));
#135062=CARTESIAN_POINT('Ctrl Pts',(16.7139357214989,15.2147719814151,4.56337665429964));
#135063=CARTESIAN_POINT('Ctrl Pts',(16.7768722886631,15.9004174434459,5.16438307162583));
#135064=CARTESIAN_POINT('Ctrl Pts',(16.8398088558272,15.7754267059423,6.06754182156959));
#135065=CARTESIAN_POINT('Ctrl Pts',(16.9027454229914,14.9523275922601,6.4597487371857));
#135066=CARTESIAN_POINT('Ctrl Pts',(16.9656819901556,14.1721474398201,5.98790412044679));
#135067=CARTESIAN_POINT('Ctrl Pts',(17.0286185573198,14.137274094579,5.07680464433289));
#135068=CARTESIAN_POINT('Ctrl Pts',(17.091555124484,14.8791036686173,4.54670341335277));
#135069=CARTESIAN_POINT('Ctrl Pts',(17.1544916916481,15.7297749019882,4.87484492973059));
#135070=CARTESIAN_POINT('Ctrl Pts',(17.2174282588123,15.9234376217902,5.76580683512822));
#135071=CARTESIAN_POINT('Ctrl Pts',(17.2803648259765,15.2857392617874,6.41746576335018));
#135072=CARTESIAN_POINT('Ctrl Pts',(17.3433013931407,14.3907930139337,6.24313992442123));
#135073=CARTESIAN_POINT('Ctrl Pts',(17.4062379603049,14.0443090792265,5.39977344089779));
#135074=CARTESIAN_POINT('Ctrl Pts',(17.469174527469,14.5582239035133,4.6466392995559));
#135075=CARTESIAN_POINT('Ctrl Pts',(17.5321110946332,15.4698641718634,4.66177776227094));
#135076=CARTESIAN_POINT('Ctrl Pts',(17.5950476617974,15.9584924118522,5.43155662856886));
#135077=CARTESIAN_POINT('Ctrl Pts',(17.6579842289616,15.5841969372227,6.26295845692337));
#135078=CARTESIAN_POINT('Ctrl Pts',(17.7209207961258,14.6839615201247,6.40746890094173));
#135079=CARTESIAN_POINT('Ctrl Pts',(17.7838573632899,14.0682398613808,5.73501046091577));
#135080=CARTESIAN_POINT('Ctrl Pts',(17.8467939304541,14.2913958777472,4.8509440843937));
#135081=CARTESIAN_POINT('Ctrl Pts',(17.9097304976183,15.1524538805926,4.55127530357883));
#135082=CARTESIAN_POINT('Ctrl Pts',(17.9726670647825,15.8763503464722,5.10561729226978));
#135083=CARTESIAN_POINT('Ctrl Pts',(18.0356036319466,15.8111004918114,6.01524380028187));
#135084=CARTESIAN_POINT('Ctrl Pts',(18.0985401991108,15.0159716304487,6.46056070654498));
#135085=CARTESIAN_POINT('Ctrl Pts',(18.161476766275,14.2057863984636,6.04196258174017));
#135086=CARTESIAN_POINT('Ctrl Pts',(18.2244172634697,14.111966986904,5.13361162962105));
#135087=CARTESIAN_POINT('Ctrl Pts',(18.2663789049429,14.5805463104091,4.75081963394569));
#135088=CARTESIAN_POINT('Ctrl Pts',(18.2873616906948,14.8443798014988,4.69953133716798));
#135089=CARTESIAN_POINT('Ctrl Pts',(14.1152436711209,15.3247449997639,6.16282333077395));
#135090=CARTESIAN_POINT('Ctrl Pts',(14.1362280267549,15.1062653839256,6.26987111778852));
#135091=CARTESIAN_POINT('Ctrl Pts',(14.1781912381104,14.558956154484,6.24937525158952));
#135092=CARTESIAN_POINT('Ctrl Pts',(14.2411333051872,14.1307318023153,5.54236915040796));
#135093=CARTESIAN_POINT('Ctrl Pts',(14.3040698723514,14.4870801187687,4.79782341372522));
#135094=CARTESIAN_POINT('Ctrl Pts',(14.3670064395155,15.3042421283455,4.68518325992769));
#135095=CARTESIAN_POINT('Ctrl Pts',(14.4299430066797,15.8479889005418,5.30624339897972));
#135096=CARTESIAN_POINT('Ctrl Pts',(14.4928795738439,15.6280488253434,6.10167428736234));
#135097=CARTESIAN_POINT('Ctrl Pts',(14.5558161410081,14.8428121442009,6.35545822361114));
#135098=CARTESIAN_POINT('Ctrl Pts',(14.6187527081723,14.1990237913524,5.83906482977647));
#135099=CARTESIAN_POINT('Ctrl Pts',(14.6816892753364,14.2763797399144,5.01742394112739));
#135100=CARTESIAN_POINT('Ctrl Pts',(14.7446258425006,15.0051858349026,4.63023652856724));
#135101=CARTESIAN_POINT('Ctrl Pts',(14.8075624096648,15.7293321277563,5.02609022911216));
#135102=CARTESIAN_POINT('Ctrl Pts',(14.870498976829,15.7968639087338,5.84859862167108));
#135103=CARTESIAN_POINT('Ctrl Pts',(14.9334355439932,15.1469899870644,6.35726802176666));
#135104=CARTESIAN_POINT('Ctrl Pts',(14.9963721111573,14.3647813415856,6.09414786642744));
#135105=CARTESIAN_POINT('Ctrl Pts',(15.0593086783215,14.1544538853912,5.29612290101818));
#135106=CARTESIAN_POINT('Ctrl Pts',(15.1222452454857,14.7053622398767,4.68164622477757));
#135107=CARTESIAN_POINT('Ctrl Pts',(15.1851818126499,15.5215299840022,4.80392474831775));
#135108=CARTESIAN_POINT('Ctrl Pts',(15.2481183798141,15.8681697740847,5.55287235875496));
#135109=CARTESIAN_POINT('Ctrl Pts',(15.3110549469782,15.4332056391742,6.25421956107508));
#135110=CARTESIAN_POINT('Ctrl Pts',(15.3739915141424,14.6082310756026,6.27655094832902));
#135111=CARTESIAN_POINT('Ctrl Pts',(15.4369280813066,14.1359618985248,5.59976182006737));
#135112=CARTESIAN_POINT('Ctrl Pts',(15.4998646484708,14.4415769829873,4.8331581899859));
#135113=CARTESIAN_POINT('Ctrl Pts',(15.5628012156349,15.2499343438656,4.66690511460918));
#135114=CARTESIAN_POINT('Ctrl Pts',(15.6257377827991,15.8332784848894,5.25067845948853));
#135115=CARTESIAN_POINT('Ctrl Pts',(15.6886743499633,15.6664309133739,6.0589133225873));
#135116=CARTESIAN_POINT('Ctrl Pts',(15.7516109171275,14.8996027133896,6.3639644952821));
#135117=CARTESIAN_POINT('Ctrl Pts',(15.8145474842917,14.2231611176365,5.89119766754112));
#135118=CARTESIAN_POINT('Ctrl Pts',(15.8774840514559,14.2460992642119,5.06623976105893));
#135119=CARTESIAN_POINT('Ctrl Pts',(15.94042061862,14.9477661850923,4.63179156139939));
#135120=CARTESIAN_POINT('Ctrl Pts',(16.0033571857842,15.6964586511974,4.97898213903037));
#135121=CARTESIAN_POINT('Ctrl Pts',(16.0662937529484,15.8181368378449,5.7952395279198));
#135122=CARTESIAN_POINT('Ctrl Pts',(16.1292303201126,15.2032551741499,6.34569592553222));
#135123=CARTESIAN_POINT('Ctrl Pts',(16.1921668872767,14.4053850496942,6.13478132073524));
#135124=CARTESIAN_POINT('Ctrl Pts',(16.2551034544409,14.1428404093677,5.35237987783294));
#135125=CARTESIAN_POINT('Ctrl Pts',(16.3180400216051,14.6519873866103,4.70287925306001));
#135126=CARTESIAN_POINT('Ctrl Pts',(16.3809765887693,15.4744463999053,4.77101791661106));
#135127=CARTESIAN_POINT('Ctrl Pts',(16.4439131559335,15.8697663905516,5.49545135801052));
#135128=CARTESIAN_POINT('Ctrl Pts',(16.5068497230977,15.4820449964198,6.22397989316257));
#135129=CARTESIAN_POINT('Ctrl Pts',(16.5697862902618,14.6603436444027,6.3007170688892));
#135130=CARTESIAN_POINT('Ctrl Pts',(16.632722857426,14.1444312788974,5.6565772260332));
#135131=CARTESIAN_POINT('Ctrl Pts',(16.6956594245902,14.3987782880603,4.87147258026479));
#135132=CARTESIAN_POINT('Ctrl Pts',(16.7585959917544,15.1943987783676,4.65222445220735));
#135133=CARTESIAN_POINT('Ctrl Pts',(16.8215325589185,15.8150041261129,5.19621958858164));
#135134=CARTESIAN_POINT('Ctrl Pts',(16.8844691260827,15.7018699709131,6.01370498171452));
#135135=CARTESIAN_POINT('Ctrl Pts',(16.9474056932469,14.9568497819623,6.36870727186765));
#135136=CARTESIAN_POINT('Ctrl Pts',(17.0103422604111,14.2506772750008,5.94162168803595));
#135137=CARTESIAN_POINT('Ctrl Pts',(17.0732788275753,14.2191120043925,5.11694882353618));
#135138=CARTESIAN_POINT('Ctrl Pts',(17.1362153947394,14.8905718568359,4.63713282968683));
#135139=CARTESIAN_POINT('Ctrl Pts',(17.1991519619036,15.6605486828174,4.93414694435498));
#135140=CARTESIAN_POINT('Ctrl Pts',(17.2620885290678,15.8358406175325,5.74059248180427));
#135141=CARTESIAN_POINT('Ctrl Pts',(17.325025096232,15.2586341246988,6.33043524771806));
#135142=CARTESIAN_POINT('Ctrl Pts',(17.3879616633962,14.4485821982738,6.17264590339857));
#135143=CARTESIAN_POINT('Ctrl Pts',(17.4508982305603,14.1349656213476,5.40928090097655));
#135144=CARTESIAN_POINT('Ctrl Pts',(17.5138347977245,14.6001306459849,4.72758882895156));
#135145=CARTESIAN_POINT('Ctrl Pts',(17.5767713648887,15.4252930033383,4.74129126182374));
#135146=CARTESIAN_POINT('Ctrl Pts',(17.6397079320529,15.8675701211627,5.43804914539642));
#135147=CARTESIAN_POINT('Ctrl Pts',(17.702644499217,15.5287801983009,6.19058445610023));
#135148=CARTESIAN_POINT('Ctrl Pts',(17.7655810663813,14.7139408315735,6.32138668455399));
#135149=CARTESIAN_POINT('Ctrl Pts',(17.8285176335454,14.1566263369844,5.7127174420267));
#135150=CARTESIAN_POINT('Ctrl Pts',(17.8914542007096,14.3586138433675,4.91251332573848));
#135151=CARTESIAN_POINT('Ctrl Pts',(17.9543907678738,15.1379921531166,4.64127103183461));
#135152=CARTESIAN_POINT('Ctrl Pts',(18.0173273350379,15.793220026438,5.14302831269285));
#135153=CARTESIAN_POINT('Ctrl Pts',(18.0802639022021,15.7341597526016,5.96636793438466));
#135154=CARTESIAN_POINT('Ctrl Pts',(18.1432004693663,15.014456566575,6.36944221806724));
#135155=CARTESIAN_POINT('Ctrl Pts',(18.2061370365305,14.2811252525384,5.99055218058262));
#135156=CARTESIAN_POINT('Ctrl Pts',(18.2690775337251,14.1962055210438,5.16836711595032));
#135157=CARTESIAN_POINT('Ctrl Pts',(18.3110391751983,14.6203355563376,4.82188664937422));
#135158=CARTESIAN_POINT('Ctrl Pts',(18.3320219609502,14.8591418849023,4.77546354440285));
#135159=CARTESIAN_POINT('Ctrl Pts',(13.9832500000001,15.4251191285151,6.36826222368042));
#135160=CARTESIAN_POINT('Ctrl Pts',(13.9999444295459,15.3215451468816,6.40038609166026));
#135161=CARTESIAN_POINT('Ctrl Pts',(14.0151347722421,15.2140895632333,6.41628947421468));
#135162=CARTESIAN_POINT('Ctrl Pts',(14.0464108252689,15.0135230598887,6.40808816006153));
#135163=CARTESIAN_POINT('Ctrl Pts',(14.0616867519111,14.9233916473141,6.38961563625844));
#135164=CARTESIAN_POINT('Ctrl Pts',(14.1014789163806,14.7191082827324,6.31037841140784));
#135165=CARTESIAN_POINT('Ctrl Pts',(14.122898891006,14.6299394659766,6.24441205772044));
#135166=CARTESIAN_POINT('Ctrl Pts',(14.150553159263,14.5162927313885,6.14013885201157));
#135167=CARTESIAN_POINT('Ctrl Pts',(14.162214770313,14.4710252601612,6.0877267220467));
#135168=CARTESIAN_POINT('Ctrl Pts',(14.1857737491176,14.3996118262497,5.97684797725505));
#135169=CARTESIAN_POINT('Ctrl Pts',(14.1973567639203,14.3727511830336,5.92043909160861));
#135170=CARTESIAN_POINT('Ctrl Pts',(14.2099481424296,14.3539251530524,5.86092110500077));
#135171=CARTESIAN_POINT('Origin',(18.2,15.,5.5));
#135172=CARTESIAN_POINT('',(18.3,15.,6.56675));
#135173=CARTESIAN_POINT('Origin',(18.3,15.,5.5));
#135174=CARTESIAN_POINT('Origin',(18.2,15.,6.56675));
#135175=CARTESIAN_POINT('Origin',(18.3,16.9,5.5));
#135176=CARTESIAN_POINT('',(18.3,13.1,5.5));
#135177=CARTESIAN_POINT('Origin',(18.3,15.,5.5));
#135178=CARTESIAN_POINT('Origin',(19.,15.,5.5));
#135179=CARTESIAN_POINT('',(19.,13.1165191798163,5.25));
#135180=CARTESIAN_POINT('',(19.,13.1,5.5));
#135181=CARTESIAN_POINT('Origin',(19.,15.,5.5));
#135182=CARTESIAN_POINT('',(19.,16.8834808201837,5.25));
#135183=CARTESIAN_POINT('',(19.,12.6,5.25));
#135184=CARTESIAN_POINT('',(19.,16.8834808201837,5.75));
#135185=CARTESIAN_POINT('Origin',(19.,15.,5.5));
#135186=CARTESIAN_POINT('',(19.,13.1165191798163,5.75));
#135187=CARTESIAN_POINT('',(19.,17.4,5.75));
#135188=CARTESIAN_POINT('Origin',(19.,15.,5.5));
#135189=CARTESIAN_POINT('Origin',(19.6,12.6,5.75));
#135190=CARTESIAN_POINT('',(19.2,13.1165191798163,5.75));
#135191=CARTESIAN_POINT('',(18.75,13.1165191798163,5.75));
#135192=CARTESIAN_POINT('',(19.2,16.8834808201837,5.75));
#135193=CARTESIAN_POINT('',(18.75,16.8834808201837,5.75));
#135194=CARTESIAN_POINT('',(19.6,16.4790199457749,5.75));
#135195=CARTESIAN_POINT('Ctrl Pts',(19.6,16.4790199457749,5.75));
#135196=CARTESIAN_POINT('Ctrl Pts',(19.4240571469012,16.6574585668375,5.75));
#135197=CARTESIAN_POINT('Ctrl Pts',(19.2000000000002,16.8834808201836,5.75));
#135198=CARTESIAN_POINT('',(19.6,13.5209800542251,5.75));
#135199=CARTESIAN_POINT('',(19.6,13.8,5.75));
#135200=CARTESIAN_POINT('Ctrl Pts',(19.2000000000002,13.1165191798164,5.75));
#135201=CARTESIAN_POINT('Ctrl Pts',(19.4240571469012,13.3425414331625,5.75));
#135202=CARTESIAN_POINT('Ctrl Pts',(19.6,13.5209800542251,5.75));
#135203=CARTESIAN_POINT('Origin',(19.6,17.4,5.25));
#135204=CARTESIAN_POINT('',(19.2,13.1165191798163,5.25));
#135205=CARTESIAN_POINT('',(18.75,13.1165191798163,5.25));
#135206=CARTESIAN_POINT('',(19.6,13.5209800542251,5.25));
#135207=CARTESIAN_POINT('Ctrl Pts',(19.6,13.5209800542251,5.25));
#135208=CARTESIAN_POINT('Ctrl Pts',(19.4240571469012,13.3425414331624,5.25));
#135209=CARTESIAN_POINT('Ctrl Pts',(19.2000000000002,13.1165191798164,5.25));
#135210=CARTESIAN_POINT('',(19.6,16.4790199457749,5.25));
#135211=CARTESIAN_POINT('',(19.6,16.2,5.25));
#135212=CARTESIAN_POINT('',(19.2,16.8834808201837,5.25));
#135213=CARTESIAN_POINT('Ctrl Pts',(19.2000000000002,16.8834808201836,5.25));
#135214=CARTESIAN_POINT('Ctrl Pts',(19.4240571469012,16.6574585668376,5.25));
#135215=CARTESIAN_POINT('Ctrl Pts',(19.6,16.4790199457749,5.25));
#135216=CARTESIAN_POINT('',(18.75,16.8834808201837,5.25));
#135217=CARTESIAN_POINT('Origin',(18.75,15.,5.5));
#135218=CARTESIAN_POINT('',(18.75,13.1,5.5));
#135219=CARTESIAN_POINT('Origin',(19.2,15.,5.5));
#135220=CARTESIAN_POINT('Origin',(19.2,15.,5.5));
#135221=CARTESIAN_POINT('Origin',(19.6,15.,5.5));
#135222=CARTESIAN_POINT('Origin',(19.6,15.,5.5));
#135223=CARTESIAN_POINT('Origin',(19.6,15.,5.5));
#135224=CARTESIAN_POINT('Origin',(19.6,15.,5.5));
#135225=CARTESIAN_POINT('Origin',(19.4,15.,5.5));
#135226=CARTESIAN_POINT('Origin',(14.3,15.65,5.5));
#135227=CARTESIAN_POINT('',(14.3,14.35,5.5));
#135228=CARTESIAN_POINT('Origin',(14.3,15.,5.5));
#135229=CARTESIAN_POINT('Origin',(14.125,15.,5.5));
#135230=CARTESIAN_POINT('',(14.125,14.175,5.5));
#135231=CARTESIAN_POINT('Origin',(19.4,15.,5.5));
#135232=CARTESIAN_POINT('',(0.,0.,0.));
#135233=CARTESIAN_POINT('',(0.,0.,0.));
#135234=CARTESIAN_POINT('',(0.,0.,0.));
#135235=CARTESIAN_POINT('',(0.,0.,0.));
#135236=CARTESIAN_POINT('',(0.,0.,0.));
#135237=CARTESIAN_POINT('',(0.,0.,0.));
#135238=CARTESIAN_POINT('',(0.,0.,0.));
#135239=CARTESIAN_POINT('',(0.,0.,0.));
#135240=CARTESIAN_POINT('',(0.,0.,0.));
#135241=CARTESIAN_POINT('',(0.,0.,0.));
#135242=CARTESIAN_POINT('',(0.,0.,0.));
#135243=CARTESIAN_POINT('',(0.,0.,0.));
#135244=CARTESIAN_POINT('',(0.,0.,0.));
#135245=CARTESIAN_POINT('',(8.57252759403147E-15,140.,0.));
#135246=CARTESIAN_POINT('',(20.,0.,0.));
#135247=CARTESIAN_POINT('',(8.57252759403147E-15,140.,0.));
#135248=CARTESIAN_POINT('',(-20.,140.,0.));
#135249=CARTESIAN_POINT('',(20.,0.,0.));
#135250=CARTESIAN_POINT('',(0.,110.,0.));
#135251=CARTESIAN_POINT('',(-5.,52.,16.));
#135252=CARTESIAN_POINT('',(-5.,58.,16.));
#135253=UNCERTAINTY_MEASURE_WITH_UNIT(LENGTH_MEASURE(0.01),#135283,
'DISTANCE_ACCURACY_VALUE',
'Maximum model space distance between geometric entities at asserted c
onnectivities');
#135254=UNCERTAINTY_MEASURE_WITH_UNIT(LENGTH_MEASURE(0.01),#135283,
'DISTANCE_ACCURACY_VALUE',
'Maximum model space distance between geometric entities at asserted c
onnectivities');
#135255=UNCERTAINTY_MEASURE_WITH_UNIT(LENGTH_MEASURE(0.01),#135283,
'DISTANCE_ACCURACY_VALUE',
'Maximum model space distance between geometric entities at asserted c
onnectivities');
#135256=UNCERTAINTY_MEASURE_WITH_UNIT(LENGTH_MEASURE(0.01),#135283,
'DISTANCE_ACCURACY_VALUE',
'Maximum model space distance between geometric entities at asserted c
onnectivities');
#135257=UNCERTAINTY_MEASURE_WITH_UNIT(LENGTH_MEASURE(0.01),#135283,
'DISTANCE_ACCURACY_VALUE',
'Maximum model space distance between geometric entities at asserted c
onnectivities');
#135258=UNCERTAINTY_MEASURE_WITH_UNIT(LENGTH_MEASURE(0.01),#135283,
'DISTANCE_ACCURACY_VALUE',
'Maximum model space distance between geometric entities at asserted c
onnectivities');
#135259=UNCERTAINTY_MEASURE_WITH_UNIT(LENGTH_MEASURE(0.01),#135283,
'DISTANCE_ACCURACY_VALUE',
'Maximum model space distance between geometric entities at asserted c
onnectivities');
#135260=UNCERTAINTY_MEASURE_WITH_UNIT(LENGTH_MEASURE(0.01),#135283,
'DISTANCE_ACCURACY_VALUE',
'Maximum model space distance between geometric entities at asserted c
onnectivities');
#135261=UNCERTAINTY_MEASURE_WITH_UNIT(LENGTH_MEASURE(0.01),#135283,
'DISTANCE_ACCURACY_VALUE',
'Maximum model space distance between geometric entities at asserted c
onnectivities');
#135262=UNCERTAINTY_MEASURE_WITH_UNIT(LENGTH_MEASURE(0.01),#135283,
'DISTANCE_ACCURACY_VALUE',
'Maximum model space distance between geometric entities at asserted c
onnectivities');
#135263=UNCERTAINTY_MEASURE_WITH_UNIT(LENGTH_MEASURE(0.01),#135283,
'DISTANCE_ACCURACY_VALUE',
'Maximum model space distance between geometric entities at asserted c
onnectivities');
#135264=UNCERTAINTY_MEASURE_WITH_UNIT(LENGTH_MEASURE(0.01),#135283,
'DISTANCE_ACCURACY_VALUE',
'Maximum model space distance between geometric entities at asserted c
onnectivities');
#135265=UNCERTAINTY_MEASURE_WITH_UNIT(LENGTH_MEASURE(0.01),#135283,
'DISTANCE_ACCURACY_VALUE',
'Maximum model space distance between geometric entities at asserted c
onnectivities');
#135266=UNCERTAINTY_MEASURE_WITH_UNIT(LENGTH_MEASURE(0.01),#135283,
'DISTANCE_ACCURACY_VALUE',
'Maximum model space distance between geometric entities at asserted c
onnectivities');
#135267=UNCERTAINTY_MEASURE_WITH_UNIT(LENGTH_MEASURE(0.01),#135283,
'DISTANCE_ACCURACY_VALUE',
'Maximum model space distance between geometric entities at asserted c
onnectivities');
#135268=(
GEOMETRIC_REPRESENTATION_CONTEXT(3)
GLOBAL_UNCERTAINTY_ASSIGNED_CONTEXT((#135253))
GLOBAL_UNIT_ASSIGNED_CONTEXT((#135283,#135285,#135286))
REPRESENTATION_CONTEXT('','3D')
);
#135269=(
GEOMETRIC_REPRESENTATION_CONTEXT(3)
GLOBAL_UNCERTAINTY_ASSIGNED_CONTEXT((#135254))
GLOBAL_UNIT_ASSIGNED_CONTEXT((#135283,#135285,#135286))
REPRESENTATION_CONTEXT('','3D')
);
#135270=(
GEOMETRIC_REPRESENTATION_CONTEXT(3)
GLOBAL_UNCERTAINTY_ASSIGNED_CONTEXT((#135255))
GLOBAL_UNIT_ASSIGNED_CONTEXT((#135283,#135285,#135286))
REPRESENTATION_CONTEXT('','3D')
);
#135271=(
GEOMETRIC_REPRESENTATION_CONTEXT(3)
GLOBAL_UNCERTAINTY_ASSIGNED_CONTEXT((#135256))
GLOBAL_UNIT_ASSIGNED_CONTEXT((#135283,#135285,#135286))
REPRESENTATION_CONTEXT('','3D')
);
#135272=(
GEOMETRIC_REPRESENTATION_CONTEXT(3)
GLOBAL_UNCERTAINTY_ASSIGNED_CONTEXT((#135257))
GLOBAL_UNIT_ASSIGNED_CONTEXT((#135283,#135285,#135286))
REPRESENTATION_CONTEXT('','3D')
);
#135273=(
GEOMETRIC_REPRESENTATION_CONTEXT(3)
GLOBAL_UNCERTAINTY_ASSIGNED_CONTEXT((#135258))
GLOBAL_UNIT_ASSIGNED_CONTEXT((#135283,#135285,#135286))
REPRESENTATION_CONTEXT('','3D')
);
#135274=(
GEOMETRIC_REPRESENTATION_CONTEXT(3)
GLOBAL_UNCERTAINTY_ASSIGNED_CONTEXT((#135259))
GLOBAL_UNIT_ASSIGNED_CONTEXT((#135283,#135285,#135286))
REPRESENTATION_CONTEXT('','3D')
);
#135275=(
GEOMETRIC_REPRESENTATION_CONTEXT(3)
GLOBAL_UNCERTAINTY_ASSIGNED_CONTEXT((#135260))
GLOBAL_UNIT_ASSIGNED_CONTEXT((#135283,#135285,#135286))
REPRESENTATION_CONTEXT('','3D')
);
#135276=(
GEOMETRIC_REPRESENTATION_CONTEXT(3)
GLOBAL_UNCERTAINTY_ASSIGNED_CONTEXT((#135261))
GLOBAL_UNIT_ASSIGNED_CONTEXT((#135283,#135285,#135286))
REPRESENTATION_CONTEXT('','3D')
);
#135277=(
GEOMETRIC_REPRESENTATION_CONTEXT(3)
GLOBAL_UNCERTAINTY_ASSIGNED_CONTEXT((#135262))
GLOBAL_UNIT_ASSIGNED_CONTEXT((#135283,#135285,#135286))
REPRESENTATION_CONTEXT('','3D')
);
#135278=(
GEOMETRIC_REPRESENTATION_CONTEXT(3)
GLOBAL_UNCERTAINTY_ASSIGNED_CONTEXT((#135263))
GLOBAL_UNIT_ASSIGNED_CONTEXT((#135283,#135285,#135286))
REPRESENTATION_CONTEXT('','3D')
);
#135279=(
GEOMETRIC_REPRESENTATION_CONTEXT(3)
GLOBAL_UNCERTAINTY_ASSIGNED_CONTEXT((#135264))
GLOBAL_UNIT_ASSIGNED_CONTEXT((#135283,#135285,#135286))
REPRESENTATION_CONTEXT('','3D')
);
#135280=(
GEOMETRIC_REPRESENTATION_CONTEXT(3)
GLOBAL_UNCERTAINTY_ASSIGNED_CONTEXT((#135265))
GLOBAL_UNIT_ASSIGNED_CONTEXT((#135283,#135285,#135286))
REPRESENTATION_CONTEXT('','3D')
);
#135281=(
GEOMETRIC_REPRESENTATION_CONTEXT(3)
GLOBAL_UNCERTAINTY_ASSIGNED_CONTEXT((#135266))
GLOBAL_UNIT_ASSIGNED_CONTEXT((#135283,#135285,#135286))
REPRESENTATION_CONTEXT('','3D')
);
#135282=(
GEOMETRIC_REPRESENTATION_CONTEXT(3)
GLOBAL_UNCERTAINTY_ASSIGNED_CONTEXT((#135267))
GLOBAL_UNIT_ASSIGNED_CONTEXT((#135283,#135285,#135286))
REPRESENTATION_CONTEXT('','3D')
);
#135283=(
LENGTH_UNIT()
NAMED_UNIT(*)
SI_UNIT(.MILLI.,.METRE.)
);
#135284=(
LENGTH_UNIT()
NAMED_UNIT(*)
SI_UNIT($,.METRE.)
);
#135285=(
NAMED_UNIT(*)
PLANE_ANGLE_UNIT()
SI_UNIT($,.RADIAN.)
);
#135286=(
NAMED_UNIT(*)
SI_UNIT($,.STERADIAN.)
SOLID_ANGLE_UNIT()
);
#135287=SHAPE_DEFINITION_REPRESENTATION(#135301,#135336);
#135288=SHAPE_DEFINITION_REPRESENTATION(#135302,#135337);
#135289=SHAPE_DEFINITION_REPRESENTATION(#135303,#135338);
#135290=SHAPE_DEFINITION_REPRESENTATION(#135304,#135339);
#135291=SHAPE_DEFINITION_REPRESENTATION(#135305,#135340);
#135292=SHAPE_DEFINITION_REPRESENTATION(#135306,#135341);
#135293=SHAPE_DEFINITION_REPRESENTATION(#135307,#135342);
#135294=SHAPE_DEFINITION_REPRESENTATION(#135308,#135343);
#135295=SHAPE_DEFINITION_REPRESENTATION(#135309,#135344);
#135296=SHAPE_DEFINITION_REPRESENTATION(#135310,#135345);
#135297=SHAPE_DEFINITION_REPRESENTATION(#135311,#135346);
#135298=SHAPE_DEFINITION_REPRESENTATION(#135312,#135347);
#135299=SHAPE_DEFINITION_REPRESENTATION(#135313,#135348);
#135300=SHAPE_DEFINITION_REPRESENTATION(#135314,#135349);
#135301=PRODUCT_DEFINITION_SHAPE('',$,#135351);
#135302=PRODUCT_DEFINITION_SHAPE('',$,#135352);
#135303=PRODUCT_DEFINITION_SHAPE('',$,#135353);
#135304=PRODUCT_DEFINITION_SHAPE('',$,#135354);
#135305=PRODUCT_DEFINITION_SHAPE('',$,#135355);
#135306=PRODUCT_DEFINITION_SHAPE('',$,#135356);
#135307=PRODUCT_DEFINITION_SHAPE('',$,#135357);
#135308=PRODUCT_DEFINITION_SHAPE('',$,#135358);
#135309=PRODUCT_DEFINITION_SHAPE('',$,#135359);
#135310=PRODUCT_DEFINITION_SHAPE('',$,#135360);
#135311=PRODUCT_DEFINITION_SHAPE('',$,#135361);
#135312=PRODUCT_DEFINITION_SHAPE('',$,#135362);
#135313=PRODUCT_DEFINITION_SHAPE('',$,#135363);
#135314=PRODUCT_DEFINITION_SHAPE('',$,#135364);
#135315=PRODUCT_DEFINITION_SHAPE($,$,#74);
#135316=PRODUCT_DEFINITION_SHAPE($,$,#75);
#135317=PRODUCT_DEFINITION_SHAPE($,$,#76);
#135318=PRODUCT_DEFINITION_SHAPE($,$,#77);
#135319=PRODUCT_DEFINITION_SHAPE($,$,#78);
#135320=PRODUCT_DEFINITION_SHAPE($,$,#79);
#135321=PRODUCT_DEFINITION_SHAPE($,$,#80);
#135322=PRODUCT_DEFINITION_SHAPE($,$,#81);
#135323=PRODUCT_DEFINITION_SHAPE($,$,#82);
#135324=PRODUCT_DEFINITION_SHAPE($,$,#83);
#135325=PRODUCT_DEFINITION_SHAPE($,$,#84);
#135326=PRODUCT_DEFINITION_SHAPE($,$,#85);
#135327=PRODUCT_DEFINITION_SHAPE($,$,#86);
#135328=PRODUCT_DEFINITION_SHAPE($,$,#87);
#135329=PRODUCT_DEFINITION_SHAPE($,$,#88);
#135330=PRODUCT_DEFINITION_SHAPE($,$,#89);
#135331=PRODUCT_DEFINITION_SHAPE($,$,#90);
#135332=PRODUCT_DEFINITION_SHAPE($,$,#91);
#135333=PRODUCT_DEFINITION_SHAPE($,$,#92);
#135334=PRODUCT_DEFINITION_SHAPE($,$,#93);
#135335=PRODUCT_DEFINITION_SHAPE($,$,#94);
#135336=SHAPE_REPRESENTATION('',(#32232,#34203,#34204,#34205,#34206,#34207,
#34208,#34209,#34210,#34211,#34212,#34213,#34214,#34215,#34216,#34217,#34218,
#34219,#34220,#34221,#34222,#34223),#135268);
#135337=SHAPE_REPRESENTATION('',(#32233),#135269);
#135338=SHAPE_REPRESENTATION('',(#32276),#135270);
#135339=SHAPE_REPRESENTATION('',(#32384),#135271);
#135340=SHAPE_REPRESENTATION('',(#32403),#135272);
#135341=SHAPE_REPRESENTATION('',(#32477),#135273);
#135342=SHAPE_REPRESENTATION('',(#32757),#135274);
#135343=SHAPE_REPRESENTATION('',(#33287),#135275);
#135344=SHAPE_REPRESENTATION('',(#33359),#135276);
#135345=SHAPE_REPRESENTATION('',(#33412),#135277);
#135346=SHAPE_REPRESENTATION('',(#33493),#135278);
#135347=SHAPE_REPRESENTATION('',(#33555),#135279);
#135348=SHAPE_REPRESENTATION('',(#33856),#135280);
#135349=SHAPE_REPRESENTATION('',(#34149),#135281);
#135350=PRODUCT_DEFINITION_CONTEXT('part definition',#135394,'design');
#135351=PRODUCT_DEFINITION('2026-10-15-19-09-11-254',
'MAS-258',#135365,#135350);
#135352=PRODUCT_DEFINITION('2026-10-15-19-09-11-255',
'Dovetail Base Rail',#135366,#135350);
#135353=PRODUCT_DEFINITION('2026-10-15-19-09-11-256',
'Dovetail Carriage',#135367,#135350);
#135354=PRODUCT_DEFINITION('2026-10-15-19-09-11-257',
'Brass Feed Nut D9 x 15 Lead 2',#135368,#135350);
#135355=PRODUCT_DEFINITION('2026-10-15-19-09-11-258',
'Precision Feed Screw D5 Lead 2',#135369,#135350);
#135356=PRODUCT_DEFINITION('2026-10-15-19-09-11-260',
'Feed Knob D15 Knurled',#135370,#135350);
#135357=PRODUCT_DEFINITION('2026-10-15-19-09-11-261',
'Stainless Scale Plate 0.1 mm Vernier',#135371,#135350);
#135358=PRODUCT_DEFINITION('2026-10-15-19-09-11-262',
'Vernier Pointer Plate',#135372,#135350);
#135359=PRODUCT_DEFINITION('2026-10-15-19-09-11-263',
'Z-Axis L-Bracket Foot',#135373,#135350);
#135360=PRODUCT_DEFINITION('2026-10-15-19-09-11-267',
'ISO 4026 - M3 x 5 - 45H',#135374,#135350);
#135361=PRODUCT_DEFINITION('2026-10-15-19-09-11-259',
'Feed Screw End Block',#135375,#135350);
#135362=PRODUCT_DEFINITION('2026-10-15-19-09-11-264',
'ISO 4762 - M3 x 12 - 12.9',#135376,#135350);
#135363=PRODUCT_DEFINITION('2026-10-15-19-09-11-265',
'ISO 4762 - M3 x 10 - 12.9',#135377,#135350);
#135364=PRODUCT_DEFINITION('2026-10-15-19-09-11-266',
'ISO 1207 - M2 x 4 - 4.8',#135378,#135350);
#135365=PRODUCT_DEFINITION_FORMATION('',$,#135396);
#135366=PRODUCT_DEFINITION_FORMATION('',$,#135397);
#135367=PRODUCT_DEFINITION_FORMATION('',$,#135398);
#135368=PRODUCT_DEFINITION_FORMATION('',$,#135399);
#135369=PRODUCT_DEFINITION_FORMATION('',$,#135400);
#135370=PRODUCT_DEFINITION_FORMATION('',$,#135401);
#135371=PRODUCT_DEFINITION_FORMATION('',$,#135402);
#135372=PRODUCT_DEFINITION_FORMATION('',$,#135403);
#135373=PRODUCT_DEFINITION_FORMATION('',$,#135404);
#135374=PRODUCT_DEFINITION_FORMATION('',$,#135405);
#135375=PRODUCT_DEFINITION_FORMATION('',$,#135406);
#135376=PRODUCT_DEFINITION_FORMATION('',$,#135407);
#135377=PRODUCT_DEFINITION_FORMATION('',$,#135408);
#135378=PRODUCT_DEFINITION_FORMATION('',$,#135409);
#135379=PRODUCT_RELATED_PRODUCT_CATEGORY('MAS-258',
'MAS-258',(#135396));
#135380=PRODUCT_RELATED_PRODUCT_CATEGORY('Dovetail Base Rail',
'Dovetail Base Rail',(#135397));
#135381=PRODUCT_RELATED_PRODUCT_CATEGORY('Dovetail Carriage',
'Dovetail Carriage',(#135398));
#135382=PRODUCT_RELATED_PRODUCT_CATEGORY(
'Brass Feed Nut D9 x 15 Lead 2','Brass Feed Nut D9 x 15 Lead 2',(#135399));
#135383=PRODUCT_RELATED_PRODUCT_CATEGORY(
'Precision Feed Screw D5 Lead 2','Precision Feed Screw D5 Lead 2',(#135400));
#135384=PRODUCT_RELATED_PRODUCT_CATEGORY('Feed Knob D15 Knurled',
'Feed Knob D15 Knurled',(#135401));
#135385=PRODUCT_RELATED_PRODUCT_CATEGORY(
'Stainless Scale Plate 0.1 mm Vernier',
'Stainless Scale Plate 0.1 mm Vernier',(#135402));
#135386=PRODUCT_RELATED_PRODUCT_CATEGORY('Vernier Pointer Plate',
'Vernier Pointer Plate',(#135403));
#135387=PRODUCT_RELATED_PRODUCT_CATEGORY('Z-Axis L-Bracket Foot',
'Z-Axis L-Bracket Foot',(#135404));
#135388=PRODUCT_RELATED_PRODUCT_CATEGORY('ISO 4026 - M3 x 5 - 45H',
'ISO 4026 - M3 x 5 - 45H',(#135405));
#135389=PRODUCT_RELATED_PRODUCT_CATEGORY('Feed Screw End Block',
'Feed Screw End Block',(#135406));
#135390=PRODUCT_RELATED_PRODUCT_CATEGORY('ISO 4762 - M3 x 12 - 12.9',
'ISO 4762 - M3 x 12 - 12.9',(#135407));
#135391=PRODUCT_RELATED_PRODUCT_CATEGORY('ISO 4762 - M3 x 10 - 12.9',
'ISO 4762 - M3 x 10 - 12.9',(#135408));
#135392=PRODUCT_RELATED_PRODUCT_CATEGORY('ISO 1207 - M2 x 4 - 4.8',
'ISO 1207 - M2 x 4 - 4.8',(#135409));
#135393=APPLICATION_PROTOCOL_DEFINITION('international standard',
'automotive_design',2009,#135394);
#135394=APPLICATION_CONTEXT(
'Core Data for Automotive Mechanical Design Process');
#135395=PRODUCT_CONTEXT('part definition',#135394,'mechanical');
#135396=PRODUCT('2026-10-15-19-09-11-254','MAS-258',$,
(#135395));
#135397=PRODUCT('2026-10-15-19-09-11-255','Dovetail Base Rail',$,(#135395));
#135398=PRODUCT('2026-10-15-19-09-11-256','Dovetail Carriage',$,(#135395));
#135399=PRODUCT('2026-10-15-19-09-11-257',
'Brass Feed Nut D9 x 15 Lead 2',$,(#135395));
#135400=PRODUCT('2026-10-15-19-09-11-258',
'Precision Feed Screw D5 Lead 2',$,(#135395));
#135401=PRODUCT('2026-10-15-19-09-11-260','Feed Knob D15 Knurled',$,(#135395));
#135402=PRODUCT('2026-10-15-19-09-11-261',
'Stainless Scale Plate 0.1 mm Vernier',$,(#135395));
#135403=PRODUCT('2026-10-15-19-09-11-262','Vernier Pointer Plate',$,(#135395));
#135404=PRODUCT('2026-10-15-19-09-11-263','Z-Axis L-Bracket Foot',$,(#135395));
#135405=PRODUCT('2026-10-15-19-09-11-267','ISO 4026 - M3 x 5 - 45H',$,(#135395));
#135406=PRODUCT('2026-10-15-19-09-11-259','Feed Screw End Block',$,(#135395));
#135407=PRODUCT('2026-10-15-19-09-11-264','ISO 4762 - M3 x 12 - 12.9',$,
(#135395));
#135408=PRODUCT('2026-10-15-19-09-11-265','ISO 4762 - M3 x 10 - 12.9',$,
(#135395));
#135409=PRODUCT('2026-10-15-19-09-11-266','ISO 1207 - M2 x 4 - 4.8',$,(#135395));
#135410=PRESENTATION_STYLE_ASSIGNMENT((#135424));
#135411=PRESENTATION_STYLE_ASSIGNMENT((#135425));
#135412=PRESENTATION_STYLE_ASSIGNMENT((#135426));
#135413=PRESENTATION_STYLE_ASSIGNMENT((#135427));
#135414=PRESENTATION_STYLE_ASSIGNMENT((#135428));
#135415=PRESENTATION_STYLE_ASSIGNMENT((#135429));
#135416=PRESENTATION_STYLE_ASSIGNMENT((#135430));
#135417=PRESENTATION_STYLE_ASSIGNMENT((#135431));
#135418=PRESENTATION_STYLE_ASSIGNMENT((#135432));
#135419=PRESENTATION_STYLE_ASSIGNMENT((#135433));
#135420=PRESENTATION_STYLE_ASSIGNMENT((#135434));
#135421=PRESENTATION_STYLE_ASSIGNMENT((#135435));
#135422=PRESENTATION_STYLE_ASSIGNMENT((#135436));
#135423=PRESENTATION_STYLE_ASSIGNMENT((#135437));
#135424=SURFACE_STYLE_USAGE(.BOTH.,#135438);
#135425=SURFACE_STYLE_USAGE(.BOTH.,#135439);
#135426=SURFACE_STYLE_USAGE(.BOTH.,#135440);
#135427=SURFACE_STYLE_USAGE(.BOTH.,#135441);
#135428=SURFACE_STYLE_USAGE(.BOTH.,#135442);
#135429=SURFACE_STYLE_USAGE(.BOTH.,#135443);
#135430=SURFACE_STYLE_USAGE(.BOTH.,#135444);
#135431=SURFACE_STYLE_USAGE(.BOTH.,#135445);
#135432=SURFACE_STYLE_USAGE(.BOTH.,#135446);
#135433=SURFACE_STYLE_USAGE(.BOTH.,#135447);
#135434=SURFACE_STYLE_USAGE(.BOTH.,#135448);
#135435=SURFACE_STYLE_USAGE(.BOTH.,#135449);
#135436=SURFACE_STYLE_USAGE(.BOTH.,#135450);
#135437=SURFACE_STYLE_USAGE(.BOTH.,#135451);
#135438=SURFACE_SIDE_STYLE('',(#135452));
#135439=SURFACE_SIDE_STYLE('',(#135453));
#135440=SURFACE_SIDE_STYLE('',(#135454));
#135441=SURFACE_SIDE_STYLE('',(#135455));
#135442=SURFACE_SIDE_STYLE('',(#135456));
#135443=SURFACE_SIDE_STYLE('',(#135457));
#135444=SURFACE_SIDE_STYLE('',(#135458));
#135445=SURFACE_SIDE_STYLE('',(#135459));
#135446=SURFACE_SIDE_STYLE('',(#135460));
#135447=SURFACE_SIDE_STYLE('',(#135461));
#135448=SURFACE_SIDE_STYLE('',(#135462));
#135449=SURFACE_SIDE_STYLE('',(#135463));
#135450=SURFACE_SIDE_STYLE('',(#135464));
#135451=SURFACE_SIDE_STYLE('',(#135465));
#135452=SURFACE_STYLE_FILL_AREA(#135466);
#135453=SURFACE_STYLE_FILL_AREA(#135467);
#135454=SURFACE_STYLE_FILL_AREA(#135468);
#135455=SURFACE_STYLE_FILL_AREA(#135469);
#135456=SURFACE_STYLE_FILL_AREA(#135470);
#135457=SURFACE_STYLE_FILL_AREA(#135471);
#135458=SURFACE_STYLE_FILL_AREA(#135472);
#135459=SURFACE_STYLE_FILL_AREA(#135473);
#135460=SURFACE_STYLE_FILL_AREA(#135474);
#135461=SURFACE_STYLE_FILL_AREA(#135475);
#135462=SURFACE_STYLE_FILL_AREA(#135476);
#135463=SURFACE_STYLE_FILL_AREA(#135477);
#135464=SURFACE_STYLE_FILL_AREA(#135478);
#135465=SURFACE_STYLE_FILL_AREA(#135479);
#135466=FILL_AREA_STYLE('Steel - Satin',(#135480));
#135467=FILL_AREA_STYLE('Opaque(206,210,216)',(#135481));
#135468=FILL_AREA_STYLE('Opaque(220,223,228)',(#135482));
#135469=FILL_AREA_STYLE('Opaque(214,178,102)',(#135483));
#135470=FILL_AREA_STYLE('Opaque(234,236,239)',(#135484));
#135471=FILL_AREA_STYLE('Opaque(228,231,235)',(#135485));
#135472=FILL_AREA_STYLE('Opaque(238,239,241)',(#135486));
#135473=FILL_AREA_STYLE('Opaque(236,238,240)',(#135487));
#135474=FILL_AREA_STYLE('Opaque(200,205,211)',(#135488));
#135475=FILL_AREA_STYLE('Opaque(196,201,207)',(#135489));
#135476=FILL_AREA_STYLE('Opaque(212,215,220)',(#135490));
#135477=FILL_AREA_STYLE('Opaque(199,204,210)',(#135491));
#135478=FILL_AREA_STYLE('Opaque(201,205,211)',(#135492));
#135479=FILL_AREA_STYLE('Opaque(203,207,213)',(#135493));
#135480=FILL_AREA_STYLE_COLOUR('Steel - Satin',#135494);
#135481=FILL_AREA_STYLE_COLOUR('Opaque(206,210,216)',#135495);
#135482=FILL_AREA_STYLE_COLOUR('Opaque(220,223,228)',#135496);
#135483=FILL_AREA_STYLE_COLOUR('Opaque(214,178,102)',#135497);
#135484=FILL_AREA_STYLE_COLOUR('Opaque(234,236,239)',#135498);
#135485=FILL_AREA_STYLE_COLOUR('Opaque(228,231,235)',#135499);
#135486=FILL_AREA_STYLE_COLOUR('Opaque(238,239,241)',#135500);
#135487=FILL_AREA_STYLE_COLOUR('Opaque(236,238,240)',#135501);
#135488=FILL_AREA_STYLE_COLOUR('Opaque(200,205,211)',#135502);
#135489=FILL_AREA_STYLE_COLOUR('Opaque(196,201,207)',#135503);
#135490=FILL_AREA_STYLE_COLOUR('Opaque(212,215,220)',#135504);
#135491=FILL_AREA_STYLE_COLOUR('Opaque(199,204,210)',#135505);
#135492=FILL_AREA_STYLE_COLOUR('Opaque(201,205,211)',#135506);
#135493=FILL_AREA_STYLE_COLOUR('Opaque(203,207,213)',#135507);
#135494=COLOUR_RGB('Steel - Satin', 0.09019608, 0.27058824, 0.51372549);
#135495=COLOUR_RGB('Opaque(206,210,216)', 0.09019608, 0.27058824, 0.51372549);
#135496=COLOUR_RGB('Opaque(220,223,228)', 0.66274510, 0.83137255, 0.94901961);
#135497=COLOUR_RGB('Opaque(214,178,102)', 0.31764706, 0.68627451, 0.89019608);
#135498=COLOUR_RGB('Opaque(234,236,239)', 0.40784314, 0.44705882, 0.49803922);
#135499=COLOUR_RGB('Opaque(228,231,235)', 0.72549020, 0.75294118, 0.79215686);
#135500=COLOUR_RGB('Opaque(238,239,241)', 0.08235294, 0.09019608, 0.10196078);
#135501=COLOUR_RGB('Opaque(236,238,240)', 0.09019608, 0.27058824, 0.51372549);
#135502=COLOUR_RGB('Opaque(200,205,211)', 0.66274510, 0.83137255, 0.94901961);
#135503=COLOUR_RGB('Opaque(196,201,207)', 0.31764706, 0.68627451, 0.89019608);
#135504=COLOUR_RGB('Opaque(212,215,220)', 0.40784314, 0.44705882, 0.49803922);
#135505=COLOUR_RGB('Opaque(199,204,210)', 0.72549020, 0.75294118, 0.79215686);
#135506=COLOUR_RGB('Opaque(201,205,211)', 0.08235294, 0.09019608, 0.10196078);
#135507=COLOUR_RGB('Opaque(203,207,213)', 0.09019608, 0.27058824, 0.51372549);
ENDSEC;
END-ISO-10303-21;
